#48527 = CARTESIAN_POINT ( 'NONE',  ( 17.20831665107776587, 37.88393115100078745, 7.208316651077764980 ) ) ;
#48528 = CARTESIAN_POINT ( 'NONE',  ( -8.000000000000000000, 80.99999999999994316, 3.000000000000000000 ) ) ;
#48530 = EDGE_CURVE ( 'NONE', #7679, #37275, #19510, .T. ) ;
#48529 = CARTESIAN_POINT ( 'NONE',  ( -0.8801773607111009756, 58.06368534415484106, 1.068504757029289695E-15 ) ) ;
#48531 = CARTESIAN_POINT ( 'NONE',  ( 6.565887622018943937, 35.16530133659708923, 12.81628187352647430 ) ) ;
#48532 = CARTESIAN_POINT ( 'NONE',  ( -5.204170427930421283E-15, -39.44625116508603213, -14.16423886937410082 ) ) ;
#48533 = CARTESIAN_POINT ( 'NONE',  ( 1.472469842513823179, 25.59226448433412315, -4.923371831947296329 ) ) ;
#48534 = CARTESIAN_POINT ( 'NONE',  ( 6.204703633549690345, 10.76208216824729824, -14.16423886937410259 ) ) ;
#48535 = ORIENTED_EDGE ( 'NONE', *, *, #61373, .T. ) ;
#48536 = ORIENTED_EDGE ( 'NONE', *, *, #81374, .F. ) ;
#48537 = EDGE_CURVE ( 'NONE', #19902, #37612, #98490, .T. ) ;
#48538 = CARTESIAN_POINT ( 'NONE',  ( 0.5774900079438590739, 32.64701867748816966, -5.440088680355550821 ) ) ;
#48539 = CARTESIAN_POINT ( 'NONE',  ( 22.26659068614895176, 34.72041550158063927, -7.082119434687042414 ) ) ;
#48540 = CARTESIAN_POINT ( 'NONE',  ( 17.20831665107776587, 47.88393115100078745, 7.208316651077764980 ) ) ;
#48541 = CARTESIAN_POINT ( 'NONE',  ( 5.076628168052704559, 10.17559781766745175, -8.527530157486179263 ) ) ;
#48543 = CARTESIAN_POINT ( 'NONE',  ( 64.56412365047462742, 13.99999999999999467, -9.500000000000000000 ) ) ;
#48542 = CARTESIAN_POINT ( 'NONE',  ( 19.38216949554541202, 50.99863466993042493, 9.382169495545424454 ) ) ;
#48544 = CARTESIAN_POINT ( 'NONE',  ( 17.96484262340118221, 24.93868534415484461, 7.964842623401181321 ) ) ;
#48545 = CARTESIAN_POINT ( 'NONE',  ( 11.49999999999999645, 75.00000000000000000, -8.525133428036872019 ) ) ;
#48546 = CARTESIAN_POINT ( 'NONE',  ( 13.43411237798105340, 25.58196800326374998, 12.81628187352647963 ) ) ;
#48547 = CARTESIAN_POINT ( 'NONE',  ( 2.791683348922237240, 35.38393115100079456, -7.208316651077763204 ) ) ;
#48548 = CARTESIAN_POINT ( 'NONE',  ( -2.915334737309917656, 4.105352010821503583, 10.88017736071110164 ) ) ;
#48549 = CARTESIAN_POINT ( 'NONE',  ( -25.69000000000001194, 93.50000000000000000, -10.09898361729590199 ) ) ;
#48551 = CARTESIAN_POINT ( 'NONE',  ( 18.95386800105010394, 33.23810908735718783, -6.500000000000008882 ) ) ;
#48550 = CARTESIAN_POINT ( 'NONE',  ( 10.00000000000000000, 61.81368534415484106, -10.88017736071110342 ) ) ;
#48552 = CARTESIAN_POINT ( 'NONE',  ( -10.91022435255008283, -52.91485255063000182, 4.000000000000000000 ) ) ;
#48553 = FACE_OUTER_BOUND ( 'NONE', #37530, .T. ) ;
#48554 = CARTESIAN_POINT ( 'NONE',  ( 7.084665262690076126, 59.10535201082150536, 10.88017736071109987 ) ) ;
#48555 = CARTESIAN_POINT ( 'NONE',  ( -0.8801773607110991993, 52.85535201082151247, -2.915334737309923874 ) ) ;
#48556 = DIRECTION ( 'NONE',  ( -0.000000000000000000, -1.000000000000000000, -0.000000000000000000 ) ) ;
#48558 = ADVANCED_FACE ( 'NONE', ( #10536 ), #93535, .T. ) ;
#48557 = FILL_AREA_STYLE ('',( #63559 ) ) ;
#48559 = CIRCLE ( 'NONE', #96479, 2.000000000000000888 ) ;
#48560 = CARTESIAN_POINT ( 'NONE',  ( 12.91533473730993009, 11.60535201082150714, -10.88017736071109987 ) ) ;
#48561 = CARTESIAN_POINT ( 'NONE',  ( 10.00000000000000178, 62.25893115100078745, 9.846743663894594434 ) ) ;
#48563 = CARTESIAN_POINT ( 'NONE',  ( 0.000000000000000000, 0.000000000000000000, 0.000000000000000000 ) ) ;
#48562 = CARTESIAN_POINT ( 'NONE',  ( 17.96484262340118221, 16.18868534415483396, -7.964842623401177768 ) ) ;
#48564 = CARTESIAN_POINT ( 'NONE',  ( 16.40814093676323893, 30.79030133659708923, 11.09922568453595026 ) ) ;
#48565 = ORIENTED_EDGE ( 'NONE', *, *, #17312, .F. ) ;
#48566 = CARTESIAN_POINT ( 'NONE',  ( -0.8801773607111009756, 53.06368534415484106, 1.068504757029289695E-15 ) ) ;
#48567 = EDGE_CURVE ( 'NONE', #30525, #40405, #27583, .T. ) ;
#48568 = CARTESIAN_POINT ( 'NONE',  ( 12.63842701281683922, 44.55059781766745175, -9.846743663894590881 ) ) ;
#48569 = AXIS2_PLACEMENT_3D ( 'NONE', #52233, #59725, #23729 ) ;
#48571 = SURFACE_STYLE_FILL_AREA ( #57055 ) ;
#48570 = CARTESIAN_POINT ( 'NONE',  ( 10.00000000000000000, 7.873634669930421381, -12.81628187352647608 ) ) ;
#48572 = CARTESIAN_POINT ( 'NONE',  ( 19.42250999205614548, 25.98035201082150891, -5.440088680355545492 ) ) ;
#48573 = CARTESIAN_POINT ( 'NONE',  ( 2.035157376598822676, 42.43868534415483396, -7.964842623401177768 ) ) ;
#48574 = CARTESIAN_POINT ( 'NONE',  ( -0.3689425029237898834, 51.17874883491397497, -10.36894250292378850 ) ) ;
#48575 = CARTESIAN_POINT ( 'NONE',  ( 17.20831665107776587, 37.88393115100078745, 7.208316651077764980 ) ) ;
#48576 = CARTESIAN_POINT ( 'NONE',  ( 19.42250999205614548, 60.98035201082151247, -5.440088680355545492 ) ) ;
#48577 = CARTESIAN_POINT ( 'NONE',  ( -0.8801773607111009756, 48.06368534415484817, 1.068504757029289695E-15 ) ) ;
#48578 = CARTESIAN_POINT ( 'NONE',  ( -8.564643372776458818, 14.63606914147517735, -12.31449893000756468 ) ) ;
#48579 = CARTESIAN_POINT ( 'NONE',  ( 24.16423886937410614, 14.30374883491396787, 8.672049930838204340E-16 ) ) ;
#48580 = DIRECTION ( 'NONE',  ( 0.000000000000000000, 1.000000000000000000, 0.000000000000000000 ) ) ;
#48581 = CARTESIAN_POINT ( 'NONE',  ( 0.2751277870542874204, 39.36607318730131055, -6.499999999999984901 ) ) ;
#48582 = ORIENTED_EDGE ( 'NONE', *, *, #57475, .T. ) ;
#48583 = ORIENTED_EDGE ( 'NONE', *, *, #57903, .F. ) ;
#48584 = CARTESIAN_POINT ( 'NONE',  ( 24.16423886937410614, 49.30374883491396787, 8.672049930838204340E-16 ) ) ;
#48585 = CARTESIAN_POINT ( 'NONE',  ( 20.36894250292379382, 38.67874883491396076, 10.36894250292379205 ) ) ;
#48586 = CARTESIAN_POINT ( 'NONE',  ( 1.472469842513823179, 21.42559781766745175, 4.923371831947296329 ) ) ;
#48587 = DIRECTION ( 'NONE',  ( -0.000000000000000000, -0.000000000000000000, 1.000000000000000000 ) ) ;
#48588 = CARTESIAN_POINT ( 'NONE',  ( 20.15039907845753220, 52.62777174578612716, -6.262539305110077947 ) ) ;
#48590 = CARTESIAN_POINT ( 'NONE',  ( -2.816281873526473856, 29.33196800326376064, 3.434112377981055619 ) ) ;
#48589 = CARTESIAN_POINT ( 'NONE',  ( 7.084665262690076126, 67.02201867748817676, -10.88017736071110164 ) ) ;
#48591 = CARTESIAN_POINT ( 'NONE',  ( -4.164238869374099927, 37.01208216824731068, 3.795296366450308767 ) ) ;
#48592 = CARTESIAN_POINT ( 'NONE',  ( 0.000000000000000000, 0.000000000000000000, 0.000000000000000000 ) ) ;
#48593 = CARTESIAN_POINT ( 'NONE',  ( 7.084665262690076126, 69.10535201082151957, 10.88017736071109987 ) ) ;
#48594 = CARTESIAN_POINT ( 'NONE',  ( -7.208316651077764980, -14.61606884899921077, -7.208316651077759651 ) ) ;
#48595 = CARTESIAN_POINT ( 'NONE',  ( 14.92337183194729633, 7.675597817667451750, 8.527530157486181039 ) ) ;
#48596 = EDGE_LOOP ( 'NONE', ( #25181, #61978, #2545, #95861 ) ) ;
#48597 =( NAMED_UNIT ( * ) SI_UNIT ( $, .STERADIAN. ) SOLID_ANGLE_UNIT ( ) );
#48598 = CARTESIAN_POINT ( 'NONE',  ( 1.472469842513823179, 16.42559781766745175, 4.923371831947296329 ) ) ;
#48599 = FACE_OUTER_BOUND ( 'NONE', #41974, .T. ) ;
#48600 = ORIENTED_EDGE ( 'NONE', *, *, #65382, .F. ) ;
#48601 = CARTESIAN_POINT ( 'NONE',  ( 24.16423886937410614, 4.512082168247300906, -3.795296366450302550 ) ) ;
#48603 = CARTESIAN_POINT ( 'NONE',  ( -0.8801773607111009756, 13.06368534415483929, 1.068504757029289695E-15 ) ) ;
#48602 = CARTESIAN_POINT ( 'NONE',  ( 7.084665262690076126, 9.105352010821503583, 10.88017736071109987 ) ) ;
#48605 = CARTESIAN_POINT ( 'NONE',  ( 0.6178305044545838731, 4.748634669930420493, 9.382169495545420901 ) ) ;
#48604 = CARTESIAN_POINT ( 'NONE',  ( 5.076628168052704559, 30.17559781766745175, -8.527530157486179263 ) ) ;
#48606 =( NAMED_UNIT ( * ) PLANE_ANGLE_UNIT ( ) SI_UNIT ( $, .RADIAN. ) );
#48607 = VECTOR ( 'NONE', #46743, 1000.000000000000000 ) ;
#48608 = CARTESIAN_POINT ( 'NONE',  ( -9.820177974736479243, 14.76984956101180835, 11.25994418464046198 ) ) ;
#48609 = EDGE_CURVE ( 'NONE', #24064, #56450, #25554, .T. ) ;
#48610 = CARTESIAN_POINT ( 'NONE',  ( 10.00000000000000000, 12.87363466993042138, -12.81628187352647608 ) ) ;
#48611 = EDGE_LOOP ( 'NONE', ( #2559, #27189, #78969, #95005 ) ) ;
#48612 = CARTESIAN_POINT ( 'NONE',  ( -0.3689425029237898834, 46.17874883491397497, -10.36894250292378850 ) ) ;
#48613 = ORIENTED_EDGE ( 'NONE', *, *, #70780, .F. ) ;
#48614 = CARTESIAN_POINT ( 'NONE',  ( 17.08211943468705840, 60.13708216824729647, -12.26659068614894466 ) ) ;
#48615 = ORIENTED_EDGE ( 'NONE', *, *, #80844, .F. ) ;
#48616 = CARTESIAN_POINT ( 'NONE',  ( 0.5774900079438590739, 27.64701867748817676, -5.440088680355550821 ) ) ;
#48617 = CARTESIAN_POINT ( 'NONE',  ( 0.5774900079438590739, 37.64701867748817676, -5.440088680355550821 ) ) ;
#48618 = CARTESIAN_POINT ( 'NONE',  ( 19.42250999205614548, 60.98035201082151247, -5.440088680355545492 ) ) ;
#48619 = CARTESIAN_POINT ( 'NONE',  ( 15.44008868035555260, 29.73035201082150891, 9.422509992056143702 ) ) ;
#48621 = EDGE_LOOP ( 'NONE', ( #6673, #70736, #79119, #4452 ) ) ;
#48620 = CARTESIAN_POINT ( 'NONE',  ( -8.000000000000000000, 41.24999999999999289, 4.000000000000000000 ) ) ;
#48622 = STYLED_ITEM ( 'NONE', ( #87864 ), #95471 ) ;
#48623 = CARTESIAN_POINT ( 'NONE',  ( 18.52753015748617571, 18.09226448433411960, 4.923371831947298993 ) ) ;
#48624 = CARTESIAN_POINT ( 'NONE',  ( -3.770608837557422710, -6.399801140515898545, 2.750000000000403677 ) ) ;
#48625 = VERTEX_POINT ( 'NONE', #4031 ) ;
#48626 = CARTESIAN_POINT ( 'NONE',  ( 11.33984840998195054, -87.82327540140187239, 3.750000000000000000 ) ) ;
#48627 = CARTESIAN_POINT ( 'NONE',  ( 2.791683348922237240, 45.38393115100079456, -7.208316651077763204 ) ) ;
#48628 = VECTOR ( 'NONE', #47441, 1000.000000000000000 ) ;
#48629 = DIRECTION ( 'NONE',  ( 0.000000000000000000, 1.000000000000000000, 0.000000000000000000 ) ) ;
#48630 = CARTESIAN_POINT ( 'NONE',  ( 3.591859063236761518, 44.95696800326376064, 11.09922568453594849 ) ) ;
#48631 = ADVANCED_FACE ( 'NONE', ( #56046 ), #96513, .T. ) ;
#48632 = CARTESIAN_POINT ( 'NONE',  ( -6.445967608602039434, -48.01283281809150338, 2.750000000000000000 ) ) ;
#48633 = CYLINDRICAL_SURFACE ( 'NONE', #26859, 1.000000000000007772 ) ;
#48634 = CARTESIAN_POINT ( 'NONE',  ( 7.993487411949270260, 0.04962888323599794205, 12.40005926694712990 ) ) ;
#48635 = CARTESIAN_POINT ( 'NONE',  ( 2.791683348922240793, 61.63393115100079456, 7.208316651077764092 ) ) ;
#48636 = CARTESIAN_POINT ( 'NONE',  ( 24.16423886937410614, 49.30374883491396787, 8.672049930838204340E-16 ) ) ;
#48637 = CARTESIAN_POINT ( 'NONE',  ( 6.689969769698871360, 15.00000000000000000, 12.58200319823975022 ) ) ;
#48638 = ORIENTED_EDGE ( 'NONE', *, *, #95617, .F. ) ;
#48639 = CARTESIAN_POINT ( 'NONE',  ( 1.042145700049401436, 4.742161081720030147, -6.499999999999861444 ) ) ;
#48640 = CARTESIAN_POINT ( 'NONE',  ( 1.472469842513823179, 26.42559781766745175, 4.923371831947296329 ) ) ;
#48641 = CARTESIAN_POINT ( 'NONE',  ( -2.816281873526473856, 64.33196800326376774, 3.434112377981055619 ) ) ;
#48642 = CARTESIAN_POINT ( 'NONE',  ( 1.472469842513823179, 65.59226448433412315, -4.923371831947296329 ) ) ;
#48643 = CARTESIAN_POINT ( 'NONE',  ( 14.92337183194729633, 2.675597817667451750, 8.527530157486181039 ) ) ;
#48644 = CARTESIAN_POINT ( 'NONE',  ( -0.03743638938523734944, 4.251975280310180239, -6.399506433553933782 ) ) ;
#48645 = B_SPLINE_CURVE_WITH_KNOTS ( 'NONE', 3,
 ( #74435, #21455, #82936, #21957, #14453, #27463 ),
 .UNSPECIFIED., .F., .F.,
 ( 4, 2, 4 ),
 ( 3.409110551496048698E-05, 0.0004400426677367984978, 0.0008459942299586365290 ),
 .UNSPECIFIED. ) ;
#48646 = CARTESIAN_POINT ( 'NONE',  ( 12.63842701281683922, 64.55059781766745175, -9.846743663894590881 ) ) ;
#48647 = CARTESIAN_POINT ( 'NONE',  ( 20.32896413005680358, 14.74545670184113710, 5.963430220938287007 ) ) ;
#48648 = MECHANICAL_DESIGN_GEOMETRIC_PRESENTATION_REPRESENTATION (  '', ( #64618 ), #37549 ) ;
#48649 = ADVANCED_FACE ( 'NONE', ( #48028 ), #89820, .T. ) ;
#48650 = EDGE_CURVE ( 'NONE', #75691, #73066, #67500, .T. ) ;
#48651 = VERTEX_POINT ( 'NONE', #21991 ) ;
#48652 = CARTESIAN_POINT ( 'NONE',  ( 24.16423886937410614, 59.51208216824728936, -3.795296366450302550 ) ) ;
#48653 = CARTESIAN_POINT ( 'NONE',  ( -18.89999999999999503, 92.00000000000000000, 8.000000000000000000 ) ) ;
#48654 = CARTESIAN_POINT ( 'NONE',  ( 7.084665262690076126, 47.02201867748818387, -10.88017736071110164 ) ) ;
#48656 = CARTESIAN_POINT ( 'NONE',  ( 17.96484262340118221, 66.18868534415483396, -7.964842623401177768 ) ) ;
#48655 = CARTESIAN_POINT ( 'NONE',  ( -2.816281873526471635, 13.91530133659708746, -3.434112377981056508 ) ) ;
#48657 = CARTESIAN_POINT ( 'NONE',  ( 10.93781366033347169, 0.5000000000000004441, -10.26470809774065351 ) ) ;
#48658 = CARTESIAN_POINT ( 'NONE',  ( 19.80777595082615861, 45.68878173731741299, -6.499999999999961808 ) ) ;
#48659 = CARTESIAN_POINT ( 'NONE',  ( 1.472469842513823179, 56.42559781766745886, 4.923371831947296329 ) ) ;
#48660 = CARTESIAN_POINT ( 'NONE',  ( 10.00000000000000178, 7.258931151000785675, 9.846743663894594434 ) ) ;
#48661 = CARTESIAN_POINT ( 'NONE',  ( 3.469446951953614189E-15, -35.68631465584515894, 10.88017736071110342 ) ) ;
#48662 = CARTESIAN_POINT ( 'NONE',  ( 22.81628187352647785, 6.623634669930420493, 6.195893100308588602E-16 ) ) ;
#48664 = DIRECTION ( 'NONE',  ( 0.000000000000000000, 0.000000000000000000, 1.000000000000000000 ) ) ;
#48663 = CARTESIAN_POINT ( 'NONE',  ( 10.00000000000000000, 21.81368534415484106, -10.88017736071110342 ) ) ;
#48665 = CARTESIAN_POINT ( 'NONE',  ( 13.99999999999999822, 10.49999999999999822, -6.000000000000000000 ) ) ;
#48666 =( GEOMETRIC_REPRESENTATION_CONTEXT ( 3 ) GLOBAL_UNCERTAINTY_ASSIGNED_CONTEXT ( ( #74264 ) ) GLOBAL_UNIT_ASSIGNED_CONTEXT ( ( #4608, #48606, #34087 ) ) REPRESENTATION_CONTEXT ( 'NONE', 'WORKASPACE' ) );
#48667 = CARTESIAN_POINT ( 'NONE',  ( 6.204703633549690345, 37.84541550158063927, 14.16423886937410082 ) ) ;
#48668 = CARTESIAN_POINT ( 'NONE',  ( 13.79529636645031943, 25.34541550158063572, -14.16423886937409904 ) ) ;
#48669 = CARTESIAN_POINT ( 'NONE',  ( 7.084665262690076126, 2.022018677488171434, -10.88017736071110164 ) ) ;
#48670 = CARTESIAN_POINT ( 'NONE',  ( 19.84674366389459266, 38.30059781766745175, 2.638427012816836559 ) ) ;
#48671 = CARTESIAN_POINT ( 'NONE',  ( 22.81628187352648496, 41.83196800326375353, -3.434112377981050290 ) ) ;
#48672 = CARTESIAN_POINT ( 'NONE',  ( -0.8801773607111009756, 13.06368534415483929, 1.068504757029289695E-15 ) ) ;
#48673 = ORIENTED_EDGE ( 'NONE', *, *, #40324, .F. ) ;
#48674 = CARTESIAN_POINT ( 'NONE',  ( 18.52753015748617571, 33.09226448433411605, 4.923371831947298993 ) ) ;
#48675 = CARTESIAN_POINT ( 'NONE',  ( -0.8801773607111008646, 43.27201867748817676, 2.915334737309923430 ) ) ;
#48676 = CARTESIAN_POINT ( 'NONE',  ( 6.565887622018943937, 10.16530133659708746, 12.81628187352647430 ) ) ;
#48678 = CARTESIAN_POINT ( 'NONE',  ( 17.35999999999999943, 33.99999999999997158, 10.00000000000000000 ) ) ;
#48677 = CARTESIAN_POINT ( 'NONE',  ( 17.08211943468705840, 15.13708216824730179, -12.26659068614894466 ) ) ;
#48680 = CARTESIAN_POINT ( 'NONE',  ( 14.40939250469964961, 15.00000000000000000, 1.618458416365853747 ) ) ;
#48679 = B_SPLINE_CURVE_WITH_KNOTS ( 'NONE', 3,
 ( #87924, #80928, #19441, #49930, #33924, #11936, #65415, #26933, #42441, #72923 ),
 .UNSPECIFIED., .F., .F.,
 ( 4, 3, 3, 4 ),
 ( 7.573910767901059648E-18, 0.0006253016069560791285, 0.001250604074564940806, 0.002501455912506563885 ),
 .UNSPECIFIED. ) ;
#48681 = CARTESIAN_POINT ( 'NONE',  ( 19.84674366389459266, 28.30059781766745886, 2.638427012816836559 ) ) ;
#48682 = CARTESIAN_POINT ( 'NONE',  ( -1.099225684535947600, 53.70696800326376064, -6.408140936763238038 ) ) ;
#48683 = CARTESIAN_POINT ( 'NONE',  ( 12.63842701281683922, 59.55059781766744464, -9.846743663894590881 ) ) ;
#48684 = ORIENTED_EDGE ( 'NONE', *, *, #46967, .F. ) ;
#48685 = EDGE_CURVE ( 'NONE', #33923, #34058, #5261, .T. ) ;
#48686 = CARTESIAN_POINT ( 'NONE',  ( 12.35505582470273644, 15.00000000000000000, -10.16021613965630443 ) ) ;
#48687 = CARTESIAN_POINT ( 'NONE',  ( 4.380000000000000782, 1.019547802438464545, 3.750000000000001776 ) ) ;
#48688 = CARTESIAN_POINT ( 'NONE',  ( -0.3689425029237881626, 62.42874883491396787, 10.36894250292379027 ) ) ;
#48689 = CARTESIAN_POINT ( 'NONE',  ( 22.26659068614895176, 9.720415501580633943, -7.082119434687042414 ) ) ;
#48690 = CARTESIAN_POINT ( 'NONE',  ( 20.88017736071110164, 65.35535201082150536, 2.915334737309930979 ) ) ;
#48691 = CARTESIAN_POINT ( 'NONE',  ( 5.076628168052704559, 45.17559781766745175, -8.527530157486179263 ) ) ;
#48692 = CARTESIAN_POINT ( 'NONE',  ( 2.035157376598824452, 23.68868534415484461, 7.964842623401179544 ) ) ;
#48693 = CARTESIAN_POINT ( 'NONE',  ( 4.219999999999999751, 36.75000000000000000, 2.750000000000000000 ) ) ;
#48694 = CARTESIAN_POINT ( 'NONE',  ( 18.52753015748617571, 63.09226448433412315, 4.923371831947298993 ) ) ;
#48695 = VECTOR ( 'NONE', #73889, 1000.000000000000000 ) ;
#48696 = ORIENTED_EDGE ( 'NONE', *, *, #92118, .F. ) ;
#48697 = EDGE_LOOP ( 'NONE', ( #38342, #28858, #3814, #4222, #10180, #7072 ) ) ;
#48698 = ORIENTED_EDGE ( 'NONE', *, *, #20227, .T. ) ;
#48699 = DIRECTION ( 'NONE',  ( 0.000000000000000000, 0.000000000000000000, 1.000000000000000000 ) ) ;
#48700 = CARTESIAN_POINT ( 'NONE',  ( 6.204703633549690345, 10.76208216824729824, -14.16423886937410259 ) ) ;
#48701 = FILL_AREA_STYLE ('',( #25248 ) ) ;
#48702 = CARTESIAN_POINT ( 'NONE',  ( 13.79529636645030344, 38.26208216824729647, 14.16423886937410614 ) ) ;
#48703 = CARTESIAN_POINT ( 'NONE',  ( 18.52753015748618282, 58.92559781766745886, -4.923371831947291888 ) ) ;
#48704 = CARTESIAN_POINT ( 'NONE',  ( 10.00000000000000000, 19.75893115100078390, -9.846743663894594434 ) ) ;
#48705 = CARTESIAN_POINT ( 'NONE',  ( -2.816281873526473856, 64.33196800326376774, 3.434112377981055619 ) ) ;
#48707 = CARTESIAN_POINT ( 'NONE',  ( 18.52753015748617571, 58.09226448433411605, 4.923371831947298993 ) ) ;
#48706 = CARTESIAN_POINT ( 'NONE',  ( 17.96484262340118221, 24.93868534415484461, 7.964842623401181321 ) ) ;
#48708 = CARTESIAN_POINT ( 'NONE',  ( -4.164238869374099927, 2.012082168247300906, 3.795296366450308767 ) ) ;
#48709 = CARTESIAN_POINT ( 'NONE',  ( 2.917880565312948704, 42.63708216824729647, 12.26659068614894643 ) ) ;
#48710 =( GEOMETRIC_REPRESENTATION_CONTEXT ( 3 ) GLOBAL_UNCERTAINTY_ASSIGNED_CONTEXT ( ( #51475 ) ) GLOBAL_UNIT_ASSIGNED_CONTEXT ( ( #67841, #14345, #13847 ) ) REPRESENTATION_CONTEXT ( 'NONE', 'WORKASPACE' ) );
#48711 = CARTESIAN_POINT ( 'NONE',  ( -0.8801773607111008646, 8.272018677488171434, 2.915334737309923430 ) ) ;
#48712 = CARTESIAN_POINT ( 'NONE',  ( 5.076628168052703671, 66.84226448433412315, 8.527530157486179263 ) ) ;
#48713 = DIRECTION ( 'NONE',  ( 0.000000000000000000, 1.000000000000000000, 0.000000000000000000 ) ) ;
#48714 = CARTESIAN_POINT ( 'NONE',  ( 15.44008868035555260, 64.73035201082151957, 9.422509992056143702 ) ) ;
#48715 = CARTESIAN_POINT ( 'NONE',  ( 14.92337183194729988, 34.34226448433411605, -8.527530157486177487 ) ) ;
#48716 = CARTESIAN_POINT ( 'NONE',  ( -7.121448108906508700, -73.25984652122873797, 3.750000000000000888 ) ) ;
#48717 = ORIENTED_EDGE ( 'NONE', *, *, #81866, .F. ) ;
#48718 = CARTESIAN_POINT ( 'NONE',  ( 0.9940297508536876103, -0.03417435944610275333, 14.21528771620250353 ) ) ;
#48719 = ORIENTED_EDGE ( 'NONE', *, *, #7294, .T. ) ;
#48720 = CARTESIAN_POINT ( 'NONE',  ( 18.52753015748617571, 23.09226448433411960, 4.923371831947298993 ) ) ;
#48721 = ORIENTED_EDGE ( 'NONE', *, *, #14032, .F. ) ;
#48722 = CARTESIAN_POINT ( 'NONE',  ( 24.16423886937410614, 39.30374883491396787, 8.672049930838204340E-16 ) ) ;
#48723 = CARTESIAN_POINT ( 'NONE',  ( 0.1532563361054083140, 36.00893115100078745, 1.131784320476157264E-15 ) ) ;
#48724 = CARTESIAN_POINT ( 'NONE',  ( 15.44008868035555260, 49.73035201082150536, 9.422509992056143702 ) ) ;
#48725 = CARTESIAN_POINT ( 'NONE',  ( 0.5774900079438590739, 47.64701867748817676, -5.440088680355550821 ) ) ;
#48726 = CARTESIAN_POINT ( 'NONE',  ( 14.49440716394873263, 4.853942851202206293E-16, 0.4026921475167233311 ) ) ;
#48727 = AXIS2_PLACEMENT_3D ( 'NONE', #24232, #32192, #86693 ) ;
#48728 = CARTESIAN_POINT ( 'NONE',  ( 6.408140936763236262, -2.543031996736243361, -11.09922568453595026 ) ) ;
#48729 = ORIENTED_EDGE ( 'NONE', *, *, #80448, .T. ) ;
#48730 = CARTESIAN_POINT ( 'NONE',  ( 20.88017736071110519, 45.56368534415484106, 2.639326808657452039E-16 ) ) ;
#48731 = CARTESIAN_POINT ( 'NONE',  ( -2.266590686148945544, 1.387082168247301128, -7.082119434687050408 ) ) ;
#48732 = ORIENTED_EDGE ( 'NONE', *, *, #32163, .F. ) ;
#48733 = CARTESIAN_POINT ( 'NONE',  ( 10.00000000000000178, 30.37363466993042138, 12.81628187352647608 ) ) ;
#48734 = CARTESIAN_POINT ( 'NONE',  ( 19.84674366389459266, 28.71726448433411960, -2.638427012816827677 ) ) ;
#48735 = PRESENTATION_STYLE_ASSIGNMENT (( #26724 ) ) ;
#48736 = CARTESIAN_POINT ( 'NONE',  ( 22.81628187352647785, 46.62363466993041783, 6.195893100308588602E-16 ) ) ;
#48737 = LINE ( 'NONE', #35709, #19186 ) ;
#48738 = CARTESIAN_POINT ( 'NONE',  ( 7.361572987183170547, 27.05059781766745175, 9.846743663894590881 ) ) ;
#48740 = EDGE_CURVE ( 'NONE', #54629, #23697, #60557, .T. ) ;
#48739 = PRESENTATION_LAYER_ASSIGNMENT (  '', '', ( #31181 ) ) ;
#48741 = CARTESIAN_POINT ( 'NONE',  ( 0.5774900079438607392, 58.48035201082151247, 5.440088680355550821 ) ) ;
#48742 = VECTOR ( 'NONE', #12646, 1000.000000000000000 ) ;
#48743 = CARTESIAN_POINT ( 'NONE',  ( 0.000000000000000000, 0.5000000000000004441, 0.000000000000000000 ) ) ;
#48744 = CARTESIAN_POINT ( 'NONE',  ( -46.30928139467842897, 104.0823827281712255, 5.529860068218143354 ) ) ;
#48745 = CARTESIAN_POINT ( 'NONE',  ( 1.847340224724850932, 14.95077488074853456, -14.63671528203490979 ) ) ;
#48746 = CARTESIAN_POINT ( 'NONE',  ( 19.84674366389459266, 3.300597817667451750, 2.638427012816836559 ) ) ;
#48747 = CARTESIAN_POINT ( 'NONE',  ( 19.38216949554541557, 7.248634669930421381, -9.382169495545420901 ) ) ;
#48748 = PLANE ( 'NONE',  #1998 ) ;
#48749 = TOROIDAL_SURFACE ( 'NONE', #43968, 14.49999999999999822, 0.5000000000000000000 ) ;
#48750 = CARTESIAN_POINT ( 'NONE',  ( 19.84674366389459266, 43.30059781766744464, 2.638427012816836559 ) ) ;
#48751 = CARTESIAN_POINT ( 'NONE',  ( 19.38216949554541557, 62.24863466993041072, -9.382169495545420901 ) ) ;
#48752 = CARTESIAN_POINT ( 'NONE',  ( 10.00000000000000178, 8.053748834913967869, 14.16423886937410082 ) ) ;
#48753 = CARTESIAN_POINT ( 'NONE',  ( 12.63842701281683922, 39.55059781766744464, -9.846743663894590881 ) ) ;
#48754 = CARTESIAN_POINT ( 'NONE',  ( -1.099225684535947600, 28.70696800326375353, -6.408140936763238038 ) ) ;
#48756 = CARTESIAN_POINT ( 'NONE',  ( 19.89103541497710737, 15.66234555792571292, -6.479102184480796112 ) ) ;
#48755 = CARTESIAN_POINT ( 'NONE',  ( 14.29730467489532408, 4.491438197698105257E-16, 2.416004766803315995 ) ) ;
#48757 = CARTESIAN_POINT ( 'NONE',  ( 2.035157376598824452, 43.68868534415484106, 7.964842623401179544 ) ) ;
#48758 = EDGE_CURVE ( 'NONE', #60661, #47206, #87992, .T. ) ;
#48759 = CARTESIAN_POINT ( 'NONE',  ( 13.43411237798106583, 12.66530133659708746, -12.81628187352647252 ) ) ;
#48760 = CARTESIAN_POINT ( 'NONE',  ( 1.472469842513823179, 41.42559781766745886, 4.923371831947296329 ) ) ;
#48761 = CARTESIAN_POINT ( 'NONE',  ( 0.1532563361054083140, 16.00893115100078390, 1.131784320476157264E-15 ) ) ;
#48762 = CARTESIAN_POINT ( 'NONE',  ( -0.8801773607111009756, 33.06368534415484106, 1.068504757029289695E-15 ) ) ;
#48763 = CARTESIAN_POINT ( 'NONE',  ( 21.09922568453595559, 27.04030133659708568, -6.408140936763230044 ) ) ;
#48764 = AXIS2_PLACEMENT_3D ( 'NONE', #93976, #24516, #85993 ) ;
#48765 = CARTESIAN_POINT ( 'NONE',  ( 5.076628168052704559, 25.17559781766745175, -8.527530157486179263 ) ) ;
#48766 =( LENGTH_UNIT ( ) NAMED_UNIT ( * ) SI_UNIT ( .MILLI., .METRE. ) );
#48767 = CARTESIAN_POINT ( 'NONE',  ( -9.884188733557275341, 88.99910865660901038, 5.687374854485731213 ) ) ;
#48768 = EDGE_CURVE ( 'NONE', #62241, #86312, #74901, .T. ) ;
#48769 = CARTESIAN_POINT ( 'NONE',  ( 4.559911319644449179, 38.89701867748817676, 9.422509992056141925 ) ) ;
#48770 = EDGE_CURVE ( 'NONE', #11363, #41505, #5008, .T. ) ;
#48771 = VERTEX_POINT ( 'NONE', #65986 ) ;
#48772 = CARTESIAN_POINT ( 'NONE',  ( 7.084665262690076126, 64.10535201082150536, 10.88017736071109987 ) ) ;
#48774 = CARTESIAN_POINT ( 'NONE',  ( 4.559911319644449179, 37.23035201082150536, -9.422509992056141925 ) ) ;
#48773 = CARTESIAN_POINT ( 'NONE',  ( 5.076628168052703671, 46.84226448433412315, 8.527530157486179263 ) ) ;
#48775 = SURFACE_STYLE_FILL_AREA ( #16818 ) ;
#48776 = CARTESIAN_POINT ( 'NONE',  ( 15.44008868035555793, 46.39701867748817676, -9.422509992056140149 ) ) ;
#48778 = SURFACE_STYLE_USAGE ( .BOTH. , #71305 ) ;
#48777 = CARTESIAN_POINT ( 'NONE',  ( 4.559911319644449179, 13.89701867748817321, 9.422509992056141925 ) ) ;
#48779 = CARTESIAN_POINT ( 'NONE',  ( 14.94699059465100888, 0.5000000000000004441, 1.259949270174915981 ) ) ;
#48780 = CARTESIAN_POINT ( 'NONE',  ( 2.791683348922237240, 40.38393115100078035, -7.208316651077763204 ) ) ;
#48782 = CARTESIAN_POINT ( 'NONE',  ( 6.382347221874334231, 15.00000000000000000, 13.57444820018231724 ) ) ;
#48781 = CARTESIAN_POINT ( 'NONE',  ( -4.164238869374098151, 36.59541550158063217, -3.795296366450310543 ) ) ;
#48783 = CARTESIAN_POINT ( 'NONE',  ( 1.821708436314931845, 6.667925641218958255, -6.500000000000002665 ) ) ;
#48784 = CARTESIAN_POINT ( 'NONE',  ( -0.2838433074297238012, 13.12729635533385597, 10.00000000000000000 ) ) ;
#48785 = CARTESIAN_POINT ( 'NONE',  ( 24.16423886937410614, 24.51208216824730002, -3.795296366450302550 ) ) ;
#48786 = CARTESIAN_POINT ( 'NONE',  ( -7.121364477235284873, -73.24716134357460362, 2.750000000000000444 ) ) ;
#48787 = ORIENTED_EDGE ( 'NONE', *, *, #6341, .F. ) ;
#48788 = MECHANICAL_DESIGN_GEOMETRIC_PRESENTATION_REPRESENTATION (  '', ( #10482 ), #37687 ) ;
#48789 = CARTESIAN_POINT ( 'NONE',  ( 0.5774900079438590739, 2.647018677488171434, -5.440088680355550821 ) ) ;
#48790 = CARTESIAN_POINT ( 'NONE',  ( 18.52753015748618282, 28.92559781766745175, -4.923371831947291888 ) ) ;
#48792 = CARTESIAN_POINT ( 'NONE',  ( -8.000343251535923628, 84.06932101904432386, -4.000000000000000000 ) ) ;
#48791 = FACE_OUTER_BOUND ( 'NONE', #61987, .T. ) ;
#48793 = CARTESIAN_POINT ( 'NONE',  ( -0.8801773607111008646, 53.27201867748816966, 2.915334737309923430 ) ) ;
#48794 = CARTESIAN_POINT ( 'NONE',  ( -2.816281873526471635, 63.91530133659708923, -3.434112377981056508 ) ) ;
#48795 = CARTESIAN_POINT ( 'NONE',  ( 12.91533473730993009, 31.60535201082150891, -10.88017736071109987 ) ) ;
#48796 = CARTESIAN_POINT ( 'NONE',  ( 3.591859063236761518, 59.95696800326375353, 11.09922568453594849 ) ) ;
#48797 = CARTESIAN_POINT ( 'NONE',  ( 0.6178305044545838731, 4.748634669930420493, 9.382169495545420901 ) ) ;
#48798 = CARTESIAN_POINT ( 'NONE',  ( 14.92337183194729633, 17.67559781766745175, 8.527530157486181039 ) ) ;
#48799 = VERTEX_POINT ( 'NONE', #58481 ) ;
#48800 = ADVANCED_FACE ( 'NONE', ( #28489 ), #58982, .F. ) ;
#48801 = LINE ( 'NONE', #33777, #7948 ) ;
#48802 = CARTESIAN_POINT ( 'NONE',  ( 6.204703633549690345, 65.76208216824731778, -14.16423886937410259 ) ) ;
#48803 = CARTESIAN_POINT ( 'NONE',  ( 20.36894250292379738, 29.92874883491396432, -10.36894250292379027 ) ) ;
#48804 = CARTESIAN_POINT ( 'NONE',  ( 12.91533473730993009, 36.60535201082151247, -10.88017736071109987 ) ) ;
#48805 = CARTESIAN_POINT ( 'NONE',  ( -0.8801773607111009756, 48.06368534415484817, 1.068504757029289695E-15 ) ) ;
#48806 = FILL_AREA_STYLE ('',( #9843 ) ) ;
#48807 = CARTESIAN_POINT ( 'NONE',  ( -7.674335239599113123, 0.2306972965111898366, -12.81961907869226991 ) ) ;
#48808 = CARTESIAN_POINT ( 'NONE',  ( 18.52753015748617571, 13.09226448433411960, 4.923371831947298993 ) ) ;
#48809 = FACE_OUTER_BOUND ( 'NONE', #85138, .T. ) ;
#48810 = CARTESIAN_POINT ( 'NONE',  ( 0.1532563361054100626, 25.80059781766744820, -2.638427012816831230 ) ) ;
#48811 = DIRECTION ( 'NONE',  ( 0.8070303256584299145, -0.5905099943842175847, 0.000000000000000000 ) ) ;
#48812 = CARTESIAN_POINT ( 'NONE',  ( 0.2751277870542967463, 70.00000000000000000, -6.500000000000000888 ) ) ;
#48813 = CARTESIAN_POINT ( 'NONE',  ( 7.361572987183169658, 19.96726448433411960, -9.846743663894592657 ) ) ;
#48814 = CARTESIAN_POINT ( 'NONE',  ( 2.791683348922240793, 46.63393115100077324, 7.208316651077764092 ) ) ;
#48815 = CARTESIAN_POINT ( 'NONE',  ( 22.81628187352647785, 41.62363466993042493, 6.195893100308588602E-16 ) ) ;
#48816 = COLOUR_RGB ( '', 0.66274510, 0.83137255, 0.94901961) ;
#48817 = CARTESIAN_POINT ( 'NONE',  ( 19.42250999205614548, 55.98035201082150536, -5.440088680355545492 ) ) ;
#48818 = CARTESIAN_POINT ( 'NONE',  ( 1.472469842513823179, 26.42559781766745175, 4.923371831947296329 ) ) ;
#48820 = CARTESIAN_POINT ( 'NONE',  ( 1.472469842513823179, 21.42559781766745175, 4.923371831947296329 ) ) ;
#48819 = CARTESIAN_POINT ( 'NONE',  ( -4.164238869374098151, 51.59541550158063217, -3.795296366450310543 ) ) ;
#48821 = DIRECTION ( 'NONE',  ( 0.9943711317468826305, 0.1059530667249613811, 0.000000000000000000 ) ) ;
#48822 = CARTESIAN_POINT ( 'NONE',  ( 1.472469842513823179, 65.59226448433412315, -4.923371831947296329 ) ) ;
#48823 = CARTESIAN_POINT ( 'NONE',  ( 22.26659068614894466, 28.88708216824730357, 7.082119434687054849 ) ) ;
#48824 = CARTESIAN_POINT ( 'NONE',  ( 0.1532563361054082862, 31.21726448433412315, 2.638427012816831674 ) ) ;
#48825 = CARTESIAN_POINT ( 'NONE',  ( 34.56412365047463453, 13.99999999999999645, -10.00000000000000000 ) ) ;
#48826 = CARTESIAN_POINT ( 'NONE',  ( 10.00000000000000178, 19.31368534415484106, 10.88017736071110342 ) ) ;
#48827 = CARTESIAN_POINT ( 'NONE',  ( 4.559911319644449179, 48.89701867748817676, 9.422509992056141925 ) ) ;
#48828 = CARTESIAN_POINT ( 'NONE',  ( 12.91533473730992121, 49.52201867748817676, 10.88017736071110164 ) ) ;
#48829 = ORIENTED_EDGE ( 'NONE', *, *, #70118, .F. ) ;
#48830 = CARTESIAN_POINT ( 'NONE',  ( 16.40814093676324603, 37.45696800326376064, -11.09922568453594671 ) ) ;
#48831 = CARTESIAN_POINT ( 'NONE',  ( 0.5774900079438607392, 58.48035201082151247, 5.440088680355550821 ) ) ;
#48832 = ORIENTED_EDGE ( 'NONE', *, *, #40681, .F. ) ;
#48833 = DIRECTION ( 'NONE',  ( -0.000000000000000000, -0.000000000000000000, 1.000000000000000000 ) ) ;
#48834 = CARTESIAN_POINT ( 'NONE',  ( 2.035157376598824452, 68.68868534415484817, 7.964842623401179544 ) ) ;
#48835 = AXIS2_PLACEMENT_3D ( 'NONE', #40917, #87383, #62405 ) ;
#48836 = ORIENTED_EDGE ( 'NONE', *, *, #77434, .F. ) ;
#48837 = CIRCLE ( 'NONE', #23316, 0.2500000000000002220 ) ;
#48838 = CARTESIAN_POINT ( 'NONE',  ( -0.8801773607111008646, 63.27201867748817676, 2.915334737309923430 ) ) ;
#48839 = CARTESIAN_POINT ( 'NONE',  ( 17.96484262340118221, 4.938685344154837509, 7.964842623401181321 ) ) ;
#48840 = CARTESIAN_POINT ( 'NONE',  ( 1.821708436314921853, 26.66792564121896802, -6.499999999999992006 ) ) ;
#48841 = LINE ( 'NONE', #63833, #26925 ) ;
#48842 = CARTESIAN_POINT ( 'NONE',  ( 4.559911319644449179, 12.23035201082150714, -9.422509992056141925 ) ) ;
#48843 = CARTESIAN_POINT ( 'NONE',  ( 0.1532563361054082862, 16.21726448433411960, 2.638427012816831674 ) ) ;
#48844 = CARTESIAN_POINT ( 'NONE',  ( 24.16423886937410614, 9.303748834913967869, 8.672049930838204340E-16 ) ) ;
#48845 = AXIS2_PLACEMENT_3D ( 'NONE', #58406, #65913, #36415 ) ;
#48846 = CARTESIAN_POINT ( 'NONE',  ( 10.00000000000000178, 2.258931151000784787, 9.846743663894594434 ) ) ;
#48847 = B_SPLINE_CURVE_WITH_KNOTS ( 'NONE', 3,
 ( #66895, #67893, #15397, #43884, #22398, #14402 ),
 .UNSPECIFIED., .F., .F.,
 ( 4, 2, 4 ),
 ( 0.000000000000000000, 0.0002701661927229319750, 0.0005403323854458639500 ),
 .UNSPECIFIED. ) ;
#48848 = CARTESIAN_POINT ( 'NONE',  ( 2.035157376598822676, 7.438685344154837509, -7.964842623401177768 ) ) ;
#48849 = CARTESIAN_POINT ( 'NONE',  ( 0.1532563361054100626, 40.80059781766745886, -2.638427012816831230 ) ) ;
#48850 = ORIENTED_EDGE ( 'NONE', *, *, #22611, .F. ) ;
#48851 = CARTESIAN_POINT ( 'NONE',  ( 10.00000000000000000, 54.75893115100078745, -9.846743663894594434 ) ) ;
#48852 = ORIENTED_EDGE ( 'NONE', *, *, #57142, .F. ) ;
#48853 = CARTESIAN_POINT ( 'NONE',  ( 7.084665262690076126, 47.02201867748818387, -10.88017736071110164 ) ) ;
#48854 = CARTESIAN_POINT ( 'NONE',  ( 7.361572987183170547, 47.05059781766745175, 9.846743663894590881 ) ) ;
#48855 = CARTESIAN_POINT ( 'NONE',  ( 3.591859063236761518, 29.95696800326375708, 11.09922568453594849 ) ) ;
#48857 = CARTESIAN_POINT ( 'NONE',  ( 6.091055032734291608, 15.00000000000000888, 13.29802223412760753 ) ) ;
#48856 = CARTESIAN_POINT ( 'NONE',  ( -13.48255862861931043, 4.084149796850864849E-16, 5.335786055104065007 ) ) ;
#48858 = CARTESIAN_POINT ( 'NONE',  ( 12.91533473730992121, 64.52201867748817676, 10.88017736071110164 ) ) ;
#48859 = CARTESIAN_POINT ( 'NONE',  ( 2.035157376598822676, 7.438685344154837509, -7.964842623401177768 ) ) ;
#48860 = EDGE_CURVE ( 'NONE', #79829, #14094, #80256, .T. ) ;
#48861 = CARTESIAN_POINT ( 'NONE',  ( 22.81628187352648496, 46.83196800326376064, -3.434112377981050290 ) ) ;
#48862 = DIRECTION ( 'NONE',  ( 0.000000000000000000, 0.000000000000000000, 1.000000000000000000 ) ) ;
#48863 = ORIENTED_EDGE ( 'NONE', *, *, #21031, .F. ) ;
#48864 = CARTESIAN_POINT ( 'NONE',  ( 21.09922568453595559, 22.04030133659708923, -6.408140936763230044 ) ) ;
#48865 = CARTESIAN_POINT ( 'NONE',  ( -0.8801773607111009756, 38.06368534415484106, 1.068504757029289695E-15 ) ) ;
#48866 = VERTEX_POINT ( 'NONE', #36490 ) ;
#48867 = CARTESIAN_POINT ( 'NONE',  ( 2.791683348922240793, 66.63393115100079456, 7.208316651077764092 ) ) ;
#48869 = CARTESIAN_POINT ( 'NONE',  ( 7.361572987183170547, 57.05059781766744464, 9.846743663894590881 ) ) ;
#48868 = CARTESIAN_POINT ( 'NONE',  ( 14.92337183194729633, 12.67559781766745353, 8.527530157486181039 ) ) ;
#48870 = CARTESIAN_POINT ( 'NONE',  ( -8.108506836784059146, -3.139057133285344303, 3.750000000000000888 ) ) ;
#48871 = CARTESIAN_POINT ( 'NONE',  ( 18.52753015748618282, 33.92559781766745886, -4.923371831947291888 ) ) ;
#48872 = DIRECTION ( 'NONE',  ( 1.000000000000000000, 0.000000000000000000, 0.000000000000000000 ) ) ;
#48873 = VECTOR ( 'NONE', #92585, 1000.000000000000000 ) ;
#48874 = AXIS2_PLACEMENT_3D ( 'NONE', #61676, #31675, #40176 ) ;
#48875 = CARTESIAN_POINT ( 'NONE',  ( -13.14228782657330896, 14.63595249122789177, -7.230509711182420141 ) ) ;
#48877 = SURFACE_STYLE_USAGE ( .BOTH. , #70420 ) ;
#48876 = CARTESIAN_POINT ( 'NONE',  ( 12.63842701281683034, 27.46726448433411250, 9.846743663894596210 ) ) ;
#48878 = FACE_OUTER_BOUND ( 'NONE', #28591, .T. ) ;
#48880 = EDGE_LOOP ( 'NONE', ( #90888, #71693, #33860, #83048 ) ) ;
#48879 = CARTESIAN_POINT ( 'NONE',  ( 14.92337183194729988, 59.34226448433412315, -8.527530157486177487 ) ) ;
#48881 = DIRECTION ( 'NONE',  ( -2.569960705150826877E-16, 1.000000000000000000, 0.000000000000000000 ) ) ;
#48882 = EDGE_CURVE ( 'NONE', #21081, #12912, #72257, .T. ) ;
#48883 = CARTESIAN_POINT ( 'NONE',  ( 3.591859063236761518, 24.95696800326375353, 11.09922568453594849 ) ) ;
#48884 = CARTESIAN_POINT ( 'NONE',  ( 19.84674366389459266, 48.71726448433413026, -2.638427012816827677 ) ) ;
#48885 = DIRECTION ( 'NONE',  ( 1.000000000000000000, 0.000000000000000000, -0.000000000000000000 ) ) ;
#48886 = CARTESIAN_POINT ( 'NONE',  ( 17.08211943468705840, 40.13708216824731068, -12.26659068614894466 ) ) ;
#48887 = CARTESIAN_POINT ( 'NONE',  ( 0.1532563361054100626, 15.80059781766745353, -2.638427012816831230 ) ) ;
#48888 = ADVANCED_FACE ( 'NONE', ( #12984 ), #51379, .T. ) ;
#48889 = VECTOR ( 'NONE', #64445, 1000.000000000000000 ) ;
#48890 = LINE ( 'NONE', #28362, #20083 ) ;
#48891 = CARTESIAN_POINT ( 'NONE',  ( -2.266590686148945544, 52.22041550158064638, 7.082119434687048631 ) ) ;
#48892 = CARTESIAN_POINT ( 'NONE',  ( 2.791683348922240793, 61.63393115100079456, 7.208316651077764092 ) ) ;
#48893 = CARTESIAN_POINT ( 'NONE',  ( -0.8801773607111008646, 8.272018677488171434, 2.915334737309923430 ) ) ;
#48894 = CARTESIAN_POINT ( 'NONE',  ( 13.79529636645031943, 40.34541550158063217, -14.16423886937409904 ) ) ;
#48896 = CARTESIAN_POINT ( 'NONE',  ( 17.39651004071897589, 34.08210964143323451, -6.499999999999361400 ) ) ;
#48895 = CARTESIAN_POINT ( 'NONE',  ( 24.16423886937410614, 44.51208216824730357, -3.795296366450302550 ) ) ;
#48897 = CARTESIAN_POINT ( 'NONE',  ( 66.76470751278411342, 40.99999999999997868, 9.500000000000000000 ) ) ;
#48898 = PRODUCT_DEFINITION ( 'UNKNOWN', '', #75905, #27487 ) ;
#48900 = CARTESIAN_POINT ( 'NONE',  ( 0.1532563361054082862, 51.21726448433412315, 2.638427012816831674 ) ) ;
#48899 = PLANE ( 'NONE',  #86765 ) ;
#48901 = ORIENTED_EDGE ( 'NONE', *, *, #55426, .T. ) ;
#48902 = CARTESIAN_POINT ( 'NONE',  ( 10.00000000000000000, 41.81368534415484106, -10.88017736071110342 ) ) ;
#48903 = DIRECTION ( 'NONE',  ( 0.000000000000000000, 0.000000000000000000, -1.000000000000000000 ) ) ;
#48904 = CARTESIAN_POINT ( 'NONE',  ( 1.042145700049408319, 64.74216108172002748, -6.499999999999931610 ) ) ;
#48905 = DIRECTION ( 'NONE',  ( 0.000000000000000000, 0.000000000000000000, -1.000000000000000000 ) ) ;
#48906 = CARTESIAN_POINT ( 'NONE',  ( 10.36894250292378850, -0.07125116508603752952, -10.36894250292379027 ) ) ;
#48907 = CARTESIAN_POINT ( 'NONE',  ( 5.076628168052703671, 61.84226448433412315, 8.527530157486179263 ) ) ;
#48908 = CARTESIAN_POINT ( 'NONE',  ( -41.94000000000001194, 93.50000000000000000, -10.09898361729590199 ) ) ;
#48909 = TOROIDAL_SURFACE ( 'NONE', #87234, 14.49999999999999822, 0.5000000000000000000 ) ;
#48910 = VERTEX_POINT ( 'NONE', #69943 ) ;
#48911 = CARTESIAN_POINT ( 'NONE',  ( 2.917880565312950480, 25.97041550158063572, -12.26659068614894821 ) ) ;
#48912 =( GEOMETRIC_REPRESENTATION_CONTEXT ( 3 ) GLOBAL_UNCERTAINTY_ASSIGNED_CONTEXT ( ( #94510 ) ) GLOBAL_UNIT_ASSIGNED_CONTEXT ( ( #13087, #49596, #80105 ) ) REPRESENTATION_CONTEXT ( 'NONE', 'WORKASPACE' ) );
#48913 = LINE ( 'NONE', #17458, #82178 ) ;
#48915 = CARTESIAN_POINT ( 'NONE',  ( 19.42250999205614193, 45.14701867748817676, 5.440088680355555262 ) ) ;
#48914 = CARTESIAN_POINT ( 'NONE',  ( -6.867320125558078914, -58.36821204062274404, -2.750000000000000000 ) ) ;
#48916 = CARTESIAN_POINT ( 'NONE',  ( 19.42250999205614548, 20.98035201082150891, -5.440088680355545492 ) ) ;
#48917 = CARTESIAN_POINT ( 'NONE',  ( 3.591859063236761518, 24.95696800326375353, 11.09922568453594849 ) ) ;
#48918 = DIRECTION ( 'NONE',  ( 0.000000000000000000, 0.000000000000000000, 1.000000000000000000 ) ) ;
#48919 = CARTESIAN_POINT ( 'NONE',  ( 1.472469842513823179, 15.59226448433411960, -4.923371831947296329 ) ) ;
#48920 = CARTESIAN_POINT ( 'NONE',  ( 20.15039907845753575, 59.72266099184918176, 6.262539305110074395 ) ) ;
#48921 = CARTESIAN_POINT ( 'NONE',  ( 2.603489959281199972, 21.58210964143324873, 6.499999999999559464 ) ) ;
#48922 = DIRECTION ( 'NONE',  ( 0.000000000000000000, -1.000000000000000000, 0.000000000000000000 ) ) ;
#48923 = CARTESIAN_POINT ( 'NONE',  ( 0.5774900079438590739, 7.647018677488171434, -5.440088680355550821 ) ) ;
#48924 = CARTESIAN_POINT ( 'NONE',  ( 12.83294900548066053, 0.3639312116172450096, -7.766300266068392411 ) ) ;
#48925 = CARTESIAN_POINT ( 'NONE',  ( 17.96484262340118221, 36.18868534415484106, -7.964842623401177768 ) ) ;
#48926 = CARTESIAN_POINT ( 'NONE',  ( -0.8801773607111008646, 33.27201867748817676, 2.915334737309923430 ) ) ;
#48927 = CARTESIAN_POINT ( 'NONE',  ( 3.591859063236763294, 3.290301336597087012, -11.09922568453595026 ) ) ;
#48928 = CARTESIAN_POINT ( 'NONE',  ( 4.999999999999999112, 61.00000000000000000, 6.500000000000000888 ) ) ;
#48929 = CARTESIAN_POINT ( 'NONE',  ( -2.816281873526473856, 59.12363466993042493, 9.499525473075851096E-16 ) ) ;
#48930 = CARTESIAN_POINT ( 'NONE',  ( 12.63842701281683922, 9.550597817667449974, -9.846743663894590881 ) ) ;
#48931 = EDGE_LOOP ( 'NONE', ( #62481, #26037, #40826, #33775 ) ) ;
#48932 = CARTESIAN_POINT ( 'NONE',  ( 12.91533473730992121, 29.52201867748817321, 10.88017736071110164 ) ) ;
#48933 = CARTESIAN_POINT ( 'NONE',  ( -1.099225684535947600, 33.70696800326375353, -6.408140936763238038 ) ) ;
#48934 = CIRCLE ( 'NONE', #50507, 0.5000000000000004441 ) ;
#48935 = VECTOR ( 'NONE', #76458, 1000.000000000000000 ) ;
#48936 = CIRCLE ( 'NONE', #95251, 14.49999999999999822 ) ;
#48937 = CARTESIAN_POINT ( 'NONE',  ( 0.1532563361054083140, 56.00893115100078745, 1.131784320476157264E-15 ) ) ;
#48938 = CARTESIAN_POINT ( 'NONE',  ( 2.035157376598822676, 67.43868534415484817, -7.964842623401177768 ) ) ;
#48939 = CARTESIAN_POINT ( 'NONE',  ( 0.1532563361054083140, 6.008931151000784787, 1.131784320476157264E-15 ) ) ;
#48940 = CARTESIAN_POINT ( 'NONE',  ( -2.816281873526473856, 29.12363466993041783, 9.499525473075851096E-16 ) ) ;
#48942 = LINE ( 'NONE', #3949, #11247 ) ;
#48941 = CARTESIAN_POINT ( 'NONE',  ( 7.361572987183169658, 4.967264484334119601, -9.846743663894592657 ) ) ;
#48943 = ORIENTED_EDGE ( 'NONE', *, *, #47163, .T. ) ;
#48944 = SURFACE_STYLE_FILL_AREA ( #56936 ) ;
#48945 = DIRECTION ( 'NONE',  ( -1.000000000000000000, -0.000000000000000000, -0.000000000000000000 ) ) ;
#48946 = CARTESIAN_POINT ( 'NONE',  ( 2.035157376598822676, 2.438685344154837953, -7.964842623401177768 ) ) ;
#48948 = CARTESIAN_POINT ( 'NONE',  ( 10.00000000000000000, 25.55374883491396787, -14.16423886937410082 ) ) ;
#48947 = CARTESIAN_POINT ( 'NONE',  ( -2.816281873526473856, 64.33196800326376774, 3.434112377981055619 ) ) ;
#48949 = CARTESIAN_POINT ( 'NONE',  ( 18.52753015748618282, 18.92559781766745175, -4.923371831947291888 ) ) ;
#48950 = CARTESIAN_POINT ( 'NONE',  ( 7.084665262690076126, 7.022018677488169658, -10.88017736071110164 ) ) ;
#48951 = CARTESIAN_POINT ( 'NONE',  ( 12.63842701281683034, 27.46726448433411250, 9.846743663894596210 ) ) ;
#48952 = CARTESIAN_POINT ( 'NONE',  ( 2.035157376598824452, 3.688685344154837953, 7.964842623401179544 ) ) ;
#48953 = VERTEX_POINT ( 'NONE', #67974 ) ;
#48954 = AXIS2_PLACEMENT_3D ( 'NONE', #39667, #62628, #4495 ) ;
#48955 = CARTESIAN_POINT ( 'NONE',  ( 17.96484262340118221, 9.938685344154837509, 7.964842623401181321 ) ) ;
#48956 = CARTESIAN_POINT ( 'NONE',  ( 15.44008868035555260, 14.73035201082150536, 9.422509992056143702 ) ) ;
#48957 = CARTESIAN_POINT ( 'NONE',  ( -45.94000000000000483, 92.00000000000000000, 5.000000000000000000 ) ) ;
#48958 = ORIENTED_EDGE ( 'NONE', *, *, #81770, .F. ) ;
#48959 = CARTESIAN_POINT ( 'NONE',  ( 12.74305857943745046, -3.163668057994810583E-15, 7.177950183686947483 ) ) ;
#48960 = CARTESIAN_POINT ( 'NONE',  ( 4.559911319644449179, 28.89701867748817321, 9.422509992056141925 ) ) ;
#48961 = CARTESIAN_POINT ( 'NONE',  ( 10.00000000000000178, 62.25893115100078745, 9.846743663894594434 ) ) ;
#48962 = CYLINDRICAL_SURFACE ( 'NONE', #39454, 11.25000000000000178 ) ;
#48963 = CARTESIAN_POINT ( 'NONE',  ( 3.591859063236763294, 48.29030133659708923, -11.09922568453595026 ) ) ;
#48964 = LINE ( 'NONE', #10973, #25308 ) ;
#48965 = CARTESIAN_POINT ( 'NONE',  ( 24.16423886937409904, 34.09541550158064638, 3.795296366450317205 ) ) ;
#48966 = CARTESIAN_POINT ( 'NONE',  ( 12.91533473730992121, 34.52201867748817676, 10.88017736071110164 ) ) ;
#48968 = B_SPLINE_CURVE_WITH_KNOTS ( 'NONE', 3,
 ( #76383, #37910, #75890, #63209, #7898, #6904 ),
 .UNSPECIFIED., .F., .F.,
 ( 4, 2, 4 ),
 ( 3.409110551494651432E-05, 0.0004400426677367925347, 0.0008459942299586384806 ),
 .UNSPECIFIED. ) ;
#48967 = CARTESIAN_POINT ( 'NONE',  ( 15.44008868035555793, 11.39701867748817143, -9.422509992056140149 ) ) ;
#48969 = CARTESIAN_POINT ( 'NONE',  ( 0.1532563361054082862, 51.21726448433412315, 2.638427012816831674 ) ) ;
#48970 = AXIS2_PLACEMENT_3D ( 'NONE', #97561, #30504, #29024 ) ;
#48971 = CARTESIAN_POINT ( 'NONE',  ( 18.72515096720590577, 61.07228050351029935, -6.499999999999718447 ) ) ;
#48972 = CARTESIAN_POINT ( 'NONE',  ( 5.076628168052703671, 36.84226448433412315, 8.527530157486179263 ) ) ;
#48973 = CARTESIAN_POINT ( 'NONE',  ( 0.000000000000000000, 14.49999999999999822, 0.000000000000000000 ) ) ;
#48974 = CARTESIAN_POINT ( 'NONE',  ( 14.92337183194729988, 14.34226448433411782, -8.527530157486177487 ) ) ;
#48975 = CARTESIAN_POINT ( 'NONE',  ( 3.469446951953614189E-15, -29.62636533006957862, 12.81628187352647608 ) ) ;
#48976 = ORIENTED_EDGE ( 'NONE', *, *, #88312, .F. ) ;
#48977 = CARTESIAN_POINT ( 'NONE',  ( -0.8801773607111009756, 18.06368534415484106, 1.068504757029289695E-15 ) ) ;
#48978 = CARTESIAN_POINT ( 'NONE',  ( 18.52753015748618282, 8.925597817667451750, -4.923371831947291888 ) ) ;
#48979 = CARTESIAN_POINT ( 'NONE',  ( 19.38216949554541202, 0.9986346699304200492, 9.382169495545424454 ) ) ;
#48980 = CARTESIAN_POINT ( 'NONE',  ( 20.88017736071110164, 50.35535201082151247, 2.915334737309930979 ) ) ;
#48982 = CARTESIAN_POINT ( 'NONE',  ( 22.81628187352648496, 41.83196800326375353, -3.434112377981050290 ) ) ;
#48981 = CARTESIAN_POINT ( 'NONE',  ( 19.42250999205614193, 20.14701867748817321, 5.440088680355555262 ) ) ;
#48983 = CARTESIAN_POINT ( 'NONE',  ( 13.79529636645030344, 28.26208216824729647, 14.16423886937410614 ) ) ;
#48984 = EDGE_CURVE ( 'NONE', #82368, #79612, #55778, .T. ) ;
#48985 = CYLINDRICAL_SURFACE ( 'NONE', #68223, 15.00000000000000000 ) ;
#48986 = PRESENTATION_LAYER_ASSIGNMENT (  '', '', ( #18657 ) ) ;
#48988 = CARTESIAN_POINT ( 'NONE',  ( 10.00000000000000000, 52.87363466993041783, -12.81628187352647608 ) ) ;
#48987 = VECTOR ( 'NONE', #84681, 1000.000000000000000 ) ;
#48989 = ORIENTED_EDGE ( 'NONE', *, *, #2579, .T. ) ;
#48990 = CARTESIAN_POINT ( 'NONE',  ( 14.92337183194729988, 64.34226448433412315, -8.527530157486177487 ) ) ;
#48991 = CARTESIAN_POINT ( 'NONE',  ( 4.559911319644449179, 37.23035201082150536, -9.422509992056141925 ) ) ;
#48992 = EDGE_LOOP ( 'NONE', ( #67602, #69193, #54762, #15144 ) ) ;
#48994 = CARTESIAN_POINT ( 'NONE',  ( -3.271887613349916180, -0.8417457659429956607, 2.500000000000000888 ) ) ;
#48993 = CARTESIAN_POINT ( 'NONE',  ( 10.00000000000000000, -0.2410688489992152128, -9.846743663894594434 ) ) ;
#48995 = CARTESIAN_POINT ( 'NONE',  ( 8.879999999999991900, 27.04366094290857347, 2.900000000000000355 ) ) ;
#48996 = CARTESIAN_POINT ( 'NONE',  ( 12.63842701281683034, 27.46726448433411250, 9.846743663894596210 ) ) ;
#48997 = CARTESIAN_POINT ( 'NONE',  ( 17.20831665107776587, 9.133931151000787452, -7.208316651077762316 ) ) ;
#48998 = CARTESIAN_POINT ( 'NONE',  ( 0.1532563361054100626, 0.8005978176674514168, -2.638427012816831230 ) ) ;
#49001 = LINE ( 'NONE', #94499, #93487 ) ;
#49000 = VECTOR ( 'NONE', #93527, 1000.000000000000000 ) ;
#48999 = CARTESIAN_POINT ( 'NONE',  ( 4.559911319644449179, 58.89701867748817676, 9.422509992056141925 ) ) ;
#49002 = CARTESIAN_POINT ( 'NONE',  ( 7.084665262690076126, 59.10535201082150536, 10.88017736071109987 ) ) ;
#49004 = ORIENTED_EDGE ( 'NONE', *, *, #29174, .T. ) ;
#49003 = CARTESIAN_POINT ( 'NONE',  ( 10.00000000000000000, 24.75893115100078745, -9.846743663894594434 ) ) ;
#49005 = CIRCLE ( 'NONE', #7496, 0.5000000000000004441 ) ;
#49006 = CARTESIAN_POINT ( 'NONE',  ( 5.815488105659666118, 14.76984994604921475, 13.76235181012722286 ) ) ;
#49008 = EDGE_CURVE ( 'NONE', #84748, #59823, #92920, .T. ) ;
#49007 =( GEOMETRIC_REPRESENTATION_CONTEXT ( 3 ) GLOBAL_UNCERTAINTY_ASSIGNED_CONTEXT ( ( #71465 ) ) GLOBAL_UNIT_ASSIGNED_CONTEXT ( ( #89494, #14498, #44969 ) ) REPRESENTATION_CONTEXT ( 'NONE', 'WORKASPACE' ) );
#49009 = CARTESIAN_POINT ( 'NONE',  ( 14.92337183194729988, 54.34226448433412315, -8.527530157486177487 ) ) ;
#49010 = ORIENTED_EDGE ( 'NONE', *, *, #48034, .T. ) ;
#49011 = CARTESIAN_POINT ( 'NONE',  ( -12.22506292814027873, 14.76930270348881002, 8.589871424854626625 ) ) ;
#49012 = CARTESIAN_POINT ( 'NONE',  ( -0.3689425029237898834, 11.17874883491396787, -10.36894250292378850 ) ) ;
#49013 = DIRECTION ( 'NONE',  ( 0.000000000000000000, 0.000000000000000000, -1.000000000000000000 ) ) ;
#49014 = CARTESIAN_POINT ( 'NONE',  ( -4.164238869374099927, 2.012082168247300906, 3.795296366450308767 ) ) ;
#49015 = CARTESIAN_POINT ( 'NONE',  ( 24.16423886937409904, 39.09541550158062506, 3.795296366450317205 ) ) ;
#49016 = CARTESIAN_POINT ( 'NONE',  ( -0.03447792253739288132, 45.15514106990688958, 6.401564815979726930 ) ) ;
#49017 = DIRECTION ( 'NONE',  ( 0.9970872288863208421, 0.07626964003977952655, -0.000000000000000000 ) ) ;
#49018 = CARTESIAN_POINT ( 'NONE',  ( 0.5774900079438590739, 37.64701867748817676, -5.440088680355550821 ) ) ;
#49019 = SURFACE_SIDE_STYLE ('',( #94518 ) ) ;
#49020 = ORIENTED_EDGE ( 'NONE', *, *, #88474, .F. ) ;
#49021 = CARTESIAN_POINT ( 'NONE',  ( 0.1532563361054100626, 10.80059781766745175, -2.638427012816831230 ) ) ;
#49022 = COLOUR_RGB ( '', 0.72549020, 0.75294118, 0.79215686) ;
#49024 = CARTESIAN_POINT ( 'NONE',  ( 10.00000000000000178, 12.25893115100078568, 9.846743663894594434 ) ) ;
#49023 = CARTESIAN_POINT ( 'NONE',  ( 2.035157376598824452, 58.68868534415482685, 7.964842623401179544 ) ) ;
#49025 = CARTESIAN_POINT ( 'NONE',  ( 16.40814093676324603, 42.45696800326375353, -11.09922568453594671 ) ) ;
#49026 = CARTESIAN_POINT ( 'NONE',  ( 10.00000000000000178, 37.25893115100078745, 9.846743663894594434 ) ) ;
#49027 = DIRECTION ( 'NONE',  ( -0.000000000000000000, -1.000000000000000000, -4.683753385137374737E-14 ) ) ;
#49028 = CARTESIAN_POINT ( 'NONE',  ( 20.88017736071110519, 60.56368534415484106, 2.639326808657452039E-16 ) ) ;
#49029 = CARTESIAN_POINT ( 'NONE',  ( 12.63842701281683034, 22.46726448433411605, 9.846743663894596210 ) ) ;
#49030 = CARTESIAN_POINT ( 'NONE',  ( 6.565887622018943937, 28.08196800326375353, -12.81628187352647608 ) ) ;
#49031 = CARTESIAN_POINT ( 'NONE',  ( 14.16423886937410259, -35.69625116508602503, -2.602085213965210642E-15 ) ) ;
#49032 = STYLED_ITEM ( 'NONE', ( #70958 ), #40953 ) ;
#49033 = CARTESIAN_POINT ( 'NONE',  ( 2.791683348922240793, 26.63393115100078745, 7.208316651077764092 ) ) ;
#49034 = CARTESIAN_POINT ( 'NONE',  ( -0.3689425029237898834, 11.17874883491396787, -10.36894250292378850 ) ) ;
#49035 = VERTEX_POINT ( 'NONE', #75957 ) ;
#49036 = CIRCLE ( 'NONE', #2817, 11.25000000000000178 ) ;
#49037 = CARTESIAN_POINT ( 'NONE',  ( 4.559911319644449179, 38.89701867748817676, 9.422509992056141925 ) ) ;
#49038 = CARTESIAN_POINT ( 'NONE',  ( -0.8801773607110991993, 57.85535201082149825, -2.915334737309923874 ) ) ;
#49039 = CARTESIAN_POINT ( 'NONE',  ( 13.79529636645031943, 35.34541550158063927, -14.16423886937409904 ) ) ;
#49040 = CARTESIAN_POINT ( 'NONE',  ( 17.20831665107776587, 54.13393115100079456, -7.208316651077762316 ) ) ;
#49041 = CARTESIAN_POINT ( 'NONE',  ( 14.92337183194729633, 12.67559781766745353, 8.527530157486181039 ) ) ;
#49043 = CARTESIAN_POINT ( 'NONE',  ( -9.402796353260967521, 15.00000000000000000, -11.68706210897770248 ) ) ;
#49042 = CARTESIAN_POINT ( 'NONE',  ( 22.81628187352648496, 61.83196800326376774, -3.434112377981050290 ) ) ;
#49044 = CARTESIAN_POINT ( 'NONE',  ( 15.44008868035555260, 39.73035201082150536, 9.422509992056143702 ) ) ;
#49045 = CARTESIAN_POINT ( 'NONE',  ( -6.767445849361338972, 0.3639308223168559175, 13.38662304974495854 ) ) ;
#49046 = EDGE_CURVE ( 'NONE', #4379, #67947, #61930, .T. ) ;
#49047 = CARTESIAN_POINT ( 'NONE',  ( 6.565887622018943937, 18.08196800326375708, -12.81628187352647608 ) ) ;
#49048 = CARTESIAN_POINT ( 'NONE',  ( 0.6178305044545818747, 18.49863466993041428, -9.382169495545419124 ) ) ;
#49049 = CARTESIAN_POINT ( 'NONE',  ( 12.63842701281683922, 54.55059781766745175, -9.846743663894590881 ) ) ;
#49050 = CARTESIAN_POINT ( 'NONE',  ( -10.88017736071110164, 17.85535201082151247, -2.915334737309917212 ) ) ;
#49051 = PRESENTATION_STYLE_ASSIGNMENT (( #33538 ) ) ;
#49053 = LINE ( 'NONE', #43389, #31841 ) ;
#49052 = CARTESIAN_POINT ( 'NONE',  ( 12.91533473730993009, 66.60535201082150536, -10.88017736071109987 ) ) ;
#49054 = EDGE_CURVE ( 'NONE', #2122, #18620, #50568, .T. ) ;
#49055 = CARTESIAN_POINT ( 'NONE',  ( 0.000000000000000000, 15.00000000000000000, 0.000000000000000000 ) ) ;
#49056 = PLANE ( 'NONE',  #75187 ) ;
#49057 = CARTESIAN_POINT ( 'NONE',  ( 0.5774900079438607392, 63.48035201082149825, 5.440088680355550821 ) ) ;
#49058 = CARTESIAN_POINT ( 'NONE',  ( 4.559911319644449179, 62.23035201082150536, -9.422509992056141925 ) ) ;
#49059 = FACE_OUTER_BOUND ( 'NONE', #53771, .T. ) ;
#49060 = CARTESIAN_POINT ( 'NONE',  ( 8.731067818237036704, 11.56330936912750573, 8.731067818237033151 ) ) ;
#49061 = CARTESIAN_POINT ( 'NONE',  ( 14.92337183194729988, 24.34226448433411960, -8.527530157486177487 ) ) ;
#49062 = AXIS2_PLACEMENT_3D ( 'NONE', #63524, #32536, #63034 ) ;
#49063 = CARTESIAN_POINT ( 'NONE',  ( 15.44008868035555793, 21.39701867748817321, -9.422509992056140149 ) ) ;
#49064 = CARTESIAN_POINT ( 'NONE',  ( 18.52753015748618282, 58.92559781766745886, -4.923371831947291888 ) ) ;
#49066 = DIRECTION ( 'NONE',  ( 0.000000000000000000, 0.000000000000000000, -1.000000000000000000 ) ) ;
#49065 = CARTESIAN_POINT ( 'NONE',  ( -0.8801773607111009756, 28.06368534415484106, 1.068504757029289695E-15 ) ) ;
#49067 =( NAMED_UNIT ( * ) PLANE_ANGLE_UNIT ( ) SI_UNIT ( $, .RADIAN. ) );
#49068 = CARTESIAN_POINT ( 'NONE',  ( 3.591859063236763294, 38.29030133659708923, -11.09922568453595026 ) ) ;
#49069 = ORIENTED_EDGE ( 'NONE', *, *, #66975, .T. ) ;
#49070 = CARTESIAN_POINT ( 'NONE',  ( 19.42250999205614548, 50.98035201082151247, -5.440088680355545492 ) ) ;
#49071 = CARTESIAN_POINT ( 'NONE',  ( 0.6178305044545838731, 14.74863466993041783, 9.382169495545420901 ) ) ;
#49072 = CARTESIAN_POINT ( 'NONE',  ( 15.44008868035555793, 26.39701867748817321, -9.422509992056140149 ) ) ;
#49073 = CARTESIAN_POINT ( 'NONE',  ( 10.00000000000000000, 55.55374883491396787, -14.16423886937410082 ) ) ;
#49074 = AXIS2_PLACEMENT_3D ( 'NONE', #39555, #85535, #25535 ) ;
#49075 = CARTESIAN_POINT ( 'NONE',  ( 7.361572987183169658, 34.96726448433411605, -9.846743663894592657 ) ) ;
#49076 = CARTESIAN_POINT ( 'NONE',  ( 18.52753015748618282, 3.925597817667451306, -4.923371831947291888 ) ) ;
#49077 = CARTESIAN_POINT ( 'NONE',  ( 0.5774900079438607392, 43.48035201082151247, 5.440088680355550821 ) ) ;
#49078 = CARTESIAN_POINT ( 'NONE',  ( -5.448048636097846398, 0.000000000000000000, 0.2378669404634123075 ) ) ;
#49079 = CARTESIAN_POINT ( 'NONE',  ( 2.917880565312950480, 10.97041550158063572, -12.26659068614894821 ) ) ;
#49080 = COLOUR_RGB ( '', 0.08235294, 0.09019608, 0.10196078) ;
#49081 = AXIS2_PLACEMENT_3D ( 'NONE', #63865, #64847, #70417 ) ;
#49082 = PRESENTATION_STYLE_ASSIGNMENT (( #18589 ) ) ;
#49083 = DIRECTION ( 'NONE',  ( 0.06975647374412544122, 0.9975640502598241977, -0.000000000000000000 ) ) ;
#49084 = ORIENTED_EDGE ( 'NONE', *, *, #64872, .T. ) ;
#49085 = CARTESIAN_POINT ( 'NONE',  ( -0.3689425029237898834, 46.17874883491397497, -10.36894250292378850 ) ) ;
#49086 = CARTESIAN_POINT ( 'NONE',  ( 24.16423886937409904, 44.09541550158063927, 3.795296366450317205 ) ) ;
#49087 = CARTESIAN_POINT ( 'NONE',  ( 12.63842701281683034, 12.46726448433411782, 9.846743663894596210 ) ) ;
#49088 = CARTESIAN_POINT ( 'NONE',  ( -2.816281873526471635, 13.91530133659708746, -3.434112377981056508 ) ) ;
#49089 = DIRECTION ( 'NONE',  ( -0.000000000000000000, 0.000000000000000000, -1.000000000000000000 ) ) ;
#49090 = CARTESIAN_POINT ( 'NONE',  ( -8.000000000000000000, 1.019547802438466100, 4.000000000000000000 ) ) ;
#49092 = CARTESIAN_POINT ( 'NONE',  ( 10.00000000000000000, 27.87363466993042138, -12.81628187352647608 ) ) ;
#49091 = CARTESIAN_POINT ( 'NONE',  ( 19.42250999205614193, 5.147018677488171434, 5.440088680355555262 ) ) ;
#49093 = CARTESIAN_POINT ( 'NONE',  ( 13.79529636645030344, 38.26208216824729647, 14.16423886937410614 ) ) ;
#49094 = FACE_OUTER_BOUND ( 'NONE', #21069, .T. ) ;
#49095 = CARTESIAN_POINT ( 'NONE',  ( -4.923371831947292776, 1.842264484334124486, 8.527530157486181039 ) ) ;
#49096 = ORIENTED_EDGE ( 'NONE', *, *, #94809, .T. ) ;
#49097 = CARTESIAN_POINT ( 'NONE',  ( 19.84674366389459621, 23.50893115100078390, 7.409399052514197653E-17 ) ) ;
#49098 = CARTESIAN_POINT ( 'NONE',  ( 0.000000000000000000, 14.49999999999999822, 0.000000000000000000 ) ) ;
#49099 = ORIENTED_EDGE ( 'NONE', *, *, #29211, .T. ) ;
#49101 = CARTESIAN_POINT ( 'NONE',  ( 10.00000000000000000, 16.81368534415483751, -10.88017736071110342 ) ) ;
#49100 = CARTESIAN_POINT ( 'NONE',  ( -4.164238869374098151, 66.59541550158060375, -3.795296366450310543 ) ) ;
#49103 = CARTESIAN_POINT ( 'NONE',  ( 6.565887622018943937, 8.081968003263751754, -12.81628187352647608 ) ) ;
#49102 = CARTESIAN_POINT ( 'NONE',  ( 1.472469842513823179, 45.59226448433412315, -4.923371831947296329 ) ) ;
#49104 = DIRECTION ( 'NONE',  ( 0.000000000000000000, -1.000000000000000000, 0.000000000000000000 ) ) ;
#49105 = CARTESIAN_POINT ( 'NONE',  ( -9.876730923139437124, 14.49999999999999112, 11.28938378619059613 ) ) ;
#49106 = EDGE_CURVE ( 'NONE', #31960, #94230, #65318, .T. ) ;
#49107 = B_SPLINE_CURVE_WITH_KNOTS ( 'NONE', 3,
 ( #98269, #16218, #98766, #259, #36756, #60720 ),
 .UNSPECIFIED., .F., .F.,
 ( 4, 2, 4 ),
 ( 0.0002800170536516726491, 0.0006862224498868382903, 0.001092427846122004040 ),
 .UNSPECIFIED. ) ;
#49108 = B_SPLINE_CURVE_WITH_KNOTS ( 'NONE', 3,
 ( #55303, #63772, #61817, #48290, #39336, #85813 ),
 .UNSPECIFIED., .F., .F.,
 ( 4, 2, 4 ),
 ( 3.409110551496102908E-05, 0.0004400426677367863006, 0.0008459942299586115924 ),
 .UNSPECIFIED. ) ;
#49109 = CARTESIAN_POINT ( 'NONE',  ( 6.565887622018943937, 25.16530133659708213, 12.81628187352647430 ) ) ;
#49110 = CIRCLE ( 'NONE', #61879, 0.5000000000000004441 ) ;
#49111 = ORIENTED_EDGE ( 'NONE', *, *, #22611, .T. ) ;
#49112 = CARTESIAN_POINT ( 'NONE',  ( -4.164238869374099039, 61.80374883491397497, 8.674139862899312516E-16 ) ) ;
#49113 = EDGE_LOOP ( 'NONE', ( #17220, #60703, #74745, #74846 ) ) ;
#49114 = CARTESIAN_POINT ( 'NONE',  ( 22.26659068614894466, 58.88708216824729647, 7.082119434687054849 ) ) ;
#49115 = VERTEX_POINT ( 'NONE', #491 ) ;
#49116 = CARTESIAN_POINT ( 'NONE',  ( 4.559911319644449179, 33.89701867748817676, 9.422509992056141925 ) ) ;
#49117 = CARTESIAN_POINT ( 'NONE',  ( 17.96484262340118221, 51.18868534415483396, -7.964842623401177768 ) ) ;
#49118 = CARTESIAN_POINT ( 'NONE',  ( 4.559911319644449179, 42.23035201082151247, -9.422509992056141925 ) ) ;
#49119 = CARTESIAN_POINT ( 'NONE',  ( -10.09048698379360687, 46.92328126389585208, 0.000000000000000000 ) ) ;
#49120 = CARTESIAN_POINT ( 'NONE',  ( 2.035157376598822676, 37.43868534415484106, -7.964842623401177768 ) ) ;
#49122 = COLOUR_RGB ( '', 0.08235294, 0.09019608, 0.10196078) ;
#49121 = CARTESIAN_POINT ( 'NONE',  ( 4.999999999999999112, 11.50000000000000000, 6.000000000000000000 ) ) ;
#49123 = EDGE_CURVE ( 'NONE', #85384, #28167, #58226, .T. ) ;
#49124 = CARTESIAN_POINT ( 'NONE',  ( 12.63842701281683922, 9.550597817667449974, -9.846743663894590881 ) ) ;
#49125 = EDGE_LOOP ( 'NONE', ( #92532, #5608, #45637, #41370, #39629, #61755 ) ) ;
#49126 = CARTESIAN_POINT ( 'NONE',  ( 11.01504402823088213, -96.09667835297135241, 4.000000000000000000 ) ) ;
#49127 = CARTESIAN_POINT ( 'NONE',  ( 19.84674366389459266, 48.71726448433413026, -2.638427012816827677 ) ) ;
#49128 = CARTESIAN_POINT ( 'NONE',  ( 10.00000000000000178, 70.00000000000000000, 0.000000000000000000 ) ) ;
#49129 = CARTESIAN_POINT ( 'NONE',  ( -1.099225684535947600, 59.54030133659708923, 6.408140936763237150 ) ) ;
#49130 = ADVANCED_FACE ( 'NONE', ( #71427 ), #18038, .T. ) ;
#49131 =( NAMED_UNIT ( * ) PLANE_ANGLE_UNIT ( ) SI_UNIT ( $, .RADIAN. ) );
#49132 = VECTOR ( 'NONE', #67680, 1000.000000000000000 ) ;
#49133 = LINE ( 'NONE', #11623, #58769 ) ;
#49134 = FILL_AREA_STYLE_COLOUR ( '', #83347 ) ;
#49135 = CARTESIAN_POINT ( 'NONE',  ( 22.26659068614895176, 59.72041550158063927, -7.082119434687042414 ) ) ;
#49136 = DIRECTION ( 'NONE',  ( 0.000000000000000000, 1.000000000000000000, 0.000000000000000000 ) ) ;
#49137 = ORIENTED_EDGE ( 'NONE', *, *, #64795, .F. ) ;
#49138 = DIRECTION ( 'NONE',  ( -1.000000000000000000, 0.000000000000000000, 0.000000000000000000 ) ) ;
#49139 = CARTESIAN_POINT ( 'NONE',  ( 12.63842701281683034, 27.46726448433411250, 9.846743663894596210 ) ) ;
#49140 = AXIS2_PLACEMENT_3D ( 'NONE', #50882, #51372, #5877 ) ;
#49141 = FILL_AREA_STYLE_COLOUR ( '', #80250 ) ;
#49142 = CARTESIAN_POINT ( 'NONE',  ( -1.099225684535947600, 4.540301336597087456, 6.408140936763237150 ) ) ;
#49143 = CARTESIAN_POINT ( 'NONE',  ( 7.084665262690076126, 67.02201867748817676, -10.88017736071110164 ) ) ;
#49144 = AXIS2_PLACEMENT_3D ( 'NONE', #17206, #88014, #9193 ) ;
#49145 = SURFACE_SIDE_STYLE ('',( #79646 ) ) ;
#49146 = CARTESIAN_POINT ( 'NONE',  ( 2.791683348922237240, 55.38393115100078745, -7.208316651077763204 ) ) ;
#49147 = AXIS2_PLACEMENT_3D ( 'NONE', #78115, #9623, #70623 ) ;
#49148 = CARTESIAN_POINT ( 'NONE',  ( 0.4400000000000020006, 1.019547802438468986, 2.750000000000000000 ) ) ;
#49149 = ORIENTED_EDGE ( 'NONE', *, *, #47254, .F. ) ;
#49150 = CARTESIAN_POINT ( 'NONE',  ( 2.035157376598822676, 2.438685344154838397, -7.964842623401177768 ) ) ;
#49151 = DIRECTION ( 'NONE',  ( -1.000000000000000000, 0.000000000000000000, 0.000000000000000000 ) ) ;
#49152 = CARTESIAN_POINT ( 'NONE',  ( 20.88017736071110164, 40.35535201082150536, 2.915334737309930979 ) ) ;
#49154 = CARTESIAN_POINT ( 'NONE',  ( 7.084665262690076126, 69.10535201082151957, 10.88017736071109987 ) ) ;
#49153 = CARTESIAN_POINT ( 'NONE',  ( -1.099225684535947600, 9.540301336597087456, 6.408140936763237150 ) ) ;
#49155 = CARTESIAN_POINT ( 'NONE',  ( 2.035157376598824452, 3.688685344154837953, 7.964842623401179544 ) ) ;
#49156 = LINE ( 'NONE', #41187, #96486 ) ;
#49157 = FACE_OUTER_BOUND ( 'NONE', #78924, .T. ) ;
#49158 = CARTESIAN_POINT ( 'NONE',  ( 0.1532563361054083140, 46.00893115100079456, 1.131784320476157264E-15 ) ) ;
#49159 = CARTESIAN_POINT ( 'NONE',  ( 17.20831665107776587, 19.13393115100078035, -7.208316651077762316 ) ) ;
#49160 = CARTESIAN_POINT ( 'NONE',  ( 5.440088680355556150, -20.26964798917849109, 9.422509992056138373 ) ) ;
#49161 = CARTESIAN_POINT ( 'NONE',  ( -2.816281873526473856, 19.33196800326375708, 3.434112377981055619 ) ) ;
#49162 = CARTESIAN_POINT ( 'NONE',  ( -11.37644997975658612, -81.99697149686846842, -4.000000000000000000 ) ) ;
#49163 = CARTESIAN_POINT ( 'NONE',  ( 19.42250999205614193, 30.14701867748817321, 5.440088680355555262 ) ) ;
#49164 = FACE_OUTER_BOUND ( 'NONE', #7805, .T. ) ;
#49165 = CARTESIAN_POINT ( 'NONE',  ( 2.917880565312950480, 30.97041550158063572, -12.26659068614894821 ) ) ;
#49166 = ADVANCED_FACE ( 'NONE', ( #71895 ), #16940, .F. ) ;
#49167 = CARTESIAN_POINT ( 'NONE',  ( -2.266590686148945544, 32.22041550158063927, 7.082119434687048631 ) ) ;
#49168 = CARTESIAN_POINT ( 'NONE',  ( 7.084665262690076126, 12.02201867748817321, -10.88017736071110164 ) ) ;
#49169 = CARTESIAN_POINT ( 'NONE',  ( 14.92337183194729633, 47.67559781766745175, 8.527530157486181039 ) ) ;
#49170 = CARTESIAN_POINT ( 'NONE',  ( 3.591859063236761518, 39.95696800326375353, 11.09922568453594849 ) ) ;
#49171 = CARTESIAN_POINT ( 'NONE',  ( 2.035157376598824452, 13.68868534415483751, 7.964842623401179544 ) ) ;
#49172 = CARTESIAN_POINT ( 'NONE',  ( 19.84674366389459266, 33.71726448433410894, -2.638427012816827677 ) ) ;
#49173 = CARTESIAN_POINT ( 'NONE',  ( 17.96484262340118221, 44.93868534415483396, 7.964842623401181321 ) ) ;
#49174 = CARTESIAN_POINT ( 'NONE',  ( 22.81628187352647785, 1.415301336597087012, 3.434112377981063169 ) ) ;
#49175 = CARTESIAN_POINT ( 'NONE',  ( 10.00000000000000178, 28.05374883491396787, 14.16423886937410082 ) ) ;
#49176 = CARTESIAN_POINT ( 'NONE',  ( 14.52844422123120616, 15.00000000000000533, 1.683098224408404953 ) ) ;
#49177 = UNCERTAINTY_MEASURE_WITH_UNIT (LENGTH_MEASURE( 1.000000000000000082E-05 ), #49709, 'distance_accuracy_value', 'NONE');
#49178 = CARTESIAN_POINT ( 'NONE',  ( 2.791683348922240793, 26.63393115100078745, 7.208316651077764092 ) ) ;
#49179 = CARTESIAN_POINT ( 'NONE',  ( -1.099225684535947600, 49.54030133659708923, 6.408140936763237150 ) ) ;
#49180 = CARTESIAN_POINT ( 'NONE',  ( 18.52753015748618282, 48.92559781766745886, -4.923371831947291888 ) ) ;
#49181 = VERTEX_POINT ( 'NONE', #55425 ) ;
#49182 = CARTESIAN_POINT ( 'NONE',  ( -7.750000000000000000, 41.24999999999999289, 6.250000000000000000 ) ) ;
#49183 = CARTESIAN_POINT ( 'NONE',  ( 2.917880565312948704, 67.63708216824730357, 12.26659068614894643 ) ) ;
#49184 = CARTESIAN_POINT ( 'NONE',  ( 10.00000000000000000, 61.81368534415484106, -10.88017736071110342 ) ) ;
#49185 = CARTESIAN_POINT ( 'NONE',  ( 2.917880565312948704, 7.637082168247301794, 12.26659068614894643 ) ) ;
#49186 = CARTESIAN_POINT ( 'NONE',  ( 0.1532563361054083140, 1.008931151000784787, 1.131784320476157264E-15 ) ) ;
#49187 = CARTESIAN_POINT ( 'NONE',  ( 10.00000000000000178, 47.25893115100078745, 9.846743663894594434 ) ) ;
#49188 = CARTESIAN_POINT ( 'NONE',  ( 19.42250999205614193, 30.14701867748817321, 5.440088680355555262 ) ) ;
#49189 = DIRECTION ( 'NONE',  ( 0.7253743710122775301, 0.000000000000000000, 0.6883545756937645699 ) ) ;
#49190 = CARTESIAN_POINT ( 'NONE',  ( 7.361572987183169658, 59.96726448433410894, -9.846743663894592657 ) ) ;
#49191 = ORIENTED_EDGE ( 'NONE', *, *, #59021, .T. ) ;
#49192 = CIRCLE ( 'NONE', #95522, 14.49999999999999822 ) ;
#49193 = CARTESIAN_POINT ( 'NONE',  ( -4.838527690343428667, 0.3640475087720985714, -14.19819177887734440 ) ) ;
#49194 = EDGE_LOOP ( 'NONE', ( #49228, #33881, #88814, #87263 ) ) ;
#49195 = ORIENTED_EDGE ( 'NONE', *, *, #11090, .F. ) ;
#49196 = DIRECTION ( 'NONE',  ( 0.000000000000000000, 1.000000000000000000, 0.000000000000000000 ) ) ;
#49197 = CARTESIAN_POINT ( 'NONE',  ( 2.917880565312948704, 7.637082168247301794, 12.26659068614894643 ) ) ;
#49198 = CARTESIAN_POINT ( 'NONE',  ( -2.266590686148945544, 16.38708216824730357, -7.082119434687050408 ) ) ;
#49199 = CARTESIAN_POINT ( 'NONE',  ( 0.1532563361054082862, 56.21726448433411605, 2.638427012816831674 ) ) ;
#49200 = CARTESIAN_POINT ( 'NONE',  ( 18.52753015748618282, 28.92559781766745175, -4.923371831947291888 ) ) ;
#49201 = CARTESIAN_POINT ( 'NONE',  ( 13.21236992757673789, -0.03417435944610275333, -5.338143956176714333 ) ) ;
#49203 = CARTESIAN_POINT ( 'NONE',  ( 0.1532563361054082862, 61.21726448433412315, 2.638427012816831674 ) ) ;
#49202 = CARTESIAN_POINT ( 'NONE',  ( 2.035157376598824452, 28.68868534415484106, 7.964842623401179544 ) ) ;
#49204 = CARTESIAN_POINT ( 'NONE',  ( 22.26659068614895176, 9.720415501580633943, -7.082119434687042414 ) ) ;
#49205 = CARTESIAN_POINT ( 'NONE',  ( 17.96484262340118221, 9.938685344154839285, 7.964842623401181321 ) ) ;
#49206 = DIRECTION ( 'NONE',  ( 0.06104853953486361756, 0.000000000000000000, -0.9981347984218665870 ) ) ;
#49207 = DIRECTION ( 'NONE',  ( -1.000000000000000000, -0.000000000000000000, -0.000000000000000000 ) ) ;
#49208 = CARTESIAN_POINT ( 'NONE',  ( 20.88017736071110164, 60.35535201082151957, 2.915334737309930979 ) ) ;
#49209 = CARTESIAN_POINT ( 'NONE',  ( 7.361572987183169658, 24.96726448433412315, -9.846743663894592657 ) ) ;
#49210 = AXIS2_PLACEMENT_3D ( 'NONE', #19093, #49573, #94594 ) ;
#49211 = CARTESIAN_POINT ( 'NONE',  ( 4.923371831947295441, -35.65773551566588395, -8.527530157486179263 ) ) ;
#49212 = EDGE_LOOP ( 'NONE', ( #5981, #36887, #78123, #28849, #61727, #56850, #34958, #5855, #45551, #65645, #29300, #46769, #79222, #39151, #18105, #53188, #35885, #66189, #79100, #87696, #76216, #58014, #75188, #66074, #29128, #61472, #31711, #23186, #21552, #65353, #60934, #63444, #92607, #76911, #56354, #74956, #6605, #77629, #33846, #83139, #16928, #8213, #20055, #83658, #39547, #38497, #53676, #42634, #6670, #63503, #17534, #84547, #55624, #88661, #80082, #28307, #76874, #73675, #96683, #20123, #74635, #16675, #40498, #45750, #28076, #61746, #43806, #7568, #54693, #24386, #34429, #50116, #44290, #84091, #70761, #47056, #46571, #90073, #51529, #92287, #91915, #39529, #46297, #2616, #87362, #80452, #53664, #89593, #30070, #16992, #20952, #81086, #48976, #41592, #32021, #8260, #74436, #92659, #13816, #71245, #93978, #74774, #92770, #15901, #90895, #47219, #91885, #38419, #4512, #68305 ) ) ;
#49213 = ORIENTED_EDGE ( 'NONE', *, *, #11408, .F. ) ;
#49214 = CARTESIAN_POINT ( 'NONE',  ( 14.92337183194729988, 24.34226448433411960, -8.527530157486177487 ) ) ;
#49215 = ORIENTED_EDGE ( 'NONE', *, *, #14952, .T. ) ;
#49216 = CARTESIAN_POINT ( 'NONE',  ( -0.3689425029237898834, 31.17874883491396787, -10.36894250292378850 ) ) ;
#49217 = CARTESIAN_POINT ( 'NONE',  ( 2.791683348922240793, 36.63393115100078035, 7.208316651077764092 ) ) ;
#49218 = CARTESIAN_POINT ( 'NONE',  ( 7.084665262690076126, 59.10535201082150536, 10.88017736071109987 ) ) ;
#49219 = VECTOR ( 'NONE', #28288, 1000.000000000000114 ) ;
#49220 = DIRECTION ( 'NONE',  ( -0.8526401643540884034, 0.000000000000000000, -0.5224985647159552382 ) ) ;
#49221 = EDGE_CURVE ( 'NONE', #15093, #95449, #93034, .T. ) ;
#49222 = CIRCLE ( 'NONE', #63619, 14.49999999999999822 ) ;
#49223 = CARTESIAN_POINT ( 'NONE',  ( 17.96484262340118221, 44.93868534415483396, 7.964842623401181321 ) ) ;
#49224 = CARTESIAN_POINT ( 'NONE',  ( 14.92337183194729633, 47.67559781766745175, 8.527530157486181039 ) ) ;
#49225 = EDGE_CURVE ( 'NONE', #91084, #95857, #86695, .T. ) ;
#49226 = EDGE_CURVE ( 'NONE', #26337, #97969, #81971, .T. ) ;
#49227 = CARTESIAN_POINT ( 'NONE',  ( -3.434112377981047626, -9.834698663402914320, 12.81628187352647963 ) ) ;
#49228 = ORIENTED_EDGE ( 'NONE', *, *, #76771, .T. ) ;
#49229 = CARTESIAN_POINT ( 'NONE',  ( -0.3689425029237898834, 21.17874883491396432, -10.36894250292378850 ) ) ;
#49230 = VERTEX_POINT ( 'NONE', #18413 ) ;
#49231 = ORIENTED_EDGE ( 'NONE', *, *, #63487, .T. ) ;
#49232 = CARTESIAN_POINT ( 'NONE',  ( 3.591859063236761518, 34.95696800326375353, 11.09922568453594849 ) ) ;
#49233 = SURFACE_SIDE_STYLE ('',( #40758 ) ) ;
#49234 = CARTESIAN_POINT ( 'NONE',  ( 7.361572987183169658, 24.96726448433412315, -9.846743663894592657 ) ) ;
#49235 = CARTESIAN_POINT ( 'NONE',  ( -0.8801773607110991993, 2.855352010821504471, -2.915334737309923874 ) ) ;
#49236 = CARTESIAN_POINT ( 'NONE',  ( 3.591859063236763294, 58.29030133659708923, -11.09922568453595026 ) ) ;
#49237 = CARTESIAN_POINT ( 'NONE',  ( 14.92337183194729988, 24.34226448433411960, -8.527530157486177487 ) ) ;
#49239 = ORIENTED_EDGE ( 'NONE', *, *, #10295, .F. ) ;
#49238 = CARTESIAN_POINT ( 'NONE',  ( 4.559911319644449179, 57.23035201082150536, -9.422509992056141925 ) ) ;
#49240 = ADVANCED_FACE ( 'NONE', ( #17925 ), #70936, .T. ) ;
#49241 = DIRECTION ( 'NONE',  ( 0.000000000000000000, 1.000000000000000000, 0.000000000000000000 ) ) ;
#49242 = CARTESIAN_POINT ( 'NONE',  ( 7.084665262690076126, 69.10535201082151957, 10.88017736071109987 ) ) ;
#49243 = CARTESIAN_POINT ( 'NONE',  ( -44.17147705133852043, 106.3134523618952869, 4.660915905273111726 ) ) ;
#49244 = CARTESIAN_POINT ( 'NONE',  ( -8.000000000000000000, 40.74999999999999289, -4.250000000000000000 ) ) ;
#49245 = CARTESIAN_POINT ( 'NONE',  ( 2.791683348922240793, 1.633931151000784565, 7.208316651077764092 ) ) ;
#49246 = CARTESIAN_POINT ( 'NONE',  ( 22.81628187352648496, 16.83196800326374998, -3.434112377981050290 ) ) ;
#49247 = EDGE_CURVE ( 'NONE', #32664, #57881, #77924, .T. ) ;
#49248 = SURFACE_SIDE_STYLE ('',( #43215 ) ) ;
#49249 = VECTOR ( 'NONE', #2355, 1000.000000000000000 ) ;
#49250 = CARTESIAN_POINT ( 'NONE',  ( 19.84674366389459266, 43.71726448433410894, -2.638427012816827677 ) ) ;
#49251 = CYLINDRICAL_SURFACE ( 'NONE', #28146, 1.999999999999996669 ) ;
#49252 = CARTESIAN_POINT ( 'NONE',  ( 20.36894250292379382, 8.678748834913967869, 10.36894250292379205 ) ) ;
#49253 = CARTESIAN_POINT ( 'NONE',  ( 10.00000000000000000, 29.75893115100078745, -9.846743663894594434 ) ) ;
#49254 =( BOUNDED_SURFACE ( )  B_SPLINE_SURFACE ( 1, 2, ( 
 ( #32251, #78255, #71261, #33719, #93256, #24780, #55256, #64668, #72187, #42203, #94703, #79204, #12179, #4204, #42685, #27671, #58157, #41718, #95690, #88667, #50173, #41231, #87680, #71709, #63697, #56222, #3221, #27174, #94200, #3716, #19194, #49676, #80683, #64182, #49197, #26208, #35166, #33685, #79700, #10714, #34177, #20175, #56700, #95179, #11197, #73164, #25731, #87191, #34674, #48700, #80181, #40722, #65170, #57677, #4703, #18714, #26687, #65666, #96188, #57183, #11694, #72669, #18220, #88172, #50679, #10230, #19686, #71224, #2748, #33202, #86716, #90634, #73659, #5186, #20676, #60136, #89658, #98677, #7153, #59151, #51671, #74653, #59649, #29629, #6654, #21168, #37170, #68155, #98173, #60631, #90140, #82149, #97681, #22158, #43661, #13661, #44143, #6164, #52641, #21670, #66666, #83145, #37657, #35673, #52155, #36668, #67156, #14165, #29143, #30126, #51170, #74147, #14670, #82648, #28659, #91133, #45136, #44649, #66156, #75144, #67663, #75642, #22658, #81171, #12671, #43171, #96690, #5680, #28169, #58663, #89165, #81654, #13163, #36165, #97191, #77112, #16626, #15159, #63095, #23653, #31608, #46616, #38635, #40111, #8626, #32094, #47610, #45639, #2139, #78105, #24628, #54114, #170, #39135, #70613, #665, #8143, #85614, #9611, #53628, #69624, #84627, #93595, #53135, #91635, #62593, #38154, #46137, #84146, #23153, #17131, #1147, #92609, #16130, #92127, #32597, #24134, #15654, #62100, #83644, #76136, #7663, #54601, #93098, #85117, #47103, #68641, #55094, #30619, #77602, #61126, #9116, #39630, #70120, #1642, #76623, #69137, #31115, #61610, #79588, #86108, #72556, #73052, #57073, #80069, #17619, #87569, #2635, #18592, #3115, #87081, #33088, #79085, #57559, #94091, #63582, #65047, #42089, #33571, #49085, #86600, #4585, #11088, #19081, #65547, #41606, #48089, #26570, #71602, #80570, #35047, #3601, #25612, #34552, #48584, #56105, #18107, #10598, #64065, #42568, #25133, #94580, #26096, #95573, #27060, #41112, #88057, #78601, #10111, #56591, #4088, #72075, #55611, #50067, #34060, #64556, #95064, #49556, #19569, #11575, #12065, #40610, #71107, #14053, #75528, #6055, #74037, #13548, #44535, #58544, #5569, #28549, #21056, #75031, #74534, #81538, #98058, #22053, #88554, #67043, #51549, #36045, #29029, #82037, #90031, #44032, #7041, #20057, #97077, #37047, #43542, #66549, #89051, #52527, #97565, #59041, #50560, #66044, #96571, #83035, #28048, #20562, #51048, #82534, #5068, #73543, #89547, #36553, #6538, #35555, #59537, #21554, #52044, #13048, #67545, #29515, #60023, #90518, #14552, #45021, #37546, #96073, #27554, #58047, #81055 ),
 ( #12559, #43062, #77989, #70007, #30017, #39018, #45520, #16014, #54009, #558, #31003, #38041, #24022, #85005, #7551, #23536, #60521, #16517, #17008, #1029, #54490, #91012, #31490, #76020, #61499, #46029, #92007, #68532, #23038, #1531, #31976, #61993, #53015, #84518, #69513, #92493, #46504, #47486, #39514, #68037, #77003, #30510, #46992, #77486, #8516, #8998, #62, #62482, #92986, #24520, #54978, #22545, #9494, #38527, #85497, #98563, #53511, #83530, #15048, #61013, #91524, #84022, #15544, #76513, #8029, #69024, #70500, #93483, #78482, #32485, #62979, #47973, #39995, #25009, #55496, #85997, #2022, #17508, #73639, #14149, #20157, #28151, #66139, #5167, #98156, #28641, #74636, #5664, #74127, #60119, #6148, #35653, #89640, #52626, #96170, #14654, #36146, #44633, #21151, #97174, #45118, #37151, #27653, #36650, #12653, #82132, #51652, #66650, #59131, #96671, #90125, #52138, #58648, #13641, #58140, #82633, #83127, #67138, #21653, #88649, #97662, #43151, #44126, #13145, #29129, #89146, #20657, #67647, #51152, #81637, #75129, #6635, #43642, #59630, #29614, #75626, #90618, #22142, #35147, #65646, #50660, #81149, #53610, #62579, #55080, #84613, #76120, #16611, #30606, #7649, #38140, #85599, #45623, #68627, #47089, #16115, #84128, #17113, #24613, #68138, #47596, #8126, #77585, #61595, #69121, #7138, #9101, #98664, #77099, #83629, #54098, #92108, #38620, #652, #157, #62087, #24118, #61111, #23639, #30112, #54587, #37640, #39119, #92594, #60618, #69609, #15145, #31101, #15639, #46600, #91620, #23137, #39615, #46122, #76609, #70104, #85102, #8611, #1130, #31592, #91117, #1629, #32078, #22640, #93083, #53121, #79573, #25597, #34535, #27045, #56576, #48072, #87555, #2617, #78585, #10096, #57543, #17602, #40594, #19065, #87067, #56090, #88042, #80054, #41593, #63078, #71588, #11072, #72060, #18577, #19554, #49544, #78090, #33554, #71091, #3587, #49070, #34045, #95049, #33072, #11557, #41091, #3100, #64541, #40097, #9593, #48566, #26556, #64052, #63568, #65029, #94564, #57053, #72538, #70597, #2123, #4072, #42077, #79067, #25114, #26082, #95556, #86582, #94076, #32582, #93579, #18091, #55596, #10581, #86091, #50050, #88539, #29012, #35030, #43045, #81037, #20041, #14038, #43526, #89531, #20546, #89035, #75016, #21040, #50543, #5551, #67527, #98044, #81524, #36539, #29500, #90015, #12544, #28531, #73525, #4568, #96055, #5053, #67028, #65532, #13032, #59025, #51530, #21535, #35536, #51031, #66029, #6521, #96557, #74022, #28032, #36029, #60008, #58527, #66531, #97058, #52028, #27539, #82022, #44016, #13533, #74519, #80553, #6039, #97550 ) ),
 .UNSPECIFIED., .F., .F., .T. ) 
 B_SPLINE_SURFACE_WITH_KNOTS ( ( 2, 2 ),
 ( 3, 2, 2, 2, 2, 2, 2, 2, 2, 2, 2, 2, 2, 2, 2, 2, 2, 2, 2, 2, 2, 2, 2, 2, 2, 2, 2, 2, 2, 2, 2, 2, 2, 2, 2, 2, 2, 2, 2, 2, 2, 2, 2, 2, 2, 2, 2, 2, 2, 2, 2, 2, 2, 2, 2, 2, 2, 2, 2, 2, 2, 2, 2, 2, 2, 2, 2, 2, 2, 2, 2, 2, 2, 2, 2, 2, 2, 2, 2, 2, 2, 2, 2, 2, 2, 2, 2, 2, 2, 2, 2, 2, 2, 2, 2, 2, 2, 2, 2, 2, 2, 2, 2, 2, 2, 2, 2, 2, 2, 2, 2, 2, 2, 2, 2, 2, 2, 2, 2, 2, 2, 2, 2, 2, 2, 2, 2, 2, 2, 2, 2, 2, 2, 2, 2, 2, 2, 2, 2, 2, 2, 2, 2, 2, 2, 2, 2, 2, 2, 2, 2, 2, 2, 2, 2, 2, 2, 2, 2, 2, 2, 2, 3 ),
 ( 0.000000000000000000, 1.000000000000000000 ),
 ( 0.000000000000000000, 0.005952380952380952051, 0.01190476190476190410, 0.01785714285714285615, 0.02380952380952380820, 0.02976190476190476025, 0.03571428571428571230, 0.04166666666666666435, 0.04761904761904761640, 0.05357142857142856845, 0.05952380952380952051, 0.06547619047619047949, 0.07142857142857142461, 0.07738095238095238360, 0.08333333333333332871, 0.08928571428571428770, 0.09523809523809523281, 0.1011904761904761918, 0.1071428571428571369, 0.1130952380952380959, 0.1190476190476190410, 0.1250000000000000000, 0.1309523809523809590, 0.1369047619047619180, 0.1428571428571428492, 0.1488095238095238082, 0.1547619047619047672, 0.1607142857142857262, 0.1666666666666666574, 0.1726190476190476164, 0.1785714285714285754, 0.1845238095238095344, 0.1904761904761904656, 0.1964285714285714246, 0.2023809523809523836, 0.2083333333333333426, 0.2142857142857142738, 0.2202380952380952328, 0.2261904761904761918, 0.2321428571428571508, 0.2380952380952380820, 0.2440476190476190410, 0.2500000000000000000, 0.2559523809523809312, 0.2619047619047619180, 0.2678571428571428492, 0.2738095238095238360, 0.2797619047619047672, 0.2857142857142856984, 0.2916666666666666852, 0.2976190476190476164, 0.3035714285714285476, 0.3095238095238095344, 0.3154761904761904656, 0.3214285714285714524, 0.3273809523809523836, 0.3333333333333333148, 0.3392857142857143016, 0.3452380952380952328, 0.3511904761904761640, 0.3571428571428571508, 0.3630952380952380820, 0.3690476190476190688, 0.3750000000000000000, 0.3809523809523809312, 0.3869047619047619180, 0.3928571428571428492, 0.3988095238095238360, 0.4047619047619047672, 0.4107142857142856984, 0.4166666666666666852, 0.4226190476190476164, 0.4285714285714285476, 0.4345238095238095344, 0.4404761904761904656, 0.4464285714285714524, 0.4523809523809523836, 0.4583333333333333148, 0.4642857142857143016, 0.4702380952380952328, 0.4761904761904761640, 0.4821428571428571508, 0.4880952380952380820, 0.4940476190476190688, 0.5000000000000000000, 0.5059523809523809312, 0.5119047619047618625, 0.5178571428571429047, 0.5238095238095238360, 0.5297619047619047672, 0.5357142857142856984, 0.5416666666666666297, 0.5476190476190476719, 0.5535714285714286031, 0.5595238095238095344, 0.5654761904761904656, 0.5714285714285713969, 0.5773809523809523281, 0.5833333333333333703, 0.5892857142857143016, 0.5952380952380952328, 0.6011904761904761640, 0.6071428571428570953, 0.6130952380952381375, 0.6190476190476190688, 0.6250000000000000000, 0.6309523809523809312, 0.6369047619047618625, 0.6428571428571429047, 0.6488095238095238360, 0.6547619047619047672, 0.6607142857142856984, 0.6666666666666666297, 0.6726190476190476719, 0.6785714285714286031, 0.6845238095238095344, 0.6904761904761904656, 0.6964285714285713969, 0.7023809523809523281, 0.7083333333333333703, 0.7142857142857143016, 0.7202380952380952328, 0.7261904761904761640, 0.7321428571428570953, 0.7380952380952381375, 0.7440476190476190688, 0.7500000000000000000, 0.7559523809523809312, 0.7619047619047618625, 0.7678571428571429047, 0.7738095238095238360, 0.7797619047619047672, 0.7857142857142856984, 0.7916666666666666297, 0.7976190476190476719, 0.8035714285714286031, 0.8095238095238095344, 0.8154761904761904656, 0.8214285714285713969, 0.8273809523809523281, 0.8333333333333333703, 0.8392857142857143016, 0.8452380952380952328, 0.8511904761904761640, 0.8571428571428570953, 0.8630952380952381375, 0.8690476190476190688, 0.8750000000000000000, 0.8809523809523809312, 0.8869047619047618625, 0.8928571428571429047, 0.8988095238095238360, 0.9047619047619047672, 0.9107142857142856984, 0.9166666666666666297, 0.9226190476190476719, 0.9285714285714286031, 0.9345238095238095344, 0.9404761904761904656, 0.9464285714285713969, 0.9523809523809523281, 0.9583333333333333703, 0.9642857142857143016 ),
 .UNSPECIFIED. ) 
 GEOMETRIC_REPRESENTATION_ITEM ( )  RATIONAL_B_SPLINE_SURFACE ( (
 ( 1.000000000000000000, 0.9659258262890683122, 1.000000000000000000, 0.9659258262890683122, 1.000000000000000000, 0.9659258262890683122, 1.000000000000000000, 0.9659258262890683122, 1.000000000000000000, 0.9659258262890683122, 1.000000000000000000, 0.9659258262890683122, 1.000000000000000000, 0.9659258262890683122, 1.000000000000000000, 0.9659258262890683122, 1.000000000000000000, 0.9659258262890683122, 1.000000000000000000, 0.9659258262890683122, 1.000000000000000000, 0.9659258262890683122, 1.000000000000000000, 0.9659258262890683122, 1.000000000000000000, 0.9659258262890683122, 1.000000000000000000, 0.9659258262890683122, 1.000000000000000000, 0.9659258262890683122, 1.000000000000000000, 0.9659258262890683122, 1.000000000000000000, 0.9659258262890683122, 1.000000000000000000, 0.9659258262890683122, 1.000000000000000000, 0.9659258262890683122, 1.000000000000000000, 0.9659258262890683122, 1.000000000000000000, 0.9659258262890683122, 1.000000000000000000, 0.9659258262890683122, 1.000000000000000000, 0.9659258262890683122, 1.000000000000000000, 0.9659258262890683122, 1.000000000000000000, 0.9659258262890683122, 1.000000000000000000, 0.9659258262890683122, 1.000000000000000000, 0.9659258262890683122, 1.000000000000000000, 0.9659258262890683122, 1.000000000000000000, 0.9659258262890683122, 1.000000000000000000, 0.9659258262890683122, 1.000000000000000000, 0.9659258262890683122, 1.000000000000000000, 0.9659258262890683122, 1.000000000000000000, 0.9659258262890683122, 1.000000000000000000, 0.9659258262890683122, 1.000000000000000000, 0.9659258262890683122, 1.000000000000000000, 0.9659258262890683122, 1.000000000000000000, 0.9659258262890683122, 1.000000000000000000, 0.9659258262890683122, 1.000000000000000000, 0.9659258262890683122, 1.000000000000000000, 0.9659258262890683122, 1.000000000000000000, 0.9659258262890683122, 1.000000000000000000, 0.9659258262890683122, 1.000000000000000000, 0.9659258262890683122, 1.000000000000000000, 0.9659258262890683122, 1.000000000000000000, 0.9659258262890683122, 1.000000000000000000, 0.9659258262890683122, 1.000000000000000000, 0.9659258262890683122, 1.000000000000000000, 0.9659258262890683122, 1.000000000000000000, 0.9659258262890683122, 1.000000000000000000, 0.9659258262890683122, 1.000000000000000000, 0.9659258262890683122, 1.000000000000000000, 0.9659258262890683122, 1.000000000000000000, 0.9659258262890683122, 1.000000000000000000, 0.9659258262890683122, 1.000000000000000000, 0.9659258262890683122, 1.000000000000000000, 0.9659258262890683122, 1.000000000000000000, 0.9659258262890683122, 1.000000000000000000, 0.9659258262890683122, 1.000000000000000000, 0.9659258262890683122, 1.000000000000000000, 0.9659258262890683122, 1.000000000000000000, 0.9659258262890683122, 1.000000000000000000, 0.9659258262890683122, 1.000000000000000000, 0.9659258262890683122, 1.000000000000000000, 0.9659258262890683122, 1.000000000000000000, 0.9659258262890683122, 1.000000000000000000, 0.9659258262890683122, 1.000000000000000000, 0.9659258262890683122, 1.000000000000000000, 0.9659258262890683122, 1.000000000000000000, 0.9659258262890683122, 1.000000000000000000, 0.9659258262890683122, 1.000000000000000000, 0.9659258262890683122, 1.000000000000000000, 0.9659258262890683122, 1.000000000000000000, 0.9659258262890683122, 1.000000000000000000, 0.9659258262890683122, 1.000000000000000000, 0.9659258262890683122, 1.000000000000000000, 0.9659258262890683122, 1.000000000000000000, 0.9659258262890683122, 1.000000000000000000, 0.9659258262890683122, 1.000000000000000000, 0.9659258262890683122, 1.000000000000000000, 0.9659258262890683122, 1.000000000000000000, 0.9659258262890683122, 1.000000000000000000, 0.9659258262890683122, 1.000000000000000000, 0.9659258262890683122, 1.000000000000000000, 0.9659258262890683122, 1.000000000000000000, 0.9659258262890683122, 1.000000000000000000, 0.9659258262890683122, 1.000000000000000000, 0.9659258262890683122, 1.000000000000000000, 0.9659258262890683122, 1.000000000000000000, 0.9659258262890683122, 1.000000000000000000, 0.9659258262890683122, 1.000000000000000000, 0.9659258262890683122, 1.000000000000000000, 0.9659258262890683122, 1.000000000000000000, 0.9659258262890683122, 1.000000000000000000, 0.9659258262890683122, 1.000000000000000000, 0.9659258262890683122, 1.000000000000000000, 0.9659258262890683122, 1.000000000000000000, 0.9659258262890683122, 1.000000000000000000, 0.9659258262890683122, 1.000000000000000000, 0.9659258262890683122, 1.000000000000000000, 0.9659258262890683122, 1.000000000000000000, 0.9659258262890683122, 1.000000000000000000, 0.9659258262890683122, 1.000000000000000000, 0.9659258262890683122, 1.000000000000000000, 0.9659258262890683122, 1.000000000000000000, 0.9659258262890683122, 1.000000000000000000, 0.9659258262890683122, 1.000000000000000000, 0.9659258262890683122, 1.000000000000000000, 0.9659258262890683122, 1.000000000000000000, 0.9659258262890683122, 1.000000000000000000, 0.9659258262890683122, 1.000000000000000000, 0.9659258262890683122, 1.000000000000000000, 0.9659258262890683122, 1.000000000000000000, 0.9659258262890683122, 1.000000000000000000, 0.9659258262890683122, 1.000000000000000000, 0.9659258262890683122, 1.000000000000000000, 0.9659258262890683122, 1.000000000000000000, 0.9659258262890683122, 1.000000000000000000, 0.9659258262890683122, 1.000000000000000000, 0.9659258262890683122, 1.000000000000000000, 0.9659258262890683122, 1.000000000000000000, 0.9659258262890683122, 1.000000000000000000, 0.9659258262890683122, 1.000000000000000000, 0.9659258262890683122, 1.000000000000000000, 0.9659258262890683122, 1.000000000000000000, 0.9659258262890683122, 1.000000000000000000, 0.9659258262890683122, 1.000000000000000000, 0.9659258262890683122, 1.000000000000000000, 0.9659258262890683122, 1.000000000000000000, 0.9659258262890683122, 1.000000000000000000, 0.9659258262890683122, 1.000000000000000000, 0.9659258262890683122, 1.000000000000000000, 0.9659258262890683122, 1.000000000000000000, 0.9659258262890683122, 1.000000000000000000, 0.9659258262890683122, 1.000000000000000000, 0.9659258262890683122, 1.000000000000000000, 0.9659258262890683122, 1.000000000000000000, 0.9659258262890683122, 1.000000000000000000, 0.9659258262890683122, 1.000000000000000000, 0.9659258262890683122, 1.000000000000000000, 0.9659258262890683122, 1.000000000000000000, 0.9659258262890683122, 1.000000000000000000, 0.9659258262890683122, 1.000000000000000000, 0.9659258262890683122, 1.000000000000000000, 0.9659258262890683122, 1.000000000000000000, 0.9659258262890683122, 1.000000000000000000, 0.9659258262890683122, 1.000000000000000000, 0.9659258262890683122, 1.000000000000000000, 0.9659258262890683122, 1.000000000000000000, 0.9659258262890683122, 1.000000000000000000, 0.9659258262890683122, 1.000000000000000000, 0.9659258262890683122, 1.000000000000000000, 0.9659258262890683122, 1.000000000000000000, 0.9659258262890683122, 1.000000000000000000, 0.9659258262890683122, 1.000000000000000000, 0.9659258262890683122, 1.000000000000000000, 0.9659258262890683122, 1.000000000000000000, 0.9659258262890683122, 1.000000000000000000, 0.9659258262890683122, 1.000000000000000000, 0.9659258262890683122, 1.000000000000000000, 0.9659258262890683122, 1.000000000000000000, 0.9659258262890683122, 1.000000000000000000, 0.9659258262890683122, 1.000000000000000000),
 ( 1.000000000000000000, 0.9659258262890683122, 1.000000000000000000, 0.9659258262890683122, 1.000000000000000000, 0.9659258262890683122, 1.000000000000000000, 0.9659258262890683122, 1.000000000000000000, 0.9659258262890683122, 1.000000000000000000, 0.9659258262890683122, 1.000000000000000000, 0.9659258262890683122, 1.000000000000000000, 0.9659258262890683122, 1.000000000000000000, 0.9659258262890683122, 1.000000000000000000, 0.9659258262890683122, 1.000000000000000000, 0.9659258262890683122, 1.000000000000000000, 0.9659258262890683122, 1.000000000000000000, 0.9659258262890683122, 1.000000000000000000, 0.9659258262890683122, 1.000000000000000000, 0.9659258262890683122, 1.000000000000000000, 0.9659258262890683122, 1.000000000000000000, 0.9659258262890683122, 1.000000000000000000, 0.9659258262890683122, 1.000000000000000000, 0.9659258262890683122, 1.000000000000000000, 0.9659258262890683122, 1.000000000000000000, 0.9659258262890683122, 1.000000000000000000, 0.9659258262890683122, 1.000000000000000000, 0.9659258262890683122, 1.000000000000000000, 0.9659258262890683122, 1.000000000000000000, 0.9659258262890683122, 1.000000000000000000, 0.9659258262890683122, 1.000000000000000000, 0.9659258262890683122, 1.000000000000000000, 0.9659258262890683122, 1.000000000000000000, 0.9659258262890683122, 1.000000000000000000, 0.9659258262890683122, 1.000000000000000000, 0.9659258262890683122, 1.000000000000000000, 0.9659258262890683122, 1.000000000000000000, 0.9659258262890683122, 1.000000000000000000, 0.9659258262890683122, 1.000000000000000000, 0.9659258262890683122, 1.000000000000000000, 0.9659258262890683122, 1.000000000000000000, 0.9659258262890683122, 1.000000000000000000, 0.9659258262890683122, 1.000000000000000000, 0.9659258262890683122, 1.000000000000000000, 0.9659258262890683122, 1.000000000000000000, 0.9659258262890683122, 1.000000000000000000, 0.9659258262890683122, 1.000000000000000000, 0.9659258262890683122, 1.000000000000000000, 0.9659258262890683122, 1.000000000000000000, 0.9659258262890683122, 1.000000000000000000, 0.9659258262890683122, 1.000000000000000000, 0.9659258262890683122, 1.000000000000000000, 0.9659258262890683122, 1.000000000000000000, 0.9659258262890683122, 1.000000000000000000, 0.9659258262890683122, 1.000000000000000000, 0.9659258262890683122, 1.000000000000000000, 0.9659258262890683122, 1.000000000000000000, 0.9659258262890683122, 1.000000000000000000, 0.9659258262890683122, 1.000000000000000000, 0.9659258262890683122, 1.000000000000000000, 0.9659258262890683122, 1.000000000000000000, 0.9659258262890683122, 1.000000000000000000, 0.9659258262890683122, 1.000000000000000000, 0.9659258262890683122, 1.000000000000000000, 0.9659258262890683122, 1.000000000000000000, 0.9659258262890683122, 1.000000000000000000, 0.9659258262890683122, 1.000000000000000000, 0.9659258262890683122, 1.000000000000000000, 0.9659258262890683122, 1.000000000000000000, 0.9659258262890683122, 1.000000000000000000, 0.9659258262890683122, 1.000000000000000000, 0.9659258262890683122, 1.000000000000000000, 0.9659258262890683122, 1.000000000000000000, 0.9659258262890683122, 1.000000000000000000, 0.9659258262890683122, 1.000000000000000000, 0.9659258262890683122, 1.000000000000000000, 0.9659258262890683122, 1.000000000000000000, 0.9659258262890683122, 1.000000000000000000, 0.9659258262890683122, 1.000000000000000000, 0.9659258262890683122, 1.000000000000000000, 0.9659258262890683122, 1.000000000000000000, 0.9659258262890683122, 1.000000000000000000, 0.9659258262890683122, 1.000000000000000000, 0.9659258262890683122, 1.000000000000000000, 0.9659258262890683122, 1.000000000000000000, 0.9659258262890683122, 1.000000000000000000, 0.9659258262890683122, 1.000000000000000000, 0.9659258262890683122, 1.000000000000000000, 0.9659258262890683122, 1.000000000000000000, 0.9659258262890683122, 1.000000000000000000, 0.9659258262890683122, 1.000000000000000000, 0.9659258262890683122, 1.000000000000000000, 0.9659258262890683122, 1.000000000000000000, 0.9659258262890683122, 1.000000000000000000, 0.9659258262890683122, 1.000000000000000000, 0.9659258262890683122, 1.000000000000000000, 0.9659258262890683122, 1.000000000000000000, 0.9659258262890683122, 1.000000000000000000, 0.9659258262890683122, 1.000000000000000000, 0.9659258262890683122, 1.000000000000000000, 0.9659258262890683122, 1.000000000000000000, 0.9659258262890683122, 1.000000000000000000, 0.9659258262890683122, 1.000000000000000000, 0.9659258262890683122, 1.000000000000000000, 0.9659258262890683122, 1.000000000000000000, 0.9659258262890683122, 1.000000000000000000, 0.9659258262890683122, 1.000000000000000000, 0.9659258262890683122, 1.000000000000000000, 0.9659258262890683122, 1.000000000000000000, 0.9659258262890683122, 1.000000000000000000, 0.9659258262890683122, 1.000000000000000000, 0.9659258262890683122, 1.000000000000000000, 0.9659258262890683122, 1.000000000000000000, 0.9659258262890683122, 1.000000000000000000, 0.9659258262890683122, 1.000000000000000000, 0.9659258262890683122, 1.000000000000000000, 0.9659258262890683122, 1.000000000000000000, 0.9659258262890683122, 1.000000000000000000, 0.9659258262890683122, 1.000000000000000000, 0.9659258262890683122, 1.000000000000000000, 0.9659258262890683122, 1.000000000000000000, 0.9659258262890683122, 1.000000000000000000, 0.9659258262890683122, 1.000000000000000000, 0.9659258262890683122, 1.000000000000000000, 0.9659258262890683122, 1.000000000000000000, 0.9659258262890683122, 1.000000000000000000, 0.9659258262890683122, 1.000000000000000000, 0.9659258262890683122, 1.000000000000000000, 0.9659258262890683122, 1.000000000000000000, 0.9659258262890683122, 1.000000000000000000, 0.9659258262890683122, 1.000000000000000000, 0.9659258262890683122, 1.000000000000000000, 0.9659258262890683122, 1.000000000000000000, 0.9659258262890683122, 1.000000000000000000, 0.9659258262890683122, 1.000000000000000000, 0.9659258262890683122, 1.000000000000000000, 0.9659258262890683122, 1.000000000000000000, 0.9659258262890683122, 1.000000000000000000, 0.9659258262890683122, 1.000000000000000000, 0.9659258262890683122, 1.000000000000000000, 0.9659258262890683122, 1.000000000000000000, 0.9659258262890683122, 1.000000000000000000, 0.9659258262890683122, 1.000000000000000000, 0.9659258262890683122, 1.000000000000000000, 0.9659258262890683122, 1.000000000000000000, 0.9659258262890683122, 1.000000000000000000, 0.9659258262890683122, 1.000000000000000000, 0.9659258262890683122, 1.000000000000000000, 0.9659258262890683122, 1.000000000000000000, 0.9659258262890683122, 1.000000000000000000, 0.9659258262890683122, 1.000000000000000000, 0.9659258262890683122, 1.000000000000000000, 0.9659258262890683122, 1.000000000000000000, 0.9659258262890683122, 1.000000000000000000, 0.9659258262890683122, 1.000000000000000000, 0.9659258262890683122, 1.000000000000000000, 0.9659258262890683122, 1.000000000000000000, 0.9659258262890683122, 1.000000000000000000, 0.9659258262890683122, 1.000000000000000000, 0.9659258262890683122, 1.000000000000000000, 0.9659258262890683122, 1.000000000000000000, 0.9659258262890683122, 1.000000000000000000, 0.9659258262890683122, 1.000000000000000000, 0.9659258262890683122, 1.000000000000000000, 0.9659258262890683122, 1.000000000000000000, 0.9659258262890683122, 1.000000000000000000, 0.9659258262890683122, 1.000000000000000000) ) ) 
 REPRESENTATION_ITEM ( '' )  SURFACE ( )  );
#49255 = CARTESIAN_POINT ( 'NONE',  ( 13.43411237798106583, 27.66530133659708568, -12.81628187352647252 ) ) ;
#49257 = CARTESIAN_POINT ( 'NONE',  ( -4.000000000000000000, 78.07179676972445748, -6.250000000000000000 ) ) ;
#49256 = CARTESIAN_POINT ( 'NONE',  ( -14.15369600240084225, 7.013432803265604835E-16, -3.689340892730420762 ) ) ;
#49258 = CARTESIAN_POINT ( 'NONE',  ( 0.5774900079438590739, 67.64701867748817676, -5.440088680355550821 ) ) ;
#49259 = CARTESIAN_POINT ( 'NONE',  ( 3.591859063236763294, 8.290301336597087456, -11.09922568453595026 ) ) ;
#49260 = CARTESIAN_POINT ( 'NONE',  ( 12.63842701281683034, 32.46726448433412315, 9.846743663894596210 ) ) ;
#49261 = CARTESIAN_POINT ( 'NONE',  ( 4.559911319644449179, 27.23035201082150536, -9.422509992056141925 ) ) ;
#49262 = CARTESIAN_POINT ( 'NONE',  ( 19.38216949554541202, 25.99863466993042138, 9.382169495545424454 ) ) ;
#49263 = AXIS2_PLACEMENT_3D ( 'NONE', #44904, #44415, #74919 ) ;
#49264 = CARTESIAN_POINT ( 'NONE',  ( 1.472469842513823179, 26.42559781766745175, 4.923371831947296329 ) ) ;
#49265 = CARTESIAN_POINT ( 'NONE',  ( -12.60874940350953111, 15.00000000000000000, 7.160268045226944267 ) ) ;
#49266 = CARTESIAN_POINT ( 'NONE',  ( 20.88017736071110519, 30.56368534415484106, 2.639326808657452039E-16 ) ) ;
#49267 = EDGE_LOOP ( 'NONE', ( #97057, #73585, #41004, #20101 ) ) ;
#49268 = CARTESIAN_POINT ( 'NONE',  ( 2.035157376598824452, 58.68868534415482685, 7.964842623401179544 ) ) ;
#49270 = CARTESIAN_POINT ( 'NONE',  ( 10.00000000000000000, 31.81368534415483751, -10.88017736071110342 ) ) ;
#49269 = CARTESIAN_POINT ( 'NONE',  ( 14.92337183194729988, 49.34226448433411605, -8.527530157486177487 ) ) ;
#49271 =( NAMED_UNIT ( * ) SI_UNIT ( $, .STERADIAN. ) SOLID_ANGLE_UNIT ( ) );
#49272 = CARTESIAN_POINT ( 'NONE',  ( 4.559911319644449179, 42.23035201082151247, -9.422509992056141925 ) ) ;
#49273 = VECTOR ( 'NONE', #5118, 1000.000000000000000 ) ;
#49275 =( NAMED_UNIT ( * ) SI_UNIT ( $, .STERADIAN. ) SOLID_ANGLE_UNIT ( ) );
#49274 = CARTESIAN_POINT ( 'NONE',  ( -0.8801773607111009756, 18.06368534415484106, 1.068504757029289695E-15 ) ) ;
#49276 = CARTESIAN_POINT ( 'NONE',  ( 5.076628168052704559, 35.17559781766745175, -8.527530157486179263 ) ) ;
#49278 = CARTESIAN_POINT ( 'NONE',  ( -12.00809552683965187, 0.5000000000000004441, 8.989195838243462688 ) ) ;
#49277 = CARTESIAN_POINT ( 'NONE',  ( 10.00000000000000178, 53.05374883491396787, 14.16423886937410082 ) ) ;
#49279 = DIRECTION ( 'NONE',  ( -1.000000000000000000, 0.000000000000000000, 0.000000000000000000 ) ) ;
#49280 = EDGE_CURVE ( 'NONE', #16647, #60661, #65908, .T. ) ;
#49281 = AXIS2_PLACEMENT_3D ( 'NONE', #9780, #54766, #17292 ) ;
#49282 = CARTESIAN_POINT ( 'NONE',  ( 6.204703633549690345, 37.84541550158063927, 14.16423886937410082 ) ) ;
#49283 = CARTESIAN_POINT ( 'NONE',  ( -3.627897631252527511, -3.626520420884125517, 2.750000000000000000 ) ) ;
#49284 = EDGE_LOOP ( 'NONE', ( #47471, #40254, #51689, #83408, #51106, #31274 ) ) ;
#49285 = CARTESIAN_POINT ( 'NONE',  ( -4.164238869374099927, 62.01208216824728936, 3.795296366450308767 ) ) ;
#49286 = CARTESIAN_POINT ( 'NONE',  ( 2.791683348922237240, 35.38393115100079456, -7.208316651077763204 ) ) ;
#49287 = SURFACE_SIDE_STYLE ('',( #71318 ) ) ;
#49288 = CARTESIAN_POINT ( 'NONE',  ( 4.559911319644449179, 53.89701867748817676, 9.422509992056141925 ) ) ;
#49289 = CARTESIAN_POINT ( 'NONE',  ( 0.6178305044545838731, 64.74863466993043914, 9.382169495545420901 ) ) ;
#49290 = CARTESIAN_POINT ( 'NONE',  ( 7.084665262690076126, 27.02201867748817676, -10.88017736071110164 ) ) ;
#49291 = CARTESIAN_POINT ( 'NONE',  ( 16.40814093676324603, 57.45696800326375353, -11.09922568453594671 ) ) ;
#49292 = CARTESIAN_POINT ( 'NONE',  ( 10.00000000000000178, 15.37363466993042138, 12.81628187352647608 ) ) ;
#49293 = CARTESIAN_POINT ( 'NONE',  ( 1.472469842513823179, 15.59226448433411960, -4.923371831947296329 ) ) ;
#49294 = ORIENTED_EDGE ( 'NONE', *, *, #1437, .F. ) ;
#49295 = CARTESIAN_POINT ( 'NONE',  ( 17.62281668512002142, 3.285933195168227794, 6.500000000000010658 ) ) ;
#49296 = CARTESIAN_POINT ( 'NONE',  ( 6.204703633549690345, 62.84541550158063927, 14.16423886937410082 ) ) ;
#49297 = CARTESIAN_POINT ( 'NONE',  ( -2.266590686148945544, 32.22041550158063927, 7.082119434687048631 ) ) ;
#49298 = CARTESIAN_POINT ( 'NONE',  ( 12.91533473730993009, 31.60535201082150891, -10.88017736071109987 ) ) ;
#49299 = CARTESIAN_POINT ( 'NONE',  ( 7.084665262690076126, 44.10535201082151247, 10.88017736071109987 ) ) ;
#49300 = DIRECTION ( 'NONE',  ( 0.000000000000000000, -0.000000000000000000, -1.000000000000000000 ) ) ;
#49301 = SURFACE_STYLE_FILL_AREA ( #95294 ) ;
#49302 = CARTESIAN_POINT ( 'NONE',  ( 17.20831665107776587, 12.88393115100078390, 7.208316651077764980 ) ) ;
#49303 = CARTESIAN_POINT ( 'NONE',  ( 14.92337183194729633, 27.67559781766745530, 8.527530157486181039 ) ) ;
#49304 = FILL_AREA_STYLE ('',( #26307 ) ) ;
#49305 = CARTESIAN_POINT ( 'NONE',  ( 0.000000000000000000, 0.5000000000000004441, 0.000000000000000000 ) ) ;
#49306 = CARTESIAN_POINT ( 'NONE',  ( 19.84674366389459266, 23.71726448433412315, -2.638427012816827677 ) ) ;
#49307 = CARTESIAN_POINT ( 'NONE',  ( 2.791683348922237240, 55.38393115100078745, -7.208316651077763204 ) ) ;
#49308 = CARTESIAN_POINT ( 'NONE',  ( 12.91533473730993009, 21.60535201082150536, -10.88017736071109987 ) ) ;
#49309 = CARTESIAN_POINT ( 'NONE',  ( 22.81628187352647785, 41.41530133659708923, 3.434112377981063169 ) ) ;
#49310 = CARTESIAN_POINT ( 'NONE',  ( 12.91533473730993009, 66.60535201082150536, -10.88017736071109987 ) ) ;
#49311 = CARTESIAN_POINT ( 'NONE',  ( 18.52753015748618282, 33.92559781766745886, -4.923371831947291888 ) ) ;
#49313 = CARTESIAN_POINT ( 'NONE',  ( 2.791683348922237240, 25.38393115100078390, -7.208316651077763204 ) ) ;
#49312 = CARTESIAN_POINT ( 'NONE',  ( 24.16423886937409904, 64.09541550158064638, 3.795296366450317205 ) ) ;
#49314 = CARTESIAN_POINT ( 'NONE',  ( -0.1038446121089033475, 44.24302437010793909, -6.337995344473784876 ) ) ;
#49315 = CARTESIAN_POINT ( 'NONE',  ( 14.92337183194729633, 62.67559781766745886, 8.527530157486181039 ) ) ;
#49316 = CARTESIAN_POINT ( 'NONE',  ( 24.16423886937409904, 4.095415501580634832, 3.795296366450317205 ) ) ;
#49317 = CARTESIAN_POINT ( 'NONE',  ( -0.3689425029237898834, 36.17874883491396787, -10.36894250292378850 ) ) ;
#49318 = CARTESIAN_POINT ( 'NONE',  ( 7.361572987183169658, 34.96726448433411605, -9.846743663894592657 ) ) ;
#49319 = DIRECTION ( 'NONE',  ( -0.9636304532086248376, 0.000000000000000000, 0.2672383760782501838 ) ) ;
#49320 = CARTESIAN_POINT ( 'NONE',  ( 10.00000000000000178, 29.31368534415483751, 10.88017736071110342 ) ) ;
#49321 = CARTESIAN_POINT ( 'NONE',  ( -0.8801773607111009756, 63.06368534415484106, 1.068504757029289695E-15 ) ) ;
#49322 = VECTOR ( 'NONE', #34160, 1000.000000000000000 ) ;
#49323 = ORIENTED_EDGE ( 'NONE', *, *, #7735, .T. ) ;
#49324 = CARTESIAN_POINT ( 'NONE',  ( 6.565887622018943937, 50.16530133659708213, 12.81628187352647430 ) ) ;
#49325 = ADVANCED_FACE ( 'NONE', ( #26890 ), #14839, .T. ) ;
#49326 = CARTESIAN_POINT ( 'NONE',  ( 0.5774900079438607392, 53.48035201082151247, 5.440088680355550821 ) ) ;
#49327 = VERTEX_POINT ( 'NONE', #85432 ) ;
#49328 = CARTESIAN_POINT ( 'NONE',  ( -10.70613742633263321, 15.00000000000000000, 9.778988772285140740 ) ) ;
#49329 = CARTESIAN_POINT ( 'NONE',  ( 20.88017736071110519, 60.56368534415484106, 2.639326808657452039E-16 ) ) ;
#49330 = ORIENTED_EDGE ( 'NONE', *, *, #52075, .T. ) ;
#49332 = EDGE_CURVE ( 'NONE', #65562, #14583, #3366, .T. ) ;
#49331 = CARTESIAN_POINT ( 'NONE',  ( 10.00000000000000178, 59.31368534415484106, 10.88017736071110342 ) ) ;
#49333 = CARTESIAN_POINT ( 'NONE',  ( 7.084665262690076126, 2.022018677488170990, -10.88017736071110164 ) ) ;
#49334 = CARTESIAN_POINT ( 'NONE',  ( 18.52753015748618282, 8.925597817667451750, -4.923371831947291888 ) ) ;
#49335 = CARTESIAN_POINT ( 'NONE',  ( 0.000000000000000000, 35.00000000000000000, -11.92686044187656513 ) ) ;
#49336 = CARTESIAN_POINT ( 'NONE',  ( 0.5774900079438607392, 13.48035201082150358, 5.440088680355550821 ) ) ;
#49337 = CARTESIAN_POINT ( 'NONE',  ( 19.84674366389459266, 3.300597817667451750, 2.638427012816836559 ) ) ;
#49338 = CARTESIAN_POINT ( 'NONE',  ( 22.26659068614895176, 9.720415501580633943, -7.082119434687042414 ) ) ;
#49339 = EDGE_CURVE ( 'NONE', #93548, #70269, #62920, .T. ) ;
#49340 = CARTESIAN_POINT ( 'NONE',  ( 12.63842701281683922, 4.550597817667451750, -9.846743663894590881 ) ) ;
#49341 = CARTESIAN_POINT ( 'NONE',  ( 0.5774900079438607392, 18.48035201082150536, 5.440088680355550821 ) ) ;
#49342 = CARTESIAN_POINT ( 'NONE',  ( 12.63842701281683922, 44.55059781766745175, -9.846743663894590881 ) ) ;
#49343 = EDGE_LOOP ( 'NONE', ( #45935, #67596, #90576, #48698, #23023, #84200 ) ) ;
#49344 = CARTESIAN_POINT ( 'NONE',  ( 7.361572987183169658, 44.96726448433412315, -9.846743663894592657 ) ) ;
#49345 = VERTEX_POINT ( 'NONE', #78416 ) ;
#49346 = DIRECTION ( 'NONE',  ( -0.000000000000000000, 0.000000000000000000, 1.000000000000000000 ) ) ;
#49347 = CARTESIAN_POINT ( 'NONE',  ( 19.42250999205614548, 50.98035201082151247, -5.440088680355545492 ) ) ;
#49348 = CARTESIAN_POINT ( 'NONE',  ( 18.52753015748617571, 53.09226448433412315, 4.923371831947298993 ) ) ;
#49350 = DIRECTION ( 'NONE',  ( -0.000000000000000000, -0.000000000000000000, -1.000000000000000000 ) ) ;
#49349 = CARTESIAN_POINT ( 'NONE',  ( 4.559911319644449179, 8.897018677488171434, 9.422509992056141925 ) ) ;
#49351 = CARTESIAN_POINT ( 'NONE',  ( 2.035157376598822676, 62.43868534415483396, -7.964842623401177768 ) ) ;
#49352 = CARTESIAN_POINT ( 'NONE',  ( -0.8801773607111008646, 8.272018677488171434, 2.915334737309923430 ) ) ;
#49353 = EDGE_CURVE ( 'NONE', #87486, #44443, #10422, .T. ) ;
#49354 = AXIS2_PLACEMENT_3D ( 'NONE', #34079, #64571, #81555 ) ;
#49355 = CARTESIAN_POINT ( 'NONE',  ( 19.38216949554541557, 37.24863466993041783, -9.382169495545420901 ) ) ;
#49356 = CARTESIAN_POINT ( 'NONE',  ( 15.44008868035555260, 29.73035201082150891, 9.422509992056143702 ) ) ;
#49357 = DIRECTION ( 'NONE',  ( 0.000000000000000000, 0.000000000000000000, 1.000000000000000000 ) ) ;
#49358 = VERTEX_POINT ( 'NONE', #48409 ) ;
#49359 = CARTESIAN_POINT ( 'NONE',  ( 16.40814093676324603, 47.45696800326375353, -11.09922568453594671 ) ) ;
#49360 = CARTESIAN_POINT ( 'NONE',  ( 15.44008868035555793, 36.39701867748816966, -9.422509992056140149 ) ) ;
#49362 = ORIENTED_EDGE ( 'NONE', *, *, #17959, .F. ) ;
#49361 = ADVANCED_FACE ( 'NONE', ( #56891 ), #32418, .F. ) ;
#49363 = CARTESIAN_POINT ( 'NONE',  ( 14.92337183194729633, 57.67559781766745886, 8.527530157486181039 ) ) ;
#49365 = CARTESIAN_POINT ( 'NONE',  ( 18.52753015748618282, 48.92559781766745886, -4.923371831947291888 ) ) ;
#49364 = CARTESIAN_POINT ( 'NONE',  ( 1.472469842513823179, 11.42559781766745175, 4.923371831947296329 ) ) ;
#49366 = CARTESIAN_POINT ( 'NONE',  ( -0.8801773607110991993, 27.85535201082150181, -2.915334737309923874 ) ) ;
#49367 = LINE ( 'NONE', #79869, #79448 ) ;
#49368 = CARTESIAN_POINT ( 'NONE',  ( 10.00000000000000000, 39.75893115100078745, -9.846743663894594434 ) ) ;
#49369 = DIRECTION ( 'NONE',  ( 1.000000000000000000, 0.000000000000000000, -6.938893903907221278E-15 ) ) ;
#49370 = FACE_OUTER_BOUND ( 'NONE', #37083, .T. ) ;
#49371 = PRESENTATION_LAYER_ASSIGNMENT (  '', '', ( #3083 ) ) ;
#49373 = CARTESIAN_POINT ( 'NONE',  ( -8.000000000000000000, 40.74999999999999289, 4.250000000000000000 ) ) ;
#49372 = CARTESIAN_POINT ( 'NONE',  ( 5.076628168052703671, 31.84226448433412315, 8.527530157486179263 ) ) ;
#49375 = VERTEX_POINT ( 'NONE', #73863 ) ;
#49374 = CARTESIAN_POINT ( 'NONE',  ( 18.52753015748618282, 53.92559781766745175, -4.923371831947291888 ) ) ;
#49376 = EDGE_CURVE ( 'NONE', #65168, #85153, #37914, .T. ) ;
#49377 = CARTESIAN_POINT ( 'NONE',  ( 19.38216949554541557, 27.24863466993041783, -9.382169495545420901 ) ) ;
#49378 = CARTESIAN_POINT ( 'NONE',  ( 5.076628168052703671, 46.84226448433412315, 8.527530157486179263 ) ) ;
#49379 = LINE ( 'NONE', #62908, #74384 ) ;
#49380 = CARTESIAN_POINT ( 'NONE',  ( 24.16423886937409904, 59.09541550158063217, 3.795296366450317205 ) ) ;
#49381 = CARTESIAN_POINT ( 'NONE',  ( 19.84674366389459266, 23.71726448433412315, -2.638427012816827677 ) ) ;
#49382 = CARTESIAN_POINT ( 'NONE',  ( -1.926860441876562025, 39.47997603579417358, -3.195792623639529761 ) ) ;
#49383 = CARTESIAN_POINT ( 'NONE',  ( -4.164238869374099927, 62.01208216824728936, 3.795296366450308767 ) ) ;
#49384 = CARTESIAN_POINT ( 'NONE',  ( 14.92337183194729988, 54.34226448433412315, -8.527530157486177487 ) ) ;
#49385 = CARTESIAN_POINT ( 'NONE',  ( -2.266590686148945544, 67.22041550158063217, 7.082119434687048631 ) ) ;
#49386 = CARTESIAN_POINT ( 'NONE',  ( -4.164238869374099039, 31.80374883491396432, 8.674139862899312516E-16 ) ) ;
#49387 = CARTESIAN_POINT ( 'NONE',  ( 6.204703633549690345, 37.84541550158063927, 14.16423886937410082 ) ) ;
#49388 = CARTESIAN_POINT ( 'NONE',  ( 2.831191079880678085, 79.91181047996344944, 9.500000000000000000 ) ) ;
#49389 = AXIS2_PLACEMENT_3D ( 'NONE', #52952, #16448, #76451 ) ;
#49391 = CARTESIAN_POINT ( 'NONE',  ( 12.63842701281683922, 59.55059781766744464, -9.846743663894590881 ) ) ;
#49390 = CARTESIAN_POINT ( 'NONE',  ( 0.8952175423694904710, 27.60160829253885950, -5.990408912944333863 ) ) ;
#49392 = CARTESIAN_POINT ( 'NONE',  ( 17.96484262340118221, 54.93868534415484106, 7.964842623401181321 ) ) ;
#49393 = DIRECTION ( 'NONE',  ( 1.000000000000000000, 0.000000000000000000, 0.000000000000000000 ) ) ;
#49394 = AXIS2_PLACEMENT_3D ( 'NONE', #41075, #66885, #96416 ) ;
#49395 = CARTESIAN_POINT ( 'NONE',  ( 7.361572987183169658, 49.96726448433410894, -9.846743663894592657 ) ) ;
#49396 = CARTESIAN_POINT ( 'NONE',  ( 17.35999999999999588, 33.99999999999997868, -9.632054252037207220 ) ) ;
#49397 = CARTESIAN_POINT ( 'NONE',  ( 10.00000000000000178, 52.25893115100078745, 9.846743663894594434 ) ) ;
#49398 = DIRECTION ( 'NONE',  ( -0.000000000000000000, -0.000000000000000000, 1.000000000000000000 ) ) ;
#49399 = ORIENTED_EDGE ( 'NONE', *, *, #87589, .F. ) ;
#49400 = CARTESIAN_POINT ( 'NONE',  ( -4.164238869374099039, 26.80374883491397142, 8.674139862899312516E-16 ) ) ;
#49401 = PRESENTATION_STYLE_ASSIGNMENT (( #20398 ) ) ;
#49403 = CARTESIAN_POINT ( 'NONE',  ( 19.10478245763052385, 46.02576239577081907, -5.990408912944311659 ) ) ;
#49402 = CARTESIAN_POINT ( 'NONE',  ( -4.285674571758069540, -17.54407107684652445, -2.500000000000000000 ) ) ;
#49404 = CARTESIAN_POINT ( 'NONE',  ( -0.8801773607111009756, 18.06368534415484106, 1.068504757029289695E-15 ) ) ;
#49405 = CARTESIAN_POINT ( 'NONE',  ( 0.6178305044545818747, 28.49863466993041783, -9.382169495545419124 ) ) ;
#49406 = CARTESIAN_POINT ( 'NONE',  ( 20.32896413005680003, 61.77164270246083788, 5.963430220938287007 ) ) ;
#49407 = CARTESIAN_POINT ( 'NONE',  ( 18.52753015748618282, 13.92559781766745175, -4.923371831947291888 ) ) ;
#49408 = VERTEX_POINT ( 'NONE', #49879 ) ;
#49409 = CARTESIAN_POINT ( 'NONE',  ( 4.573751236499521866, -6.413519960490759786, -4.000000000000000000 ) ) ;
#49410 = CARTESIAN_POINT ( 'NONE',  ( 17.08211943468705130, 33.47041550158063927, 12.26659068614894998 ) ) ;
#49411 = FACE_OUTER_BOUND ( 'NONE', #84051, .T. ) ;
#49412 = EDGE_CURVE ( 'NONE', #23105, #3928, #33922, .T. ) ;
#49413 = CARTESIAN_POINT ( 'NONE',  ( 20.88017736071110519, 5.563685344154838397, 2.639326808657452039E-16 ) ) ;
#49414 = LINE ( 'NONE', #20414, #55947 ) ;
#49415 = CARTESIAN_POINT ( 'NONE',  ( -0.8801773607111008646, 43.27201867748817676, 2.915334737309923430 ) ) ;
#49416 = CARTESIAN_POINT ( 'NONE',  ( 19.42250999205614193, 35.14701867748816966, 5.440088680355555262 ) ) ;
#49417 = CARTESIAN_POINT ( 'NONE',  ( 22.81628187352648496, 1.831968003263753753, -3.434112377981050290 ) ) ;
#49418 = CARTESIAN_POINT ( 'NONE',  ( 17.20831665107776587, 64.13393115100079456, -7.208316651077762316 ) ) ;
#49419 = DIRECTION ( 'NONE',  ( -0.9990482215818579093, 0.000000000000000000, 0.04361938736533305799 ) ) ;
#49420 = CARTESIAN_POINT ( 'NONE',  ( 18.52753015748617571, 13.09226448433411960, 4.923371831947298993 ) ) ;
#49421 = CARTESIAN_POINT ( 'NONE',  ( 18.39792806157246829, 49.52224192338640307, 6.500000000000079936 ) ) ;
#49422 = EDGE_CURVE ( 'NONE', #65076, #23913, #33991, .T. ) ;
#49423 = CARTESIAN_POINT ( 'NONE',  ( 10.00000000000000178, 49.31368534415484106, 10.88017736071110342 ) ) ;
#49424 = CARTESIAN_POINT ( 'NONE',  ( -1.099225684535947600, 3.706968003263753531, -6.408140936763238038 ) ) ;
#49425 = CARTESIAN_POINT ( 'NONE',  ( -0.8801773607110991993, 62.85535201082150536, -2.915334737309923874 ) ) ;
#49426 = CARTESIAN_POINT ( 'NONE',  ( 1.472469842513823179, 30.59226448433411960, -4.923371831947296329 ) ) ;
#49427 = CARTESIAN_POINT ( 'NONE',  ( 19.38216949554541557, 37.24863466993041783, -9.382169495545420901 ) ) ;
#49429 = CARTESIAN_POINT ( 'NONE',  ( -5.815488105659576412, 14.76984994604921475, -13.76235181012726549 ) ) ;
#49428 = CARTESIAN_POINT ( 'NONE',  ( 10.00000000000000000, 9.758931151000785675, -9.846743663894594434 ) ) ;
#49430 = ORIENTED_EDGE ( 'NONE', *, *, #44801, .T. ) ;
#49431 = DIRECTION ( 'NONE',  ( 0.000000000000000000, -1.000000000000000000, 0.000000000000000000 ) ) ;
#49432 = CARTESIAN_POINT ( 'NONE',  ( 8.629999999999995453, 40.74999999999999289, 4.250000000000000000 ) ) ;
#49433 = CARTESIAN_POINT ( 'NONE',  ( 10.00000000000000000, 6.813685344154838397, -10.88017736071110342 ) ) ;
#49435 = CARTESIAN_POINT ( 'NONE',  ( -0.3689425029237881626, 22.42874883491397142, 10.36894250292379027 ) ) ;
#49434 = CARTESIAN_POINT ( 'NONE',  ( 21.09922568453594849, 61.20696800326376064, 6.408140936763242479 ) ) ;
#49436 = CARTESIAN_POINT ( 'NONE',  ( 2.791683348922237240, 35.38393115100079456, -7.208316651077763204 ) ) ;
#49437 = AXIS2_PLACEMENT_3D ( 'NONE', #95419, #65398, #74374 ) ;
#49438 = CARTESIAN_POINT ( 'NONE',  ( 4.559911319644449179, 22.23035201082150536, -9.422509992056141925 ) ) ;
#49439 = CARTESIAN_POINT ( 'NONE',  ( 10.00000000000000000, 6.813685344154838397, -10.88017736071110342 ) ) ;
#49440 = ORIENTED_EDGE ( 'NONE', *, *, #73827, .T. ) ;
#49441 = VECTOR ( 'NONE', #67820, 1000.000000000000000 ) ;
#49442 = CARTESIAN_POINT ( 'NONE',  ( 15.44008868035555260, 19.73035201082150536, 9.422509992056143702 ) ) ;
#49443 = CARTESIAN_POINT ( 'NONE',  ( 2.035157376598824452, 23.68868534415484461, 7.964842623401179544 ) ) ;
#49444 = DIRECTION ( 'NONE',  ( 0.000000000000000000, -1.000000000000000000, 0.000000000000000000 ) ) ;
#49445 = ORIENTED_EDGE ( 'NONE', *, *, #80497, .F. ) ;
#49446 = CARTESIAN_POINT ( 'NONE',  ( 10.00000000000000178, 67.25893115100079456, 9.846743663894594434 ) ) ;
#49448 = EDGE_CURVE ( 'NONE', #67150, #75159, #5392, .T. ) ;
#49447 = CARTESIAN_POINT ( 'NONE',  ( 10.00000000000000178, 24.31368534415484106, 10.88017736071110342 ) ) ;
#49449 = CARTESIAN_POINT ( 'NONE',  ( 17.20831665107776587, 57.88393115100078745, 7.208316651077764980 ) ) ;
#49450 = DIRECTION ( 'NONE',  ( 1.000000000000000000, 0.000000000000000000, 0.000000000000000000 ) ) ;
#49451 = DIRECTION ( 'NONE',  ( 1.776356839400250465E-15, 0.000000000000000000, 1.000000000000000000 ) ) ;
#49452 = CARTESIAN_POINT ( 'NONE',  ( 6.204703633549690345, 27.84541550158063217, 14.16423886937410082 ) ) ;
#49453 = CARTESIAN_POINT ( 'NONE',  ( 20.88017736071110164, 45.35535201082149115, 2.915334737309930979 ) ) ;
#49454 = CARTESIAN_POINT ( 'NONE',  ( 7.084665262690076126, 19.10535201082150181, 10.88017736071109987 ) ) ;
#49455 = CARTESIAN_POINT ( 'NONE',  ( 1.472469842513823179, 60.59226448433412315, -4.923371831947296329 ) ) ;
#49456 = EDGE_CURVE ( 'NONE', #51188, #43096, #85128, .T. ) ;
#49457 = CARTESIAN_POINT ( 'NONE',  ( -11.26206397713064256, -93.45673894084376343, -3.749999999999999556 ) ) ;
#49458 = CARTESIAN_POINT ( 'NONE',  ( 0.1532563361054082862, 46.21726448433411605, 2.638427012816831674 ) ) ;
#49459 = CARTESIAN_POINT ( 'NONE',  ( 12.63842701281683034, 2.467264484334118269, 9.846743663894596210 ) ) ;
#49460 = CARTESIAN_POINT ( 'NONE',  ( 12.81628187352647252, -38.16803199673624647, -3.434112377981059172 ) ) ;
#49461 = ORIENTED_EDGE ( 'NONE', *, *, #35122, .F. ) ;
#49462 = CARTESIAN_POINT ( 'NONE',  ( 20.88017736071110164, 10.35535201082150714, 2.915334737309930979 ) ) ;
#49463 = CARTESIAN_POINT ( 'NONE',  ( 1.472469842513823179, 6.425597817667451750, 4.923371831947296329 ) ) ;
#49464 = CARTESIAN_POINT ( 'NONE',  ( 22.81628187352647785, 1.415301336597087012, 3.434112377981063169 ) ) ;
#49465 = CARTESIAN_POINT ( 'NONE',  ( 15.44008868035555793, 46.39701867748817676, -9.422509992056140149 ) ) ;
#49467 = CARTESIAN_POINT ( 'NONE',  ( -2.816281873526473856, 39.33196800326374643, 3.434112377981055619 ) ) ;
#49466 = CARTESIAN_POINT ( 'NONE',  ( 0.5774900079438607392, 13.48035201082150358, 5.440088680355550821 ) ) ;
#49468 = CARTESIAN_POINT ( 'NONE',  ( -4.164238869374099927, 27.01208216824730357, 3.795296366450308767 ) ) ;
#49469 = CARTESIAN_POINT ( 'NONE',  ( -2.168404344971008868E-15, 78.91966277462715595, -9.500000000000000000 ) ) ;
#49470 = EDGE_CURVE ( 'NONE', #17007, #38580, #9681, .T. ) ;
#49471 = CARTESIAN_POINT ( 'NONE',  ( 16.40814093676324603, 52.45696800326375353, -11.09922568453594671 ) ) ;
#49472 = ORIENTED_EDGE ( 'NONE', *, *, #5431, .F. ) ;
#49473 = CARTESIAN_POINT ( 'NONE',  ( 22.81628187352647785, 6.415301336597088344, 3.434112377981063169 ) ) ;
#49474 = CARTESIAN_POINT ( 'NONE',  ( 0.5774900079438607392, 33.48035201082150536, 5.440088680355550821 ) ) ;
#49475 = CARTESIAN_POINT ( 'NONE',  ( 0.1532563361054083140, 61.00893115100078745, 1.131784320476157264E-15 ) ) ;
#49477 = EDGE_LOOP ( 'NONE', ( #17601, #23439, #18355, #38109, #83162 ) ) ;
#49476 = EDGE_CURVE ( 'NONE', #18635, #8299, #65866, .T. ) ;
#49479 = CARTESIAN_POINT ( 'NONE',  ( -6.617298650316659980, -58.37178459782695228, 2.500000000000000000 ) ) ;
#49478 = CARTESIAN_POINT ( 'NONE',  ( 14.92337183194729633, 7.675597817667451750, 8.527530157486181039 ) ) ;
#49480 = CARTESIAN_POINT ( 'NONE',  ( 17.20831665107776587, 7.883931151000784787, 7.208316651077764980 ) ) ;
#49481 = CARTESIAN_POINT ( 'NONE',  ( 5.076628168052703671, 16.84226448433411960, 8.527530157486179263 ) ) ;
#49482 = CARTESIAN_POINT ( 'NONE',  ( 2.791683348922237240, 5.383931151000785675, -7.208316651077763204 ) ) ;
#49483 = SURFACE_SIDE_STYLE ('',( #56987 ) ) ;
#49485 = CARTESIAN_POINT ( 'NONE',  ( -0.8801773607110990882, 37.85535201082150536, -2.915334737309924318 ) ) ;
#49484 = CARTESIAN_POINT ( 'NONE',  ( 0.5774900079438607392, 58.48035201082151247, 5.440088680355550821 ) ) ;
#49486 = CARTESIAN_POINT ( 'NONE',  ( 12.91533473730993009, 66.60535201082150536, -10.88017736071109987 ) ) ;
#49488 = ORIENTED_EDGE ( 'NONE', *, *, #50935, .T. ) ;
#49487 = CARTESIAN_POINT ( 'NONE',  ( 17.20831665107776587, 14.13393115100078568, -7.208316651077762316 ) ) ;
#49489 = CARTESIAN_POINT ( 'NONE',  ( 5.810213597521703299, 14.95037102642602278, 13.56092647078875224 ) ) ;
#49490 = CARTESIAN_POINT ( 'NONE',  ( 0.1532563361054100626, 55.80059781766745175, -2.638427012816831230 ) ) ;
#49491 = VERTEX_POINT ( 'NONE', #58353 ) ;
#49492 = ORIENTED_EDGE ( 'NONE', *, *, #58216, .F. ) ;
#49493 = FACE_OUTER_BOUND ( 'NONE', #25727, .T. ) ;
#49494 = CARTESIAN_POINT ( 'NONE',  ( 10.00000000000000178, 13.05374883491396787, 14.16423886937410082 ) ) ;
#49495 = UNCERTAINTY_MEASURE_WITH_UNIT (LENGTH_MEASURE( 1.000000000000000082E-05 ), #75690, 'distance_accuracy_value', 'NONE');
#49496 = CARTESIAN_POINT ( 'NONE',  ( 2.393480905993071062, 0.3639310596586424751, 14.80781041047755942 ) ) ;
#49497 = CARTESIAN_POINT ( 'NONE',  ( 22.26659068614894466, 13.88708216824730179, 7.082119434687054849 ) ) ;
#49498 = CIRCLE ( 'NONE', #28735, 1.499999999999996669 ) ;
#49499 = CARTESIAN_POINT ( 'NONE',  ( -0.3689425029237898834, 26.17874883491396432, -10.36894250292378850 ) ) ;
#49500 = CARTESIAN_POINT ( 'NONE',  ( 10.00000000000000000, 31.81368534415483751, -10.88017736071110342 ) ) ;
#49501 = CARTESIAN_POINT ( 'NONE',  ( 14.99847009497950800, 14.49999999999999112, -0.2142307401080081053 ) ) ;
#49502 = EDGE_LOOP ( 'NONE', ( #92888, #1060, #9661, #22178 ) ) ;
#49503 = CARTESIAN_POINT ( 'NONE',  ( 5.076628168052703671, 11.84226448433411960, 8.527530157486179263 ) ) ;
#49505 = CARTESIAN_POINT ( 'NONE',  ( 0.1532563361054082862, 11.21726448433411605, 2.638427012816831674 ) ) ;
#49504 = CARTESIAN_POINT ( 'NONE',  ( 2.035157376598822676, 52.43868534415483396, -7.964842623401177768 ) ) ;
#49506 = CARTESIAN_POINT ( 'NONE',  ( -1.099225684535947600, 49.54030133659708923, 6.408140936763237150 ) ) ;
#49507 = CARTESIAN_POINT ( 'NONE',  ( 2.791683348922240793, 36.63393115100078035, 7.208316651077764092 ) ) ;
#49508 = VECTOR ( 'NONE', #41986, 1000.000000000000227 ) ;
#49509 = CARTESIAN_POINT ( 'NONE',  ( 0.000000000000000000, 15.00000000000000000, 0.000000000000000000 ) ) ;
#49510 = CARTESIAN_POINT ( 'NONE',  ( 22.81628187352647785, 31.41530133659709279, 3.434112377981063169 ) ) ;
#49511 = CARTESIAN_POINT ( 'NONE',  ( -10.36894250292379205, -38.82125116508603924, -10.36894250292378672 ) ) ;
#49512 = CARTESIAN_POINT ( 'NONE',  ( 0.1532563361054083140, 26.00893115100078745, 1.131784320476157264E-15 ) ) ;
#49513 = CARTESIAN_POINT ( 'NONE',  ( 20.36894250292379382, 18.67874883491397142, 10.36894250292379205 ) ) ;
#49514 = ORIENTED_EDGE ( 'NONE', *, *, #31312, .F. ) ;
#49515 = CARTESIAN_POINT ( 'NONE',  ( -0.8801773607111008646, 48.27201867748816966, 2.915334737309923430 ) ) ;
#49516 = CARTESIAN_POINT ( 'NONE',  ( 20.88017736071110164, 55.35535201082149825, 2.915334737309930979 ) ) ;
#49517 = CARTESIAN_POINT ( 'NONE',  ( -2.266590686148945544, 47.22041550158063927, 7.082119434687048631 ) ) ;
#49518 = CARTESIAN_POINT ( 'NONE',  ( 2.791683348922240793, 51.63393115100078745, 7.208316651077764092 ) ) ;
#49519 = CARTESIAN_POINT ( 'NONE',  ( 2.791683348922240793, 16.63393115100078745, 7.208316651077764092 ) ) ;
#49521 = CARTESIAN_POINT ( 'NONE',  ( -8.646548597236174416, 87.41340560412834293, 4.720830526302458807 ) ) ;
#49520 = CARTESIAN_POINT ( 'NONE',  ( 10.00000000000000178, 65.37363466993042493, 12.81628187352647608 ) ) ;
#49522 = CARTESIAN_POINT ( 'NONE',  ( 4.559911319644449179, 42.23035201082151247, -9.422509992056141925 ) ) ;
#49523 = CARTESIAN_POINT ( 'NONE',  ( 0.000000000000000000, 99.74999999999998579, -7.750000000000000000 ) ) ;
#49524 = VECTOR ( 'NONE', #74224, 1000.000000000000000 ) ;
#49525 = CARTESIAN_POINT ( 'NONE',  ( -2.816281873526473856, 29.33196800326376064, 3.434112377981055619 ) ) ;
#49526 = CARTESIAN_POINT ( 'NONE',  ( 1.472469842513823179, 56.42559781766745886, 4.923371831947296329 ) ) ;
#49527 = CARTESIAN_POINT ( 'NONE',  ( 5.440088680355549045, 16.39701867748817676, -9.422509992056141925 ) ) ;
#49528 = CARTESIAN_POINT ( 'NONE',  ( 20.88017736071110519, 5.563685344154837509, 2.639326808657452039E-16 ) ) ;
#49529 = CARTESIAN_POINT ( 'NONE',  ( 2.035157376598822676, 67.43868534415484817, -7.964842623401177768 ) ) ;
#49530 = EDGE_CURVE ( 'NONE', #31960, #31762, #20875, .T. ) ;
#49531 = SURFACE_STYLE_FILL_AREA ( #36016 ) ;
#49532 = CARTESIAN_POINT ( 'NONE',  ( 0.2751277870542909176, 59.36607318730130345, -6.499999999999992006 ) ) ;
#49533 = CARTESIAN_POINT ( 'NONE',  ( -0.8801773607111009756, 63.06368534415484106, 1.068504757029289695E-15 ) ) ;
#49534 = CARTESIAN_POINT ( 'NONE',  ( 12.63842701281683034, 2.467264484334118269, 9.846743663894596210 ) ) ;
#49535 = CARTESIAN_POINT ( 'NONE',  ( 18.00000000000000000, 78.09931407715666296, -3.985200473436270485 ) ) ;
#49536 = CARTESIAN_POINT ( 'NONE',  ( 0.1532563361054083140, 36.00893115100078745, 1.131784320476157264E-15 ) ) ;
#49537 = CARTESIAN_POINT ( 'NONE',  ( 0.5774900079438607392, 18.48035201082150536, 5.440088680355550821 ) ) ;
#49538 = CARTESIAN_POINT ( 'NONE',  ( 17.20831665107776587, 62.88393115100078745, 7.208316651077764980 ) ) ;
#49540 = CARTESIAN_POINT ( 'NONE',  ( -9.011287250621620615, 14.76930270348882068, -11.91783356064799726 ) ) ;
#49539 = CARTESIAN_POINT ( 'NONE',  ( 15.44008868035555260, 34.73035201082151247, 9.422509992056143702 ) ) ;
#49541 =( NAMED_UNIT ( * ) SI_UNIT ( $, .STERADIAN. ) SOLID_ANGLE_UNIT ( ) );
#49542 = CARTESIAN_POINT ( 'NONE',  ( -2.816281873526473856, 34.12363466993042493, 9.499525473075851096E-16 ) ) ;
#49543 = ORIENTED_EDGE ( 'NONE', *, *, #14589, .T. ) ;
#49544 = CARTESIAN_POINT ( 'NONE',  ( 17.96484262340118221, 49.93868534415484106, 7.964842623401181321 ) ) ;
#49545 = CARTESIAN_POINT ( 'NONE',  ( 19.38216949554541557, 22.24863466993041428, -9.382169495545420901 ) ) ;
#49546 = CARTESIAN_POINT ( 'NONE',  ( 2.035157376598824452, 28.68868534415484106, 7.964842623401179544 ) ) ;
#49547 = CARTESIAN_POINT ( 'NONE',  ( 2.035157376598822676, 2.438685344154838397, -7.964842623401177768 ) ) ;
#49548 = CARTESIAN_POINT ( 'NONE',  ( 7.361572987183169658, 44.96726448433412315, -9.846743663894592657 ) ) ;
#49549 = CARTESIAN_POINT ( 'NONE',  ( 1.472469842513823179, 6.425597817667451750, 4.923371831947296329 ) ) ;
#49550 = CARTESIAN_POINT ( 'NONE',  ( -0.8801773607111009756, 58.06368534415484106, 1.068504757029289695E-15 ) ) ;
#49551 = DIRECTION ( 'NONE',  ( -6.938893903907222067E-15, 0.000000000000000000, 1.000000000000000000 ) ) ;
#49552 = CARTESIAN_POINT ( 'NONE',  ( 17.08211943468705840, 35.13708216824730357, -12.26659068614894466 ) ) ;
#49553 = CARTESIAN_POINT ( 'NONE',  ( -3.750000001621983436, 0.08803144853716619866, -4.000000000000000000 ) ) ;
#49554 = EDGE_LOOP ( 'NONE', ( #5447, #36077, #86062, #46758 ) ) ;
#49555 = ORIENTED_EDGE ( 'NONE', *, *, #22702, .F. ) ;
#49556 = CARTESIAN_POINT ( 'NONE',  ( 24.16423886937409904, 54.09541550158063217, 3.795296366450317205 ) ) ;
#49558 = EDGE_CURVE ( 'NONE', #93263, #44802, #34875, .T. ) ;
#49557 = CARTESIAN_POINT ( 'NONE',  ( 13.79529636645030344, 53.26208216824730357, 14.16423886937410614 ) ) ;
#49559 = CARTESIAN_POINT ( 'NONE',  ( 19.84674366389459266, 13.30059781766745353, 2.638427012816836559 ) ) ;
#49560 = CARTESIAN_POINT ( 'NONE',  ( 19.38216949554541202, 15.99863466993042138, 9.382169495545424454 ) ) ;
#49561 = CARTESIAN_POINT ( 'NONE',  ( -27.43587634952537968, 22.49999999999998934, 10.00000000000000000 ) ) ;
#49562 = LINE ( 'NONE', #65551, #41888 ) ;
#49564 = CARTESIAN_POINT ( 'NONE',  ( 16.40814093676323893, 30.79030133659708923, 11.09922568453595026 ) ) ;
#49563 = CARTESIAN_POINT ( 'NONE',  ( -0.8801773607110991993, 2.855352010821504471, -2.915334737309923874 ) ) ;
#49565 = CARTESIAN_POINT ( 'NONE',  ( 2.917880565312950480, 45.97041550158063927, -12.26659068614894821 ) ) ;
#49566 = ADVANCED_FACE ( 'NONE', ( #13869 ), #50874, .T. ) ;
#49567 = DIRECTION ( 'NONE',  ( 0.000000000000000000, 0.000000000000000000, -1.000000000000000000 ) ) ;
#49568 = CARTESIAN_POINT ( 'NONE',  ( 10.00000000000000178, 12.25893115100078568, 9.846743663894594434 ) ) ;
#49569 = STYLED_ITEM ( 'NONE', ( #44383 ), #45605 ) ;
#49570 = AXIS2_PLACEMENT_3D ( 'NONE', #63930, #71942, #33921 ) ;
#49571 = CARTESIAN_POINT ( 'NONE',  ( 8.527530157486175710, -1.074402182332540034, -4.923371831947298993 ) ) ;
#49572 = ORIENTED_EDGE ( 'NONE', *, *, #70799, .T. ) ;
#49573 = DIRECTION ( 'NONE',  ( -0.8320502943378437211, 0.5547001962252290364, 0.000000000000000000 ) ) ;
#49574 = CARTESIAN_POINT ( 'NONE',  ( 10.00000000000000000, 19.75893115100078390, -9.846743663894594434 ) ) ;
#49575 = VECTOR ( 'NONE', #88705, 1000.000000000000000 ) ;
#49576 = ORIENTED_EDGE ( 'NONE', *, *, #95041, .T. ) ;
#49578 = CARTESIAN_POINT ( 'NONE',  ( 20.88017736071110875, 30.77201867748816966, -2.915334737309920765 ) ) ;
#49577 = CARTESIAN_POINT ( 'NONE',  ( 6.204703633549690345, 67.84541550158060375, 14.16423886937410082 ) ) ;
#49580 = CARTESIAN_POINT ( 'NONE',  ( 6.565887622018943937, -1.918031996736246692, -12.81628187352647608 ) ) ;
#49579 = CARTESIAN_POINT ( 'NONE',  ( 2.791683348922237240, 55.38393115100078745, -7.208316651077763204 ) ) ;
#49581 = FACE_OUTER_BOUND ( 'NONE', #98866, .T. ) ;
#49582 = CARTESIAN_POINT ( 'NONE',  ( 3.591859063236763294, 18.29030133659708568, -11.09922568453595026 ) ) ;
#49583 = VERTEX_POINT ( 'NONE', #36864 ) ;
#49584 = CARTESIAN_POINT ( 'NONE',  ( 6.204703633549690345, 65.76208216824731778, -14.16423886937410259 ) ) ;
#49585 = CARTESIAN_POINT ( 'NONE',  ( 24.16423886937409904, 59.09541550158063217, 3.795296366450317205 ) ) ;
#49586 = ORIENTED_EDGE ( 'NONE', *, *, #82899, .F. ) ;
#49587 = CARTESIAN_POINT ( 'NONE',  ( 0.5774900079438607392, 33.48035201082150536, 5.440088680355550821 ) ) ;
#49588 = CARTESIAN_POINT ( 'NONE',  ( 19.42250999205614193, 50.14701867748817676, 5.440088680355555262 ) ) ;
#49589 = AXIS2_PLACEMENT_3D ( 'NONE', #98141, #45105, #83113 ) ;
#49590 = CARTESIAN_POINT ( 'NONE',  ( 7.084665262690076126, 52.02201867748816255, -10.88017736071110164 ) ) ;
#49591 = DIRECTION ( 'NONE',  ( -0.06975647374412567714, -0.9975640502598243087, 0.000000000000000000 ) ) ;
#49592 = CARTESIAN_POINT ( 'NONE',  ( 20.88017736071110519, 40.56368534415484106, 2.639326808657452039E-16 ) ) ;
#49593 = B_SPLINE_CURVE_WITH_KNOTS ( 'NONE', 3,
 ( #45405, #38417, #60902, #30895, #53399, #84893 ),
 .UNSPECIFIED., .F., .F.,
 ( 4, 2, 4 ),
 ( 3.409110551495941633E-05, 0.0004400426677367835358, 0.0008459942299586075808 ),
 .UNSPECIFIED. ) ;
#49594 = VECTOR ( 'NONE', #17580, 1000.000000000000000 ) ;
#49595 = EDGE_CURVE ( 'NONE', #91901, #41376, #19898, .T. ) ;
#49596 =( NAMED_UNIT ( * ) PLANE_ANGLE_UNIT ( ) SI_UNIT ( $, .RADIAN. ) );
#49597 = VECTOR ( 'NONE', #71164, 1000.000000000000000 ) ;
#49598 = CARTESIAN_POINT ( 'NONE',  ( 19.84674366389459266, 13.30059781766745353, 2.638427012816836559 ) ) ;
#49599 = VERTEX_POINT ( 'NONE', #53834 ) ;
#49600 = CARTESIAN_POINT ( 'NONE',  ( 11.33984840991517373, -87.82327540140084920, 4.000000000000000000 ) ) ;
#49601 = CARTESIAN_POINT ( 'NONE',  ( 19.84674366389459621, 38.50893115100078745, 7.409399052514197653E-17 ) ) ;
#49602 = CARTESIAN_POINT ( 'NONE',  ( -9.000000000000003553, 80.99999999999994316, -1.249999999999987121 ) ) ;
#49603 = CARTESIAN_POINT ( 'NONE',  ( 0.6178305044545838731, 49.74863466993041072, 9.382169495545420901 ) ) ;
#49604 = CARTESIAN_POINT ( 'NONE',  ( -6.841090228438033272, -58.65898919720570603, 2.750000000000000000 ) ) ;
#49605 = ORIENTED_EDGE ( 'NONE', *, *, #84272, .T. ) ;
#49606 = CYLINDRICAL_SURFACE ( 'NONE', #71564, 11.92686044187656513 ) ;
#49607 = CARTESIAN_POINT ( 'NONE',  ( -7.750000000000000000, 40.99999999999999289, -6.250000000000000000 ) ) ;
#49608 = DIRECTION ( 'NONE',  ( 0.000000000000000000, -1.000000000000000000, 0.000000000000000000 ) ) ;
#49609 = CARTESIAN_POINT ( 'NONE',  ( 10.00000000000000000, 65.55374883491396076, -14.16423886937410082 ) ) ;
#49610 = CARTESIAN_POINT ( 'NONE',  ( 0.000000000000000000, 0.5000000000000004441, 0.000000000000000000 ) ) ;
#49611 = VERTEX_POINT ( 'NONE', #61813 ) ;
#49612 = CARTESIAN_POINT ( 'NONE',  ( 14.35000000000000142, 98.49999999999998579, -8.525133428036873795 ) ) ;
#49613 = CARTESIAN_POINT ( 'NONE',  ( 14.92337183194729988, 39.34226448433412315, -8.527530157486177487 ) ) ;
#49614 = PRESENTATION_STYLE_ASSIGNMENT (( #94144 ) ) ;
#49615 = CARTESIAN_POINT ( 'NONE',  ( 22.81628187352648496, 11.83196800326375531, -3.434112377981050290 ) ) ;
#49616 = CARTESIAN_POINT ( 'NONE',  ( 12.91533473730993009, 66.60535201082150536, -10.88017736071109987 ) ) ;
#49617 = CARTESIAN_POINT ( 'NONE',  ( -0.1038446121089073443, 4.243024370107933763, -6.337995344473778658 ) ) ;
#49618 = CARTESIAN_POINT ( 'NONE',  ( 19.84674366389459266, 8.717264484334116048, -2.638427012816827677 ) ) ;
#49619 = CARTESIAN_POINT ( 'NONE',  ( 19.84674366389459266, 58.71726448433411605, -2.638427012816827677 ) ) ;
#49620 = DIRECTION ( 'NONE',  ( 0.000000000000000000, -1.000000000000000000, 0.000000000000000000 ) ) ;
#49621 = CIRCLE ( 'NONE', #6535, 2.500000000000002220 ) ;
#49622 = ORIENTED_EDGE ( 'NONE', *, *, #5326, .F. ) ;
#49623 = CARTESIAN_POINT ( 'NONE',  ( -2.266590686148945544, 61.38708216824730357, -7.082119434687050408 ) ) ;
#49624 = CARTESIAN_POINT ( 'NONE',  ( -2.266590686148945544, 12.22041550158063394, 7.082119434687048631 ) ) ;
#49625 = CARTESIAN_POINT ( 'NONE',  ( 12.63842701281683034, 12.46726448433411782, 9.846743663894596210 ) ) ;
#49626 = CARTESIAN_POINT ( 'NONE',  ( -0.8801773607111008646, 48.27201867748816966, 2.915334737309923430 ) ) ;
#49627 = VECTOR ( 'NONE', #78582, 999.9999999999998863 ) ;
#49629 = CARTESIAN_POINT ( 'NONE',  ( 10.44173051747104708, 12.78704354326105275, -4.918064008119704233 ) ) ;
#49628 = CARTESIAN_POINT ( 'NONE',  ( 22.81628187352647785, 26.62363466993042138, 6.195893100308588602E-16 ) ) ;
#49630 = CARTESIAN_POINT ( 'NONE',  ( 19.42250999205614193, 5.147018677488171434, 5.440088680355555262 ) ) ;
#49632 = AXIS2_PLACEMENT_3D ( 'NONE', #92394, #32376, #70894 ) ;
#49631 = CARTESIAN_POINT ( 'NONE',  ( 0.000000000000000000, 0.5000000000000004441, 0.000000000000000000 ) ) ;
#49633 = DIRECTION ( 'NONE',  ( -1.000000000000000000, 0.000000000000000000, 0.000000000000000000 ) ) ;
#49634 = CARTESIAN_POINT ( 'NONE',  ( 1.472469842513823179, 55.59226448433412315, -4.923371831947296329 ) ) ;
#49635 = CARTESIAN_POINT ( 'NONE',  ( 5.076628168052703671, 11.84226448433411960, 8.527530157486179263 ) ) ;
#49636 = CARTESIAN_POINT ( 'NONE',  ( 5.440088680355556150, -30.26964798917849109, 9.422509992056138373 ) ) ;
#49637 = CARTESIAN_POINT ( 'NONE',  ( 16.40814093676323893, 20.79030133659708923, 11.09922568453595026 ) ) ;
#49638 = CARTESIAN_POINT ( 'NONE',  ( 1.274849032794292736, 52.55509018479936856, -6.499999999999977796 ) ) ;
#49639 = CARTESIAN_POINT ( 'NONE',  ( 15.44008868035555793, 31.39701867748817676, -9.422509992056140149 ) ) ;
#49640 = DIRECTION ( 'NONE',  ( 0.000000000000000000, 0.000000000000000000, 1.000000000000000000 ) ) ;
#49641 = CARTESIAN_POINT ( 'NONE',  ( 24.16423886937409904, 49.09541550158063217, 3.795296366450317205 ) ) ;
#49642 = ADVANCED_FACE ( 'NONE', ( #60830 ), #30106, .T. ) ;
#49643 = CARTESIAN_POINT ( 'NONE',  ( 10.00000000000000000, 25.55374883491396787, -14.16423886937410082 ) ) ;
#49644 = CARTESIAN_POINT ( 'NONE',  ( 7.361572987183170547, 42.05059781766745886, 9.846743663894590881 ) ) ;
#49645 = CARTESIAN_POINT ( 'NONE',  ( 0.6178305044545838731, 34.74863466993042493, 9.382169495545420901 ) ) ;
#49646 = CARTESIAN_POINT ( 'NONE',  ( 10.00000000000000178, 24.31368534415484106, 10.88017736071110342 ) ) ;
#49647 = B_SPLINE_CURVE_WITH_KNOTS ( 'NONE', 3,
 ( #57141, #19151, #26645, #96145, #88129, #19641, #3669, #55681, #4159, #87637, #49629, #34626, #94158, #50134, #79655, #11153, #80138, #71665, #56657, #11648, #3175, #17691, #25684, #33640 ),
 .UNSPECIFIED., .F., .F.,
 ( 4, 2, 2, 2, 2, 2, 2, 2, 2, 2, 2, 4 ),
 ( 0.000000000000000000, 0.002011827134370535418, 0.003017740701555803127, 0.004023654268741070836, 0.006035481403111603652, 0.007041394970296870927, 0.008047308537482138202, 0.01005913567185267796, 0.01106504923903794783, 0.01207096280622321945, 0.01408278994059376787, 0.01609461707496431804 ),
 .UNSPECIFIED. ) ;
#49648 = CARTESIAN_POINT ( 'NONE',  ( 12.63842701281683034, 57.46726448433411605, 9.846743663894596210 ) ) ;
#49649 = CARTESIAN_POINT ( 'NONE',  ( 20.88017736071110519, 45.56368534415484106, 2.639326808657452039E-16 ) ) ;
#49650 = CARTESIAN_POINT ( 'NONE',  ( 13.43411237798105340, 10.58196800326375353, 12.81628187352647963 ) ) ;
#49651 = CARTESIAN_POINT ( 'NONE',  ( 13.79529636645030344, 38.26208216824729647, 14.16423886937410614 ) ) ;
#49652 = DIRECTION ( 'NONE',  ( 0.6755902076156591329, 0.000000000000000000, -0.7372773368101250835 ) ) ;
#49653 = CARTESIAN_POINT ( 'NONE',  ( 1.472469842513823179, 30.59226448433411960, -4.923371831947296329 ) ) ;
#49654 = CARTESIAN_POINT ( 'NONE',  ( 13.43411237798106583, 62.66530133659708923, -12.81628187352647252 ) ) ;
#49655 = CARTESIAN_POINT ( 'NONE',  ( 3.591859063236761518, 4.956968003263753531, 11.09922568453594849 ) ) ;
#49656 = VERTEX_POINT ( 'NONE', #26289 ) ;
#49657 = DIRECTION ( 'NONE',  ( 0.000000000000000000, 0.000000000000000000, 1.000000000000000000 ) ) ;
#49658 = LINE ( 'NONE', #50662, #71485 ) ;
#49659 = CARTESIAN_POINT ( 'NONE',  ( 15.44008868035555260, 19.73035201082150536, 9.422509992056143702 ) ) ;
#49661 = DIRECTION ( 'NONE',  ( -0.000000000000000000, 1.000000000000000000, -0.000000000000000000 ) ) ;
#49660 = CARTESIAN_POINT ( 'NONE',  ( 20.36894250292379738, 9.928748834913966093, -10.36894250292379027 ) ) ;
#49662 = CARTESIAN_POINT ( 'NONE',  ( 17.20831665107776587, 4.133931151000785675, -7.208316651077762316 ) ) ;
#49663 = CARTESIAN_POINT ( 'NONE',  ( 10.00000000000000178, 52.25893115100078745, 9.846743663894594434 ) ) ;
#49664 = CARTESIAN_POINT ( 'NONE',  ( 7.084665262690076126, 34.10535201082151247, 10.88017736071109987 ) ) ;
#49665 = CARTESIAN_POINT ( 'NONE',  ( 10.93781366033347169, 15.00000000000000000, -10.26470809774065351 ) ) ;
#49666 = CARTESIAN_POINT ( 'NONE',  ( 18.72515096720568195, 26.07228050351032778, -6.500000000000018652 ) ) ;
#49667 = ADVANCED_FACE ( 'NONE', ( #95279 ), #9830, .F. ) ;
#49668 = AXIS2_PLACEMENT_3D ( 'NONE', #46341, #8343, #1361 ) ;
#49669 = VECTOR ( 'NONE', #69831, 1000.000000000000000 ) ;
#49670 = ORIENTED_EDGE ( 'NONE', *, *, #36258, .F. ) ;
#49671 = CARTESIAN_POINT ( 'NONE',  ( -18.89999999999999503, 92.00000000000000000, -7.750000000000000000 ) ) ;
#49672 = VERTEX_POINT ( 'NONE', #87285 ) ;
#49673 = ORIENTED_EDGE ( 'NONE', *, *, #6708, .F. ) ;
#49674 = VECTOR ( 'NONE', #7988, 1000.000000000000000 ) ;
#49675 = CARTESIAN_POINT ( 'NONE',  ( 6.382347221874359988, 0.3639313913011580359, 13.57444820018234388 ) ) ;
#49676 = CARTESIAN_POINT ( 'NONE',  ( -4.164238869374099927, 7.012082168247302683, 3.795296366450308767 ) ) ;
#49678 = EDGE_CURVE ( 'NONE', #22113, #28657, #16470, .T. ) ;
#49677 = CARTESIAN_POINT ( 'NONE',  ( 17.08211943468705840, 5.137082168247300906, -12.26659068614894466 ) ) ;
#49679 = CARTESIAN_POINT ( 'NONE',  ( 13.79529636645031943, 50.34541550158064638, -14.16423886937409904 ) ) ;
#49680 = CARTESIAN_POINT ( 'NONE',  ( 1.472469842513823179, 60.59226448433412315, -4.923371831947296329 ) ) ;
#49681 = CARTESIAN_POINT ( 'NONE',  ( 10.00000000000000000, 34.75893115100078745, -9.846743663894594434 ) ) ;
#49682 = CARTESIAN_POINT ( 'NONE',  ( 0.1922240491738438917, 38.18878173731739878, 6.499999999999968914 ) ) ;
#49684 = CARTESIAN_POINT ( 'NONE',  ( 3.591859063236763294, -1.709698663402913210, -11.09922568453595026 ) ) ;
#49683 = CARTESIAN_POINT ( 'NONE',  ( 10.00000000000000178, 29.31368534415483751, 10.88017736071110342 ) ) ;
#49685 = CARTESIAN_POINT ( 'NONE',  ( 2.917880565312950480, 0.9704155015806342766, -12.26659068614894821 ) ) ;
#49686 = CARTESIAN_POINT ( 'NONE',  ( 13.79529636645030344, 58.26208216824728936, 14.16423886937410614 ) ) ;
#49687 = CARTESIAN_POINT ( 'NONE',  ( -0.8801773607111009756, 3.063685344154838397, 1.068504757029289695E-15 ) ) ;
#49688 = CARTESIAN_POINT ( 'NONE',  ( 0.000000000000000000, 15.00000000000000000, 0.000000000000000000 ) ) ;
#49689 = CARTESIAN_POINT ( 'NONE',  ( 0.4195498155886417946, 0.4999999999999971689, -9.500000000000000000 ) ) ;
#49690 = EDGE_CURVE ( 'NONE', #28000, #39649, #15239, .T. ) ;
#49691 = CARTESIAN_POINT ( 'NONE',  ( -7.208316651077764980, -34.61606884899921965, -7.208316651077759651 ) ) ;
#49692 = ORIENTED_EDGE ( 'NONE', *, *, #61077, .F. ) ;
#49693 = LINE ( 'NONE', #4221, #23614 ) ;
#49694 = CARTESIAN_POINT ( 'NONE',  ( 1.472469842513823179, 20.59226448433411960, -4.923371831947296329 ) ) ;
#49695 = VERTEX_POINT ( 'NONE', #2347 ) ;
#49696 = CARTESIAN_POINT ( 'NONE',  ( 13.79529636645031943, 35.34541550158063927, -14.16423886937409904 ) ) ;
#49697 = CARTESIAN_POINT ( 'NONE',  ( 19.84674366389459266, 38.71726448433412315, -2.638427012816827677 ) ) ;
#49698 = CARTESIAN_POINT ( 'NONE',  ( 10.00000000000000000, 61.81368534415484106, -10.88017736071110342 ) ) ;
#49699 = DIRECTION ( 'NONE',  ( -0.000000000000000000, -0.000000000000000000, -1.000000000000000000 ) ) ;
#49700 = AXIS2_PLACEMENT_3D ( 'NONE', #37519, #90005, #83505 ) ;
#49701 = CARTESIAN_POINT ( 'NONE',  ( 0.5774900079438607392, 48.48035201082150536, 5.440088680355550821 ) ) ;
#49702 = CARTESIAN_POINT ( 'NONE',  ( 2.791683348922240793, 51.63393115100078745, 7.208316651077764092 ) ) ;
#49703 = CARTESIAN_POINT ( 'NONE',  ( 19.38216949554541557, 62.24863466993041072, -9.382169495545420901 ) ) ;
#49704 = CARTESIAN_POINT ( 'NONE',  ( -11.09922568453595382, 8.706968003263760636, -6.408140936763226492 ) ) ;
#49705 = VERTEX_POINT ( 'NONE', #55823 ) ;
#49706 = CARTESIAN_POINT ( 'NONE',  ( -4.164238869374098151, 21.59541550158063217, -3.795296366450310543 ) ) ;
#49707 = VERTEX_POINT ( 'NONE', #56314 ) ;
#49708 = CARTESIAN_POINT ( 'NONE',  ( 13.43411237798106583, 32.66530133659708213, -12.81628187352647252 ) ) ;
#49709 =( LENGTH_UNIT ( ) NAMED_UNIT ( * ) SI_UNIT ( .MILLI., .METRE. ) );
#49710 = CARTESIAN_POINT ( 'NONE',  ( 2.791683348922237240, 25.38393115100078390, -7.208316651077763204 ) ) ;
#49711 = CARTESIAN_POINT ( 'NONE',  ( 19.42250999205614193, 15.14701867748817143, 5.440088680355555262 ) ) ;
#49712 = VECTOR ( 'NONE', #32594, 1000.000000000000000 ) ;
#49713 = CARTESIAN_POINT ( 'NONE',  ( 3.591859063236763294, 53.29030133659708923, -11.09922568453595026 ) ) ;
#49714 = CARTESIAN_POINT ( 'NONE',  ( -46.21538524526005887, 104.1852450480875660, -5.851526435683386040 ) ) ;
#49715 = CARTESIAN_POINT ( 'NONE',  ( 10.00000000000000178, 27.25893115100078390, 9.846743663894594434 ) ) ;
#49716 = EDGE_CURVE ( 'NONE', #26946, #89452, #30794, .T. ) ;
#49718 = ORIENTED_EDGE ( 'NONE', *, *, #36058, .T. ) ;
#49717 = CARTESIAN_POINT ( 'NONE',  ( 19.39235739573469530, 19.87576471608601025, 6.499999999999990230 ) ) ;
#49719 = SURFACE_STYLE_FILL_AREA ( #20222 ) ;
#49720 = CARTESIAN_POINT ( 'NONE',  ( 17.96484262340118221, 64.93868534415483396, 7.964842623401181321 ) ) ;
#49721 = CARTESIAN_POINT ( 'NONE',  ( -0.1503990784575328643, 70.00000000000000000, -6.262539305110068177 ) ) ;
#49722 = CARTESIAN_POINT ( 'NONE',  ( 0.2751277870542986892, 7.282175860852375671, -6.500000000000003553 ) ) ;
#49723 = CARTESIAN_POINT ( 'NONE',  ( 10.00000000000000178, 7.258931151000785675, 9.846743663894594434 ) ) ;
#49724 = CARTESIAN_POINT ( 'NONE',  ( -2.816281873526473856, 24.12363466993042138, 9.499525473075851096E-16 ) ) ;
#49725 =( LENGTH_UNIT ( ) NAMED_UNIT ( * ) SI_UNIT ( .MILLI., .METRE. ) );
#49726 = EDGE_CURVE ( 'NONE', #93626, #12985, #46214, .T. ) ;
#49727 = B_SPLINE_CURVE_WITH_KNOTS ( 'NONE', 3,
 ( #41359, #49314, #11320, #3836, #33799, #79816 ),
 .UNSPECIFIED., .F., .F.,
 ( 4, 2, 4 ),
 ( 7.944000812428443953E-18, 0.0002626113303185986965, 0.0005252226606371893699 ),
 .UNSPECIFIED. ) ;
#49728 = CARTESIAN_POINT ( 'NONE',  ( 2.791683348922237240, 50.38393115100078035, -7.208316651077763204 ) ) ;
#49729 = CARTESIAN_POINT ( 'NONE',  ( 17.39651004071890128, 29.08210964143323096, -6.499999999999448441 ) ) ;
#49730 = CARTESIAN_POINT ( 'NONE',  ( -0.3689425029237881626, 27.42874883491397142, 10.36894250292379027 ) ) ;
#49731 = CARTESIAN_POINT ( 'NONE',  ( 7.361572987183170547, 37.05059781766744464, 9.846743663894590881 ) ) ;
#49732 = CARTESIAN_POINT ( 'NONE',  ( 6.565887622018943937, 35.16530133659708923, 12.81628187352647430 ) ) ;
#49734 = FACE_OUTER_BOUND ( 'NONE', #44792, .T. ) ;
#49733 = LINE ( 'NONE', #26744, #72410 ) ;
#49735 = CARTESIAN_POINT ( 'NONE',  ( -0.8801773607110991993, 62.85535201082150536, -2.915334737309923874 ) ) ;
#49736 = CARTESIAN_POINT ( 'NONE',  ( 22.81628187352647785, 6.623634669930420493, 6.195893100308588602E-16 ) ) ;
#49737 = CIRCLE ( 'NONE', #16219, 1.000000000000000000 ) ;
#49738 = CARTESIAN_POINT ( 'NONE',  ( 9.876730923139298568, 0.5000000000000004441, -11.28938378619063165 ) ) ;
#49739 = CARTESIAN_POINT ( 'NONE',  ( 10.00000000000000000, 34.75893115100078745, -9.846743663894594434 ) ) ;
#49740 = CARTESIAN_POINT ( 'NONE',  ( 20.88017736071110519, 20.56368534415484106, 2.639326808657452039E-16 ) ) ;
#49741 = CARTESIAN_POINT ( 'NONE',  ( 22.81628187352647785, 31.41530133659709279, 3.434112377981063169 ) ) ;
#49742 = CARTESIAN_POINT ( 'NONE',  ( 1.472469842513823179, 31.42559781766745530, 4.923371831947296329 ) ) ;
#49743 = DIRECTION ( 'NONE',  ( 0.2920631208464272710, 0.8487660001727248549, 0.4407895307198656520 ) ) ;
#49744 = CARTESIAN_POINT ( 'NONE',  ( 18.00000000000000355, 77.07179676972445748, -6.500000000000000888 ) ) ;
#49745 = CARTESIAN_POINT ( 'NONE',  ( 15.44008868035555793, 26.39701867748817321, -9.422509992056140149 ) ) ;
#49746 = VERTEX_POINT ( 'NONE', #72764 ) ;
#49747 = CARTESIAN_POINT ( 'NONE',  ( 10.00000000000000000, 66.81368534415484817, -10.88017736071110342 ) ) ;
#49748 = CARTESIAN_POINT ( 'NONE',  ( 2.035157376598822676, 7.438685344154837509, -7.964842623401177768 ) ) ;
#49750 = CARTESIAN_POINT ( 'NONE',  ( 15.44008868035555793, 26.39701867748817321, -9.422509992056140149 ) ) ;
#49749 = CARTESIAN_POINT ( 'NONE',  ( 19.84674366389459266, 58.30059781766745886, 2.638427012816836559 ) ) ;
#49751 = CARTESIAN_POINT ( 'NONE',  ( 9.399392868737718842, 15.00000000000000000, 11.04089732309479110 ) ) ;
#49752 = CARTESIAN_POINT ( 'NONE',  ( 10.00000000000000178, 44.31368534415484106, 10.88017736071110342 ) ) ;
#49754 = CARTESIAN_POINT ( 'NONE',  ( 20.00000000000001066, 90.58866250142803267, -4.971011743019353446 ) ) ;
#49753 = CARTESIAN_POINT ( 'NONE',  ( 17.96484262340118221, 21.18868534415483396, -7.964842623401177768 ) ) ;
#49755 = CARTESIAN_POINT ( 'NONE',  ( 0.1532563361054082862, 6.217264484334118713, 2.638427012816831674 ) ) ;
#49756 = DIRECTION ( 'NONE',  ( -0.000000000000000000, -0.000000000000000000, 1.000000000000000000 ) ) ;
#49757 = CARTESIAN_POINT ( 'NONE',  ( 2.791683348922240793, 46.63393115100077324, 7.208316651077764092 ) ) ;
#49758 = CARTESIAN_POINT ( 'NONE',  ( 0.000000000000000000, 15.00000000000000000, 0.000000000000000000 ) ) ;
#49760 = FILL_AREA_STYLE ('',( #12261 ) ) ;
#49759 = CARTESIAN_POINT ( 'NONE',  ( 22.26659068614894466, 48.88708216824730357, 7.082119434687054849 ) ) ;
#49761 = PRESENTATION_STYLE_ASSIGNMENT (( #72753 ) ) ;
#49762 = CARTESIAN_POINT ( 'NONE',  ( 24.16423886937409904, 14.09541550158063217, 3.795296366450317205 ) ) ;
#49763 = EDGE_CURVE ( 'NONE', #25641, #35624, #88273, .T. ) ;
#49764 = CARTESIAN_POINT ( 'NONE',  ( 2.917880565312948704, 37.63708216824731068, 12.26659068614894643 ) ) ;
#49765 = STYLED_ITEM ( 'NONE', ( #34521 ), #63828 ) ;
#49766 = CARTESIAN_POINT ( 'NONE',  ( 22.81628187352647785, 6.623634669930420493, 6.195893100308588602E-16 ) ) ;
#49767 = COLOUR_RGB ( '', 0.09019608, 0.27058824, 0.51372549) ;
#49768 = DIRECTION ( 'NONE',  ( -0.000000000000000000, -0.000000000000000000, 1.000000000000000000 ) ) ;
#49769 = VERTEX_POINT ( 'NONE', #44248 ) ;
#49770 = CARTESIAN_POINT ( 'NONE',  ( 13.79529636645030344, 63.26208216824730357, 14.16423886937410614 ) ) ;
#49771 = EDGE_CURVE ( 'NONE', #25131, #48799, #94027, .T. ) ;
#49772 = CARTESIAN_POINT ( 'NONE',  ( 0.1532563361054083140, 31.00893115100078390, 1.131784320476157264E-15 ) ) ;
#49774 = CARTESIAN_POINT ( 'NONE',  ( -9.884188733557275341, 88.99910865660910986, -5.687374854485797826 ) ) ;
#49773 = CARTESIAN_POINT ( 'NONE',  ( -6.715867195167532167, 15.00000000000000000, 12.85095824508320028 ) ) ;
#49775 = CARTESIAN_POINT ( 'NONE',  ( 19.42250999205614548, 65.98035201082151957, -5.440088680355545492 ) ) ;
#49776 = CARTESIAN_POINT ( 'NONE',  ( 11.03499054390001533, 2.041642599432720750, 4.094770669169175648 ) ) ;
#49777 = CARTESIAN_POINT ( 'NONE',  ( 0.5774900079438590739, 27.64701867748817676, -5.440088680355550821 ) ) ;
#49778 = AXIS2_PLACEMENT_3D ( 'NONE', #54267, #75300, #46772 ) ;
#49779 = FACE_OUTER_BOUND ( 'NONE', #68764, .T. ) ;
#49780 = CARTESIAN_POINT ( 'NONE',  ( 22.81628187352648496, 21.83196800326374643, -3.434112377981050290 ) ) ;
#49781 = CARTESIAN_POINT ( 'NONE',  ( 18.52753015748617571, 33.09226448433411605, 4.923371831947298993 ) ) ;
#49782 = ORIENTED_EDGE ( 'NONE', *, *, #95410, .T. ) ;
#49783 = PLANE ( 'NONE',  #87580 ) ;
#49784 = CARTESIAN_POINT ( 'NONE',  ( -0.3689425029237898834, 61.17874883491396076, -10.36894250292378850 ) ) ;
#49785 = CARTESIAN_POINT ( 'NONE',  ( 10.00000000000000178, 33.05374883491396787, 14.16423886937410082 ) ) ;
#49786 = CARTESIAN_POINT ( 'NONE',  ( 10.00000000000000178, 29.31368534415483751, 10.88017736071110342 ) ) ;
#49787 = CARTESIAN_POINT ( 'NONE',  ( 20.88017736071110875, 50.77201867748817676, -2.915334737309920765 ) ) ;
#49788 = DIRECTION ( 'NONE',  ( 0.9981347984218670311, 0.000000000000000000, -0.06104853953485662316 ) ) ;
#49789 = CARTESIAN_POINT ( 'NONE',  ( 8.705944879818165560, -3.115743166029874889, -4.000000000000000888 ) ) ;
#49790 = CARTESIAN_POINT ( 'NONE',  ( 0.1532563361054082862, 11.21726448433411605, 2.638427012816831674 ) ) ;
#49791 = SURFACE_STYLE_FILL_AREA ( #13276 ) ;
#49792 =( NAMED_UNIT ( * ) PLANE_ANGLE_UNIT ( ) SI_UNIT ( $, .RADIAN. ) );
#49793 = TOROIDAL_SURFACE ( 'NONE', #81691, 14.49999999999999822, 0.5000000000000000000 ) ;
#49794 = CARTESIAN_POINT ( 'NONE',  ( 12.63842701281683922, 24.55059781766745175, -9.846743663894590881 ) ) ;
#49795 = CARTESIAN_POINT ( 'NONE',  ( 12.63842701281683922, 54.55059781766745175, -9.846743663894590881 ) ) ;
#49796 = CARTESIAN_POINT ( 'NONE',  ( -1.099225684535947600, 48.70696800326375353, -6.408140936763238038 ) ) ;
#49798 = EDGE_CURVE ( 'NONE', #78252, #49181, #36766, .T. ) ;
#49797 = DIRECTION ( 'NONE',  ( 0.8616291604415301508, 0.000000000000000000, -0.5075383629606968761 ) ) ;
#49799 = CARTESIAN_POINT ( 'NONE',  ( 0.5774900079438607392, 68.48035201082150536, 5.440088680355550821 ) ) ;
#49800 = CARTESIAN_POINT ( 'NONE',  ( 14.92337183194729633, 27.67559781766745530, 8.527530157486181039 ) ) ;
#49802 = CARTESIAN_POINT ( 'NONE',  ( 18.52753015748617571, 23.09226448433411960, 4.923371831947298993 ) ) ;
#49801 = CARTESIAN_POINT ( 'NONE',  ( -4.164238869374099927, 62.01208216824728936, 3.795296366450308767 ) ) ;
#49803 = CARTESIAN_POINT ( 'NONE',  ( -0.1023957841222417897, 60.13377557478297319, 6.340343622311918281 ) ) ;
#49804 = CARTESIAN_POINT ( 'NONE',  ( 12.63842701281683922, 59.55059781766744464, -9.846743663894590881 ) ) ;
#49805 = CARTESIAN_POINT ( 'NONE',  ( 10.00000000000000178, 23.05374883491397142, 14.16423886937410082 ) ) ;
#49806 = CARTESIAN_POINT ( 'NONE',  ( 22.26659068614895176, 29.72041550158063572, -7.082119434687042414 ) ) ;
#49807 = CARTESIAN_POINT ( 'NONE',  ( 7.361572987183169658, 39.96726448433411605, -9.846743663894592657 ) ) ;
#49808 = CARTESIAN_POINT ( 'NONE',  ( 4.555630843329481650, 77.03495325336413657, -9.500000000000000000 ) ) ;
#49809 = CARTESIAN_POINT ( 'NONE',  ( 20.88017736071110875, 30.77201867748816966, -2.915334737309920765 ) ) ;
#49810 = ADVANCED_FACE ( 'NONE', ( #27270 ), #51762, .T. ) ;
#49811 = CARTESIAN_POINT ( 'NONE',  ( 4.559911319644449179, 63.89701867748817676, 9.422509992056141925 ) ) ;
#49812 = ORIENTED_EDGE ( 'NONE', *, *, #61474, .F. ) ;
#49813 = B_SPLINE_CURVE_WITH_KNOTS ( 'NONE', 3,
 ( #9779, #2796, #71752, #93268, #10273, #93761 ),
 .UNSPECIFIED., .F., .F.,
 ( 4, 2, 4 ),
 ( 3.409110551496109007E-05, 0.0004400426677367863006, 0.0008459942299586115924 ),
 .UNSPECIFIED. ) ;
#49814 = CARTESIAN_POINT ( 'NONE',  ( 6.565887622018943937, 40.16530133659708923, 12.81628187352647430 ) ) ;
#49815 = CARTESIAN_POINT ( 'NONE',  ( 4.559911319644449179, 48.89701867748817676, 9.422509992056141925 ) ) ;
#49816 = ORIENTED_EDGE ( 'NONE', *, *, #69112, .F. ) ;
#49817 = CARTESIAN_POINT ( 'NONE',  ( 0.000000000000000000, 0.000000000000000000, 0.000000000000000000 ) ) ;
#49818 = CARTESIAN_POINT ( 'NONE',  ( -0.8801773607111009756, 58.06368534415484106, 1.068504757029289695E-15 ) ) ;
#49819 = ORIENTED_EDGE ( 'NONE', *, *, #35698, .T. ) ;
#49820 = CARTESIAN_POINT ( 'NONE',  ( 19.42250999205614193, 65.14701867748817676, 5.440088680355555262 ) ) ;
#49821 = CARTESIAN_POINT ( 'NONE',  ( 7.084665262690076126, 19.10535201082150181, 10.88017736071109987 ) ) ;
#49822 = LINE ( 'NONE', #80332, #65941 ) ;
#49823 = CARTESIAN_POINT ( 'NONE',  ( 20.25387647958508808, 5.218815989627756379E-14, 6.092576751097550591 ) ) ;
#49824 = CARTESIAN_POINT ( 'NONE',  ( 15.44008868035555260, 9.730352010821505360, 9.422509992056143702 ) ) ;
#49825 = CARTESIAN_POINT ( 'NONE',  ( 1.472469842513823179, 10.59226448433411782, -4.923371831947296329 ) ) ;
#49826 = CARTESIAN_POINT ( 'NONE',  ( 6.204703633549690345, 17.84541550158063217, 14.16423886937410082 ) ) ;
#49827 = CARTESIAN_POINT ( 'NONE',  ( 0.5774900079438590739, 22.64701867748817321, -5.440088680355550821 ) ) ;
#49828 = CARTESIAN_POINT ( 'NONE',  ( 7.361572987183169658, 64.96726448433412315, -9.846743663894592657 ) ) ;
#49829 = ORIENTED_EDGE ( 'NONE', *, *, #81811, .F. ) ;
#49830 = CARTESIAN_POINT ( 'NONE',  ( 10.00000000000000178, 57.25893115100078745, 9.846743663894594434 ) ) ;
#49831 = VERTEX_POINT ( 'NONE', #29248 ) ;
#49832 = CARTESIAN_POINT ( 'NONE',  ( 1.274849032794292736, 47.55509018479936856, -6.499999999999977796 ) ) ;
#49833 =( BOUNDED_SURFACE ( )  B_SPLINE_SURFACE ( 1, 2, ( 
 ( #89402, #7406, #81894, #13405, #14906, #14407, #5914, #50910, #81406, #44878, #12908, #75380, #43405, #31845, #46853, #47836, #39859, #68392, #23887, #30868, #1390, #39375, #77349, #85354, #7892, #70365, #31356, #92361, #62341, #30366, #78339, #38884, #8860, #61857, #53881, #55348, #54353, #47342, #62843, #60872, #17367, #32341, #76861, #84865, #69373, #16374, #85855, #15887, #23396, #1882, #93343, #68887, #69870, #895, #9860, #98913, #38386, #77845, #53370, #61365, #417, #91875, #24865, #92848, #24376, #54841, #8374, #91372, #16868, #84388, #9354, #22898, #83880, #15406, #45889, #76377, #46372, #48332, #71349, #79329, #40847, #71827, #19802, #10347, #64305, #10839, #4328, #2867, #94816, #72791, #78836, #18833, #70860, #34294, #87798, #34800, #33318, #18340, #95817, #42318, #63813, #11319, #26319, #94323, #48820, #57796, #50293, #86836, #41358, #11810, #65290, #25844, #49802, #32830, #63329, #56342, #19316, #3336, #88304, #27297, #33798, #56817, #87315, #49313, #80310, #64791, #79815, #95308, #80806, #57306, #40359, #41838, #72305, #3835, #2375, #26812, #93837, #25363, #55849, #86344, #17847, #96816, #14296, #37297, #4819, #82273, #66789, #51291, #44275, #97308, #6289, #59278, #90767, #35293, #13291, #52277, #58786, #20802, #5315, #67784, #13788, #81776, #65786, #81294, #12790, #98306, #96319, #73295, #44768, #29760, #20305, #88797, #74270, #36291, #29275, #50805, #28780, #5801, #74780, #28292, #43290, #75273, #36792, #6783, #60268, #22292, #43779, #97814, #52765, #82776, #73785, #89777, #35793, #27794, #58279, #66281, #59771, #89292, #21294, #51787, #67286, #12303, #42811, #90264, #21797, #24262, #46264, #8266, #46742, #45270, #93223, #53758, #61734, #76749, #68771, #70250, #38766, #62231, #77730, #75765, #32222, #47227, #91759, #69266, #84276, #786, #1766, #30747, #38278, #16752, #9242, #83768, #31239, #15775, #24747, #83273, #22783, #92738, #68284, #76266, #15291, #53262, #39753, #92252, #23777, #54242, #23282, #62723, #84755, #45773, #16260, #14797, #7286, #37787, #77240, #54726, #8744, #91257, #98805, #7783, #30253, #39265, #60757, #69754, #1282, #31735, #85246, #303, #61254, #79210, #65177, #64189, #17253, #3723, #4212, #87198, #11205, #47729, #18721, #32717, #48707, #33210, #18227, #63215, #10236, #87687, #25253, #93719, #95186, #72194, #63704, #10720, #17740, #34682, #41237, #49203, #95698, #71715, #78226, #56707, #2754, #11701, #55226, #33691, #55738, #64676, #78726, #86229, #48216, #85740, #40729, #71231, #26694, #94709, #94207, #9738, #57190, #79707, #40238, #3227, #41724, #34184, #26214, #70746, #19201 ),
 ( #2262, #25737, #49684, #56229, #72677, #80188, #86723, #42210, #20684, #5688, #74661, #51678, #66165, #82157, #14173, #44153, #6662, #36174, #5193, #43668, #6172, #88676, #35681, #58671, #51178, #36676, #66674, #12679, #29150, #52164, #19694, #97199, #81661, #96698, #59159, #13171, #21176, #74155, #37178, #50181, #28177, #67164, #73666, #89173, #20184, #82657, #28667, #89665, #80691, #96195, #27680, #44657, #12187, #88180, #59657, #75152, #35173, #4711, #13669, #97688, #90148, #65674, #21678, #67671, #27182, #43178, #58165, #57684, #42693, #73172, #50687, #81179, #30625, #84634, #16634, #39141, #30133, #76630, #60639, #52649, #45143, #91140, #16136, #83152, #61132, #8149, #38642, #69631, #92616, #7670, #7161, #1155, #22666, #38161, #98684, #91642, #77609, #68164, #23160, #68647, #62106, #53142, #53635, #31615, #37664, #69143, #29637, #92134, #46622, #24140, #83651, #76144, #54607, #85123, #15166, #671, #84155, #45647, #177, #47109, #9122, #15661, #46144, #39637, #98181, #31121, #8632, #90642, #61616, #23659, #54121, #77120, #60145, #22167, #14677, #75649, #78609, #41612, #72081, #63101, #79595, #62599, #93104, #9618, #49092, #10118, #87575, #95072, #48096, #40616, #63589, #48590, #18599, #94587, #71115, #26102, #57080, #87089, #49564, #79093, #2642, #86606, #11096, #32605, #33096, #94098, #25619, #3607, #10605, #55618, #34068, #26577, #24634, #41119, #56112, #18115, #3120, #71609, #64072, #33578, #80076, #55101, #56598, #64562, #17626, #19087, #93603, #11582, #70126, #1648, #85621, #40119, #70620, #32100, #17138, #47617, #78112, #2145, #25140, #86115, #6409, #67411, #60394, #81911, #97940, #36920, #75395, #28902, #13421, #45392, #37425, #75897, #60888, #91386, #74908, #29892, #22916, #83403, #74406, #21927, #5931, #95580, #89420, #36422, #90891, #27067, #29397, #52406, #82907, #14924, #37919, #51920, #51421, #7422, #66916, #82404, #43906, #59898, #53384, #97437, #90390, #13930, #68408, #59405, #14424, #98930, #89910, #44894, #72562, #67913, #22419, #30385, #21424, #44406, #83894, #42097, #6915, #4096, #34559, #98435, #52893, #65054, #58919, #20933, #39390, #93357, #9876, #7908, #63346, #78356, #23901, #69884, #16388, #8872, #32846, #61870, #69386, #47850, #40375, #15898, #1404, #84881, #55864, #15424, #53893, #24882, #432, #8390, #46389, #84399, #70876, #31858, #54858, #46873, #54370, #2393, #85371, #76875, #62357, #93852, #76392, #25379, #77363, #55366, #92861, #23409, #45905, #38900, #38403, #16882, #91887, #24391, #47358, #77860, #9370, #908, #70380, #39873, #68904, #1899, #30882, #62862, #61379, #32355, #85869 ) ),
 .UNSPECIFIED., .F., .F., .F. ) 
 B_SPLINE_SURFACE_WITH_KNOTS ( ( 2, 2 ),
 ( 3, 2, 2, 2, 2, 2, 2, 2, 2, 2, 2, 2, 2, 2, 2, 2, 2, 2, 2, 2, 2, 2, 2, 2, 2, 2, 2, 2, 2, 2, 2, 2, 2, 2, 2, 2, 2, 2, 2, 2, 2, 2, 2, 2, 2, 2, 2, 2, 2, 2, 2, 2, 2, 2, 2, 2, 2, 2, 2, 2, 2, 2, 2, 2, 2, 2, 2, 2, 2, 2, 2, 2, 2, 2, 2, 2, 2, 2, 2, 2, 2, 2, 2, 2, 2, 2, 2, 2, 2, 2, 2, 2, 2, 2, 2, 2, 2, 2, 2, 2, 2, 2, 2, 2, 2, 2, 2, 2, 2, 2, 2, 2, 2, 2, 2, 2, 2, 2, 2, 2, 2, 2, 2, 2, 2, 2, 2, 2, 2, 2, 2, 2, 2, 2, 2, 2, 2, 2, 2, 2, 2, 2, 2, 2, 2, 2, 2, 2, 2, 2, 2, 2, 2, 2, 2, 2, 2, 2, 2, 2, 2, 2, 3 ),
 ( 0.000000000000000000, 1.000000000000000000 ),
 ( 0.000000000000000000, 0.005952380952380952051, 0.01190476190476190410, 0.01785714285714285615, 0.02380952380952380820, 0.02976190476190476025, 0.03571428571428571230, 0.04166666666666666435, 0.04761904761904761640, 0.05357142857142856845, 0.05952380952380952051, 0.06547619047619047949, 0.07142857142857142461, 0.07738095238095238360, 0.08333333333333332871, 0.08928571428571428770, 0.09523809523809523281, 0.1011904761904761918, 0.1071428571428571369, 0.1130952380952380959, 0.1190476190476190410, 0.1250000000000000000, 0.1309523809523809590, 0.1369047619047619180, 0.1428571428571428492, 0.1488095238095238082, 0.1547619047619047672, 0.1607142857142857262, 0.1666666666666666574, 0.1726190476190476164, 0.1785714285714285754, 0.1845238095238095344, 0.1904761904761904656, 0.1964285714285714246, 0.2023809523809523836, 0.2083333333333333426, 0.2142857142857142738, 0.2202380952380952328, 0.2261904761904761918, 0.2321428571428571508, 0.2380952380952380820, 0.2440476190476190410, 0.2500000000000000000, 0.2559523809523809312, 0.2619047619047619180, 0.2678571428571428492, 0.2738095238095238360, 0.2797619047619047672, 0.2857142857142856984, 0.2916666666666666852, 0.2976190476190476164, 0.3035714285714285476, 0.3095238095238095344, 0.3154761904761904656, 0.3214285714285714524, 0.3273809523809523836, 0.3333333333333333148, 0.3392857142857143016, 0.3452380952380952328, 0.3511904761904761640, 0.3571428571428571508, 0.3630952380952380820, 0.3690476190476190688, 0.3750000000000000000, 0.3809523809523809312, 0.3869047619047619180, 0.3928571428571428492, 0.3988095238095238360, 0.4047619047619047672, 0.4107142857142856984, 0.4166666666666666852, 0.4226190476190476164, 0.4285714285714285476, 0.4345238095238095344, 0.4404761904761904656, 0.4464285714285714524, 0.4523809523809523836, 0.4583333333333333148, 0.4642857142857143016, 0.4702380952380952328, 0.4761904761904761640, 0.4821428571428571508, 0.4880952380952380820, 0.4940476190476190688, 0.5000000000000000000, 0.5059523809523809312, 0.5119047619047618625, 0.5178571428571429047, 0.5238095238095238360, 0.5297619047619047672, 0.5357142857142856984, 0.5416666666666666297, 0.5476190476190476719, 0.5535714285714286031, 0.5595238095238095344, 0.5654761904761904656, 0.5714285714285713969, 0.5773809523809523281, 0.5833333333333333703, 0.5892857142857143016, 0.5952380952380952328, 0.6011904761904761640, 0.6071428571428570953, 0.6130952380952381375, 0.6190476190476190688, 0.6250000000000000000, 0.6309523809523809312, 0.6369047619047618625, 0.6428571428571429047, 0.6488095238095238360, 0.6547619047619047672, 0.6607142857142856984, 0.6666666666666666297, 0.6726190476190476719, 0.6785714285714286031, 0.6845238095238095344, 0.6904761904761904656, 0.6964285714285713969, 0.7023809523809523281, 0.7083333333333333703, 0.7142857142857143016, 0.7202380952380952328, 0.7261904761904761640, 0.7321428571428570953, 0.7380952380952381375, 0.7440476190476190688, 0.7500000000000000000, 0.7559523809523809312, 0.7619047619047618625, 0.7678571428571429047, 0.7738095238095238360, 0.7797619047619047672, 0.7857142857142856984, 0.7916666666666666297, 0.7976190476190476719, 0.8035714285714286031, 0.8095238095238095344, 0.8154761904761904656, 0.8214285714285713969, 0.8273809523809523281, 0.8333333333333333703, 0.8392857142857143016, 0.8452380952380952328, 0.8511904761904761640, 0.8571428571428570953, 0.8630952380952381375, 0.8690476190476190688, 0.8750000000000000000, 0.8809523809523809312, 0.8869047619047618625, 0.8928571428571429047, 0.8988095238095238360, 0.9047619047619047672, 0.9107142857142856984, 0.9166666666666666297, 0.9226190476190476719, 0.9285714285714286031, 0.9345238095238095344, 0.9404761904761904656, 0.9464285714285713969, 0.9523809523809523281, 0.9583333333333333703, 0.9642857142857143016 ),
 .UNSPECIFIED. ) 
 GEOMETRIC_REPRESENTATION_ITEM ( )  RATIONAL_B_SPLINE_SURFACE ( (
 ( 1.000000000000000000, 0.9659258262890683122, 1.000000000000000000, 0.9659258262890683122, 1.000000000000000000, 0.9659258262890683122, 1.000000000000000000, 0.9659258262890683122, 1.000000000000000000, 0.9659258262890683122, 1.000000000000000000, 0.9659258262890683122, 1.000000000000000000, 0.9659258262890683122, 1.000000000000000000, 0.9659258262890683122, 1.000000000000000000, 0.9659258262890683122, 1.000000000000000000, 0.9659258262890683122, 1.000000000000000000, 0.9659258262890683122, 1.000000000000000000, 0.9659258262890683122, 1.000000000000000000, 0.9659258262890683122, 1.000000000000000000, 0.9659258262890683122, 1.000000000000000000, 0.9659258262890683122, 1.000000000000000000, 0.9659258262890683122, 1.000000000000000000, 0.9659258262890683122, 1.000000000000000000, 0.9659258262890683122, 1.000000000000000000, 0.9659258262890683122, 1.000000000000000000, 0.9659258262890683122, 1.000000000000000000, 0.9659258262890683122, 1.000000000000000000, 0.9659258262890683122, 1.000000000000000000, 0.9659258262890683122, 1.000000000000000000, 0.9659258262890683122, 1.000000000000000000, 0.9659258262890683122, 1.000000000000000000, 0.9659258262890683122, 1.000000000000000000, 0.9659258262890683122, 1.000000000000000000, 0.9659258262890683122, 1.000000000000000000, 0.9659258262890683122, 1.000000000000000000, 0.9659258262890683122, 1.000000000000000000, 0.9659258262890683122, 1.000000000000000000, 0.9659258262890683122, 1.000000000000000000, 0.9659258262890683122, 1.000000000000000000, 0.9659258262890683122, 1.000000000000000000, 0.9659258262890683122, 1.000000000000000000, 0.9659258262890683122, 1.000000000000000000, 0.9659258262890683122, 1.000000000000000000, 0.9659258262890683122, 1.000000000000000000, 0.9659258262890683122, 1.000000000000000000, 0.9659258262890683122, 1.000000000000000000, 0.9659258262890683122, 1.000000000000000000, 0.9659258262890683122, 1.000000000000000000, 0.9659258262890683122, 1.000000000000000000, 0.9659258262890683122, 1.000000000000000000, 0.9659258262890683122, 1.000000000000000000, 0.9659258262890683122, 1.000000000000000000, 0.9659258262890683122, 1.000000000000000000, 0.9659258262890683122, 1.000000000000000000, 0.9659258262890683122, 1.000000000000000000, 0.9659258262890683122, 1.000000000000000000, 0.9659258262890683122, 1.000000000000000000, 0.9659258262890683122, 1.000000000000000000, 0.9659258262890683122, 1.000000000000000000, 0.9659258262890683122, 1.000000000000000000, 0.9659258262890683122, 1.000000000000000000, 0.9659258262890683122, 1.000000000000000000, 0.9659258262890683122, 1.000000000000000000, 0.9659258262890683122, 1.000000000000000000, 0.9659258262890683122, 1.000000000000000000, 0.9659258262890683122, 1.000000000000000000, 0.9659258262890683122, 1.000000000000000000, 0.9659258262890683122, 1.000000000000000000, 0.9659258262890683122, 1.000000000000000000, 0.9659258262890683122, 1.000000000000000000, 0.9659258262890683122, 1.000000000000000000, 0.9659258262890683122, 1.000000000000000000, 0.9659258262890683122, 1.000000000000000000, 0.9659258262890683122, 1.000000000000000000, 0.9659258262890683122, 1.000000000000000000, 0.9659258262890683122, 1.000000000000000000, 0.9659258262890683122, 1.000000000000000000, 0.9659258262890683122, 1.000000000000000000, 0.9659258262890683122, 1.000000000000000000, 0.9659258262890683122, 1.000000000000000000, 0.9659258262890683122, 1.000000000000000000, 0.9659258262890683122, 1.000000000000000000, 0.9659258262890683122, 1.000000000000000000, 0.9659258262890683122, 1.000000000000000000, 0.9659258262890683122, 1.000000000000000000, 0.9659258262890683122, 1.000000000000000000, 0.9659258262890683122, 1.000000000000000000, 0.9659258262890683122, 1.000000000000000000, 0.9659258262890683122, 1.000000000000000000, 0.9659258262890683122, 1.000000000000000000, 0.9659258262890683122, 1.000000000000000000, 0.9659258262890683122, 1.000000000000000000, 0.9659258262890683122, 1.000000000000000000, 0.9659258262890683122, 1.000000000000000000, 0.9659258262890683122, 1.000000000000000000, 0.9659258262890683122, 1.000000000000000000, 0.9659258262890683122, 1.000000000000000000, 0.9659258262890683122, 1.000000000000000000, 0.9659258262890683122, 1.000000000000000000, 0.9659258262890683122, 1.000000000000000000, 0.9659258262890683122, 1.000000000000000000, 0.9659258262890683122, 1.000000000000000000, 0.9659258262890683122, 1.000000000000000000, 0.9659258262890683122, 1.000000000000000000, 0.9659258262890683122, 1.000000000000000000, 0.9659258262890683122, 1.000000000000000000, 0.9659258262890683122, 1.000000000000000000, 0.9659258262890683122, 1.000000000000000000, 0.9659258262890683122, 1.000000000000000000, 0.9659258262890683122, 1.000000000000000000, 0.9659258262890683122, 1.000000000000000000, 0.9659258262890683122, 1.000000000000000000, 0.9659258262890683122, 1.000000000000000000, 0.9659258262890683122, 1.000000000000000000, 0.9659258262890683122, 1.000000000000000000, 0.9659258262890683122, 1.000000000000000000, 0.9659258262890683122, 1.000000000000000000, 0.9659258262890683122, 1.000000000000000000, 0.9659258262890683122, 1.000000000000000000, 0.9659258262890683122, 1.000000000000000000, 0.9659258262890683122, 1.000000000000000000, 0.9659258262890683122, 1.000000000000000000, 0.9659258262890683122, 1.000000000000000000, 0.9659258262890683122, 1.000000000000000000, 0.9659258262890683122, 1.000000000000000000, 0.9659258262890683122, 1.000000000000000000, 0.9659258262890683122, 1.000000000000000000, 0.9659258262890683122, 1.000000000000000000, 0.9659258262890683122, 1.000000000000000000, 0.9659258262890683122, 1.000000000000000000, 0.9659258262890683122, 1.000000000000000000, 0.9659258262890683122, 1.000000000000000000, 0.9659258262890683122, 1.000000000000000000, 0.9659258262890683122, 1.000000000000000000, 0.9659258262890683122, 1.000000000000000000, 0.9659258262890683122, 1.000000000000000000, 0.9659258262890683122, 1.000000000000000000, 0.9659258262890683122, 1.000000000000000000, 0.9659258262890683122, 1.000000000000000000, 0.9659258262890683122, 1.000000000000000000, 0.9659258262890683122, 1.000000000000000000, 0.9659258262890683122, 1.000000000000000000, 0.9659258262890683122, 1.000000000000000000, 0.9659258262890683122, 1.000000000000000000, 0.9659258262890683122, 1.000000000000000000, 0.9659258262890683122, 1.000000000000000000, 0.9659258262890683122, 1.000000000000000000, 0.9659258262890683122, 1.000000000000000000, 0.9659258262890683122, 1.000000000000000000, 0.9659258262890683122, 1.000000000000000000, 0.9659258262890683122, 1.000000000000000000, 0.9659258262890683122, 1.000000000000000000, 0.9659258262890683122, 1.000000000000000000, 0.9659258262890683122, 1.000000000000000000, 0.9659258262890683122, 1.000000000000000000, 0.9659258262890683122, 1.000000000000000000, 0.9659258262890683122, 1.000000000000000000, 0.9659258262890683122, 1.000000000000000000, 0.9659258262890683122, 1.000000000000000000, 0.9659258262890683122, 1.000000000000000000, 0.9659258262890683122, 1.000000000000000000, 0.9659258262890683122, 1.000000000000000000, 0.9659258262890683122, 1.000000000000000000, 0.9659258262890683122, 1.000000000000000000, 0.9659258262890683122, 1.000000000000000000, 0.9659258262890683122, 1.000000000000000000, 0.9659258262890683122, 1.000000000000000000, 0.9659258262890683122, 1.000000000000000000),
 ( 1.000000000000000000, 0.9659258262890683122, 1.000000000000000000, 0.9659258262890683122, 1.000000000000000000, 0.9659258262890683122, 1.000000000000000000, 0.9659258262890683122, 1.000000000000000000, 0.9659258262890683122, 1.000000000000000000, 0.9659258262890683122, 1.000000000000000000, 0.9659258262890683122, 1.000000000000000000, 0.9659258262890683122, 1.000000000000000000, 0.9659258262890683122, 1.000000000000000000, 0.9659258262890683122, 1.000000000000000000, 0.9659258262890683122, 1.000000000000000000, 0.9659258262890683122, 1.000000000000000000, 0.9659258262890683122, 1.000000000000000000, 0.9659258262890683122, 1.000000000000000000, 0.9659258262890683122, 1.000000000000000000, 0.9659258262890683122, 1.000000000000000000, 0.9659258262890683122, 1.000000000000000000, 0.9659258262890683122, 1.000000000000000000, 0.9659258262890683122, 1.000000000000000000, 0.9659258262890683122, 1.000000000000000000, 0.9659258262890683122, 1.000000000000000000, 0.9659258262890683122, 1.000000000000000000, 0.9659258262890683122, 1.000000000000000000, 0.9659258262890683122, 1.000000000000000000, 0.9659258262890683122, 1.000000000000000000, 0.9659258262890683122, 1.000000000000000000, 0.9659258262890683122, 1.000000000000000000, 0.9659258262890683122, 1.000000000000000000, 0.9659258262890683122, 1.000000000000000000, 0.9659258262890683122, 1.000000000000000000, 0.9659258262890683122, 1.000000000000000000, 0.9659258262890683122, 1.000000000000000000, 0.9659258262890683122, 1.000000000000000000, 0.9659258262890683122, 1.000000000000000000, 0.9659258262890683122, 1.000000000000000000, 0.9659258262890683122, 1.000000000000000000, 0.9659258262890683122, 1.000000000000000000, 0.9659258262890683122, 1.000000000000000000, 0.9659258262890683122, 1.000000000000000000, 0.9659258262890683122, 1.000000000000000000, 0.9659258262890683122, 1.000000000000000000, 0.9659258262890683122, 1.000000000000000000, 0.9659258262890683122, 1.000000000000000000, 0.9659258262890683122, 1.000000000000000000, 0.9659258262890683122, 1.000000000000000000, 0.9659258262890683122, 1.000000000000000000, 0.9659258262890683122, 1.000000000000000000, 0.9659258262890683122, 1.000000000000000000, 0.9659258262890683122, 1.000000000000000000, 0.9659258262890683122, 1.000000000000000000, 0.9659258262890683122, 1.000000000000000000, 0.9659258262890683122, 1.000000000000000000, 0.9659258262890683122, 1.000000000000000000, 0.9659258262890683122, 1.000000000000000000, 0.9659258262890683122, 1.000000000000000000, 0.9659258262890683122, 1.000000000000000000, 0.9659258262890683122, 1.000000000000000000, 0.9659258262890683122, 1.000000000000000000, 0.9659258262890683122, 1.000000000000000000, 0.9659258262890683122, 1.000000000000000000, 0.9659258262890683122, 1.000000000000000000, 0.9659258262890683122, 1.000000000000000000, 0.9659258262890683122, 1.000000000000000000, 0.9659258262890683122, 1.000000000000000000, 0.9659258262890683122, 1.000000000000000000, 0.9659258262890683122, 1.000000000000000000, 0.9659258262890683122, 1.000000000000000000, 0.9659258262890683122, 1.000000000000000000, 0.9659258262890683122, 1.000000000000000000, 0.9659258262890683122, 1.000000000000000000, 0.9659258262890683122, 1.000000000000000000, 0.9659258262890683122, 1.000000000000000000, 0.9659258262890683122, 1.000000000000000000, 0.9659258262890683122, 1.000000000000000000, 0.9659258262890683122, 1.000000000000000000, 0.9659258262890683122, 1.000000000000000000, 0.9659258262890683122, 1.000000000000000000, 0.9659258262890683122, 1.000000000000000000, 0.9659258262890683122, 1.000000000000000000, 0.9659258262890683122, 1.000000000000000000, 0.9659258262890683122, 1.000000000000000000, 0.9659258262890683122, 1.000000000000000000, 0.9659258262890683122, 1.000000000000000000, 0.9659258262890683122, 1.000000000000000000, 0.9659258262890683122, 1.000000000000000000, 0.9659258262890683122, 1.000000000000000000, 0.9659258262890683122, 1.000000000000000000, 0.9659258262890683122, 1.000000000000000000, 0.9659258262890683122, 1.000000000000000000, 0.9659258262890683122, 1.000000000000000000, 0.9659258262890683122, 1.000000000000000000, 0.9659258262890683122, 1.000000000000000000, 0.9659258262890683122, 1.000000000000000000, 0.9659258262890683122, 1.000000000000000000, 0.9659258262890683122, 1.000000000000000000, 0.9659258262890683122, 1.000000000000000000, 0.9659258262890683122, 1.000000000000000000, 0.9659258262890683122, 1.000000000000000000, 0.9659258262890683122, 1.000000000000000000, 0.9659258262890683122, 1.000000000000000000, 0.9659258262890683122, 1.000000000000000000, 0.9659258262890683122, 1.000000000000000000, 0.9659258262890683122, 1.000000000000000000, 0.9659258262890683122, 1.000000000000000000, 0.9659258262890683122, 1.000000000000000000, 0.9659258262890683122, 1.000000000000000000, 0.9659258262890683122, 1.000000000000000000, 0.9659258262890683122, 1.000000000000000000, 0.9659258262890683122, 1.000000000000000000, 0.9659258262890683122, 1.000000000000000000, 0.9659258262890683122, 1.000000000000000000, 0.9659258262890683122, 1.000000000000000000, 0.9659258262890683122, 1.000000000000000000, 0.9659258262890683122, 1.000000000000000000, 0.9659258262890683122, 1.000000000000000000, 0.9659258262890683122, 1.000000000000000000, 0.9659258262890683122, 1.000000000000000000, 0.9659258262890683122, 1.000000000000000000, 0.9659258262890683122, 1.000000000000000000, 0.9659258262890683122, 1.000000000000000000, 0.9659258262890683122, 1.000000000000000000, 0.9659258262890683122, 1.000000000000000000, 0.9659258262890683122, 1.000000000000000000, 0.9659258262890683122, 1.000000000000000000, 0.9659258262890683122, 1.000000000000000000, 0.9659258262890683122, 1.000000000000000000, 0.9659258262890683122, 1.000000000000000000, 0.9659258262890683122, 1.000000000000000000, 0.9659258262890683122, 1.000000000000000000, 0.9659258262890683122, 1.000000000000000000, 0.9659258262890683122, 1.000000000000000000, 0.9659258262890683122, 1.000000000000000000, 0.9659258262890683122, 1.000000000000000000, 0.9659258262890683122, 1.000000000000000000, 0.9659258262890683122, 1.000000000000000000, 0.9659258262890683122, 1.000000000000000000, 0.9659258262890683122, 1.000000000000000000, 0.9659258262890683122, 1.000000000000000000, 0.9659258262890683122, 1.000000000000000000, 0.9659258262890683122, 1.000000000000000000, 0.9659258262890683122, 1.000000000000000000, 0.9659258262890683122, 1.000000000000000000, 0.9659258262890683122, 1.000000000000000000, 0.9659258262890683122, 1.000000000000000000, 0.9659258262890683122, 1.000000000000000000, 0.9659258262890683122, 1.000000000000000000, 0.9659258262890683122, 1.000000000000000000, 0.9659258262890683122, 1.000000000000000000, 0.9659258262890683122, 1.000000000000000000, 0.9659258262890683122, 1.000000000000000000, 0.9659258262890683122, 1.000000000000000000, 0.9659258262890683122, 1.000000000000000000, 0.9659258262890683122, 1.000000000000000000, 0.9659258262890683122, 1.000000000000000000, 0.9659258262890683122, 1.000000000000000000, 0.9659258262890683122, 1.000000000000000000, 0.9659258262890683122, 1.000000000000000000, 0.9659258262890683122, 1.000000000000000000, 0.9659258262890683122, 1.000000000000000000, 0.9659258262890683122, 1.000000000000000000, 0.9659258262890683122, 1.000000000000000000, 0.9659258262890683122, 1.000000000000000000) ) ) 
 REPRESENTATION_ITEM ( '' )  SURFACE ( )  );
#49834 = CARTESIAN_POINT ( 'NONE',  ( 0.5774900079438590739, 52.64701867748817676, -5.440088680355550821 ) ) ;
#49835 = CARTESIAN_POINT ( 'NONE',  ( 19.84674366389459266, 48.30059781766745175, 2.638427012816836559 ) ) ;
#49836 = CARTESIAN_POINT ( 'NONE',  ( 22.81628187352647785, 41.41530133659708923, 3.434112377981063169 ) ) ;
#49838 = LINE ( 'NONE', #19838, #43092 ) ;
#49837 = CARTESIAN_POINT ( 'NONE',  ( 19.42250999205614193, 10.14701867748816966, 5.440088680355555262 ) ) ;
#49839 = CARTESIAN_POINT ( 'NONE',  ( 10.00000000000000178, 64.31368534415483396, 10.88017736071110342 ) ) ;
#49840 = CARTESIAN_POINT ( 'NONE',  ( -0.8801773607111009756, 8.063685344154837509, 1.068504757029289695E-15 ) ) ;
#49841 = EDGE_CURVE ( 'NONE', #74297, #87937, #59745, .T. ) ;
#49842 = VECTOR ( 'NONE', #18760, 1000.000000000000000 ) ;
#49843 = VERTEX_POINT ( 'NONE', #80283 ) ;
#49844 = CARTESIAN_POINT ( 'NONE',  ( 6.565887622018943937, 45.16530133659708923, 12.81628187352647430 ) ) ;
#49845 = CARTESIAN_POINT ( 'NONE',  ( 10.00000000000000000, 36.81368534415484106, -10.88017736071110342 ) ) ;
#49846 = DIRECTION ( 'NONE',  ( 0.000000000000000000, 0.000000000000000000, -1.000000000000000000 ) ) ;
#49847 = ORIENTED_EDGE ( 'NONE', *, *, #63640, .F. ) ;
#49848 = CARTESIAN_POINT ( 'NONE',  ( 10.00000000000000000, 47.87363466993042493, -12.81628187352647608 ) ) ;
#49849 = CARTESIAN_POINT ( 'NONE',  ( 17.96484262340118221, 29.93868534415484106, 7.964842623401181321 ) ) ;
#49850 = CARTESIAN_POINT ( 'NONE',  ( 5.076628168052703671, 51.84226448433412315, 8.527530157486179263 ) ) ;
#49851 = ORIENTED_EDGE ( 'NONE', *, *, #32507, .F. ) ;
#49852 = VECTOR ( 'NONE', #59542, 999.9999999999998863 ) ;
#49853 = VECTOR ( 'NONE', #30841, 1000.000000000000000 ) ;
#49854 = CARTESIAN_POINT ( 'NONE',  ( 19.84674366389459621, 58.50893115100078745, 7.409399052514197653E-17 ) ) ;
#49856 = CARTESIAN_POINT ( 'NONE',  ( 1.472469842513823179, 45.59226448433412315, -4.923371831947296329 ) ) ;
#49855 = FACE_OUTER_BOUND ( 'NONE', #37692, .T. ) ;
#49857 = CARTESIAN_POINT ( 'NONE',  ( 17.96484262340118221, 26.18868534415483396, -7.964842623401177768 ) ) ;
#49858 = FACE_OUTER_BOUND ( 'NONE', #97906, .T. ) ;
#49859 = DIRECTION ( 'NONE',  ( 0.000000000000000000, 0.000000000000000000, 1.000000000000000000 ) ) ;
#49860 = LINE ( 'NONE', #9916, #86744 ) ;
#49861 = CARTESIAN_POINT ( 'NONE',  ( 7.361572987183169658, 39.96726448433411605, -9.846743663894592657 ) ) ;
#49863 = ORIENTED_EDGE ( 'NONE', *, *, #25425, .F. ) ;
#49862 = CARTESIAN_POINT ( 'NONE',  ( 5.076628168052703671, 56.84226448433412315, 8.527530157486179263 ) ) ;
#49864 = B_SPLINE_CURVE_WITH_KNOTS ( 'NONE', 3,
 ( #34401, #72900, #4919, #18934, #95417, #87903 ),
 .UNSPECIFIED., .F., .F.,
 ( 4, 2, 4 ),
 ( 0.000000000000000000, 0.0002626113303184859395, 0.0005252226606369718789 ),
 .UNSPECIFIED. ) ;
#49865 = CARTESIAN_POINT ( 'NONE',  ( 16.40814093676323893, 35.79030133659708923, 11.09922568453595026 ) ) ;
#49866 = CARTESIAN_POINT ( 'NONE',  ( 19.84674366389459621, 48.50893115100078745, 7.409399052514197653E-17 ) ) ;
#49867 = DIRECTION ( 'NONE',  ( -0.6225146366376236307, 0.000000000000000000, 0.7826081568524105858 ) ) ;
#49868 = CARTESIAN_POINT ( 'NONE',  ( 10.00000000000000178, 63.05374883491396076, 14.16423886937410082 ) ) ;
#49869 = CARTESIAN_POINT ( 'NONE',  ( 5.076628168052704559, 30.17559781766745175, -8.527530157486179263 ) ) ;
#49870 = EDGE_LOOP ( 'NONE', ( #56697, #87223, #37952, #23722 ) ) ;
#49871 = PLANE ( 'NONE',  #7322 ) ;
#49872 = CARTESIAN_POINT ( 'NONE',  ( -4.164238869374099927, 57.01208216824731068, 3.795296366450308767 ) ) ;
#49873 = CARTESIAN_POINT ( 'NONE',  ( 12.67122524790590710, 14.95077488074853456, -7.555537761805753760 ) ) ;
#49874 = CARTESIAN_POINT ( 'NONE',  ( 4.559911319644449179, 8.897018677488173211, 9.422509992056141925 ) ) ;
#49875 = CIRCLE ( 'NONE', #46751, 0.5000000000000004441 ) ;
#49876 = CARTESIAN_POINT ( 'NONE',  ( 17.08211943468705130, 33.47041550158063927, 12.26659068614894998 ) ) ;
#49878 = CARTESIAN_POINT ( 'NONE',  ( 0.2751277870542980231, 10.30223176428831522, 6.500000000000002665 ) ) ;
#49877 = CARTESIAN_POINT ( 'NONE',  ( -0.3689425029237881626, 42.42874883491396787, 10.36894250292379027 ) ) ;
#49879 = CARTESIAN_POINT ( 'NONE',  ( 6.829574850505126804, -88.00372650098204019, 2.750000000000002665 ) ) ;
#49880 = CARTESIAN_POINT ( 'NONE',  ( 12.63842701281683034, 17.46726448433411250, 9.846743663894596210 ) ) ;
#49882 = CARTESIAN_POINT ( 'NONE',  ( 14.92337183194729988, 64.34226448433412315, -8.527530157486177487 ) ) ;
#49881 = CARTESIAN_POINT ( 'NONE',  ( 0.2751277870542967463, 70.00000000000000000, 6.000000000000000000 ) ) ;
#49883 = ORIENTED_EDGE ( 'NONE', *, *, #19548, .F. ) ;
#49884 = CARTESIAN_POINT ( 'NONE',  ( 12.91533473730992121, 49.52201867748817676, 10.88017736071110164 ) ) ;
#49885 = FILL_AREA_STYLE_COLOUR ( '', #75234 ) ;
#49886 = CARTESIAN_POINT ( 'NONE',  ( 12.63842701281683034, 47.46726448433412315, 9.846743663894596210 ) ) ;
#49887 = DIRECTION ( 'NONE',  ( -0.000000000000000000, -0.000000000000000000, -1.000000000000000000 ) ) ;
#49888 = CARTESIAN_POINT ( 'NONE',  ( 17.20831665107776587, 52.88393115100078035, 7.208316651077764980 ) ) ;
#49889 = DIRECTION ( 'NONE',  ( 0.000000000000000000, 0.000000000000000000, 1.000000000000000000 ) ) ;
#49890 = EDGE_CURVE ( 'NONE', #35983, #44442, #4299, .T. ) ;
#49891 = VECTOR ( 'NONE', #84426, 1000.000000000000000 ) ;
#49892 = VERTEX_POINT ( 'NONE', #5288 ) ;
#49893 = CARTESIAN_POINT ( 'NONE',  ( 22.26659068614895176, 24.72041550158063572, -7.082119434687042414 ) ) ;
#49894 = ADVANCED_FACE ( 'NONE', ( #5775 ), #65260, .T. ) ;
#49895 = EDGE_CURVE ( 'NONE', #20729, #16419, #77508, .T. ) ;
#49896 = CARTESIAN_POINT ( 'NONE',  ( -14.09394518620605297, 15.00000000000000000, -3.407449058785551710 ) ) ;
#49898 = CARTESIAN_POINT ( 'NONE',  ( -8.099999999999999645, 80.99999999999994316, 3.000000000000000000 ) ) ;
#49897 = CARTESIAN_POINT ( 'NONE',  ( -3.500000000000000444, 1.019547802438453887, -2.499999999999999556 ) ) ;
#49899 = CARTESIAN_POINT ( 'NONE',  ( 17.96484262340118221, 24.93868534415484461, 7.964842623401181321 ) ) ;
#49900 = CARTESIAN_POINT ( 'NONE',  ( 0.6178305044545838731, 24.74863466993042493, 9.382169495545420901 ) ) ;
#49901 = CARTESIAN_POINT ( 'NONE',  ( -5.963430220938290560, 8.854976035794180689, -10.32896413005679648 ) ) ;
#49902 = CARTESIAN_POINT ( 'NONE',  ( 12.63842701281683034, 7.467264484334118713, 9.846743663894596210 ) ) ;
#49903 = CARTESIAN_POINT ( 'NONE',  ( 3.591859063236763294, 53.29030133659708923, -11.09922568453595026 ) ) ;
#49904 = ORIENTED_EDGE ( 'NONE', *, *, #84212, .T. ) ;
#49905 = CARTESIAN_POINT ( 'NONE',  ( 6.575338752131433040, -50.90849809618014632, -3.750000000000000000 ) ) ;
#49906 = B_SPLINE_CURVE_WITH_KNOTS ( 'NONE', 3,
 ( #12607, #5122, #67098, #6592, #58096, #96625, #90084, #43108, #73595, #51105 ),
 .UNSPECIFIED., .F., .F.,
 ( 4, 3, 3, 4 ),
 ( 5.003707553108401214E-17, 0.0006253016069560650338, 0.001250604074564886812, 0.002501455912506567354 ),
 .UNSPECIFIED. ) ;
#49907 = CARTESIAN_POINT ( 'NONE',  ( 22.26659068614894466, 23.88708216824730357, 7.082119434687054849 ) ) ;
#49908 = CARTESIAN_POINT ( 'NONE',  ( 1.820328553599968036, 0.000000000000000000, -5.140449258537787891 ) ) ;
#49909 = CARTESIAN_POINT ( 'NONE',  ( -6.281451360760613944, -39.80862496263594608, 4.000000000000000000 ) ) ;
#49910 = CARTESIAN_POINT ( 'NONE',  ( 12.91533473730992121, 4.522018677488170546, 10.88017736071110164 ) ) ;
#49911 = DIRECTION ( 'NONE',  ( 0.000000000000000000, -1.000000000000000000, 0.000000000000000000 ) ) ;
#49912 = CARTESIAN_POINT ( 'NONE',  ( -1.326261724323127389, 14.76984959128327901, 14.88164196614432377 ) ) ;
#49913 = CARTESIAN_POINT ( 'NONE',  ( 7.084665262690076126, 37.02201867748817676, -10.88017736071110164 ) ) ;
#49914 = CARTESIAN_POINT ( 'NONE',  ( 20.88017736071110519, 50.56368534415484106, 2.639326808657452039E-16 ) ) ;
#49915 = CARTESIAN_POINT ( 'NONE',  ( -1.099225684535947600, 9.540301336597087456, 6.408140936763237150 ) ) ;
#49916 = DIRECTION ( 'NONE',  ( -0.000000000000000000, -1.000000000000000000, -0.000000000000000000 ) ) ;
#49917 = CARTESIAN_POINT ( 'NONE',  ( 0.5774900079438607392, 3.480352010821504916, 5.440088680355550821 ) ) ;
#49918 = CARTESIAN_POINT ( 'NONE',  ( 19.84674366389459266, 3.717264484334118713, -2.638427012816827677 ) ) ;
#49919 = CARTESIAN_POINT ( 'NONE',  ( 7.084665262690076126, 42.02201867748816966, -10.88017736071110164 ) ) ;
#49920 = AXIS2_PLACEMENT_3D ( 'NONE', #37109, #67605, #98112 ) ;
#49921 = CARTESIAN_POINT ( 'NONE',  ( 22.81628187352647785, 6.623634669930420493, 6.195893100308588602E-16 ) ) ;
#49922 = CARTESIAN_POINT ( 'NONE',  ( 20.88017736071110519, 60.56368534415484106, 2.639326808657452039E-16 ) ) ;
#49923 = CARTESIAN_POINT ( 'NONE',  ( 18.52753015748617571, 23.09226448433411960, 4.923371831947298993 ) ) ;
#49924 = CARTESIAN_POINT ( 'NONE',  ( 21.09922568453595559, 52.04030133659708923, -6.408140936763230044 ) ) ;
#49925 = AXIS2_PLACEMENT_3D ( 'NONE', #86999, #71028, #94008 ) ;
#49927 = CARTESIAN_POINT ( 'NONE',  ( -4.850115630859779259, 14.95077488074853456, 13.93278430610803831 ) ) ;
#49926 = CARTESIAN_POINT ( 'NONE',  ( 14.92337183194729633, 2.675597817667451750, 8.527530157486181039 ) ) ;
#49928 = AXIS2_PLACEMENT_3D ( 'NONE', #28967, #73982, #96010 ) ;
#49929 = ORIENTED_EDGE ( 'NONE', *, *, #10623, .T. ) ;
#49930 = CARTESIAN_POINT ( 'NONE',  ( 1.602071938427517495, 57.02224192338643149, -6.500000000000039080 ) ) ;
#49931 = CARTESIAN_POINT ( 'NONE',  ( 1.274849032794223680, 28.57228050351031001, 6.499999999999884537 ) ) ;
#49932 = CARTESIAN_POINT ( 'NONE',  ( 12.91533473730993009, 21.60535201082150536, -10.88017736071109987 ) ) ;
#49934 = CARTESIAN_POINT ( 'NONE',  ( -4.164238869374099039, 21.80374883491396787, 8.674139862899312516E-16 ) ) ;
#49933 = CARTESIAN_POINT ( 'NONE',  ( 19.38216949554541557, 57.24863466993042493, -9.382169495545420901 ) ) ;
#49935 = ADVANCED_FACE ( 'NONE', ( #42783 ), #16865, .F. ) ;
#49936 = CARTESIAN_POINT ( 'NONE',  ( 1.472469842513823179, 25.59226448433412315, -4.923371831947296329 ) ) ;
#49937 = AXIS2_PLACEMENT_3D ( 'NONE', #7928, #23431, #38425 ) ;
#49938 = CARTESIAN_POINT ( 'NONE',  ( 19.42250999205614193, 20.14701867748817321, 5.440088680355555262 ) ) ;
#49939 = CARTESIAN_POINT ( 'NONE',  ( 12.91533473730993009, 6.605352010821504471, -10.88017736071109987 ) ) ;
#49940 = ORIENTED_EDGE ( 'NONE', *, *, #1410, .F. ) ;
#49941 = AXIS2_PLACEMENT_3D ( 'NONE', #50072, #95579, #27066 ) ;
#49942 = CARTESIAN_POINT ( 'NONE',  ( 4.559911319644449179, 7.230352010821504471, -9.422509992056141925 ) ) ;
#49943 = CARTESIAN_POINT ( 'NONE',  ( 20.88017736071110164, 30.35535201082151247, 2.915334737309930979 ) ) ;
#49944 = ADVANCED_FACE ( 'NONE', ( #96287 ), #66303, .T. ) ;
#49946 = CARTESIAN_POINT ( 'NONE',  ( 0.5774900079438607392, 28.48035201082150891, 5.440088680355550821 ) ) ;
#49945 = CARTESIAN_POINT ( 'NONE',  ( -13.78891971893200186, 0.3640475087720986824, -5.904717858191729007 ) ) ;
#49947 = ORIENTED_EDGE ( 'NONE', *, *, #14472, .T. ) ;
#49948 = CARTESIAN_POINT ( 'NONE',  ( 17.20831665107776587, 64.13393115100079456, -7.208316651077762316 ) ) ;
#49949 = CARTESIAN_POINT ( 'NONE',  ( 0.5774900079438590739, 17.64701867748817321, -5.440088680355550821 ) ) ;
#49950 = CARTESIAN_POINT ( 'NONE',  ( 19.84674366389459266, 63.30059781766745886, 2.638427012816836559 ) ) ;
#49951 = CARTESIAN_POINT ( 'NONE',  ( 8.879999999999991900, 18.00000000000000355, 3.000000000000000000 ) ) ;
#49952 = CARTESIAN_POINT ( 'NONE',  ( -10.58981376305295008, 15.00000000000000000, 9.535111140613638625 ) ) ;
#49953 = CARTESIAN_POINT ( 'NONE',  ( -4.164238869374099927, 27.01208216824730357, 3.795296366450308767 ) ) ;
#49954 = CARTESIAN_POINT ( 'NONE',  ( 20.88017736071110519, 45.56368534415484106, 2.639326808657452039E-16 ) ) ;
#49955 = CARTESIAN_POINT ( 'NONE',  ( 4.559911319644449179, 17.23035201082150536, -9.422509992056141925 ) ) ;
#49956 = CARTESIAN_POINT ( 'NONE',  ( 19.72487221294570858, 9.782175860852373006, 6.500000000000000000 ) ) ;
#49957 = CARTESIAN_POINT ( 'NONE',  ( -11.58474105865894010, -69.55891867961692299, -3.750000000000000444 ) ) ;
#49958 = CARTESIAN_POINT ( 'NONE',  ( 1.472469842513823179, 51.42559781766745886, 4.923371831947296329 ) ) ;
#49959 = AXIS2_PLACEMENT_3D ( 'NONE', #25939, #93445, #24478 ) ;
#49960 = CARTESIAN_POINT ( 'NONE',  ( 19.84674366389459266, 18.71726448433411960, -2.638427012816827677 ) ) ;
#49961 = CARTESIAN_POINT ( 'NONE',  ( -11.09922568453595382, -36.29303199673623936, -6.408140936763226492 ) ) ;
#49962 = CARTESIAN_POINT ( 'NONE',  ( 12.91533473730992121, 14.52201867748817143, 10.88017736071110164 ) ) ;
#49963 = CARTESIAN_POINT ( 'NONE',  ( 1.472469842513823179, 16.42559781766745175, 4.923371831947296329 ) ) ;
#49964 = CARTESIAN_POINT ( 'NONE',  ( 17.96484262340118221, 54.93868534415484106, 7.964842623401181321 ) ) ;
#49966 = CARTESIAN_POINT ( 'NONE',  ( 22.81628187352647785, 61.41530133659709634, 3.434112377981063169 ) ) ;
#49965 = CARTESIAN_POINT ( 'NONE',  ( 15.44008868035555793, 16.39701867748817321, -9.422509992056140149 ) ) ;
#49967 = CARTESIAN_POINT ( 'NONE',  ( 10.00000000000000000, 25.55374883491396787, -14.16423886937410082 ) ) ;
#49968 = CIRCLE ( 'NONE', #40418, 0.5000000000000004441 ) ;
#49969 = DIRECTION ( 'NONE',  ( -0.000000000000000000, -1.000000000000000000, -0.000000000000000000 ) ) ;
#49970 = AXIS2_PLACEMENT_3D ( 'NONE', #15814, #37337, #7820 ) ;
#49971 = CARTESIAN_POINT ( 'NONE',  ( 19.38216949554541557, 62.24863466993041072, -9.382169495545420901 ) ) ;
#49972 = ORIENTED_EDGE ( 'NONE', *, *, #57106, .F. ) ;
#49973 = CARTESIAN_POINT ( 'NONE',  ( 22.81628187352647785, 6.623634669930420493, 6.195893100308588602E-16 ) ) ;
#49974 = CARTESIAN_POINT ( 'NONE',  ( -1.926860441876563801, 14.89664270246084143, 3.195792623639529761 ) ) ;
#49975 = CARTESIAN_POINT ( 'NONE',  ( -0.8801773607111009756, 38.06368534415484106, 1.068504757029289695E-15 ) ) ;
#49976 = CARTESIAN_POINT ( 'NONE',  ( 5.076628168052703671, 56.84226448433412315, 8.527530157486179263 ) ) ;
#49977 = VERTEX_POINT ( 'NONE', #50774 ) ;
#49979 = CARTESIAN_POINT ( 'NONE',  ( -12.60589901313228012, 0.3640475087720979053, 8.129656208641964810 ) ) ;
#49978 = CARTESIAN_POINT ( 'NONE',  ( 5.076628168052703671, 16.84226448433411960, 8.527530157486179263 ) ) ;
#49980 = CARTESIAN_POINT ( 'NONE',  ( 12.63842701281683922, 9.550597817667449974, -9.846743663894590881 ) ) ;
#49981 = CARTESIAN_POINT ( 'NONE',  ( 10.00000000000000000, 19.75893115100078390, -9.846743663894594434 ) ) ;
#49982 = CARTESIAN_POINT ( 'NONE',  ( 10.00000000000000000, 14.75893115100078568, -9.846743663894594434 ) ) ;
#49983 = CARTESIAN_POINT ( 'NONE',  ( 2.791683348922237240, 0.3839311510007847872, -7.208316651077763204 ) ) ;
#49984 = ADVANCED_FACE ( 'NONE', ( #61229, #31213 ), #61709, .T. ) ;
#49986 = DIRECTION ( 'NONE',  ( -0.9953961983671785196, 0.000000000000000000, -0.09584575252022721481 ) ) ;
#49985 = CARTESIAN_POINT ( 'NONE',  ( 20.88017736071110875, 60.77201867748817676, -2.915334737309920765 ) ) ;
#49987 = CARTESIAN_POINT ( 'NONE',  ( 5.076628168052704559, 0.1755978176674514724, -8.527530157486179263 ) ) ;
#49990 = ORIENTED_EDGE ( 'NONE', *, *, #52742, .F. ) ;
#49989 =( GEOMETRIC_REPRESENTATION_CONTEXT ( 3 ) GLOBAL_UNCERTAINTY_ASSIGNED_CONTEXT ( ( #45263 ) ) GLOBAL_UNIT_ASSIGNED_CONTEXT ( ( #11799, #88784, #65277 ) ) REPRESENTATION_CONTEXT ( 'NONE', 'WORKASPACE' ) );
#49988 = CARTESIAN_POINT ( 'NONE',  ( 7.361572987183170547, 22.05059781766745530, 9.846743663894590881 ) ) ;
#49991 = DIRECTION ( 'NONE',  ( -0.9366721892483947931, 0.000000000000000000, -0.3502073812594747038 ) ) ;
#49992 = CARTESIAN_POINT ( 'NONE',  ( -2.816281873526473856, 4.331968003263754419, 3.434112377981055619 ) ) ;
#49993 = ORIENTED_EDGE ( 'NONE', *, *, #61875, .T. ) ;
#49994 = ORIENTED_EDGE ( 'NONE', *, *, #80532, .T. ) ;
#49995 = DIRECTION ( 'NONE',  ( 0.000000000000000000, 0.000000000000000000, 1.000000000000000000 ) ) ;
#49996 = CARTESIAN_POINT ( 'NONE',  ( 24.16423886937409904, 19.09541550158063927, 3.795296366450317205 ) ) ;
#49997 = AXIS2_PLACEMENT_3D ( 'NONE', #50606, #90076, #21602 ) ;
#49998 = AXIS2_PLACEMENT_3D ( 'NONE', #35867, #19392, #81853 ) ;
#49999 = CARTESIAN_POINT ( 'NONE',  ( -10.58981376305295008, 0.000000000000000000, 9.535111140613638625 ) ) ;
#50000 = MECHANICAL_DESIGN_GEOMETRIC_PRESENTATION_REPRESENTATION (  '', ( #6909 ), #5344 ) ;
#50001 = CARTESIAN_POINT ( 'NONE',  ( 17.08211943468705840, 20.13708216824730357, -12.26659068614894466 ) ) ;
#50002 = CARTESIAN_POINT ( 'NONE',  ( 13.79529636645031943, 35.34541550158063927, -14.16423886937409904 ) ) ;
#50003 = PLANE ( 'NONE',  #65776 ) ;
#50004 = CARTESIAN_POINT ( 'NONE',  ( 19.42250999205614548, 35.98035201082151247, -5.440088680355545492 ) ) ;
#50005 = PRESENTATION_STYLE_ASSIGNMENT (( #87510 ) ) ;
#50006 = ORIENTED_EDGE ( 'NONE', *, *, #57583, .T. ) ;
#50008 = VECTOR ( 'NONE', #42859, 1000.000000000000114 ) ;
#50007 = CARTESIAN_POINT ( 'NONE',  ( 5.076628168052703671, 16.84226448433411960, 8.527530157486179263 ) ) ;
#50009 = ADVANCED_FACE ( 'NONE', ( #38251 ), #23256, .F. ) ;
#50011 = CARTESIAN_POINT ( 'NONE',  ( 18.52753015748618282, 13.92559781766745175, -4.923371831947291888 ) ) ;
#50010 = CARTESIAN_POINT ( 'NONE',  ( 12.91533473730993009, 61.60535201082150536, -10.88017736071109987 ) ) ;
#50012 = CARTESIAN_POINT ( 'NONE',  ( 17.96484262340118221, 4.938685344154837509, 7.964842623401181321 ) ) ;
#50013 = CARTESIAN_POINT ( 'NONE',  ( 22.81628187352648496, 51.83196800326376064, -3.434112377981050290 ) ) ;
#50014 = CARTESIAN_POINT ( 'NONE',  ( 1.472469842513823179, 55.59226448433412315, -4.923371831947296329 ) ) ;
#50015 = CARTESIAN_POINT ( 'NONE',  ( -0.1503990784575328643, 25.12777174578613426, 6.262539305110068177 ) ) ;
#50016 = CARTESIAN_POINT ( 'NONE',  ( -1.099225684535947600, 29.54030133659708923, 6.408140936763237150 ) ) ;
#50017 = CARTESIAN_POINT ( 'NONE',  ( 10.36894250292378850, -30.07125116508602858, -10.36894250292379027 ) ) ;
#50018 = CARTESIAN_POINT ( 'NONE',  ( 12.63842701281683922, 44.55059781766745175, -9.846743663894590881 ) ) ;
#50019 = EDGE_CURVE ( 'NONE', #71601, #70379, #83879, .T. ) ;
#50020 = CARTESIAN_POINT ( 'NONE',  ( -4.164238869374098151, 16.59541550158063927, -3.795296366450310543 ) ) ;
#50021 = ORIENTED_EDGE ( 'NONE', *, *, #20687, .F. ) ;
#50022 = DIRECTION ( 'NONE',  ( -0.000000000000000000, -1.000000000000000000, 0.000000000000000000 ) ) ;
#50023 = EDGE_CURVE ( 'NONE', #93536, #93548, #67759, .T. ) ;
#50024 = CARTESIAN_POINT ( 'NONE',  ( 15.44008868035555260, 49.73035201082150536, 9.422509992056143702 ) ) ;
#50025 = CARTESIAN_POINT ( 'NONE',  ( 4.559911319644449179, 52.23035201082151247, -9.422509992056141925 ) ) ;
#50026 = CARTESIAN_POINT ( 'NONE',  ( 2.917880565312950480, 40.97041550158063217, -12.26659068614894821 ) ) ;
#50027 = CARTESIAN_POINT ( 'NONE',  ( 14.92337183194729988, 59.34226448433412315, -8.527530157486177487 ) ) ;
#50028 = CARTESIAN_POINT ( 'NONE',  ( 7.313705784284503686, 0.5000000000000004441, 13.09617149020748705 ) ) ;
#50029 = CARTESIAN_POINT ( 'NONE',  ( 2.035157376598822676, 37.43868534415484106, -7.964842623401177768 ) ) ;
#50030 = CARTESIAN_POINT ( 'NONE',  ( -14.97687855664613465, 14.49999999999999112, -0.8325315005902816923 ) ) ;
#50031 = CARTESIAN_POINT ( 'NONE',  ( 1.472469842513823179, 55.59226448433412315, -4.923371831947296329 ) ) ;
#50032 = CARTESIAN_POINT ( 'NONE',  ( 10.88017736071110164, 20.35535201082150536, 2.915334737309921209 ) ) ;
#50033 = CARTESIAN_POINT ( 'NONE',  ( 20.88017736071110164, 5.355352010821502695, 2.915334737309930979 ) ) ;
#50034 = CARTESIAN_POINT ( 'NONE',  ( 7.084665262690076126, 62.02201867748816966, -10.88017736071110164 ) ) ;
#50035 = TOROIDAL_SURFACE ( 'NONE', #54802, 14.49999999999999822, 0.5000000000000000000 ) ;
#50036 = FACE_OUTER_BOUND ( 'NONE', #12716, .T. ) ;
#50037 = CARTESIAN_POINT ( 'NONE',  ( 2.035157376598822676, 62.43868534415483396, -7.964842623401177768 ) ) ;
#50039 = CARTESIAN_POINT ( 'NONE',  ( 0.1532563361054082862, 1.217264484334117824, 2.638427012816831674 ) ) ;
#50038 = AXIS2_PLACEMENT_3D ( 'NONE', #68941, #61909, #92903 ) ;
#50040 = CARTESIAN_POINT ( 'NONE',  ( 17.87804611792018150, 78.26090218833560641, -4.039389165979423879 ) ) ;
#50042 = B_SPLINE_CURVE_WITH_KNOTS ( 'NONE', 3,
 ( #16111, #8608, #85099, #62576, #9098, #23636 ),
 .UNSPECIFIED., .F., .F.,
 ( 4, 2, 4 ),
 ( 3.409110551496111039E-05, 0.0004400426677367854874, 0.0008459942299586098577 ),
 .UNSPECIFIED. ) ;
#50041 = CARTESIAN_POINT ( 'NONE',  ( 5.076628168052704559, 40.17559781766745175, -8.527530157486179263 ) ) ;
#50043 = CARTESIAN_POINT ( 'NONE',  ( 12.91533473730993009, 26.60535201082150536, -10.88017736071109987 ) ) ;
#50044 = CARTESIAN_POINT ( 'NONE',  ( 3.591859063236763294, 8.290301336597087456, -11.09922568453595026 ) ) ;
#50046 = CARTESIAN_POINT ( 'NONE',  ( -3.627897627657490798, -3.626520239197509987, -3.750000000000000444 ) ) ;
#50045 = CARTESIAN_POINT ( 'NONE',  ( 4.559911319644449179, 33.89701867748817676, 9.422509992056141925 ) ) ;
#50047 = FILL_AREA_STYLE_COLOUR ( '', #75278 ) ;
#50048 = CARTESIAN_POINT ( 'NONE',  ( 13.43411237798105340, 35.58196800326375353, 12.81628187352647963 ) ) ;
#50049 = ORIENTED_EDGE ( 'NONE', *, *, #76418, .F. ) ;
#50050 = CARTESIAN_POINT ( 'NONE',  ( -0.8801773607111009756, 58.06368534415484106, 1.068504757029289695E-15 ) ) ;
#50052 = DIRECTION ( 'NONE',  ( 0.000000000000000000, 0.000000000000000000, 1.000000000000000000 ) ) ;
#50051 = CARTESIAN_POINT ( 'NONE',  ( -2.816281873526473856, 19.12363466993042138, 9.499525473075851096E-16 ) ) ;
#50053 = EDGE_CURVE ( 'NONE', #69049, #59353, #10434, .T. ) ;
#50054 = DIRECTION ( 'NONE',  ( -1.000000000000000000, 0.000000000000000000, 0.000000000000000000 ) ) ;
#50055 = CARTESIAN_POINT ( 'NONE',  ( 20.88017736071110519, 20.56368534415484106, 2.639326808657452039E-16 ) ) ;
#50056 = CARTESIAN_POINT ( 'NONE',  ( -0.3689425029237881626, 67.42874883491396076, 10.36894250292379027 ) ) ;
#50057 = CARTESIAN_POINT ( 'NONE',  ( 19.84674366389459266, 58.30059781766745886, 2.638427012816836559 ) ) ;
#50058 = CARTESIAN_POINT ( 'NONE',  ( -0.8801773607111008646, 68.27201867748817676, 2.915334737309923430 ) ) ;
#50059 = CARTESIAN_POINT ( 'NONE',  ( 19.42250999205614548, 65.98035201082151957, -5.440088680355545492 ) ) ;
#50060 = CARTESIAN_POINT ( 'NONE',  ( -8.375939845167836850, 15.00000000000000000, 11.52849216984293257 ) ) ;
#50061 = CARTESIAN_POINT ( 'NONE',  ( -2.266590686148945544, 36.38708216824730357, -7.082119434687050408 ) ) ;
#50062 = FACE_OUTER_BOUND ( 'NONE', #6536, .T. ) ;
#50063 = ADVANCED_FACE ( 'NONE', ( #39236 ), #39204, .T. ) ;
#50064 = CARTESIAN_POINT ( 'NONE',  ( 13.48255862861927312, 3.989652714533045580E-16, -5.335786055104159153 ) ) ;
#50065 = ORIENTED_EDGE ( 'NONE', *, *, #73587, .T. ) ;
#50066 = ORIENTED_EDGE ( 'NONE', *, *, #28684, .T. ) ;
#50067 = CARTESIAN_POINT ( 'NONE',  ( 13.79529636645030344, 53.26208216824730357, 14.16423886937410614 ) ) ;
#50068 = CARTESIAN_POINT ( 'NONE',  ( -4.164238869374098151, 51.59541550158063217, -3.795296366450310543 ) ) ;
#50069 = CARTESIAN_POINT ( 'NONE',  ( 18.52753015748618282, 13.92559781766745175, -4.923371831947291888 ) ) ;
#50070 = CARTESIAN_POINT ( 'NONE',  ( -13.68576102233676295, 90.96604444080064411, 7.941738159297530686 ) ) ;
#50071 = CARTESIAN_POINT ( 'NONE',  ( -0.1503990784575282014, 42.22266099184918886, -6.262539305110077947 ) ) ;
#50072 = CARTESIAN_POINT ( 'NONE',  ( -3.250000000000000444, 1.019547802438465656, -2.750000000000000000 ) ) ;
#50073 = CARTESIAN_POINT ( 'NONE',  ( 24.16423886937410614, 39.51208216824731068, -3.795296366450302550 ) ) ;
#50074 = VECTOR ( 'NONE', #5613, 1000.000000000000000 ) ;
#50075 = CARTESIAN_POINT ( 'NONE',  ( -4.838527690343426002, 14.49999999999999112, -14.19819177887740302 ) ) ;
#50076 = CARTESIAN_POINT ( 'NONE',  ( 10.00000000000000000, 9.758931151000785675, -9.846743663894594434 ) ) ;
#50077 = VECTOR ( 'NONE', #2503, 1000.000000000000000 ) ;
#50078 = CARTESIAN_POINT ( 'NONE',  ( -4.923371831947292776, 6.842264484334122265, 8.527530157486181039 ) ) ;
#50079 = ORIENTED_EDGE ( 'NONE', *, *, #31963, .F. ) ;
#50080 = CARTESIAN_POINT ( 'NONE',  ( 3.969999999999999751, 10.00000000000000000, 2.500000000000000000 ) ) ;
#50081 = VERTEX_POINT ( 'NONE', #69725 ) ;
#50082 = LINE ( 'NONE', #81071, #82906 ) ;
#50083 = ORIENTED_EDGE ( 'NONE', *, *, #74320, .T. ) ;
#50085 = CARTESIAN_POINT ( 'NONE',  ( -0.8801773607111008646, 23.27201867748817676, 2.915334737309923430 ) ) ;
#50084 = CARTESIAN_POINT ( 'NONE',  ( 0.5774900079438607392, 18.48035201082150536, 5.440088680355550821 ) ) ;
#50087 = CARTESIAN_POINT ( 'NONE',  ( 16.40814093676324603, 22.45696800326375353, -11.09922568453594671 ) ) ;
#50086 = CARTESIAN_POINT ( 'NONE',  ( 19.84674366389459266, 43.30059781766744464, 2.638427012816836559 ) ) ;
#50088 = DIRECTION ( 'NONE',  ( 0.9099612708765425495, 0.000000000000000000, 0.4146932426562403018 ) ) ;
#50089 = B_SPLINE_CURVE_WITH_KNOTS ( 'NONE', 3,
 ( #62950, #32454, #24978, #75989 ),
 .UNSPECIFIED., .F., .F.,
 ( 4, 4 ),
 ( 4.336808689942017736E-19, 0.002562518741975332043 ),
 .UNSPECIFIED. ) ;
#50090 = CARTESIAN_POINT ( 'NONE',  ( -2.816281873526473856, 24.33196800326375353, 3.434112377981055619 ) ) ;
#50091 = EDGE_LOOP ( 'NONE', ( #81553, #50204, #93454, #27312, #65090 ) ) ;
#50092 = CARTESIAN_POINT ( 'NONE',  ( 19.84674366389459266, 28.71726448433411960, -2.638427012816827677 ) ) ;
#50093 = CARTESIAN_POINT ( 'NONE',  ( -2.266590686148945544, 66.38708216824730357, -7.082119434687050408 ) ) ;
#50094 = ORIENTED_EDGE ( 'NONE', *, *, #72602, .F. ) ;
#50095 = CARTESIAN_POINT ( 'NONE',  ( 4.559911319644449179, 3.897018677488171434, 9.422509992056141925 ) ) ;
#50096 = ORIENTED_EDGE ( 'NONE', *, *, #52821, .F. ) ;
#50097 = CARTESIAN_POINT ( 'NONE',  ( -0.8801773607111008646, 38.27201867748816255, 2.915334737309923430 ) ) ;
#50098 = CARTESIAN_POINT ( 'NONE',  ( 12.91533473730992121, 39.52201867748817676, 10.88017736071110164 ) ) ;
#50099 = CARTESIAN_POINT ( 'NONE',  ( 0.5774900079438607392, 53.48035201082151247, 5.440088680355550821 ) ) ;
#50100 = DIRECTION ( 'NONE',  ( -1.000000000000000000, 0.000000000000000000, 0.000000000000000000 ) ) ;
#50101 = CARTESIAN_POINT ( 'NONE',  ( -0.8801773607111009756, 43.06368534415484106, 1.068504757029289695E-15 ) ) ;
#50102 = DIRECTION ( 'NONE',  ( 6.938893903907221278E-15, 1.000000000000000000, 0.000000000000000000 ) ) ;
#50103 = ADVANCED_FACE ( 'NONE', ( #60243 ), #82747, .T. ) ;
#50104 = CARTESIAN_POINT ( 'NONE',  ( 10.19513985507828302, 14.49999999999999112, 11.00268709613230200 ) ) ;
#50105 = CARTESIAN_POINT ( 'NONE',  ( 18.52753015748618282, 13.92559781766745175, -4.923371831947291888 ) ) ;
#50106 = VERTEX_POINT ( 'NONE', #21773 ) ;
#50107 = CARTESIAN_POINT ( 'NONE',  ( 19.84674366389459621, 63.50893115100078745, 7.409399052514197653E-17 ) ) ;
#50108 = CARTESIAN_POINT ( 'NONE',  ( 13.14228782657334804, 0.5000000000000004441, 7.230509711182329546 ) ) ;
#50109 = CARTESIAN_POINT ( 'NONE',  ( -7.127794346849581686, -80.93619716733995517, 2.750000000000000000 ) ) ;
#50110 = VERTEX_POINT ( 'NONE', #31707 ) ;
#50111 = CARTESIAN_POINT ( 'NONE',  ( -4.547378612396795639, 0.000000000000000000, 3.009844244835475635 ) ) ;
#50113 = CARTESIAN_POINT ( 'NONE',  ( 5.076628168052703671, 31.84226448433412315, 8.527530157486179263 ) ) ;
#50112 = CARTESIAN_POINT ( 'NONE',  ( 5.076628168052703671, 66.84226448433412315, 8.527530157486179263 ) ) ;
#50114 = CARTESIAN_POINT ( 'NONE',  ( 24.16423886937410614, 64.51208216824728936, -3.795296366450302550 ) ) ;
#50115 = CARTESIAN_POINT ( 'NONE',  ( 12.25993886608603489, 14.49999999999999112, 8.642563219313760925 ) ) ;
#50116 = ORIENTED_EDGE ( 'NONE', *, *, #98201, .F. ) ;
#50117 = CARTESIAN_POINT ( 'NONE',  ( -7.108715748589260919, 0.04922511925147068923, 12.92719074505362542 ) ) ;
#50118 = CARTESIAN_POINT ( 'NONE',  ( 5.076628168052703671, 26.84226448433411960, 8.527530157486179263 ) ) ;
#50119 = CARTESIAN_POINT ( 'NONE',  ( -2.816281873526471635, 3.915301336597087456, -3.434112377981056508 ) ) ;
#50120 = CARTESIAN_POINT ( 'NONE',  ( 5.076628168052704559, 5.175597817667451750, -8.527530157486179263 ) ) ;
#50121 = DIRECTION ( 'NONE',  ( 0.000000000000000000, 0.000000000000000000, -1.000000000000000000 ) ) ;
#50122 = CARTESIAN_POINT ( 'NONE',  ( 14.92337183194729988, 4.342264484334117824, -8.527530157486177487 ) ) ;
#50123 = CARTESIAN_POINT ( 'NONE',  ( 14.92337183194729988, 64.34226448433412315, -8.527530157486177487 ) ) ;
#50124 = CARTESIAN_POINT ( 'NONE',  ( 11.22915323889580463, 15.00000000000000000, -8.773176023390609757 ) ) ;
#50125 = EDGE_CURVE ( 'NONE', #76878, #5586, #36651, .T. ) ;
#50126 = AXIS2_PLACEMENT_3D ( 'NONE', #86222, #76744, #31729 ) ;
#50127 = VERTEX_POINT ( 'NONE', #90737 ) ;
#50128 = EDGE_CURVE ( 'NONE', #43266, #13075, #45549, .T. ) ;
#50129 = CARTESIAN_POINT ( 'NONE',  ( 12.91533473730993009, 11.60535201082150714, -10.88017736071109987 ) ) ;
#50130 = CARTESIAN_POINT ( 'NONE',  ( 22.26659068614895176, 9.720415501580633943, -7.082119434687042414 ) ) ;
#50131 = CARTESIAN_POINT ( 'NONE',  ( 19.84674366389459621, 8.508931151000785675, 7.409399052514197653E-17 ) ) ;
#50132 = CARTESIAN_POINT ( 'NONE',  ( 17.96484262340118221, 39.93868534415484106, 7.964842623401181321 ) ) ;
#50134 = CARTESIAN_POINT ( 'NONE',  ( 9.508231703811905078, 12.87087484978187746, -6.715038726106763001 ) ) ;
#50133 = CARTESIAN_POINT ( 'NONE',  ( 10.00000000000000178, 20.37363466993042138, 12.81628187352647608 ) ) ;
#50135 = CARTESIAN_POINT ( 'NONE',  ( -8.000000000000000000, 80.99999999999994316, 1.249999999999987121 ) ) ;
#50136 = DIRECTION ( 'NONE',  ( 0.000000000000000000, -1.000000000000000000, 0.000000000000000000 ) ) ;
#50137 = CARTESIAN_POINT ( 'NONE',  ( 3.591859063236761518, -0.04303199673624671928, 11.09922568453594849 ) ) ;
#50138 = CARTESIAN_POINT ( 'NONE',  ( 0.1532563361054082862, 66.21726448433413736, 2.638427012816831674 ) ) ;
#50139 = CARTESIAN_POINT ( 'NONE',  ( 1.472469842513823179, 11.42559781766745175, 4.923371831947296329 ) ) ;
#50140 = CARTESIAN_POINT ( 'NONE',  ( 2.915334737309928315, -25.47798132251181968, 10.88017736071109987 ) ) ;
#50141 = CARTESIAN_POINT ( 'NONE',  ( 6.565887622018943937, 18.08196800326375708, -12.81628187352647608 ) ) ;
#50142 = CARTESIAN_POINT ( 'NONE',  ( -10.53011945866295029, -98.59345040283277228, -3.999999999999994671 ) ) ;
#50143 = CARTESIAN_POINT ( 'NONE',  ( 0.5774900079438590739, 32.64701867748816966, -5.440088680355550821 ) ) ;
#50144 = DIRECTION ( 'NONE',  ( 0.000000000000000000, 0.000000000000000000, 1.000000000000000000 ) ) ;
#50145 = CARTESIAN_POINT ( 'NONE',  ( -0.3689425029237881626, 52.42874883491396076, 10.36894250292379027 ) ) ;
#50146 = CARTESIAN_POINT ( 'NONE',  ( 14.35840480524204388, 14.63606918001612556, -4.340070442838849019 ) ) ;
#50147 = CARTESIAN_POINT ( 'NONE',  ( 10.00000000000000000, 32.87363466993042493, -12.81628187352647608 ) ) ;
#50148 = CARTESIAN_POINT ( 'NONE',  ( -0.8801773607110991993, 32.85535201082151247, -2.915334737309923874 ) ) ;
#50149 = CARTESIAN_POINT ( 'NONE',  ( 18.52753015748618282, 53.92559781766745175, -4.923371831947291888 ) ) ;
#50150 = CARTESIAN_POINT ( 'NONE',  ( 12.91533473730993009, 56.60535201082151247, -10.88017736071109987 ) ) ;
#50151 = B_SPLINE_CURVE_WITH_KNOTS ( 'NONE', 3,
 ( #55580, #39105, #40580, #86078, #17590, #15625 ),
 .UNSPECIFIED., .F., .F.,
 ( 4, 2, 4 ),
 ( 0.000000000000000000, 0.0002565770811491039499, 0.0005131541622982078998 ),
 .UNSPECIFIED. ) ;
#50152 = CARTESIAN_POINT ( 'NONE',  ( 10.00000000000000000, 35.55374883491396787, -14.16423886937410082 ) ) ;
#50153 = DIRECTION ( 'NONE',  ( 0.000000000000000000, -1.000000000000000000, 0.000000000000000000 ) ) ;
#50154 = UNCERTAINTY_MEASURE_WITH_UNIT (LENGTH_MEASURE( 1.000000000000000082E-05 ), #94015, 'distance_accuracy_value', 'NONE');
#50155 = CARTESIAN_POINT ( 'NONE',  ( 0.1532563361054100626, 20.80059781766744464, -2.638427012816831230 ) ) ;
#50156 = CARTESIAN_POINT ( 'NONE',  ( -2.816281873526471635, 58.91530133659707502, -3.434112377981056508 ) ) ;
#50157 = CARTESIAN_POINT ( 'NONE',  ( 0.6178305044545818747, -1.501365330069579951, -9.382169495545419124 ) ) ;
#50158 = ORIENTED_EDGE ( 'NONE', *, *, #97928, .F. ) ;
#50159 = CARTESIAN_POINT ( 'NONE',  ( 21.92686044187657046, 7.396642702460841434, -3.195792623639524432 ) ) ;
#50160 = CARTESIAN_POINT ( 'NONE',  ( 6.533420211785746723, -50.31490269211863620, 3.750000000000001776 ) ) ;
#50161 = CARTESIAN_POINT ( 'NONE',  ( 17.96484262340118221, 14.93868534415484106, 7.964842623401181321 ) ) ;
#50162 = CARTESIAN_POINT ( 'NONE',  ( 24.16423886937410614, 19.51208216824729647, -3.795296366450302550 ) ) ;
#50163 = CARTESIAN_POINT ( 'NONE',  ( 0.1532563361054083140, 11.00893115100078568, 1.131784320476157264E-15 ) ) ;
#50164 = FACE_OUTER_BOUND ( 'NONE', #9257, .T. ) ;
#50165 = CARTESIAN_POINT ( 'NONE',  ( -0.8801773607111009756, 38.06368534415484106, 1.068504757029289695E-15 ) ) ;
#50166 = LINE ( 'NONE', #80675, #8052 ) ;
#50167 = CARTESIAN_POINT ( 'NONE',  ( 7.993154516101047768, 0.04922511925147154271, -12.39982181464614541 ) ) ;
#50168 = VERTEX_POINT ( 'NONE', #84728 ) ;
#50169 = CARTESIAN_POINT ( 'NONE',  ( 0.1532563361054082862, 41.21726448433411605, 2.638427012816831674 ) ) ;
#50170 = ORIENTED_EDGE ( 'NONE', *, *, #21940, .F. ) ;
#50171 = ORIENTED_EDGE ( 'NONE', *, *, #85272, .F. ) ;
#50172 = DIRECTION ( 'NONE',  ( -1.000000000000000000, 0.000000000000000000, 0.000000000000000000 ) ) ;
#50173 = CARTESIAN_POINT ( 'NONE',  ( 22.26659068614895176, 4.720415501580633943, -7.082119434687042414 ) ) ;
#50174 = CARTESIAN_POINT ( 'NONE',  ( 6.204703633549690345, 7.845415501580634832, 14.16423886937410082 ) ) ;
#50175 = CARTESIAN_POINT ( 'NONE',  ( 20.88017736071110164, 45.35535201082149115, 2.915334737309930979 ) ) ;
#50176 = CARTESIAN_POINT ( 'NONE',  ( 2.917880565312948704, 57.63708216824731068, 12.26659068614894643 ) ) ;
#50177 = CARTESIAN_POINT ( 'NONE',  ( 14.92337183194729988, 59.34226448433412315, -8.527530157486177487 ) ) ;
#50178 = CARTESIAN_POINT ( 'NONE',  ( 14.92337183194729633, 32.67559781766745175, 8.527530157486181039 ) ) ;
#50179 = CARTESIAN_POINT ( 'NONE',  ( -10.85644721913293154, -98.10785618599911118, 3.750000000000000000 ) ) ;
#50181 = CARTESIAN_POINT ( 'NONE',  ( 19.38216949554541202, 5.998634669930420493, 9.382169495545424454 ) ) ;
#50180 = CARTESIAN_POINT ( 'NONE',  ( 12.91533473730992121, 39.52201867748817676, 10.88017736071110164 ) ) ;
#50182 = CARTESIAN_POINT ( 'NONE',  ( -4.164238869374099039, 1.803748834913967647, 8.674139862899312516E-16 ) ) ;
#50183 = CARTESIAN_POINT ( 'NONE',  ( 22.26659068614895176, 54.72041550158063217, -7.082119434687042414 ) ) ;
#50184 = CARTESIAN_POINT ( 'NONE',  ( 20.88017736071110875, 10.77201867748817143, -2.915334737309920765 ) ) ;
#50185 = DIRECTION ( 'NONE',  ( 0.000000000000000000, 1.000000000000000000, 0.000000000000000000 ) ) ;
#50186 = CARTESIAN_POINT ( 'NONE',  ( 0.000000000000000000, 70.00000000000000000, 5.000000000000000000 ) ) ;
#50187 = CARTESIAN_POINT ( 'NONE',  ( 7.208316651077764980, -37.11606884899919834, 7.208316651077762316 ) ) ;
#50188 = VERTEX_POINT ( 'NONE', #22265 ) ;
#50189 = CARTESIAN_POINT ( 'NONE',  ( 0.000000000000000000, -97.00000000000000000, 4.000000000000000000 ) ) ;
#50190 = ORIENTED_EDGE ( 'NONE', *, *, #36721, .F. ) ;
#50191 = ORIENTED_EDGE ( 'NONE', *, *, #44949, .T. ) ;
#50192 = CARTESIAN_POINT ( 'NONE',  ( -0.3689425029237881626, 42.42874883491396787, 10.36894250292379027 ) ) ;
#50193 = CARTESIAN_POINT ( 'NONE',  ( 2.791683348922240793, 31.63393115100078745, 7.208316651077764092 ) ) ;
#50194 = CARTESIAN_POINT ( 'NONE',  ( 7.084665262690076126, 62.02201867748816966, -10.88017736071110164 ) ) ;
#50195 = CARTESIAN_POINT ( 'NONE',  ( 20.15039907845753575, 36.74884699246889141, 6.262539305110075283 ) ) ;
#50196 = CARTESIAN_POINT ( 'NONE',  ( 7.084665262690076126, 59.10535201082150536, 10.88017736071109987 ) ) ;
#50197 = AXIS2_PLACEMENT_3D ( 'NONE', #62905, #3401, #71413 ) ;
#50199 = CARTESIAN_POINT ( 'NONE',  ( 3.591859063236763294, 63.29030133659708923, -11.09922568453595026 ) ) ;
#50198 = TOROIDAL_SURFACE ( 'NONE', #45421, 18.93999999999999773, 0.5000000000000000000 ) ;
#50200 = CARTESIAN_POINT ( 'NONE',  ( 12.81628187352647608, 1.623634669930422492, -2.602085213965210642E-15 ) ) ;
#50201 = ORIENTED_EDGE ( 'NONE', *, *, #91343, .F. ) ;
#50202 = CARTESIAN_POINT ( 'NONE',  ( 24.16423886937410614, 19.51208216824729647, -3.795296366450302550 ) ) ;
#50203 = VECTOR ( 'NONE', #9571, 1000.000000000000000 ) ;
#50204 = ORIENTED_EDGE ( 'NONE', *, *, #43080, .T. ) ;
#50205 = CARTESIAN_POINT ( 'NONE',  ( 10.00000000000000178, 50.37363466993042493, 12.81628187352647608 ) ) ;
#50206 = CARTESIAN_POINT ( 'NONE',  ( 20.88017736071110164, 15.35535201082150358, 2.915334737309930979 ) ) ;
#50207 = CARTESIAN_POINT ( 'NONE',  ( 7.361572987183170547, 27.05059781766745175, 9.846743663894590881 ) ) ;
#50208 = CARTESIAN_POINT ( 'NONE',  ( 2.035157376598822676, 17.43868534415483751, -7.964842623401177768 ) ) ;
#50209 = CARTESIAN_POINT ( 'NONE',  ( 13.43411237798106583, 52.66530133659708213, -12.81628187352647252 ) ) ;
#50210 = CARTESIAN_POINT ( 'NONE',  ( -46.59701958359876528, 103.7651961684614861, -6.068442458532171457 ) ) ;
#50211 = CARTESIAN_POINT ( 'NONE',  ( 12.63842701281683034, 37.46726448433411605, 9.846743663894596210 ) ) ;
#50212 = EDGE_CURVE ( 'NONE', #25656, #35357, #4091, .T. ) ;
#50213 = CARTESIAN_POINT ( 'NONE',  ( -12.58848565468362857, 15.00000000000000888, 7.447709424579771031 ) ) ;
#50214 = LINE ( 'NONE', #71271, #32280 ) ;
#50215 = DIRECTION ( 'NONE',  ( 0.000000000000000000, 1.000000000000000000, 0.000000000000000000 ) ) ;
#50216 = CARTESIAN_POINT ( 'NONE',  ( 0.1916775849787259733, 17.25868815902069642, -6.500000000000001776 ) ) ;
#50217 = CARTESIAN_POINT ( 'NONE',  ( 10.00000000000000178, 22.25893115100078745, 9.846743663894594434 ) ) ;
#50218 = CARTESIAN_POINT ( 'NONE',  ( 0.6178305044545838731, 19.74863466993042138, 9.382169495545420901 ) ) ;
#50219 = CARTESIAN_POINT ( 'NONE',  ( 11.39601241150452182, 15.00000000000000000, 11.22534175661874301 ) ) ;
#50220 = CARTESIAN_POINT ( 'NONE',  ( 19.84674366389459621, 43.50893115100078745, 7.409399052514197653E-17 ) ) ;
#50221 = LINE ( 'NONE', #42739, #64954 ) ;
#50222 = CARTESIAN_POINT ( 'NONE',  ( 17.08211943468705840, 15.13708216824730179, -12.26659068614894466 ) ) ;
#50223 = CARTESIAN_POINT ( 'NONE',  ( 19.84674366389459621, 38.50893115100078745, 7.409399052514197653E-17 ) ) ;
#50224 = CARTESIAN_POINT ( 'NONE',  ( 21.09922568453595559, 32.04030133659708923, -6.408140936763230044 ) ) ;
#50225 = CARTESIAN_POINT ( 'NONE',  ( -14.04391541078760675, 4.104531544909319036E-16, -3.608107528143027043 ) ) ;
#50226 = CARTESIAN_POINT ( 'NONE',  ( 2.035157376598824452, 63.68868534415484106, 7.964842623401179544 ) ) ;
#50227 = CARTESIAN_POINT ( 'NONE',  ( 19.38216949554541557, 7.248634669930421381, -9.382169495545420901 ) ) ;
#50228 = FACE_OUTER_BOUND ( 'NONE', #11406, .T. ) ;
#50229 = COLOUR_RGB ( '', 0.66274510, 0.83137255, 0.94901961) ;
#50230 = CARTESIAN_POINT ( 'NONE',  ( 1.472469842513823179, 36.42559781766745175, 4.923371831947296329 ) ) ;
#50231 = CARTESIAN_POINT ( 'NONE',  ( 7.084665262690076126, 24.10535201082150181, 10.88017736071109987 ) ) ;
#50232 = CARTESIAN_POINT ( 'NONE',  ( -1.099225684535947600, 33.70696800326375353, -6.408140936763238038 ) ) ;
#50233 = CARTESIAN_POINT ( 'NONE',  ( 5.076628168052704559, 30.17559781766745175, -8.527530157486179263 ) ) ;
#50234 = SHAPE_DEFINITION_REPRESENTATION ( #21304, #19841 ) ;
#50235 = CARTESIAN_POINT ( 'NONE',  ( -2.393480905993257579, 0.3640475087720981273, 14.80781041047750435 ) ) ;
#50236 = ADVANCED_FACE ( 'NONE', ( #45745 ), #50384, .T. ) ;
#50237 = CARTESIAN_POINT ( 'NONE',  ( 2.035157376598822676, 37.43868534415484106, -7.964842623401177768 ) ) ;
#50238 = ORIENTED_EDGE ( 'NONE', *, *, #59192, .F. ) ;
#50239 = CARTESIAN_POINT ( 'NONE',  ( -11.25000000000000178, 4.909700295649315649, -3.014428414850122806 ) ) ;
#50240 = CARTESIAN_POINT ( 'NONE',  ( 20.88017736071110875, 5.772018677488170546, -2.915334737309920765 ) ) ;
#50242 = CARTESIAN_POINT ( 'NONE',  ( -0.8801773607111008646, 33.27201867748817676, 2.915334737309923430 ) ) ;
#50241 = CARTESIAN_POINT ( 'NONE',  ( 19.84674366389459266, 53.71726448433411605, -2.638427012816827677 ) ) ;
#50243 = CARTESIAN_POINT ( 'NONE',  ( 4.559911319644449179, 57.23035201082150536, -9.422509992056141925 ) ) ;
#50245 = DIRECTION ( 'NONE',  ( 0.000000000000000000, 0.000000000000000000, 1.000000000000000000 ) ) ;
#50244 = CARTESIAN_POINT ( 'NONE',  ( 4.559911319644449179, 28.89701867748817321, 9.422509992056141925 ) ) ;
#50246 = CARTESIAN_POINT ( 'NONE',  ( 14.92337183194729633, 2.675597817667451750, 8.527530157486181039 ) ) ;
#50247 = DIRECTION ( 'NONE',  ( -0.000000000000000000, -1.000000000000000000, -0.000000000000000000 ) ) ;
#50248 = CARTESIAN_POINT ( 'NONE',  ( 2.791683348922240793, 56.63393115100078035, 7.208316651077764092 ) ) ;
#50250 = CARTESIAN_POINT ( 'NONE',  ( 4.380000000000002558, 1.019547802438462547, 3.750000000000000000 ) ) ;
#50249 = CARTESIAN_POINT ( 'NONE',  ( 22.26659068614894466, 58.88708216824729647, 7.082119434687054849 ) ) ;
#50251 = DIRECTION ( 'NONE',  ( 1.000000000000000000, 0.000000000000000000, 0.000000000000000000 ) ) ;
#50252 = CARTESIAN_POINT ( 'NONE',  ( 6.204703633549690345, 2.845415501580634388, 14.16423886937410082 ) ) ;
#50253 = CARTESIAN_POINT ( 'NONE',  ( -0.3689425029237898834, 31.17874883491396787, -10.36894250292378850 ) ) ;
#50254 = CARTESIAN_POINT ( 'NONE',  ( 16.40814093676324603, 7.456968003263754419, -11.09922568453594671 ) ) ;
#50255 = PLANE ( 'NONE',  #7468 ) ;
#50256 = VERTEX_POINT ( 'NONE', #6755 ) ;
#50257 = MECHANICAL_DESIGN_GEOMETRIC_PRESENTATION_REPRESENTATION (  '', ( #67848 ), #56702 ) ;
#50258 = CARTESIAN_POINT ( 'NONE',  ( 7.084665262690076126, 17.02201867748817676, -10.88017736071110164 ) ) ;
#50259 = CARTESIAN_POINT ( 'NONE',  ( 7.361572987183170547, 42.05059781766745886, 9.846743663894590881 ) ) ;
#50260 = CARTESIAN_POINT ( 'NONE',  ( -10.94840535726567943, 89.72140148746872512, -6.176821657850955383 ) ) ;
#50261 = CARTESIAN_POINT ( 'NONE',  ( 20.88017736071110164, 60.35535201082151957, 2.915334737309930979 ) ) ;
#50262 = CARTESIAN_POINT ( 'NONE',  ( 3.115783986955448892, 15.00000000000000000, 14.16128137375397600 ) ) ;
#50263 = VECTOR ( 'NONE', #81478, 1000.000000000000000 ) ;
#50264 = CARTESIAN_POINT ( 'NONE',  ( 21.09922568453595559, 62.04030133659709634, -6.408140936763230044 ) ) ;
#50265 = CARTESIAN_POINT ( 'NONE',  ( 21.09922568453594849, 21.20696800326375353, 6.408140936763242479 ) ) ;
#50266 = CARTESIAN_POINT ( 'NONE',  ( 19.84674366389459621, 33.50893115100078745, 7.409399052514197653E-17 ) ) ;
#50267 = ORIENTED_EDGE ( 'NONE', *, *, #82865, .T. ) ;
#50268 = FACE_BOUND ( 'NONE', #24763, .T. ) ;
#50269 = CARTESIAN_POINT ( 'NONE',  ( -0.8801773607111009756, 3.063685344154838397, 1.068504757029289695E-15 ) ) ;
#50270 = CARTESIAN_POINT ( 'NONE',  ( 10.00000000000000178, 19.31368534415484106, 10.88017736071110342 ) ) ;
#50271 = CARTESIAN_POINT ( 'NONE',  ( 20.36894250292379738, 34.92874883491396076, -10.36894250292379027 ) ) ;
#50272 = CARTESIAN_POINT ( 'NONE',  ( 17.96484262340118221, 34.93868534415482685, 7.964842623401181321 ) ) ;
#50273 = CARTESIAN_POINT ( 'NONE',  ( 2.035157376598824452, 58.68868534415482685, 7.964842623401179544 ) ) ;
#50274 = CARTESIAN_POINT ( 'NONE',  ( -13.61464873478175797, 14.63606918187687000, 6.296136897217746053 ) ) ;
#50275 = EDGE_CURVE ( 'NONE', #77529, #97699, #45242, .T. ) ;
#50276 = CARTESIAN_POINT ( 'NONE',  ( 10.76917535773492141, -96.07946373138615570, -4.000000000000000000 ) ) ;
#50277 = CARTESIAN_POINT ( 'NONE',  ( 10.00000000000000000, 9.758931151000785675, -9.846743663894594434 ) ) ;
#50278 = CARTESIAN_POINT ( 'NONE',  ( 19.88701968852512536, 21.79427333184091964, 6.480634945678691139 ) ) ;
#50279 = CARTESIAN_POINT ( 'NONE',  ( 10.00000000000000000, 9.758931151000785675, -9.846743663894594434 ) ) ;
#50280 = SURFACE_STYLE_FILL_AREA ( #95807 ) ;
#50281 = CARTESIAN_POINT ( 'NONE',  ( 17.20831665107776587, 37.88393115100078745, 7.208316651077764980 ) ) ;
#50282 = CARTESIAN_POINT ( 'NONE',  ( 6.565887622018943937, 0.1653013365970866511, 12.81628187352647430 ) ) ;
#50283 = ADVANCED_FACE ( 'NONE', ( #83741 ), #76241, .F. ) ;
#50284 = CARTESIAN_POINT ( 'NONE',  ( 15.44008868035555793, 26.39701867748817321, -9.422509992056140149 ) ) ;
#50285 = UNCERTAINTY_MEASURE_WITH_UNIT (LENGTH_MEASURE( 1.000000000000000082E-05 ), #76156, 'distance_accuracy_value', 'NONE');
#50286 = VERTEX_POINT ( 'NONE', #15264 ) ;
#50287 = CARTESIAN_POINT ( 'NONE',  ( 3.591859063236761518, 39.95696800326375353, 11.09922568453594849 ) ) ;
#50288 = AXIS2_PLACEMENT_3D ( 'NONE', #85950, #86441, #17460 ) ;
#50289 = DIRECTION ( 'NONE',  ( 1.257568779154408793E-17, 1.000000000000000000, -0.000000000000000000 ) ) ;
#50290 = CARTESIAN_POINT ( 'NONE',  ( 12.91533473730992121, 59.52201867748816966, 10.88017736071110164 ) ) ;
#50291 = CARTESIAN_POINT ( 'NONE',  ( -2.816281873526471635, 43.91530133659708923, -3.434112377981056508 ) ) ;
#50293 = CARTESIAN_POINT ( 'NONE',  ( 5.076628168052703671, 21.84226448433411960, 8.527530157486179263 ) ) ;
#50292 = CARTESIAN_POINT ( 'NONE',  ( -0.3689425029237881626, 57.42874883491397497, 10.36894250292379027 ) ) ;
#50294 = CARTESIAN_POINT ( 'NONE',  ( 0.2751277870542911397, 50.30223176428831522, 6.499999999999992006 ) ) ;
#50295 = CARTESIAN_POINT ( 'NONE',  ( 10.00000000000000178, 62.25893115100078745, 9.846743663894594434 ) ) ;
#50296 = CARTESIAN_POINT ( 'NONE',  ( 2.917880565312950480, 30.97041550158063572, -12.26659068614894821 ) ) ;
#50297 = CARTESIAN_POINT ( 'NONE',  ( 17.20831665107776587, 47.88393115100078745, 7.208316651077764980 ) ) ;
#50298 = CARTESIAN_POINT ( 'NONE',  ( 31.00000000000000000, -1.803764545938971194E-15, 7.000000000000000000 ) ) ;
#50299 = CARTESIAN_POINT ( 'NONE',  ( 4.559911319644449179, 23.89701867748817321, 9.422509992056141925 ) ) ;
#50300 = CARTESIAN_POINT ( 'NONE',  ( 20.88017736071110519, 60.56368534415484106, 2.639326808657452039E-16 ) ) ;
#50301 = CARTESIAN_POINT ( 'NONE',  ( 0.000000000000000000, -97.00000000000000000, -3.750000000000000000 ) ) ;
#50302 = VERTEX_POINT ( 'NONE', #85712 ) ;
#50303 = CARTESIAN_POINT ( 'NONE',  ( 6.565887622018943937, 48.08196800326375353, -12.81628187352647608 ) ) ;
#50304 = CARTESIAN_POINT ( 'NONE',  ( 2.035157376598824452, 53.68868534415484817, 7.964842623401179544 ) ) ;
#50305 = ORIENTED_EDGE ( 'NONE', *, *, #19506, .T. ) ;
#50306 = SURFACE_STYLE_FILL_AREA ( #93490 ) ;
#50307 = DIRECTION ( 'NONE',  ( -0.000000000000000000, -1.000000000000000000, -0.000000000000000000 ) ) ;
#50308 = CYLINDRICAL_SURFACE ( 'NONE', #13812, 0.2500000000000002220 ) ;
#50309 = ORIENTED_EDGE ( 'NONE', *, *, #39176, .T. ) ;
#50310 = CARTESIAN_POINT ( 'NONE',  ( 0.5774900079438607392, 63.48035201082149825, 5.440088680355550821 ) ) ;
#50311 = CARTESIAN_POINT ( 'NONE',  ( 15.44008868035555260, 9.730352010821505360, 9.422509992056143702 ) ) ;
#50312 = DIRECTION ( 'NONE',  ( 0.000000000000000000, 1.000000000000000000, 0.000000000000000000 ) ) ;
#50313 = SURFACE_STYLE_FILL_AREA ( #84169 ) ;
#50314 = CARTESIAN_POINT ( 'NONE',  ( 20.88017736071110875, 5.772018677488170546, -2.915334737309920765 ) ) ;
#50315 = CARTESIAN_POINT ( 'NONE',  ( 20.36894250292379382, 13.67874883491396965, 10.36894250292379205 ) ) ;
#50316 = CARTESIAN_POINT ( 'NONE',  ( 20.88017736071110875, 20.77201867748816611, -2.915334737309920765 ) ) ;
#50317 = CARTESIAN_POINT ( 'NONE',  ( 18.52753015748617571, 58.09226448433411605, 4.923371831947298993 ) ) ;
#50318 = ORIENTED_EDGE ( 'NONE', *, *, #44271, .T. ) ;
#50319 = CARTESIAN_POINT ( 'NONE',  ( 5.076628168052703671, 61.84226448433412315, 8.527530157486179263 ) ) ;
#50320 = ORIENTED_EDGE ( 'NONE', *, *, #76910, .T. ) ;
#50321 = AXIS2_PLACEMENT_3D ( 'NONE', #98095, #53052, #84060 ) ;
#50322 = AXIS2_PLACEMENT_3D ( 'NONE', #1320, #15812, #39788 ) ;
#50323 = CARTESIAN_POINT ( 'NONE',  ( 0.5774900079438590739, 57.64701867748817676, -5.440088680355550821 ) ) ;
#50324 = CARTESIAN_POINT ( 'NONE',  ( 5.076628168052703671, 66.84226448433412315, 8.527530157486179263 ) ) ;
#50325 = CARTESIAN_POINT ( 'NONE',  ( 16.40814093676323893, 35.79030133659708923, 11.09922568453595026 ) ) ;
#50327 = LINE ( 'NONE', #33834, #44668 ) ;
#50326 = CARTESIAN_POINT ( 'NONE',  ( 12.91533473730992121, 4.522018677488169658, 10.88017736071110164 ) ) ;
#50328 = CARTESIAN_POINT ( 'NONE',  ( 19.42250999205614193, 60.14701867748817676, 5.440088680355555262 ) ) ;
#50329 = CARTESIAN_POINT ( 'NONE',  ( 10.00000000000000000, 16.81368534415483751, -10.88017736071110342 ) ) ;
#50330 = ADVANCED_FACE ( 'NONE', ( #87167 ), #62200, .F. ) ;
#50331 = B_SPLINE_CURVE_WITH_KNOTS ( 'NONE', 3,
 ( #14993, #83472, #68967, #91951, #37492, #29961 ),
 .UNSPECIFIED., .F., .F.,
 ( 4, 2, 4 ),
 ( 3.409110551494637202E-05, 0.0004400426677367925347, 0.0008459942299586386974 ),
 .UNSPECIFIED. ) ;
#50332 = CARTESIAN_POINT ( 'NONE',  ( 3.591859063236763294, 53.29030133659708923, -11.09922568453595026 ) ) ;
#50333 = CARTESIAN_POINT ( 'NONE',  ( 2.035157376598824452, 23.68868534415484461, 7.964842623401179544 ) ) ;
#50334 = CARTESIAN_POINT ( 'NONE',  ( -8.209432707284950226, 0.5000000000000004441, 12.55409154915480485 ) ) ;
#50335 = EDGE_CURVE ( 'NONE', #49345, #65924, #42485, .T. ) ;
#50336 = AXIS2_PLACEMENT_3D ( 'NONE', #45829, #22345, #16807 ) ;
#50337 = CARTESIAN_POINT ( 'NONE',  ( -2.816281873526473856, 39.33196800326374643, 3.434112377981055619 ) ) ;
#50338 = CARTESIAN_POINT ( 'NONE',  ( 19.42250999205614548, 30.98035201082150536, -5.440088680355545492 ) ) ;
#50339 = CARTESIAN_POINT ( 'NONE',  ( 0.1532563361054082862, 61.21726448433412315, 2.638427012816831674 ) ) ;
#50340 = ORIENTED_EDGE ( 'NONE', *, *, #42064, .F. ) ;
#50341 = DIRECTION ( 'NONE',  ( 0.000000000000000000, 1.000000000000000000, 0.000000000000000000 ) ) ;
#50342 = CARTESIAN_POINT ( 'NONE',  ( 19.84674366389459621, 8.508931151000785675, 7.409399052514197653E-17 ) ) ;
#50343 = CARTESIAN_POINT ( 'NONE',  ( 0.1532563361054082862, 66.21726448433413736, 2.638427012816831674 ) ) ;
#50345 = CARTESIAN_POINT ( 'NONE',  ( 10.00000000000000178, 47.25893115100078745, 9.846743663894594434 ) ) ;
#50344 = CARTESIAN_POINT ( 'NONE',  ( -13.78092363094822304, 90.91979277574868945, -7.864123332961985291 ) ) ;
#50346 = CARTESIAN_POINT ( 'NONE',  ( 4.559911319644449179, 18.89701867748817321, 9.422509992056141925 ) ) ;
#50347 = DIRECTION ( 'NONE',  ( 0.000000000000000000, 0.000000000000000000, 1.000000000000000000 ) ) ;
#50348 = CARTESIAN_POINT ( 'NONE',  ( 12.63842701281683922, 34.55059781766745886, -9.846743663894590881 ) ) ;
#50349 = CARTESIAN_POINT ( 'NONE',  ( 9.876730923139357188, 14.49999999999999112, -11.28938378619066363 ) ) ;
#50350 = FILL_AREA_STYLE ('',( #52331 ) ) ;
#50352 = CARTESIAN_POINT ( 'NONE',  ( 12.63842701281683922, 4.550597817667451750, -9.846743663894590881 ) ) ;
#50351 = CARTESIAN_POINT ( 'NONE',  ( 14.92337183194729988, 44.34226448433412315, -8.527530157486177487 ) ) ;
#50353 = CARTESIAN_POINT ( 'NONE',  ( -20.19000000000000838, 92.00000000000000000, -9.500000000000000000 ) ) ;
#50355 = ORIENTED_EDGE ( 'NONE', *, *, #60315, .F. ) ;
#50354 = CARTESIAN_POINT ( 'NONE',  ( 19.84674366389459621, 58.50893115100078745, 7.409399052514197653E-17 ) ) ;
#50356 = DIRECTION ( 'NONE',  ( 1.000000000000000000, 0.000000000000000000, 0.000000000000000000 ) ) ;
#50357 = CARTESIAN_POINT ( 'NONE',  ( 22.81628187352648496, 36.83196800326376064, -3.434112377981050290 ) ) ;
#50358 = AXIS2_PLACEMENT_3D ( 'NONE', #56201, #77702, #32690 ) ;
#50359 = EDGE_CURVE ( 'NONE', #39257, #63305, #11175, .T. ) ;
#50360 = CARTESIAN_POINT ( 'NONE',  ( 14.92337183194729988, 49.34226448433411605, -8.527530157486177487 ) ) ;
#50361 = DIRECTION ( 'NONE',  ( -0.7385627893568607050, 0.6741846973770715401, 0.000000000000000000 ) ) ;
#50362 = CARTESIAN_POINT ( 'NONE',  ( 24.16423886937410614, 59.30374883491397497, 8.672049930838204340E-16 ) ) ;
#50363 = CARTESIAN_POINT ( 'NONE',  ( 14.92337183194729988, 34.34226448433411605, -8.527530157486177487 ) ) ;
#50364 = CARTESIAN_POINT ( 'NONE',  ( -0.3289641300568005855, 40.10497603579417358, 5.963430220938281678 ) ) ;
#50365 = EDGE_CURVE ( 'NONE', #85655, #4847, #60360, .T. ) ;
#50366 = CARTESIAN_POINT ( 'NONE',  ( 24.16423886937410614, 54.51208216824730357, -3.795296366450302550 ) ) ;
#50367 = CARTESIAN_POINT ( 'NONE',  ( -42.60666666666668334, 92.50000000000000000, 9.500000000000000000 ) ) ;
#50368 = CARTESIAN_POINT ( 'NONE',  ( 10.00000000000000178, 14.31368534415483929, 10.88017736071110342 ) ) ;
#50369 = CARTESIAN_POINT ( 'NONE',  ( 24.16423886937410614, 39.30374883491396787, 8.672049930838204340E-16 ) ) ;
#50371 = CARTESIAN_POINT ( 'NONE',  ( -2.933660812630105141, 15.00000000000000000, 15.72485391577587954 ) ) ;
#50370 = CARTESIAN_POINT ( 'NONE',  ( 22.26659068614894466, 58.88708216824729647, 7.082119434687054849 ) ) ;
#50372 = CARTESIAN_POINT ( 'NONE',  ( 0.2751277870542967463, 69.50000000000000000, 6.500000000000000888 ) ) ;
#50373 = CARTESIAN_POINT ( 'NONE',  ( 12.63842701281683034, 7.467264484334118713, 9.846743663894596210 ) ) ;
#50374 = CARTESIAN_POINT ( 'NONE',  ( 7.361572987183170547, 67.05059781766746596, 9.846743663894590881 ) ) ;
#50375 = VERTEX_POINT ( 'NONE', #63675 ) ;
#50376 = CARTESIAN_POINT ( 'NONE',  ( 10.00000000000000000, 46.81368534415484106, -10.88017736071110342 ) ) ;
#50377 = VECTOR ( 'NONE', #83718, 1000.000000000000114 ) ;
#50378 = CARTESIAN_POINT ( 'NONE',  ( -0.8801773607111009756, 18.27201867748817321, 2.915334737309923874 ) ) ;
#50379 = CARTESIAN_POINT ( 'NONE',  ( 0.000000000000000000, 0.000000000000000000, 0.000000000000000000 ) ) ;
#50380 = B_SPLINE_CURVE_WITH_KNOTS ( 'NONE', 3,
 ( #27132, #34134, #88131, #88624, #44102, #19643 ),
 .UNSPECIFIED., .F., .F.,
 ( 4, 2, 4 ),
 ( 0.000000000000000000, 0.0002701661927229229761, 0.0005403323854458459523 ),
 .UNSPECIFIED. ) ;
#50381 = CARTESIAN_POINT ( 'NONE',  ( 0.1532563361054083140, 51.00893115100078745, 1.131784320476157264E-15 ) ) ;
#50382 = CARTESIAN_POINT ( 'NONE',  ( -0.3093388210927672244, 0.3640475087720984049, 14.99680997725066867 ) ) ;
#50383 = ORIENTED_EDGE ( 'NONE', *, *, #91679, .T. ) ;
#50384 = TOROIDAL_SURFACE ( 'NONE', #12068, 14.49999999999999822, 0.5000000000000000000 ) ;
#50385 = CARTESIAN_POINT ( 'NONE',  ( 2.917880565312948704, 27.63708216824730357, 12.26659068614894643 ) ) ;
#50386 = DIRECTION ( 'NONE',  ( 0.000000000000000000, 1.000000000000000000, 0.000000000000000000 ) ) ;
#50388 = CARTESIAN_POINT ( 'NONE',  ( 0.000000000000000000, 0.000000000000000000, 0.000000000000000000 ) ) ;
#50387 = CARTESIAN_POINT ( 'NONE',  ( -6.866255446112624838, -80.67934795256483937, -2.500000000000000000 ) ) ;
#50389 = CARTESIAN_POINT ( 'NONE',  ( 10.00000000000000178, 19.31368534415484106, 10.88017736071110342 ) ) ;
#50390 = CARTESIAN_POINT ( 'NONE',  ( -2.816281873526473856, 44.33196800326375353, 3.434112377981055619 ) ) ;
#50391 = CARTESIAN_POINT ( 'NONE',  ( -8.731067818237036704, 9.063309369127512838, -8.731067818237033151 ) ) ;
#50392 = CARTESIAN_POINT ( 'NONE',  ( 5.076628168052704559, 10.17559781766745175, -8.527530157486179263 ) ) ;
#50393 = CARTESIAN_POINT ( 'NONE',  ( 6.565887622018943937, 60.16530133659707502, 12.81628187352647430 ) ) ;
#50394 = EDGE_LOOP ( 'NONE', ( #93264, #74581, #76260, #27939 ) ) ;
#50395 = FACE_OUTER_BOUND ( 'NONE', #19813, .T. ) ;
#50396 = CARTESIAN_POINT ( 'NONE',  ( -4.164238869374099039, 31.80374883491396432, 8.674139862899312516E-16 ) ) ;
#50397 = FILL_AREA_STYLE_COLOUR ( '', #31467 ) ;
#50398 = CARTESIAN_POINT ( 'NONE',  ( -7.287667432647796595, -86.26780665046146623, 4.000000000000000000 ) ) ;
#50399 = CARTESIAN_POINT ( 'NONE',  ( 10.00000000000000178, 29.31368534415483751, 10.88017736071110342 ) ) ;
#50400 = DIRECTION ( 'NONE',  ( 0.000000000000000000, 0.000000000000000000, -1.000000000000000000 ) ) ;
#50401 = CARTESIAN_POINT ( 'NONE',  ( 8.209432707284861408, 15.00000000000000000, -12.55409154915486170 ) ) ;
#50402 = CARTESIAN_POINT ( 'NONE',  ( 12.91533473730993009, 46.60535201082150536, -10.88017736071109987 ) ) ;
#50403 = CARTESIAN_POINT ( 'NONE',  ( -0.8801773607110991993, 47.85535201082150536, -2.915334737309923874 ) ) ;
#50404 = CARTESIAN_POINT ( 'NONE',  ( 3.591859063236761518, 19.95696800326375353, 11.09922568453594849 ) ) ;
#50405 = CARTESIAN_POINT ( 'NONE',  ( 19.84674366389459621, 63.50893115100078745, 7.409399052514197653E-17 ) ) ;
#50406 = CARTESIAN_POINT ( 'NONE',  ( 1.282179089048214760, 0.8662784883469558661, 6.500000000000002665 ) ) ;
#50407 = CARTESIAN_POINT ( 'NONE',  ( 19.84674366389459266, 28.71726448433411960, -2.638427012816827677 ) ) ;
#50408 = PRESENTATION_STYLE_ASSIGNMENT (( #19917 ) ) ;
#50409 = CARTESIAN_POINT ( 'NONE',  ( -0.8801773607111008646, 43.27201867748817676, 2.915334737309923430 ) ) ;
#50410 = ADVANCED_FACE ( 'NONE', ( #41209 ), #71689, .F. ) ;
#50411 = AXIS2_PLACEMENT_3D ( 'NONE', #4400, #34868, #27371 ) ;
#50412 = CARTESIAN_POINT ( 'NONE',  ( 3.591859063236761518, 4.956968003263753531, 11.09922568453594849 ) ) ;
#50413 = CARTESIAN_POINT ( 'NONE',  ( 10.00000000000000178, 59.31368534415484106, 10.88017736071110342 ) ) ;
#50414 = AXIS2_PLACEMENT_3D ( 'NONE', #28994, #44000, #98533 ) ;
#50415 = CARTESIAN_POINT ( 'NONE',  ( 7.361572987183170547, 27.05059781766745175, 9.846743663894590881 ) ) ;
#50416 = CARTESIAN_POINT ( 'NONE',  ( 22.81628187352648496, 51.83196800326376064, -3.434112377981050290 ) ) ;
#50418 =( NAMED_UNIT ( * ) PLANE_ANGLE_UNIT ( ) SI_UNIT ( $, .RADIAN. ) );
#50417 = CARTESIAN_POINT ( 'NONE',  ( 5.076628168052704559, 10.17559781766745175, -8.527530157486179263 ) ) ;
#50419 = EDGE_LOOP ( 'NONE', ( #22597, #47913, #53559 ) ) ;
#50420 = CARTESIAN_POINT ( 'NONE',  ( 14.99999999999997691, 80.32179676972448590, -4.000000000000000000 ) ) ;
#50421 = CARTESIAN_POINT ( 'NONE',  ( 0.1532563361054083140, 36.00893115100078745, 1.131784320476157264E-15 ) ) ;
#50422 = CARTESIAN_POINT ( 'NONE',  ( 19.42250999205614548, 25.98035201082150891, -5.440088680355545492 ) ) ;
#50424 = CARTESIAN_POINT ( 'NONE',  ( 2.917880565312950480, 20.97041550158063217, -12.26659068614894821 ) ) ;
#50423 = CARTESIAN_POINT ( 'NONE',  ( 22.81628187352647785, 56.62363466993042493, 6.195893100308588602E-16 ) ) ;
#50425 = CARTESIAN_POINT ( 'NONE',  ( 14.92337183194729633, 27.67559781766745530, 8.527530157486181039 ) ) ;
#50426 = CARTESIAN_POINT ( 'NONE',  ( -0.8801773607111008646, 18.27201867748817321, 2.915334737309923430 ) ) ;
#50427 = CARTESIAN_POINT ( 'NONE',  ( 24.16423886937410614, 64.51208216824728936, -3.795296366450302550 ) ) ;
#50428 = ORIENTED_EDGE ( 'NONE', *, *, #55560, .F. ) ;
#50429 = CARTESIAN_POINT ( 'NONE',  ( 19.42250999205614193, 15.14701867748817143, 5.440088680355555262 ) ) ;
#50430 = CARTESIAN_POINT ( 'NONE',  ( 10.00000000000000178, 29.31368534415483751, 10.88017736071110342 ) ) ;
#50431 = CARTESIAN_POINT ( 'NONE',  ( 7.084665262690076126, 37.02201867748817676, -10.88017736071110164 ) ) ;
#50432 = ORIENTED_EDGE ( 'NONE', *, *, #94928, .F. ) ;
#50433 = CARTESIAN_POINT ( 'NONE',  ( -4.250000000000000000, 10.25000000000000000, -4.000000000000000000 ) ) ;
#50434 = CARTESIAN_POINT ( 'NONE',  ( 20.88017736071110164, 20.35535201082150891, 2.915334737309930979 ) ) ;
#50435 = CARTESIAN_POINT ( 'NONE',  ( 17.20831665107776587, 64.13393115100079456, -7.208316651077762316 ) ) ;
#50436 = CIRCLE ( 'NONE', #80774, 15.00000000000000000 ) ;
#50437 = CARTESIAN_POINT ( 'NONE',  ( -8.502626202121433607, 14.95077488074853456, 12.05617882333531554 ) ) ;
#50438 = LINE ( 'NONE', #35929, #22854 ) ;
#50439 = CARTESIAN_POINT ( 'NONE',  ( -5.149999999999996803, 98.49999999999998579, -8.525133428036873795 ) ) ;
#50440 = CARTESIAN_POINT ( 'NONE',  ( 10.00000000000000178, 38.05374883491396787, 14.16423886937410082 ) ) ;
#50441 = CARTESIAN_POINT ( 'NONE',  ( 20.88017736071110164, 35.35535201082150536, 2.915334737309930979 ) ) ;
#50442 = CARTESIAN_POINT ( 'NONE',  ( 15.44008868035555260, 29.73035201082150891, 9.422509992056143702 ) ) ;
#50443 = CARTESIAN_POINT ( 'NONE',  ( 1.472469842513823179, 65.59226448433412315, -4.923371831947296329 ) ) ;
#50444 = FACE_OUTER_BOUND ( 'NONE', #83401, .T. ) ;
#50446 = EDGE_CURVE ( 'NONE', #27786, #4847, #41695, .T. ) ;
#50445 = CARTESIAN_POINT ( 'NONE',  ( 2.791683348922237240, 45.38393115100079456, -7.208316651077763204 ) ) ;
#50447 = CARTESIAN_POINT ( 'NONE',  ( 0.1532563361054100626, 20.80059781766744464, -2.638427012816831230 ) ) ;
#50448 = CARTESIAN_POINT ( 'NONE',  ( -3.434112377981067610, -26.91803199673625002, -12.81628187352647252 ) ) ;
#50449 = CARTESIAN_POINT ( 'NONE',  ( -0.8801773607111009756, 8.063685344154837509, 1.068504757029289695E-15 ) ) ;
#50450 = CARTESIAN_POINT ( 'NONE',  ( 14.92337183194729988, 29.34226448433411960, -8.527530157486177487 ) ) ;
#50451 = CARTESIAN_POINT ( 'NONE',  ( 22.81628187352647785, 6.623634669930420493, 6.195893100308588602E-16 ) ) ;
#50453 = CARTESIAN_POINT ( 'NONE',  ( 19.42250999205614193, 50.14701867748817676, 5.440088680355555262 ) ) ;
#50452 = CARTESIAN_POINT ( 'NONE',  ( 20.88017736071110164, 55.35535201082149825, 2.915334737309930979 ) ) ;
#50455 = CARTESIAN_POINT ( 'NONE',  ( 0.6178305044545838731, 59.74863466993041783, 9.382169495545420901 ) ) ;
#50454 = CARTESIAN_POINT ( 'NONE',  ( 20.88017736071110875, 20.77201867748816611, -2.915334737309920765 ) ) ;
#50456 = CARTESIAN_POINT ( 'NONE',  ( -2.266590686148945544, 31.38708216824730002, -7.082119434687050408 ) ) ;
#50457 =( GEOMETRIC_REPRESENTATION_CONTEXT ( 3 ) GLOBAL_UNCERTAINTY_ASSIGNED_CONTEXT ( ( #78333 ) ) GLOBAL_UNIT_ASSIGNED_CONTEXT ( ( #14258, #83735, #53724 ) ) REPRESENTATION_CONTEXT ( 'NONE', 'WORKASPACE' ) );
#50458 = EDGE_CURVE ( 'NONE', #77048, #65600, #59951, .T. ) ;
#50459 = EDGE_CURVE ( 'NONE', #43985, #76019, #66383, .T. ) ;
#50460 = CARTESIAN_POINT ( 'NONE',  ( 20.32896413005680714, 35.57879003517447103, -5.963430220938276349 ) ) ;
#50461 = EDGE_CURVE ( 'NONE', #87279, #49892, #24233, .T. ) ;
#50462 = ORIENTED_EDGE ( 'NONE', *, *, #17647, .T. ) ;
#50463 = CARTESIAN_POINT ( 'NONE',  ( 19.38216949554541202, 0.9986346699304200492, 9.382169495545424454 ) ) ;
#50464 = FACE_OUTER_BOUND ( 'NONE', #6069, .T. ) ;
#50465 = CARTESIAN_POINT ( 'NONE',  ( 20.88017736071110519, 30.56368534415484106, 2.639326808657452039E-16 ) ) ;
#50466 = CARTESIAN_POINT ( 'NONE',  ( 18.52753015748617571, 58.09226448433411605, 4.923371831947298993 ) ) ;
#50467 = ORIENTED_EDGE ( 'NONE', *, *, #17959, .T. ) ;
#50468 = CARTESIAN_POINT ( 'NONE',  ( 19.84674366389459266, 13.71726448433411782, -2.638427012816827677 ) ) ;
#50469 = CARTESIAN_POINT ( 'NONE',  ( 5.963430220938279902, 8.021642702460848540, -10.32896413005680181 ) ) ;
#50470 = CARTESIAN_POINT ( 'NONE',  ( 2.791683348922237240, 25.38393115100078390, -7.208316651077763204 ) ) ;
#50471 = CARTESIAN_POINT ( 'NONE',  ( 7.361572987183170547, 7.050597817667451750, 9.846743663894590881 ) ) ;
#50472 = MECHANICAL_DESIGN_GEOMETRIC_PRESENTATION_REPRESENTATION (  '', ( #28134 ), #60104 ) ;
#50473 = CARTESIAN_POINT ( 'NONE',  ( 19.84674366389459621, 3.508931151000785231, 7.409399052514197653E-17 ) ) ;
#50474 = DIRECTION ( 'NONE',  ( 0.000000000000000000, 0.000000000000000000, 1.000000000000000000 ) ) ;
#50476 = LINE ( 'NONE', #80980, #85081 ) ;
#50475 = CARTESIAN_POINT ( 'NONE',  ( 10.00000000000000178, 69.31368534415484817, 10.88017736071110342 ) ) ;
#50477 = CARTESIAN_POINT ( 'NONE',  ( 19.84674366389459621, 3.508931151000785231, 7.409399052514197653E-17 ) ) ;
#50478 = CIRCLE ( 'NONE', #55263, 15.00000000000000000 ) ;
#50480 = ORIENTED_EDGE ( 'NONE', *, *, #96429, .T. ) ;
#50479 = CARTESIAN_POINT ( 'NONE',  ( 7.361572987183169658, 19.96726448433411960, -9.846743663894592657 ) ) ;
#50481 = AXIS2_PLACEMENT_3D ( 'NONE', #40306, #70315, #31795 ) ;
#50482 = LINE ( 'NONE', #80985, #56564 ) ;
#50484 = EDGE_CURVE ( 'NONE', #27552, #12702, #70220, .T. ) ;
#50483 = CARTESIAN_POINT ( 'NONE',  ( 13.43411237798106583, 2.665301336597086568, -12.81628187352647252 ) ) ;
#50485 = B_SPLINE_CURVE_WITH_KNOTS ( 'NONE', 3,
 ( #24431, #8911, #17902, #23936 ),
 .UNSPECIFIED., .F., .F.,
 ( 4, 4 ),
 ( 0.000000000000000000, 0.001036303429213384589 ),
 .UNSPECIFIED. ) ;
#50486 = VERTEX_POINT ( 'NONE', #79182 ) ;
#50487 = CARTESIAN_POINT ( 'NONE',  ( 20.88017736071110519, 5.563685344154837509, 2.639326808657452039E-16 ) ) ;
#50488 = VECTOR ( 'NONE', #59689, 1000.000000000000000 ) ;
#50489 = CARTESIAN_POINT ( 'NONE',  ( -0.3689425029237881626, 17.42874883491397142, 10.36894250292379027 ) ) ;
#50490 = UNCERTAINTY_MEASURE_WITH_UNIT (LENGTH_MEASURE( 1.000000000000000082E-05 ), #65354, 'distance_accuracy_value', 'NONE');
#50491 = DIRECTION ( 'NONE',  ( 0.000000000000000000, 1.000000000000000000, 0.000000000000000000 ) ) ;
#50492 = EDGE_CURVE ( 'NONE', #59916, #37810, #33664, .T. ) ;
#50493 = CARTESIAN_POINT ( 'NONE',  ( 24.16423886937409904, 19.09541550158063927, 3.795296366450317205 ) ) ;
#50494 = CARTESIAN_POINT ( 'NONE',  ( -0.3689425029237898834, 31.17874883491396787, -10.36894250292378850 ) ) ;
#50496 = CARTESIAN_POINT ( 'NONE',  ( 10.00000000000000178, 69.31368534415484817, 10.88017736071110342 ) ) ;
#50495 = CARTESIAN_POINT ( 'NONE',  ( -4.164238869374098151, 16.59541550158063927, -3.795296366450310543 ) ) ;
#50497 = CARTESIAN_POINT ( 'NONE',  ( 15.44008868035555793, 31.39701867748817676, -9.422509992056140149 ) ) ;
#50498 = CARTESIAN_POINT ( 'NONE',  ( -11.49638213510188756, 14.95077488074853456, 9.245501498401852203 ) ) ;
#50499 = ORIENTED_EDGE ( 'NONE', *, *, #12228, .F. ) ;
#50500 = CARTESIAN_POINT ( 'NONE',  ( 0.1532563361054100626, 20.80059781766744464, -2.638427012816831230 ) ) ;
#50502 = CARTESIAN_POINT ( 'NONE',  ( 10.00000000000000000, 34.75893115100078745, -9.846743663894594434 ) ) ;
#50501 = CARTESIAN_POINT ( 'NONE',  ( 2.035157376598824452, 53.68868534415484817, 7.964842623401179544 ) ) ;
#50503 = CARTESIAN_POINT ( 'NONE',  ( 19.42250999205614193, 5.147018677488171434, 5.440088680355555262 ) ) ;
#50504 = CARTESIAN_POINT ( 'NONE',  ( 6.565887622018943937, 45.16530133659708923, 12.81628187352647430 ) ) ;
#50505 = CARTESIAN_POINT ( 'NONE',  ( 7.361572987183170547, 57.05059781766744464, 9.846743663894590881 ) ) ;
#50506 = CARTESIAN_POINT ( 'NONE',  ( 14.43100913237647731, 15.00000000000000000, -1.412789942450803027 ) ) ;
#50508 = CARTESIAN_POINT ( 'NONE',  ( 0.6178305044545818747, 48.49863466993042493, -9.382169495545419124 ) ) ;
#50507 = AXIS2_PLACEMENT_3D ( 'NONE', #32166, #78172, #24204 ) ;
#50509 = CARTESIAN_POINT ( 'NONE',  ( -12.26659068614894110, -27.77958449841936073, 7.082119434687058401 ) ) ;
#50510 = PRESENTATION_LAYER_ASSIGNMENT (  '', '', ( #95248 ) ) ;
#50511 = CARTESIAN_POINT ( 'NONE',  ( 18.52753015748617571, 43.09226448433412315, 4.923371831947298993 ) ) ;
#50512 = CARTESIAN_POINT ( 'NONE',  ( 6.204703633549690345, 25.76208216824730712, -14.16423886937410259 ) ) ;
#50513 = ORIENTED_EDGE ( 'NONE', *, *, #6804, .F. ) ;
#50514 = CARTESIAN_POINT ( 'NONE',  ( 8.375939845167756914, -0.03417435944610275333, -11.52849216984298941 ) ) ;
#50515 = CARTESIAN_POINT ( 'NONE',  ( 0.5774900079438590739, 47.64701867748817676, -5.440088680355550821 ) ) ;
#50516 = CARTESIAN_POINT ( 'NONE',  ( 4.559911319644449179, 48.89701867748817676, 9.422509992056141925 ) ) ;
#50517 = CARTESIAN_POINT ( 'NONE',  ( -2.266590686148945544, 51.38708216824730357, -7.082119434687050408 ) ) ;
#50518 = CARTESIAN_POINT ( 'NONE',  ( 12.63842701281683034, 62.46726448433410894, 9.846743663894596210 ) ) ;
#50519 = LINE ( 'NONE', #13006, #24159 ) ;
#50520 = CARTESIAN_POINT ( 'NONE',  ( 20.88017736071110875, 40.77201867748818387, -2.915334737309920765 ) ) ;
#50521 = CARTESIAN_POINT ( 'NONE',  ( -6.767445849361333643, 0.5000000000000004441, 13.38662304974491946 ) ) ;
#50522 = CARTESIAN_POINT ( 'NONE',  ( 0.6178305044545838731, 24.74863466993042493, 9.382169495545420901 ) ) ;
#50523 = CARTESIAN_POINT ( 'NONE',  ( 10.00000000000000000, 49.75893115100078745, -9.846743663894594434 ) ) ;
#50524 = CARTESIAN_POINT ( 'NONE',  ( 3.469446951953614189E-15, 9.313685344154846391, 10.88017736071110342 ) ) ;
#50525 = FACE_OUTER_BOUND ( 'NONE', #15608, .T. ) ;
#50526 = CARTESIAN_POINT ( 'NONE',  ( 17.96484262340118221, 61.18868534415482685, -7.964842623401177768 ) ) ;
#50527 = ORIENTED_EDGE ( 'NONE', *, *, #10881, .T. ) ;
#50528 = VECTOR ( 'NONE', #72964, 1000.000000000000227 ) ;
#50529 = CARTESIAN_POINT ( 'NONE',  ( 2.035157376598822676, 2.438685344154837953, -7.964842623401177768 ) ) ;
#50530 = DIRECTION ( 'NONE',  ( 1.563194018672220156E-13, 0.000000000000000000, 1.000000000000000000 ) ) ;
#50531 = CARTESIAN_POINT ( 'NONE',  ( 15.44008868035555793, 66.39701867748817676, -9.422509992056140149 ) ) ;
#50532 = CARTESIAN_POINT ( 'NONE',  ( 10.00000000000000000, 4.758931151000784787, -9.846743663894594434 ) ) ;
#50533 = CARTESIAN_POINT ( 'NONE',  ( 18.00000000000000000, 77.35022402049111179, -4.131279366365265382 ) ) ;
#50534 = CARTESIAN_POINT ( 'NONE',  ( 17.20831665107776587, 29.13393115100078390, -7.208316651077762316 ) ) ;
#50535 = CARTESIAN_POINT ( 'NONE',  ( 4.559911319644449179, 17.23035201082150536, -9.422509992056141925 ) ) ;
#50536 = MECHANICAL_DESIGN_GEOMETRIC_PRESENTATION_REPRESENTATION (  '', ( #45776 ), #47315 ) ;
#50537 = CARTESIAN_POINT ( 'NONE',  ( 0.6178305044545818747, 3.498634669930420049, -9.382169495545419124 ) ) ;
#50539 = DIRECTION ( 'NONE',  ( -0.7826081568524105858, 0.000000000000000000, -0.6225146366376238527 ) ) ;
#50538 = CARTESIAN_POINT ( 'NONE',  ( 20.88017736071110519, 35.56368534415484106, 2.639326808657452039E-16 ) ) ;
#50540 = DIRECTION ( 'NONE',  ( 0.000000000000000000, 0.000000000000000000, -1.000000000000000000 ) ) ;
#50541 = CARTESIAN_POINT ( 'NONE',  ( 19.38216949554541557, 42.24863466993041783, -9.382169495545420901 ) ) ;
#50542 = VERTEX_POINT ( 'NONE', #9214 ) ;
#50543 = CARTESIAN_POINT ( 'NONE',  ( 19.42250999205614548, 60.98035201082151247, -5.440088680355545492 ) ) ;
#50545 = CARTESIAN_POINT ( 'NONE',  ( 0.000000000000000000, 0.5000000000000004441, 0.000000000000000000 ) ) ;
#50544 = CARTESIAN_POINT ( 'NONE',  ( 19.38216949554541202, 15.99863466993042138, 9.382169495545424454 ) ) ;
#50546 = CARTESIAN_POINT ( 'NONE',  ( 19.42250999205614193, 45.14701867748817676, 5.440088680355555262 ) ) ;
#50547 = CARTESIAN_POINT ( 'NONE',  ( 0.1532563361054082862, 61.21726448433412315, 2.638427012816831674 ) ) ;
#50548 = CARTESIAN_POINT ( 'NONE',  ( 20.36894250292379382, 58.67874883491396076, 10.36894250292379205 ) ) ;
#50549 = CARTESIAN_POINT ( 'NONE',  ( 12.63842701281683034, 57.46726448433411605, 9.846743663894596210 ) ) ;
#50550 = CARTESIAN_POINT ( 'NONE',  ( -0.8801773607110991993, 67.85535201082151957, -2.915334737309923874 ) ) ;
#50551 = CARTESIAN_POINT ( 'NONE',  ( 7.084665262690076126, 64.10535201082150536, 10.88017736071109987 ) ) ;
#50552 = FACE_OUTER_BOUND ( 'NONE', #40374, .T. ) ;
#50553 = CARTESIAN_POINT ( 'NONE',  ( -0.3689425029237898834, 31.17874883491396787, -10.36894250292378850 ) ) ;
#50554 = COLOUR_RGB ( '', 0.08235294, 0.09019608, 0.10196078) ;
#50555 = CARTESIAN_POINT ( 'NONE',  ( 11.20711848508407016, -56.83082008004717522, -3.750000000000000000 ) ) ;
#50556 = CARTESIAN_POINT ( 'NONE',  ( -4.021995598253403692, -6.415937870592102854, -4.000000000000000000 ) ) ;
#50557 = MECHANICAL_DESIGN_GEOMETRIC_PRESENTATION_REPRESENTATION (  '', ( #37808 ), #45711 ) ;
#50558 = VERTEX_POINT ( 'NONE', #39727 ) ;
#50559 = VERTEX_POINT ( 'NONE', #3692 ) ;
#50560 = CARTESIAN_POINT ( 'NONE',  ( -2.266590686148945544, 62.22041550158063927, 7.082119434687048631 ) ) ;
#50561 = CARTESIAN_POINT ( 'NONE',  ( 24.16423886937410614, 44.51208216824730357, -3.795296366450302550 ) ) ;
#50562 = CARTESIAN_POINT ( 'NONE',  ( 17.20831665107776587, 29.13393115100078390, -7.208316651077762316 ) ) ;
#50563 = CARTESIAN_POINT ( 'NONE',  ( 16.40814093676323893, 25.79030133659708923, 11.09922568453595026 ) ) ;
#50564 = CARTESIAN_POINT ( 'NONE',  ( -7.750000000000000000, 83.99999999999994316, 4.000000000000000000 ) ) ;
#50565 = CARTESIAN_POINT ( 'NONE',  ( 4.559911319644449179, 67.23035201082150536, -9.422509992056141925 ) ) ;
#50566 = CARTESIAN_POINT ( 'NONE',  ( 13.79529636645030344, 43.26208216824730357, 14.16423886937410614 ) ) ;
#50567 = AXIS2_PLACEMENT_3D ( 'NONE', #9657, #32637, #18148 ) ;
#50568 =( BOUNDED_CURVE ( )  B_SPLINE_CURVE ( 2, ( #68472, #8447, #13589, #30445, #98499, #60945, #22981, #29954, #53948, #966, #60459, #90949, #15481 ),
 .UNSPECIFIED., .F., .T. ) 
 B_SPLINE_CURVE_WITH_KNOTS ( ( 3, 2, 2, 2, 2, 2, 3 ),
 ( 0.6666666666666666297, 0.6722222222222222765, 0.6777777777777778123, 0.6833333333333333481, 0.6888888888888888840, 0.6944444444444444198, 0.6999999999999999556 ),
 .UNSPECIFIED. ) 
 CURVE ( )  GEOMETRIC_REPRESENTATION_ITEM ( )  RATIONAL_B_SPLINE_CURVE ( ( 1.000000000000000000, 0.9659258262890684232, 1.000000000000000000, 0.9659258262890684232, 1.000000000000000000, 0.9659258262890684232, 1.000000000000000000, 0.9659258262890684232, 1.000000000000000000, 0.9659258262890684232, 1.000000000000000000, 0.9659258262890684232, 1.000000000000000000 ) ) 
 REPRESENTATION_ITEM ( '' )  );
#50569 = CARTESIAN_POINT ( 'NONE',  ( -4.838527690343427778, 14.63606918327098327, -14.19819177887737638 ) ) ;
#50570 = CARTESIAN_POINT ( 'NONE',  ( 17.20831665107776587, 7.883931151000784787, 7.208316651077764980 ) ) ;
#50571 = CARTESIAN_POINT ( 'NONE',  ( -14.62617646268096827, 14.49999999999999112, 3.327906561566773558 ) ) ;
#50572 = CARTESIAN_POINT ( 'NONE',  ( 4.923371831947301658, -2.324402182332541145, 8.527530157486175710 ) ) ;
#50573 = ORIENTED_EDGE ( 'NONE', *, *, #88343, .F. ) ;
#50574 = ORIENTED_EDGE ( 'NONE', *, *, #48327, .T. ) ;
#50576 = EDGE_CURVE ( 'NONE', #24815, #80599, #78197, .T. ) ;
#50575 =( NAMED_UNIT ( * ) PLANE_ANGLE_UNIT ( ) SI_UNIT ( $, .RADIAN. ) );
#50577 = ORIENTED_EDGE ( 'NONE', *, *, #16669, .F. ) ;
#50578 = CARTESIAN_POINT ( 'NONE',  ( -2.266590686148945544, 11.38708216824730179, -7.082119434687050408 ) ) ;
#50580 = CARTESIAN_POINT ( 'NONE',  ( 10.00000000000000000, 26.81368534415484106, -10.88017736071110342 ) ) ;
#50579 = CARTESIAN_POINT ( 'NONE',  ( 0.5774900079438590739, 22.64701867748817321, -5.440088680355550821 ) ) ;
#50582 = CARTESIAN_POINT ( 'NONE',  ( 22.81628187352647785, 16.62363466993042138, 6.195893100308588602E-16 ) ) ;
#50581 = CARTESIAN_POINT ( 'NONE',  ( 19.84674366389459266, 53.30059781766744464, 2.638427012816836559 ) ) ;
#50583 =( GEOMETRIC_REPRESENTATION_CONTEXT ( 3 ) GLOBAL_UNCERTAINTY_ASSIGNED_CONTEXT ( ( #34286 ) ) GLOBAL_UNIT_ASSIGNED_CONTEXT ( ( #74458, #58470, #12975 ) ) REPRESENTATION_CONTEXT ( 'NONE', 'WORKASPACE' ) );
#50584 = VECTOR ( 'NONE', #35547, 1000.000000000000000 ) ;
#50585 = EDGE_CURVE ( 'NONE', #47609, #18352, #53535, .T. ) ;
#50586 = AXIS2_PLACEMENT_3D ( 'NONE', #28497, #13497, #74479 ) ;
#50587 = CARTESIAN_POINT ( 'NONE',  ( 10.00000000000000000, 27.87363466993042138, -12.81628187352647608 ) ) ;
#50588 = EDGE_CURVE ( 'NONE', #27809, #98371, #43713, .T. ) ;
#50589 = ORIENTED_EDGE ( 'NONE', *, *, #35057, .T. ) ;
#50590 = CARTESIAN_POINT ( 'NONE',  ( 7.361572987183170547, 32.05059781766745175, 9.846743663894590881 ) ) ;
#50591 = CARTESIAN_POINT ( 'NONE',  ( 17.08211943468705130, 63.47041550158063927, 12.26659068614894998 ) ) ;
#50592 = ORIENTED_EDGE ( 'NONE', *, *, #82133, .F. ) ;
#50593 = CARTESIAN_POINT ( 'NONE',  ( 15.44008868035555260, 4.730352010821505360, 9.422509992056143702 ) ) ;
#50594 = ORIENTED_EDGE ( 'NONE', *, *, #53716, .F. ) ;
#50595 = CARTESIAN_POINT ( 'NONE',  ( 2.035157376598822676, 42.43868534415483396, -7.964842623401177768 ) ) ;
#50596 = CARTESIAN_POINT ( 'NONE',  ( 20.88017736071110164, 40.35535201082150536, 2.915334737309930979 ) ) ;
#50597 = CARTESIAN_POINT ( 'NONE',  ( 15.44008868035555793, 46.39701867748817676, -9.422509992056140149 ) ) ;
#50598 = FILL_AREA_STYLE ('',( #11122 ) ) ;
#50599 = CARTESIAN_POINT ( 'NONE',  ( 15.44008868035555793, 36.39701867748816966, -9.422509992056140149 ) ) ;
#50600 = LINE ( 'NONE', #88588, #26721 ) ;
#50602 = VERTEX_POINT ( 'NONE', #27647 ) ;
#50601 = DIRECTION ( 'NONE',  ( -1.000000000000000000, 0.000000000000000000, 0.000000000000000000 ) ) ;
#50603 = CARTESIAN_POINT ( 'NONE',  ( 19.84674366389459266, 28.30059781766745886, 2.638427012816836559 ) ) ;
#50604 = ORIENTED_EDGE ( 'NONE', *, *, #85750, .F. ) ;
#50605 = CARTESIAN_POINT ( 'NONE',  ( 17.20831665107776587, 57.88393115100078745, 7.208316651077764980 ) ) ;
#50606 = CARTESIAN_POINT ( 'NONE',  ( 0.000000000000000000, 14.49999999999999822, 0.000000000000000000 ) ) ;
#50607 = COLOUR_RGB ( '', 0.72549020, 0.75294118, 0.79215686) ;
#50608 = EDGE_CURVE ( 'NONE', #11604, #28932, #65641, .T. ) ;
#50609 = DIRECTION ( 'NONE',  ( 0.000000000000000000, 1.000000000000000000, 0.000000000000000000 ) ) ;
#50610 = CARTESIAN_POINT ( 'NONE',  ( -11.57731665747925831, 12.81546821322845986, 0.2203853198082409703 ) ) ;
#50611 = DIRECTION ( 'NONE',  ( 0.3007057995042701770, 0.000000000000000000, 0.9537169507482278208 ) ) ;
#50613 = CARTESIAN_POINT ( 'NONE',  ( 19.84674366389459266, 38.71726448433412315, -2.638427012816827677 ) ) ;
#50612 = CARTESIAN_POINT ( 'NONE',  ( -3.270351084886603310, 0.04962888917231444985, -14.38617789677966385 ) ) ;
#50614 = CARTESIAN_POINT ( 'NONE',  ( 2.917880565312948704, 57.63708216824731068, 12.26659068614894643 ) ) ;
#50615 = CARTESIAN_POINT ( 'NONE',  ( 6.767445849361153343, 15.00000000000000000, 13.38662304974501360 ) ) ;
#50616 = ORIENTED_EDGE ( 'NONE', *, *, #50458, .F. ) ;
#50617 = DIRECTION ( 'NONE',  ( 0.000000000000000000, 1.000000000000000000, 0.000000000000000000 ) ) ;
#50618 = CARTESIAN_POINT ( 'NONE',  ( 5.076628168052703671, 31.84226448433412315, 8.527530157486179263 ) ) ;
#50619 = DIRECTION ( 'NONE',  ( -0.7826081568524232424, -0.000000000000000000, 0.6225146366376079765 ) ) ;
#50620 = CARTESIAN_POINT ( 'NONE',  ( 3.591859063236761518, 4.956968003263753531, 11.09922568453594849 ) ) ;
#50621 = CARTESIAN_POINT ( 'NONE',  ( 19.84674366389459266, 8.717264484334116048, -2.638427012816827677 ) ) ;
#50622 = CARTESIAN_POINT ( 'NONE',  ( 0.000000000000000000, 15.00000000000000000, 0.000000000000000000 ) ) ;
#50623 = CARTESIAN_POINT ( 'NONE',  ( 10.00000000000000000, 9.758931151000785675, -9.846743663894594434 ) ) ;
#50624 = CARTESIAN_POINT ( 'NONE',  ( 18.52753015748618282, 53.92559781766745175, -4.923371831947291888 ) ) ;
#50625 = FACE_OUTER_BOUND ( 'NONE', #55214, .T. ) ;
#50626 = VECTOR ( 'NONE', #92061, 1000.000000000000114 ) ;
#50627 = EDGE_LOOP ( 'NONE', ( #69778, #83643, #47520, #48615 ) ) ;
#50628 = CARTESIAN_POINT ( 'NONE',  ( 12.91533473730993009, 6.605352010821504471, -10.88017736071109987 ) ) ;
#50629 = CARTESIAN_POINT ( 'NONE',  ( 6.204703633549690345, 5.762082168247301794, -14.16423886937410259 ) ) ;
#50630 = CARTESIAN_POINT ( 'NONE',  ( 5.076628168052703671, 11.84226448433411960, 8.527530157486179263 ) ) ;
#50631 = CARTESIAN_POINT ( 'NONE',  ( -0.8801773607111008646, 53.27201867748816966, 2.915334737309923430 ) ) ;
#50633 = CARTESIAN_POINT ( 'NONE',  ( -5.112373461513591621, -25.53775085953292390, -3.750000000000000000 ) ) ;
#50632 = CARTESIAN_POINT ( 'NONE',  ( 21.09922568453595559, 27.04030133659708568, -6.408140936763230044 ) ) ;
#50634 = CARTESIAN_POINT ( 'NONE',  ( 17.96484262340118221, 6.188685344154836621, -7.964842623401177768 ) ) ;
#50635 = DIRECTION ( 'NONE',  ( 1.000000000000000000, 0.000000000000000000, -0.000000000000000000 ) ) ;
#50636 = CARTESIAN_POINT ( 'NONE',  ( 20.05723567505238947, 0.1676365378933190875, -6.413539670616452248 ) ) ;
#50637 = AXIS2_PLACEMENT_3D ( 'NONE', #12105, #25288, #34591 ) ;
#50638 = CARTESIAN_POINT ( 'NONE',  ( 16.40814093676323893, 0.7903013365970867898, 11.09922568453595026 ) ) ;
#50639 = CARTESIAN_POINT ( 'NONE',  ( 2.791683348922237240, 65.38393115100078035, -7.208316651077763204 ) ) ;
#50640 = CARTESIAN_POINT ( 'NONE',  ( 19.84674366389459621, 13.50893115100078568, 7.409399052514197653E-17 ) ) ;
#50641 = CARTESIAN_POINT ( 'NONE',  ( 9.422509992056141925, -29.01964798917849109, -5.440088680355554374 ) ) ;
#50642 = CARTESIAN_POINT ( 'NONE',  ( 21.09922568453594849, 16.20696800326375353, 6.408140936763242479 ) ) ;
#50643 = CARTESIAN_POINT ( 'NONE',  ( -11.62646502397220871, -81.99905065409890881, -4.000000000003602452 ) ) ;
#50645 = CARTESIAN_POINT ( 'NONE',  ( -0.9082943533608713871, 15.00000000000000000, -14.47152380946376660 ) ) ;
#50644 = CARTESIAN_POINT ( 'NONE',  ( -0.8801773607110991993, 27.85535201082150181, -2.915334737309923874 ) ) ;
#50646 = CARTESIAN_POINT ( 'NONE',  ( 12.50534872682730914, 15.00000000000000000, -7.339363270777500503 ) ) ;
#50647 = CARTESIAN_POINT ( 'NONE',  ( 17.08211943468705130, 53.47041550158063217, 12.26659068614894998 ) ) ;
#50648 = AXIS2_PLACEMENT_3D ( 'NONE', #27846, #73346, #23208 ) ;
#50649 = CARTESIAN_POINT ( 'NONE',  ( 0.000000000000000000, 15.00000000000000000, 0.000000000000000000 ) ) ;
#50650 = AXIS2_PLACEMENT_3D ( 'NONE', #60016, #20556, #13041 ) ;
#50651 = CARTESIAN_POINT ( 'NONE',  ( 2.035157376598822676, 27.43868534415483396, -7.964842623401177768 ) ) ;
#50652 = CARTESIAN_POINT ( 'NONE',  ( 2.791683348922237240, 45.38393115100079456, -7.208316651077763204 ) ) ;
#50653 = CARTESIAN_POINT ( 'NONE',  ( 0.5774900079438607392, 58.48035201082151247, 5.440088680355550821 ) ) ;
#50654 = CARTESIAN_POINT ( 'NONE',  ( -4.164238869374098151, 31.59541550158063927, -3.795296366450310543 ) ) ;
#50655 = DIRECTION ( 'NONE',  ( 0.8141155183563107967, 0.000000000000000000, 0.5807029557109515405 ) ) ;
#50656 = CARTESIAN_POINT ( 'NONE',  ( 14.92337183194729633, 37.67559781766745175, 8.527530157486181039 ) ) ;
#50657 = CARTESIAN_POINT ( 'NONE',  ( 6.565887622018943937, 65.16530133659709634, 12.81628187352647430 ) ) ;
#50658 = CARTESIAN_POINT ( 'NONE',  ( 5.076628168052703671, 66.84226448433412315, 8.527530157486179263 ) ) ;
#50659 = ORIENTED_EDGE ( 'NONE', *, *, #60997, .F. ) ;
#50660 = CARTESIAN_POINT ( 'NONE',  ( 19.42250999205614548, 30.98035201082150536, -5.440088680355545492 ) ) ;
#50661 = LINE ( 'NONE', #87663, #38148 ) ;
#50662 = CARTESIAN_POINT ( 'NONE',  ( 14.49999999999999822, 11.50000000000000000, -5.000000000000000000 ) ) ;
#50663 = CARTESIAN_POINT ( 'NONE',  ( 10.00000000000000178, 9.313685344154839285, 10.88017736071110342 ) ) ;
#50664 = CARTESIAN_POINT ( 'NONE',  ( 17.96484262340118221, 66.18868534415483396, -7.964842623401177768 ) ) ;
#50665 = CARTESIAN_POINT ( 'NONE',  ( -2.266590686148945544, 26.38708216824730357, -7.082119434687050408 ) ) ;
#50666 = EDGE_CURVE ( 'NONE', #45674, #36088, #81143, .T. ) ;
#50667 = CARTESIAN_POINT ( 'NONE',  ( 10.00000000000000000, 9.758931151000785675, -9.846743663894594434 ) ) ;
#50668 = CARTESIAN_POINT ( 'NONE',  ( 5.076628168052704559, 60.17559781766745175, -8.527530157486179263 ) ) ;
#50669 = CARTESIAN_POINT ( 'NONE',  ( 2.035157376598822676, 32.43868534415483396, -7.964842623401177768 ) ) ;
#50670 = CARTESIAN_POINT ( 'NONE',  ( 19.05914839598885280, 64.96693863883976405, 6.499999999999962697 ) ) ;
#50671 = PLANE ( 'NONE',  #82506 ) ;
#50672 = EDGE_CURVE ( 'NONE', #61531, #27349, #20150, .T. ) ;
#50673 = VERTEX_POINT ( 'NONE', #74123 ) ;
#50674 = DIRECTION ( 'NONE',  ( 1.000000000000000000, -0.000000000000000000, -0.000000000000000000 ) ) ;
#50675 = CARTESIAN_POINT ( 'NONE',  ( 7.361572987183170547, 47.05059781766745175, 9.846743663894590881 ) ) ;
#50676 = ORIENTED_EDGE ( 'NONE', *, *, #31276, .F. ) ;
#50677 = VERTEX_POINT ( 'NONE', #58133 ) ;
#50678 = CARTESIAN_POINT ( 'NONE',  ( 3.014428414850134796, 9.380135511184867880, 11.24999999999999822 ) ) ;
#50679 = CARTESIAN_POINT ( 'NONE',  ( 22.26659068614894466, 13.88708216824730179, 7.082119434687054849 ) ) ;
#50680 = CARTESIAN_POINT ( 'NONE',  ( 2.917880565312950480, 5.970415501580634832, -12.26659068614894821 ) ) ;
#50681 = CARTESIAN_POINT ( 'NONE',  ( 4.559911319644449179, 53.89701867748817676, 9.422509992056141925 ) ) ;
#50682 = CARTESIAN_POINT ( 'NONE',  ( 10.00000000000000000, 55.55374883491396787, -14.16423886937410082 ) ) ;
#50683 = CARTESIAN_POINT ( 'NONE',  ( 3.591859063236763294, 3.290301336597087012, -11.09922568453595026 ) ) ;
#50684 = CARTESIAN_POINT ( 'NONE',  ( 2.791683348922240793, 31.63393115100078745, 7.208316651077764092 ) ) ;
#50685 = CARTESIAN_POINT ( 'NONE',  ( -10.95094547707107502, -94.44763431416964750, 4.000000000000000000 ) ) ;
#50687 = CARTESIAN_POINT ( 'NONE',  ( 16.40814093676324603, 12.45696800326375353, -11.09922568453594671 ) ) ;
#50686 = CARTESIAN_POINT ( 'NONE',  ( 2.035157376598822676, 27.43868534415483396, -7.964842623401177768 ) ) ;
#50688 = CARTESIAN_POINT ( 'NONE',  ( 17.08211943468705130, 3.470415501580634388, 12.26659068614894998 ) ) ;
#50689 = CARTESIAN_POINT ( 'NONE',  ( 20.88017736071110164, 15.35535201082150358, 2.915334737309930979 ) ) ;
#50690 = CARTESIAN_POINT ( 'NONE',  ( -1.926860441876562247, 67.45379003517449235, -3.195792623639530650 ) ) ;
#50691 = LINE ( 'NONE', #66170, #82694 ) ;
#50692 = CARTESIAN_POINT ( 'NONE',  ( -0.8801773607111008646, 38.27201867748816255, 2.915334737309923430 ) ) ;
#50693 = CARTESIAN_POINT ( 'NONE',  ( 9.846743663894590881, -36.28273551566587685, -2.638427012816833894 ) ) ;
#50694 = VERTEX_POINT ( 'NONE', #88644 ) ;
#50695 = DIRECTION ( 'NONE',  ( -0.000000000000000000, -1.000000000000000000, -0.000000000000000000 ) ) ;
#50696 = EDGE_LOOP ( 'NONE', ( #12120, #65685, #82086, #9630 ) ) ;
#50697 = EDGE_LOOP ( 'NONE', ( #10712, #37168, #76986, #82289 ) ) ;
#50698 = CARTESIAN_POINT ( 'NONE',  ( 10.00000000000000178, 48.05374883491396787, 14.16423886937410082 ) ) ;
#50699 = CARTESIAN_POINT ( 'NONE',  ( 17.20831665107776587, 52.88393115100078035, 7.208316651077764980 ) ) ;
#50700 = CARTESIAN_POINT ( 'NONE',  ( 20.88017736071110875, 55.77201867748816966, -2.915334737309920765 ) ) ;
#50701 = VECTOR ( 'NONE', #44093, 1000.000000000000114 ) ;
#50702 = DIRECTION ( 'NONE',  ( -0.000000000000000000, -1.000000000000000000, -0.000000000000000000 ) ) ;
#50703 = AXIS2_PLACEMENT_3D ( 'NONE', #282, #59752, #60251 ) ;
#50704 = CARTESIAN_POINT ( 'NONE',  ( 0.5774900079438607392, 58.48035201082151247, 5.440088680355550821 ) ) ;
#50705 = ADVANCED_FACE ( 'NONE', ( #26667 ), #19172, .F. ) ;
#50706 = CARTESIAN_POINT ( 'NONE',  ( -2.816281873526473856, 59.33196800326374643, 3.434112377981055619 ) ) ;
#50707 = CARTESIAN_POINT ( 'NONE',  ( -9.382169495545422677, 8.498634669930423158, -9.382169495545417348 ) ) ;
#50708 = ADVANCED_FACE ( 'NONE', ( #43144 ), #31185, .T. ) ;
#50709 = EDGE_LOOP ( 'NONE', ( #93979, #20281, #22374, #63506, #66564 ) ) ;
#50710 = CARTESIAN_POINT ( 'NONE',  ( 15.44008868035555260, 49.73035201082150536, 9.422509992056143702 ) ) ;
#50711 = CARTESIAN_POINT ( 'NONE',  ( 2.917880565312950480, 20.97041550158063217, -12.26659068614894821 ) ) ;
#50712 = CARTESIAN_POINT ( 'NONE',  ( 10.00000000000000000, 27.87363466993042138, -12.81628187352647608 ) ) ;
#50713 = ORIENTED_EDGE ( 'NONE', *, *, #19665, .F. ) ;
#50714 = CARTESIAN_POINT ( 'NONE',  ( 3.591859063236761518, 44.95696800326376064, 11.09922568453594849 ) ) ;
#50715 = CIRCLE ( 'NONE', #45936, 0.2500000000000002220 ) ;
#50716 = CARTESIAN_POINT ( 'NONE',  ( 10.00000000000000178, 32.25893115100078745, 9.846743663894594434 ) ) ;
#50717 = CARTESIAN_POINT ( 'NONE',  ( 2.035157376598824452, 8.688685344154839285, 7.964842623401179544 ) ) ;
#50718 = CARTESIAN_POINT ( 'NONE',  ( 3.591859063236761518, 49.95696800326375353, 11.09922568453594849 ) ) ;
#50719 = DIRECTION ( 'NONE',  ( 0.2334453638559155775, 0.000000000000000000, -0.9723699203976741146 ) ) ;
#50720 = CARTESIAN_POINT ( 'NONE',  ( 2.791683348922237240, 45.38393115100079456, -7.208316651077763204 ) ) ;
#50721 = AXIS2_PLACEMENT_3D ( 'NONE', #38844, #6862, #860 ) ;
#50722 = MECHANICAL_DESIGN_GEOMETRIC_PRESENTATION_REPRESENTATION (  '', ( #71513 ), #34793 ) ;
#50723 = AXIS2_PLACEMENT_3D ( 'NONE', #74031, #97559, #81534 ) ;
#50725 = ORIENTED_EDGE ( 'NONE', *, *, #25344, .T. ) ;
#50724 = CARTESIAN_POINT ( 'NONE',  ( -0.8801773607110991993, 67.85535201082151957, -2.915334737309923874 ) ) ;
#50727 = EDGE_CURVE ( 'NONE', #20156, #47721, #43957, .T. ) ;
#50726 = CARTESIAN_POINT ( 'NONE',  ( 0.000000000000000000, 15.00000000000000000, 0.000000000000000000 ) ) ;
#50728 = CARTESIAN_POINT ( 'NONE',  ( 0.000000000000000000, 15.00000000000000000, 0.000000000000000000 ) ) ;
#50729 = EDGE_CURVE ( 'NONE', #35322, #46560, #66134, .T. ) ;
#50730 = CARTESIAN_POINT ( 'NONE',  ( 10.58981376305288613, 0.000000000000000000, -9.535111140613709679 ) ) ;
#50731 = CARTESIAN_POINT ( 'NONE',  ( 19.84674366389459266, 23.71726448433412315, -2.638427012816827677 ) ) ;
#50732 = CARTESIAN_POINT ( 'NONE',  ( 6.565887622018943937, 25.16530133659708213, 12.81628187352647430 ) ) ;
#50733 = PLANE ( 'NONE',  #40386 ) ;
#50734 = EDGE_CURVE ( 'NONE', #77766, #50974, #58057, .T. ) ;
#50735 = EDGE_LOOP ( 'NONE', ( #70035, #69781, #50592, #60022 ) ) ;
#50736 = DIRECTION ( 'NONE',  ( -0.000000000000000000, -0.000000000000000000, -1.000000000000000000 ) ) ;
#50737 = CARTESIAN_POINT ( 'NONE',  ( 24.16423886937410614, 24.30374883491396787, 8.672049930838204340E-16 ) ) ;
#50738 = CARTESIAN_POINT ( 'NONE',  ( 17.20831665107776587, 39.13393115100079456, -7.208316651077762316 ) ) ;
#50739 = CARTESIAN_POINT ( 'NONE',  ( 16.40814093676323893, 45.79030133659708923, 11.09922568453595026 ) ) ;
#50741 = LINE ( 'NONE', #28223, #38521 ) ;
#50740 = CARTESIAN_POINT ( 'NONE',  ( -14.94699059465099822, 14.49999999999999822, -1.259949270175015013 ) ) ;
#50742 = CARTESIAN_POINT ( 'NONE',  ( 12.91533473730993009, 61.60535201082150536, -10.88017736071109987 ) ) ;
#50743 = CARTESIAN_POINT ( 'NONE',  ( -1.099225684535947600, 14.54030133659708568, 6.408140936763237150 ) ) ;
#50744 = DIRECTION ( 'NONE',  ( 0.000000000000000000, 0.000000000000000000, 1.000000000000000000 ) ) ;
#50745 = CARTESIAN_POINT ( 'NONE',  ( 1.472469842513823179, 40.59226448433411605, -4.923371831947296329 ) ) ;
#50746 = CARTESIAN_POINT ( 'NONE',  ( 15.44008868035555260, 34.73035201082151247, 9.422509992056143702 ) ) ;
#50747 = CARTESIAN_POINT ( 'NONE',  ( -2.816281873526473856, 44.12363466993042493, 9.499525473075851096E-16 ) ) ;
#50748 = CARTESIAN_POINT ( 'NONE',  ( 0.1532563361054083140, 31.00893115100078390, 1.131784320476157264E-15 ) ) ;
#50749 = DIRECTION ( 'NONE',  ( -0.7319527173941134945, -0.4481680578296335371, -0.5132159501034501137 ) ) ;
#50750 = CARTESIAN_POINT ( 'NONE',  ( 14.93928340878672500, 14.76930270348881180, 0.2363597353050709837 ) ) ;
#50751 = CARTESIAN_POINT ( 'NONE',  ( 19.42250999205614193, 35.14701867748816966, 5.440088680355555262 ) ) ;
#50752 = ORIENTED_EDGE ( 'NONE', *, *, #40035, .T. ) ;
#50753 = CYLINDRICAL_SURFACE ( 'NONE', #39391, 7.000000000000006217 ) ;
#50754 = CARTESIAN_POINT ( 'NONE',  ( 20.88017736071110875, 10.77201867748817143, -2.915334737309920765 ) ) ;
#50756 = CARTESIAN_POINT ( 'NONE',  ( 12.91533473730992121, 34.52201867748817676, 10.88017736071110164 ) ) ;
#50755 = CARTESIAN_POINT ( 'NONE',  ( 2.791683348922237240, 55.38393115100078745, -7.208316651077763204 ) ) ;
#50757 = LINE ( 'NONE', #26764, #21714 ) ;
#50758 = CARTESIAN_POINT ( 'NONE',  ( 0.5774900079438590739, 57.64701867748817676, -5.440088680355550821 ) ) ;
#50759 = CARTESIAN_POINT ( 'NONE',  ( 20.88017736071110519, 25.56368534415483751, 2.639326808657452039E-16 ) ) ;
#50760 = CARTESIAN_POINT ( 'NONE',  ( 14.92337183194729988, 24.34226448433411960, -8.527530157486177487 ) ) ;
#50761 = CARTESIAN_POINT ( 'NONE',  ( 0.000000000000000000, 15.00000000000000000, 0.000000000000000000 ) ) ;
#50762 = CARTESIAN_POINT ( 'NONE',  ( -14.16423886937410437, 1.595415501580629503, -3.795296366450299885 ) ) ;
#50763 = CARTESIAN_POINT ( 'NONE',  ( 14.92337183194729633, 52.67559781766745175, 8.527530157486181039 ) ) ;
#50765 = CARTESIAN_POINT ( 'NONE',  ( -11.75209714983983567, 0.04922511925149412187, 8.918201205061931702 ) ) ;
#50764 = CARTESIAN_POINT ( 'NONE',  ( -4.164238869374099927, 57.01208216824731068, 3.795296366450308767 ) ) ;
#50766 = CARTESIAN_POINT ( 'NONE',  ( 10.00000000000000178, 8.053748834913967869, 14.16423886937410082 ) ) ;
#50767 = CARTESIAN_POINT ( 'NONE',  ( 20.36894250292379382, 33.67874883491396076, 10.36894250292379205 ) ) ;
#50768 = AXIS2_PLACEMENT_3D ( 'NONE', #32697, #93699, #25234 ) ;
#50769 = CARTESIAN_POINT ( 'NONE',  ( 0.6178305044545838731, -0.2513653300695798953, 9.382169495545420901 ) ) ;
#50770 = ORIENTED_EDGE ( 'NONE', *, *, #16284, .T. ) ;
#50771 = CARTESIAN_POINT ( 'NONE',  ( 2.035157376598822676, 17.43868534415483751, -7.964842623401177768 ) ) ;
#50772 = CARTESIAN_POINT ( 'NONE',  ( 7.361572987183169658, 39.96726448433411605, -9.846743663894592657 ) ) ;
#50773 = CARTESIAN_POINT ( 'NONE',  ( -13.83909701985791152, 90.94176541299273708, -7.900788997805661573 ) ) ;
#50774 = CARTESIAN_POINT ( 'NONE',  ( 14.26139399674455710, 4.125707382711286748E-16, 2.619664342929903356 ) ) ;
#50775 = CARTESIAN_POINT ( 'NONE',  ( -11.48952521350009448, 15.00000000000000000, -8.845383562533896793 ) ) ;
#50776 = CARTESIAN_POINT ( 'NONE',  ( -1.099225684535947600, 23.70696800326375708, -6.408140936763238038 ) ) ;
#50777 = CARTESIAN_POINT ( 'NONE',  ( 2.791683348922240793, 26.63393115100078745, 7.208316651077764092 ) ) ;
#50778 = ORIENTED_EDGE ( 'NONE', *, *, #60374, .F. ) ;
#50779 = CARTESIAN_POINT ( 'NONE',  ( 17.20831665107776587, 4.133931151000785675, -7.208316651077762316 ) ) ;
#50780 = B_SPLINE_CURVE_WITH_KNOTS ( 'NONE', 3,
 ( #81845, #29335, #51854, #83339 ),
 .UNSPECIFIED., .F., .F.,
 ( 4, 4 ),
 ( 2.523187944655234921E-17, 0.002562518741975313395 ),
 .UNSPECIFIED. ) ;
#50781 = DIRECTION ( 'NONE',  ( -0.5519369853120501546, 0.000000000000000000, -0.8338858220671735433 ) ) ;
#50782 = CARTESIAN_POINT ( 'NONE',  ( 19.42250999205614193, 5.147018677488171434, 5.440088680355555262 ) ) ;
#50783 = CARTESIAN_POINT ( 'NONE',  ( 0.5774900079438590739, 17.64701867748817321, -5.440088680355550821 ) ) ;
#50784 = CARTESIAN_POINT ( 'NONE',  ( -2.266590686148945544, 37.22041550158063217, 7.082119434687048631 ) ) ;
#50785 = CARTESIAN_POINT ( 'NONE',  ( 4.559911319644449179, 27.23035201082150536, -9.422509992056141925 ) ) ;
#50786 = VECTOR ( 'NONE', #44078, 1000.000000000000114 ) ;
#50787 = CARTESIAN_POINT ( 'NONE',  ( 19.42250999205614193, 65.14701867748817676, 5.440088680355555262 ) ) ;
#50788 = DIRECTION ( 'NONE',  ( -0.000000000000000000, -1.000000000000000000, -0.000000000000000000 ) ) ;
#50789 = CARTESIAN_POINT ( 'NONE',  ( 14.19749592853504438, -0.03417435944610275333, -7.369430493279943484 ) ) ;
#50790 = CARTESIAN_POINT ( 'NONE',  ( 12.63842701281683034, 17.46726448433411250, 9.846743663894596210 ) ) ;
#50791 = CARTESIAN_POINT ( 'NONE',  ( 17.20831665107776587, 4.133931151000785675, -7.208316651077762316 ) ) ;
#50792 = CARTESIAN_POINT ( 'NONE',  ( -11.48952521350030587, 15.00000000000000000, 8.845383562533664090 ) ) ;
#50793 = CARTESIAN_POINT ( 'NONE',  ( 7.361572987183170547, 42.05059781766745886, 9.846743663894590881 ) ) ;
#50794 = CARTESIAN_POINT ( 'NONE',  ( 14.92337183194729633, 62.67559781766745886, 8.527530157486181039 ) ) ;
#50795 = EDGE_CURVE ( 'NONE', #88686, #10324, #58643, .T. ) ;
#50796 = CARTESIAN_POINT ( 'NONE',  ( -0.8801773607111008646, 38.27201867748816255, 2.915334737309923430 ) ) ;
#50797 = VECTOR ( 'NONE', #2609, 1000.000000000000114 ) ;
#50798 = CIRCLE ( 'NONE', #25276, 15.00000000000000000 ) ;
#50799 = ORIENTED_EDGE ( 'NONE', *, *, #94629, .F. ) ;
#50800 = CARTESIAN_POINT ( 'NONE',  ( 16.40814093676324603, 47.45696800326375353, -11.09922568453594671 ) ) ;
#50801 = DIRECTION ( 'NONE',  ( -1.000000000000000000, 1.257568779154408793E-17, 0.000000000000000000 ) ) ;
#50802 = CARTESIAN_POINT ( 'NONE',  ( 7.084665262690076126, 62.02201867748816966, -10.88017736071110164 ) ) ;
#50803 = CARTESIAN_POINT ( 'NONE',  ( -2.816281873526473856, 44.33196800326375353, 3.434112377981055619 ) ) ;
#50805 = CARTESIAN_POINT ( 'NONE',  ( 0.1532563361054082862, 36.21726448433410894, 2.638427012816831674 ) ) ;
#50804 = CARTESIAN_POINT ( 'NONE',  ( 17.08211943468705130, 58.47041550158063927, 12.26659068614894998 ) ) ;
#50806 = CARTESIAN_POINT ( 'NONE',  ( 19.72487221294571569, 20.71833443783938122, -6.499999999999990230 ) ) ;
#50807 = CARTESIAN_POINT ( 'NONE',  ( 14.92337183194729988, 64.34226448433412315, -8.527530157486177487 ) ) ;
#50808 = CARTESIAN_POINT ( 'NONE',  ( 6.204703633549690345, 25.76208216824730712, -14.16423886937410259 ) ) ;
#50809 = CARTESIAN_POINT ( 'NONE',  ( 17.20831665107776587, 44.13393115100078745, -7.208316651077762316 ) ) ;
#50810 = CARTESIAN_POINT ( 'NONE',  ( -8.564643372776465924, 14.49999999999999112, -12.31449893000758955 ) ) ;
#50811 = CARTESIAN_POINT ( 'NONE',  ( 10.00000000000000000, 31.81368534415483751, -10.88017736071110342 ) ) ;
#50812 = CARTESIAN_POINT ( 'NONE',  ( 0.5774900079438590739, 52.64701867748817676, -5.440088680355550821 ) ) ;
#50813 = VERTEX_POINT ( 'NONE', #13139 ) ;
#50814 = CARTESIAN_POINT ( 'NONE',  ( -1.099225684535947600, 43.70696800326375353, -6.408140936763238038 ) ) ;
#50815 = ORIENTED_EDGE ( 'NONE', *, *, #82984, .F. ) ;
#50816 = CARTESIAN_POINT ( 'NONE',  ( 19.84674366389459266, 3.300597817667451750, 2.638427012816836559 ) ) ;
#50817 = ORIENTED_EDGE ( 'NONE', *, *, #79658, .T. ) ;
#50818 = CARTESIAN_POINT ( 'NONE',  ( 17.08211943468705840, 5.137082168247300906, -12.26659068614894466 ) ) ;
#50819 = CARTESIAN_POINT ( 'NONE',  ( 10.00000000000000178, 2.258931151000784787, 9.846743663894594434 ) ) ;
#50820 = CARTESIAN_POINT ( 'NONE',  ( 2.599899806584774264, 0.4361964623231012195, -6.495912400107028084 ) ) ;
#50821 = ORIENTED_EDGE ( 'NONE', *, *, #84582, .F. ) ;
#50822 = FACE_OUTER_BOUND ( 'NONE', #84765, .T. ) ;
#50823 = CARTESIAN_POINT ( 'NONE',  ( 12.91533473730993009, 11.60535201082150536, -10.88017736071109987 ) ) ;
#50824 = ADVANCED_FACE ( 'NONE', ( #12158 ), #69538, .T. ) ;
#50825 = DIRECTION ( 'NONE',  ( -1.000000000000000000, -0.000000000000000000, -0.000000000000000000 ) ) ;
#50826 = CARTESIAN_POINT ( 'NONE',  ( 10.00000000000000000, 20.55374883491396787, -14.16423886937410082 ) ) ;
#50827 = ADVANCED_FACE ( 'NONE', ( #73139 ), #95158, .F. ) ;
#50828 = CARTESIAN_POINT ( 'NONE',  ( 20.88017736071110164, 25.35535201082150891, 2.915334737309930979 ) ) ;
#50829 = CARTESIAN_POINT ( 'NONE',  ( 19.84674366389459266, 53.30059781766744464, 2.638427012816836559 ) ) ;
#50830 = ORIENTED_EDGE ( 'NONE', *, *, #43941, .F. ) ;
#50831 = CARTESIAN_POINT ( 'NONE',  ( 0.1532563361054082862, 61.21726448433412315, 2.638427012816831674 ) ) ;
#50832 = EDGE_LOOP ( 'NONE', ( #44286, #71241, #13563, #81684, #97679 ) ) ;
#50833 = CARTESIAN_POINT ( 'NONE',  ( 19.42250999205614193, 60.14701867748817676, 5.440088680355555262 ) ) ;
#50834 = CARTESIAN_POINT ( 'NONE',  ( 1.472469842513823179, 66.42559781766745175, 4.923371831947296329 ) ) ;
#50835 = CARTESIAN_POINT ( 'NONE',  ( 0.6178305044545838731, 34.74863466993042493, 9.382169495545420901 ) ) ;
#50837 = DIRECTION ( 'NONE',  ( 0.9862856015372297724, 0.000000000000000000, 0.1650476058606878682 ) ) ;
#50836 = CARTESIAN_POINT ( 'NONE',  ( 15.44008868035555260, 4.730352010821504471, 9.422509992056143702 ) ) ;
#50838 = CARTESIAN_POINT ( 'NONE',  ( 10.00000000000000000, 4.758931151000784787, -9.846743663894594434 ) ) ;
#50839 = CARTESIAN_POINT ( 'NONE',  ( 15.44008868035555793, 21.39701867748817321, -9.422509992056140149 ) ) ;
#50840 = ORIENTED_EDGE ( 'NONE', *, *, #71792, .T. ) ;
#50841 = CARTESIAN_POINT ( 'NONE',  ( 13.43411237798106583, 57.66530133659708923, -12.81628187352647252 ) ) ;
#50842 = CARTESIAN_POINT ( 'NONE',  ( 15.44008868035555260, 24.73035201082150891, 9.422509992056143702 ) ) ;
#50843 = DIRECTION ( 'NONE',  ( -0.000000000000000000, 1.000000000000000000, 0.000000000000000000 ) ) ;
#50844 = CARTESIAN_POINT ( 'NONE',  ( 21.09922568453594849, 46.20696800326376064, 6.408140936763242479 ) ) ;
#50845 = CARTESIAN_POINT ( 'NONE',  ( 20.88017736071110875, 45.77201867748816966, -2.915334737309920765 ) ) ;
#50846 = CARTESIAN_POINT ( 'NONE',  ( 1.472469842513823179, 55.59226448433412315, -4.923371831947296329 ) ) ;
#50847 = ORIENTED_EDGE ( 'NONE', *, *, #17533, .F. ) ;
#50848 = AXIS2_PLACEMENT_3D ( 'NONE', #25435, #40921, #40430 ) ;
#50849 = CARTESIAN_POINT ( 'NONE',  ( 0.1532563361054100626, 20.80059781766744464, -2.638427012816831230 ) ) ;
#50850 = CARTESIAN_POINT ( 'NONE',  ( 3.591859063236761518, -0.04303199673624671928, 11.09922568453594849 ) ) ;
#50852 = CARTESIAN_POINT ( 'NONE',  ( -6.898461952320517732, 15.00000000000000000, 12.75387089053304557 ) ) ;
#50851 = LINE ( 'NONE', #42371, #50008 ) ;
#50853 = CARTESIAN_POINT ( 'NONE',  ( -0.8801773607111008646, 18.27201867748817321, 2.915334737309923430 ) ) ;
#50854 = CARTESIAN_POINT ( 'NONE',  ( 17.20831665107776587, 54.13393115100079456, -7.208316651077762316 ) ) ;
#50855 = FACE_OUTER_BOUND ( 'NONE', #54976, .T. ) ;
#50856 = ADVANCED_FACE ( 'NONE', ( #80160, #24377 ), #9861, .F. ) ;
#50857 = CARTESIAN_POINT ( 'NONE',  ( 7.361572987183169658, 9.967264484334119601, -9.846743663894592657 ) ) ;
#50859 = ORIENTED_EDGE ( 'NONE', *, *, #80288, .F. ) ;
#50858 = CARTESIAN_POINT ( 'NONE',  ( 19.38216949554541202, 0.9986346699304200492, 9.382169495545424454 ) ) ;
#50860 = AXIS2_PLACEMENT_3D ( 'NONE', #54990, #54500, #16529 ) ;
#50861 = CARTESIAN_POINT ( 'NONE',  ( 9.323033696084937816, 14.95037104545395046, 11.43408728005520203 ) ) ;
#50862 = CARTESIAN_POINT ( 'NONE',  ( 6.879999999999995453, 43.00000000000000000, 6.250000000000000000 ) ) ;
#50863 = CARTESIAN_POINT ( 'NONE',  ( 19.38216949554541557, 37.24863466993041783, -9.382169495545420901 ) ) ;
#50864 = CARTESIAN_POINT ( 'NONE',  ( 12.63842701281683034, 37.46726448433411605, 9.846743663894596210 ) ) ;
#50865 = CARTESIAN_POINT ( 'NONE',  ( 14.82269085861168811, 0.5000000000000004441, -2.299529454046961519 ) ) ;
#50866 = CARTESIAN_POINT ( 'NONE',  ( -0.3689425029237881626, 62.42874883491396787, 10.36894250292379027 ) ) ;
#50867 = CARTESIAN_POINT ( 'NONE',  ( 18.52753015748618282, 28.92559781766745175, -4.923371831947291888 ) ) ;
#50868 = CARTESIAN_POINT ( 'NONE',  ( -0.2418659066527655277, 39.26028685723174050, -6.114288769123055189 ) ) ;
#50869 = CARTESIAN_POINT ( 'NONE',  ( 13.79529636645030344, 53.26208216824730357, 14.16423886937410614 ) ) ;
#50870 = CARTESIAN_POINT ( 'NONE',  ( -7.754989057094395122, 84.52548903604052555, -4.000000000000000000 ) ) ;
#50871 = CARTESIAN_POINT ( 'NONE',  ( 15.44008868035555260, 24.73035201082150891, 9.422509992056143702 ) ) ;
#50872 = CARTESIAN_POINT ( 'NONE',  ( -0.3689425029237881626, 42.42874883491396787, 10.36894250292379027 ) ) ;
#50873 = CARTESIAN_POINT ( 'NONE',  ( 20.36894250292379382, 58.67874883491396076, 10.36894250292379205 ) ) ;
#50874 = CYLINDRICAL_SURFACE ( 'NONE', #8469, 0.5000000000000004441 ) ;
#50875 = CARTESIAN_POINT ( 'NONE',  ( 18.52753015748617571, 8.092264484334117824, 4.923371831947298993 ) ) ;
#50876 = CARTESIAN_POINT ( 'NONE',  ( 3.591859063236763294, -1.709698663402913210, -11.09922568453595026 ) ) ;
#50877 = CARTESIAN_POINT ( 'NONE',  ( 17.84635730667655906, 13.63791097397318985, 6.500000000000019540 ) ) ;
#50878 = VERTEX_POINT ( 'NONE', #92849 ) ;
#50879 = CARTESIAN_POINT ( 'NONE',  ( 20.88017736071110875, 50.77201867748817676, -2.915334737309920765 ) ) ;
#50880 = CARTESIAN_POINT ( 'NONE',  ( 14.29730467489533652, 3.971653163193037558E-16, -2.416004766803220516 ) ) ;
#50881 = CARTESIAN_POINT ( 'NONE',  ( 0.1532563361054083140, 51.00893115100078745, 1.131784320476157264E-15 ) ) ;
#50882 = CARTESIAN_POINT ( 'NONE',  ( -3.749999999999999112, 78.07179676972445748, -4.250000000000000000 ) ) ;
#50883 = CARTESIAN_POINT ( 'NONE',  ( 3.969999999999999751, 36.75000000000000000, -2.750000000000000000 ) ) ;
#50884 = ORIENTED_EDGE ( 'NONE', *, *, #34358, .T. ) ;
#50885 = CARTESIAN_POINT ( 'NONE',  ( -4.164238869374099927, 47.01208216824729647, 3.795296366450308767 ) ) ;
#50887 = LINE ( 'NONE', #35879, #808 ) ;
#50886 = DIRECTION ( 'NONE',  ( 0.000000000000000000, 0.000000000000000000, 1.000000000000000000 ) ) ;
#50888 = CARTESIAN_POINT ( 'NONE',  ( 7.084665262690076126, 17.02201867748817676, -10.88017736071110164 ) ) ;
#50889 = CARTESIAN_POINT ( 'NONE',  ( -1.099225684535947600, 44.54030133659708923, 6.408140936763237150 ) ) ;
#50890 = CARTESIAN_POINT ( 'NONE',  ( -3.195792623639522212, 10.72997603579417536, 11.92686044187656691 ) ) ;
#50891 = CARTESIAN_POINT ( 'NONE',  ( -2.816281873526473856, 19.12363466993042138, 9.499525473075851096E-16 ) ) ;
#50892 = DIRECTION ( 'NONE',  ( 0.000000000000000000, 0.000000000000000000, 1.000000000000000000 ) ) ;
#50893 = ORIENTED_EDGE ( 'NONE', *, *, #14032, .T. ) ;
#50894 = CARTESIAN_POINT ( 'NONE',  ( -10.60841941975015601, -98.07601481626471696, -4.000000000000000000 ) ) ;
#50895 = CARTESIAN_POINT ( 'NONE',  ( -0.3689425029237881626, 27.42874883491397142, 10.36894250292379027 ) ) ;
#50896 = CARTESIAN_POINT ( 'NONE',  ( 6.204703633549690345, 0.7620821682473009062, -14.16423886937410259 ) ) ;
#50897 = CARTESIAN_POINT ( 'NONE',  ( -3.772056942336352581, -0.8420495280537244609, 4.000000000000000000 ) ) ;
#50898 = CARTESIAN_POINT ( 'NONE',  ( 7.084665262690076126, 22.02201867748817321, -10.88017736071110164 ) ) ;
#50899 = PLANE ( 'NONE',  #11119 ) ;
#50900 = DIRECTION ( 'NONE',  ( 0.000000000000000000, -1.000000000000000000, 0.000000000000000000 ) ) ;
#50901 = CARTESIAN_POINT ( 'NONE',  ( 4.559911319644449179, 47.23035201082150536, -9.422509992056141925 ) ) ;
#50902 = CARTESIAN_POINT ( 'NONE',  ( 12.91533473730992121, 54.52201867748816255, 10.88017736071110164 ) ) ;
#50903 = CARTESIAN_POINT ( 'NONE',  ( 3.591859063236763294, 8.290301336597087456, -11.09922568453595026 ) ) ;
#50904 = CARTESIAN_POINT ( 'NONE',  ( 14.88232117145530786, 14.49999999999999822, -1.875237731503139438 ) ) ;
#50905 = CARTESIAN_POINT ( 'NONE',  ( 1.274849032794102888, 3.572280503510291361, 6.499999999999721112 ) ) ;
#50906 = CARTESIAN_POINT ( 'NONE',  ( 18.52753015748617571, 18.09226448433411960, 4.923371831947298993 ) ) ;
#50907 = CARTESIAN_POINT ( 'NONE',  ( 15.44008868035555260, 39.73035201082150536, 9.422509992056143702 ) ) ;
#50908 = ADVANCED_FACE ( 'NONE', ( #55850 ), #24866, .F. ) ;
#50909 = CARTESIAN_POINT ( 'NONE',  ( 19.38216949554541557, 2.248634669930420049, -9.382169495545420901 ) ) ;
#50910 = CARTESIAN_POINT ( 'NONE',  ( 0.1532563361054082862, 1.217264484334117824, 2.638427012816831674 ) ) ;
#50911 = CARTESIAN_POINT ( 'NONE',  ( 5.076628168052704559, 20.17559781766745175, -8.527530157486179263 ) ) ;
#50912 = CARTESIAN_POINT ( 'NONE',  ( -2.816281873526471635, 53.91530133659709634, -3.434112377981056508 ) ) ;
#50913 = CARTESIAN_POINT ( 'NONE',  ( 2.791683348922240793, 6.633931151000785675, 7.208316651077764092 ) ) ;
#50914 = ORIENTED_EDGE ( 'NONE', *, *, #40282, .T. ) ;
#50915 = DIRECTION ( 'NONE',  ( 0.000000000000000000, 0.000000000000000000, 1.000000000000000000 ) ) ;
#50916 = DIRECTION ( 'NONE',  ( 1.000000000000000000, -0.000000000000000000, -0.000000000000000000 ) ) ;
#50917 = CARTESIAN_POINT ( 'NONE',  ( 20.88017736071110519, 20.56368534415484106, 2.639326808657452039E-16 ) ) ;
#50919 = CARTESIAN_POINT ( 'NONE',  ( 6.204703633549690345, 30.76208216824730357, -14.16423886937410259 ) ) ;
#50918 = PLANE ( 'NONE',  #83972 ) ;
#50920 = CARTESIAN_POINT ( 'NONE',  ( 0.1532563361054100626, 30.80059781766744820, -2.638427012816831230 ) ) ;
#50921 = MECHANICAL_DESIGN_GEOMETRIC_PRESENTATION_REPRESENTATION (  '', ( #14244 ), #20598 ) ;
#50922 = CARTESIAN_POINT ( 'NONE',  ( 17.96484262340118221, 21.18868534415483396, -7.964842623401177768 ) ) ;
#50923 = CARTESIAN_POINT ( 'NONE',  ( 0.5774900079438607392, 8.480352010821505360, 5.440088680355550821 ) ) ;
#50924 = EDGE_LOOP ( 'NONE', ( #21307, #88524, #88966, #8883, #86248, #69040 ) ) ;
#50925 = CARTESIAN_POINT ( 'NONE',  ( -0.8801773607110991993, 32.85535201082151247, -2.915334737309923874 ) ) ;
#50926 = AXIS2_PLACEMENT_3D ( 'NONE', #46157, #5333, #60157 ) ;
#50927 = CARTESIAN_POINT ( 'NONE',  ( 17.96484262340118221, 41.18868534415484106, -7.964842623401177768 ) ) ;
#50929 = CARTESIAN_POINT ( 'NONE',  ( 2.035157376598824452, 43.68868534415484106, 7.964842623401179544 ) ) ;
#50928 = FACE_OUTER_BOUND ( 'NONE', #46649, .T. ) ;
#50930 = AXIS2_PLACEMENT_3D ( 'NONE', #82419, #81925, #35441 ) ;
#50931 = ORIENTED_EDGE ( 'NONE', *, *, #71792, .F. ) ;
#50932 = CARTESIAN_POINT ( 'NONE',  ( 19.84674366389459621, 63.50893115100078745, 7.409399052514197653E-17 ) ) ;
#50933 = CARTESIAN_POINT ( 'NONE',  ( 17.96484262340118221, 39.93868534415484106, 7.964842623401181321 ) ) ;
#50934 = DIRECTION ( 'NONE',  ( -1.257568779154408793E-17, -1.000000000000000000, 0.000000000000000000 ) ) ;
#50935 = EDGE_CURVE ( 'NONE', #31636, #81215, #87805, .T. ) ;
#50936 = CARTESIAN_POINT ( 'NONE',  ( -2.816281873526473856, 64.33196800326376774, 3.434112377981055619 ) ) ;
#50937 = LINE ( 'NONE', #51431, #4534 ) ;
#50938 = CARTESIAN_POINT ( 'NONE',  ( 10.00000000000000000, 35.55374883491396787, -14.16423886937410082 ) ) ;
#50939 = CARTESIAN_POINT ( 'NONE',  ( 7.084665262690076126, 47.02201867748818387, -10.88017736071110164 ) ) ;
#50940 = CARTESIAN_POINT ( 'NONE',  ( 10.00000000000000178, 67.25893115100079456, 9.846743663894594434 ) ) ;
#50941 = DIRECTION ( 'NONE',  ( -0.000000000000000000, 1.000000000000000000, -0.000000000000000000 ) ) ;
#50942 = CARTESIAN_POINT ( 'NONE',  ( 5.076628168052703671, 46.84226448433412315, 8.527530157486179263 ) ) ;
#50943 = EDGE_CURVE ( 'NONE', #14583, #31163, #53604, .T. ) ;
#50944 = VERTEX_POINT ( 'NONE', #47343 ) ;
#50945 = CARTESIAN_POINT ( 'NONE',  ( -9.399392868737642459, 15.00000000000000000, -11.04089732309485861 ) ) ;
#50946 = CARTESIAN_POINT ( 'NONE',  ( 7.361572987183170547, 17.05059781766745530, 9.846743663894590881 ) ) ;
#50947 = CARTESIAN_POINT ( 'NONE',  ( 12.81628187352647252, -13.16803199673624825, -3.434112377981059172 ) ) ;
#50948 = CARTESIAN_POINT ( 'NONE',  ( 2.035157376598824452, 8.688685344154839285, 7.964842623401179544 ) ) ;
#50949 = CARTESIAN_POINT ( 'NONE',  ( 0.1532563361054083140, 31.00893115100078390, 1.131784320476157264E-15 ) ) ;
#50950 = CARTESIAN_POINT ( 'NONE',  ( 19.38216949554541202, 10.99863466993042138, 9.382169495545424454 ) ) ;
#50951 = CARTESIAN_POINT ( 'NONE',  ( -0.8801773607111009756, 58.06368534415484106, 1.068504757029289695E-15 ) ) ;
#50953 = CARTESIAN_POINT ( 'NONE',  ( -1.099225684535947600, 58.70696800326375353, -6.408140936763238038 ) ) ;
#50952 = CARTESIAN_POINT ( 'NONE',  ( 0.5774900079438590739, 32.64701867748816966, -5.440088680355550821 ) ) ;
#50954 = CARTESIAN_POINT ( 'NONE',  ( 13.79529636645030344, 43.26208216824730357, 14.16423886937410614 ) ) ;
#50955 = CARTESIAN_POINT ( 'NONE',  ( -13.07661834287492120, -3.167479706257454935E-15, 6.550615570651588726 ) ) ;
#50956 = ORIENTED_EDGE ( 'NONE', *, *, #17779, .T. ) ;
#50957 = CARTESIAN_POINT ( 'NONE',  ( 22.81628187352647785, 1.623634669930420271, 6.195893100308588602E-16 ) ) ;
#50958 = CARTESIAN_POINT ( 'NONE',  ( 2.035157376598824452, 3.688685344154837953, 7.964842623401179544 ) ) ;
#50959 = CARTESIAN_POINT ( 'NONE',  ( 20.88017736071110875, 40.77201867748818387, -2.915334737309920765 ) ) ;
#50960 = CARTESIAN_POINT ( 'NONE',  ( 10.00000000000000178, 62.25893115100078745, 9.846743663894594434 ) ) ;
#50961 = B_SPLINE_CURVE_WITH_KNOTS ( 'NONE', 3,
 ( #82963, #45957, #89477, #7961, #29448, #37975, #14482, #66974, #44952, #13482 ),
 .UNSPECIFIED., .F., .F.,
 ( 4, 3, 3, 4 ),
 ( 7.573910767901059648E-18, 0.0006253016069560859589, 0.001250604074564941890, 0.002501455912506543935 ),
 .UNSPECIFIED. ) ;
#50962 = ORIENTED_EDGE ( 'NONE', *, *, #40419, .F. ) ;
#50963 = CARTESIAN_POINT ( 'NONE',  ( 0.1532563361054100626, 15.80059781766745353, -2.638427012816831230 ) ) ;
#50964 = CARTESIAN_POINT ( 'NONE',  ( 19.84674366389459621, 13.50893115100078568, 7.409399052514197653E-17 ) ) ;
#50965 = CARTESIAN_POINT ( 'NONE',  ( 1.472469842513823179, 26.42559781766745175, 4.923371831947296329 ) ) ;
#50966 = CARTESIAN_POINT ( 'NONE',  ( 12.63842701281683922, 14.55059781766744997, -9.846743663894590881 ) ) ;
#50967 =( NAMED_UNIT ( * ) PLANE_ANGLE_UNIT ( ) SI_UNIT ( $, .RADIAN. ) );
#50968 = CARTESIAN_POINT ( 'NONE',  ( -7.072497013479695838, -84.40007040885043921, 2.500000000001209255 ) ) ;
#50969 = ADVANCED_FACE ( 'NONE', ( #25364 ), #55349, .F. ) ;
#50971 = CYLINDRICAL_SURFACE ( 'NONE', #41987, 2.000000000000000000 ) ;
#50970 = CARTESIAN_POINT ( 'NONE',  ( 10.00000000000000178, 7.258931151000785675, 9.846743663894594434 ) ) ;
#50972 = CARTESIAN_POINT ( 'NONE',  ( 10.00000000000000000, 9.758931151000785675, -9.846743663894594434 ) ) ;
#50974 = VERTEX_POINT ( 'NONE', #40360 ) ;
#50973 = CARTESIAN_POINT ( 'NONE',  ( 0.1532563361054082862, 21.21726448433412315, 2.638427012816831674 ) ) ;
#50975 = CARTESIAN_POINT ( 'NONE',  ( 0.2078314800211761848, 0.04962894115304285203, 14.75174957775520213 ) ) ;
#50976 = CARTESIAN_POINT ( 'NONE',  ( 12.63842701281683922, 64.55059781766745175, -9.846743663894590881 ) ) ;
#50977 = ORIENTED_EDGE ( 'NONE', *, *, #5834, .F. ) ;
#50978 = CARTESIAN_POINT ( 'NONE',  ( 6.204703633549690345, 17.84541550158063217, 14.16423886937410082 ) ) ;
#50979 = CARTESIAN_POINT ( 'NONE',  ( 2.913501739333762774, 15.00000000000000000, -14.20427779279532565 ) ) ;
#50980 = CARTESIAN_POINT ( 'NONE',  ( -4.164238869374099039, 16.80374883491396787, 8.674139862899312516E-16 ) ) ;
#50981 = EDGE_CURVE ( 'NONE', #765, #61749, #23889, .T. ) ;
#50982 = CARTESIAN_POINT ( 'NONE',  ( -0.3689425029237881626, 47.42874883491396787, 10.36894250292379027 ) ) ;
#50983 = DIRECTION ( 'NONE',  ( 0.000000000000000000, 1.000000000000000000, 0.000000000000000000 ) ) ;
#50985 = CARTESIAN_POINT ( 'NONE',  ( 20.88017736071110164, 65.35535201082150536, 2.915334737309930979 ) ) ;
#50984 = CARTESIAN_POINT ( 'NONE',  ( 22.26659068614895176, 14.72041550158063572, -7.082119434687042414 ) ) ;
#50986 = CARTESIAN_POINT ( 'NONE',  ( 12.91533473730993009, 36.60535201082151247, -10.88017736071109987 ) ) ;
#50987 = DIRECTION ( 'NONE',  ( -0.000000000000000000, 0.000000000000000000, 1.000000000000000000 ) ) ;
#50988 = CARTESIAN_POINT ( 'NONE',  ( 0.1532563361054082862, 26.21726448433411605, 2.638427012816831674 ) ) ;
#50990 = CARTESIAN_POINT ( 'NONE',  ( 1.472469842513823179, 35.59226448433412315, -4.923371831947296329 ) ) ;
#50989 = CARTESIAN_POINT ( 'NONE',  ( 17.96484262340118221, 51.18868534415483396, -7.964842623401177768 ) ) ;
#50991 = CARTESIAN_POINT ( 'NONE',  ( 20.88017736071110875, 10.77201867748817143, -2.915334737309920765 ) ) ;
#50992 = CARTESIAN_POINT ( 'NONE',  ( 16.40814093676323893, 55.79030133659708923, 11.09922568453595026 ) ) ;
#50993 = CARTESIAN_POINT ( 'NONE',  ( 10.00000000000000178, 57.25893115100078745, 9.846743663894594434 ) ) ;
#50994 = DIRECTION ( 'NONE',  ( 0.000000000000000000, 1.000000000000000000, 0.000000000000000000 ) ) ;
#50995 = CARTESIAN_POINT ( 'NONE',  ( 13.43411237798105340, 40.58196800326375353, 12.81628187352647963 ) ) ;
#50996 = CARTESIAN_POINT ( 'NONE',  ( -3.795296366450300773, -22.15458449841936073, 14.16423886937410437 ) ) ;
#50997 = CARTESIAN_POINT ( 'NONE',  ( -0.8801773607111009756, 48.06368534415484817, 1.068504757029289695E-15 ) ) ;
#50998 = CARTESIAN_POINT ( 'NONE',  ( 12.63842701281683922, 39.55059781766744464, -9.846743663894590881 ) ) ;
#50999 = CARTESIAN_POINT ( 'NONE',  ( 10.00000000000000178, 33.05374883491396787, 14.16423886937410082 ) ) ;
#51000 = VERTEX_POINT ( 'NONE', #86345 ) ;
#51001 = CARTESIAN_POINT ( 'NONE',  ( 10.00000000000000000, 0.5537488349139675359, -14.16423886937410082 ) ) ;
#51002 = CARTESIAN_POINT ( 'NONE',  ( 19.42250999205614548, 55.98035201082150536, -5.440088680355545492 ) ) ;
#51003 = CARTESIAN_POINT ( 'NONE',  ( 4.559911319644449179, 68.89701867748817676, 9.422509992056141925 ) ) ;
#51004 = CARTESIAN_POINT ( 'NONE',  ( -4.164238869374099927, 52.01208216824729647, 3.795296366450308767 ) ) ;
#51005 = CARTESIAN_POINT ( 'NONE',  ( 13.43411237798105340, 0.5819680032637533085, 12.81628187352647963 ) ) ;
#51006 = CARTESIAN_POINT ( 'NONE',  ( 19.38216949554541202, 60.99863466993042493, 9.382169495545424454 ) ) ;
#51007 = CARTESIAN_POINT ( 'NONE',  ( 7.084665262690076126, 44.10535201082151247, 10.88017736071109987 ) ) ;
#51008 = CARTESIAN_POINT ( 'NONE',  ( -3.271887613349915735, -0.8417457659429951056, -2.500000000000000444 ) ) ;
#51009 = VECTOR ( 'NONE', #8649, 1000.000000000000000 ) ;
#51010 = CARTESIAN_POINT ( 'NONE',  ( -2.816281873526471635, 23.91530133659708568, -3.434112377981056508 ) ) ;
#51011 = CARTESIAN_POINT ( 'NONE',  ( 5.076628168052703671, 51.84226448433412315, 8.527530157486179263 ) ) ;
#51012 = CARTESIAN_POINT ( 'NONE',  ( -9.422509992056145478, 17.64701867748817676, -5.440088680355541939 ) ) ;
#51013 = CARTESIAN_POINT ( 'NONE',  ( 10.00000000000000000, 1.813685344154837731, -10.88017736071110342 ) ) ;
#51014 = CARTESIAN_POINT ( 'NONE',  ( 0.5774900079438590739, 17.64701867748817321, -5.440088680355550821 ) ) ;
#51015 = DIRECTION ( 'NONE',  ( 1.000000000000000000, -3.469446951953623261E-15, 0.000000000000000000 ) ) ;
#51016 = ORIENTED_EDGE ( 'NONE', *, *, #74405, .F. ) ;
#51017 = CARTESIAN_POINT ( 'NONE',  ( 2.035157376598822676, 7.438685344154837509, -7.964842623401177768 ) ) ;
#51018 = EDGE_CURVE ( 'NONE', #91827, #3599, #93838, .T. ) ;
#51019 = DIRECTION ( 'NONE',  ( 0.000000000000000000, 0.000000000000000000, 1.000000000000000000 ) ) ;
#51020 = CARTESIAN_POINT ( 'NONE',  ( 10.00000000000000000, 66.81368534415484817, -10.88017736071110342 ) ) ;
#51021 = CARTESIAN_POINT ( 'NONE',  ( 1.472469842513823179, 0.5922644843341181575, -4.923371831947296329 ) ) ;
#51022 = CARTESIAN_POINT ( 'NONE',  ( 1.472469842513823179, 36.42559781766745175, 4.923371831947296329 ) ) ;
#51023 = EDGE_CURVE ( 'NONE', #1044, #42348, #1391, .T. ) ;
#51024 = CARTESIAN_POINT ( 'NONE',  ( 2.035157376598822676, 27.43868534415483396, -7.964842623401177768 ) ) ;
#51025 = CARTESIAN_POINT ( 'NONE',  ( 6.565887622018943937, 5.165301336597086568, 12.81628187352647430 ) ) ;
#51027 = DIRECTION ( 'NONE',  ( 0.000000000000000000, 0.000000000000000000, -1.000000000000000000 ) ) ;
#51026 = CARTESIAN_POINT ( 'NONE',  ( 0.5774900079438590739, 32.64701867748816966, -5.440088680355550821 ) ) ;
#51028 = SURFACE_STYLE_FILL_AREA ( #35533 ) ;
#51029 = CARTESIAN_POINT ( 'NONE',  ( 6.565887622018943937, 38.08196800326376064, -12.81628187352647608 ) ) ;
#51030 = ORIENTED_EDGE ( 'NONE', *, *, #83876, .T. ) ;
#51031 = CARTESIAN_POINT ( 'NONE',  ( 20.88017736071110164, 65.35535201082150536, 2.915334737309930979 ) ) ;
#51033 = CARTESIAN_POINT ( 'NONE',  ( 22.26659068614894466, 3.887082168247300906, 7.082119434687054849 ) ) ;
#51032 = CARTESIAN_POINT ( 'NONE',  ( 0.6178305044545818747, 28.49863466993041783, -9.382169495545419124 ) ) ;
#51034 = CARTESIAN_POINT ( 'NONE',  ( 21.92686044187657046, 32.39664270246083788, -3.195792623639524432 ) ) ;
#51035 = CARTESIAN_POINT ( 'NONE',  ( 0.5774900079438590739, 37.64701867748817676, -5.440088680355550821 ) ) ;
#51036 = CARTESIAN_POINT ( 'NONE',  ( 1.472469842513823179, 65.59226448433412315, -4.923371831947296329 ) ) ;
#51037 = CARTESIAN_POINT ( 'NONE',  ( 10.00000000000000000, 1.813685344154838175, -10.88017736071110342 ) ) ;
#51038 = CARTESIAN_POINT ( 'NONE',  ( 14.92337183194729633, 52.67559781766745175, 8.527530157486181039 ) ) ;
#51039 = CARTESIAN_POINT ( 'NONE',  ( 18.52753015748617571, 8.092264484334117824, 4.923371831947298993 ) ) ;
#51040 = CARTESIAN_POINT ( 'NONE',  ( -0.8801773607111009756, 68.06368534415484817, 1.068504757029289695E-15 ) ) ;
#51041 = DIRECTION ( 'NONE',  ( 0.000000000000000000, 0.000000000000000000, -1.000000000000000000 ) ) ;
#51042 = CARTESIAN_POINT ( 'NONE',  ( 22.26659068614894466, 28.88708216824730357, 7.082119434687054849 ) ) ;
#51043 = ADVANCED_FACE ( 'NONE', ( #78837 ), #16869, .F. ) ;
#51044 = CIRCLE ( 'NONE', #44621, 0.5000000000000004441 ) ;
#51045 = FILL_AREA_STYLE_COLOUR ( '', #2557 ) ;
#51046 = VERTEX_POINT ( 'NONE', #84866 ) ;
#51047 = EDGE_LOOP ( 'NONE', ( #90436, #32881, #62891, #96205 ) ) ;
#51048 = CARTESIAN_POINT ( 'NONE',  ( 17.08211943468705130, 63.47041550158063927, 12.26659068614894998 ) ) ;
#51049 = CARTESIAN_POINT ( 'NONE',  ( 24.16423886937409904, 54.09541550158063217, 3.795296366450317205 ) ) ;
#51050 = CARTESIAN_POINT ( 'NONE',  ( 2.791683348922237240, 25.38393115100078390, -7.208316651077763204 ) ) ;
#51051 = CARTESIAN_POINT ( 'NONE',  ( -2.816281873526471635, 23.91530133659708568, -3.434112377981056508 ) ) ;
#51052 = CARTESIAN_POINT ( 'NONE',  ( 4.431036607602561794, 0.5000000000000004441, -14.33059365769911153 ) ) ;
#51053 = DIRECTION ( 'NONE',  ( -0.8320502943378437211, 0.5547001962252290364, 0.000000000000000000 ) ) ;
#51054 = CARTESIAN_POINT ( 'NONE',  ( 15.44008868035555793, 16.39701867748817321, -9.422509992056140149 ) ) ;
#51055 = CARTESIAN_POINT ( 'NONE',  ( 24.16423886937409904, 54.09541550158063217, 3.795296366450317205 ) ) ;
#51056 = CARTESIAN_POINT ( 'NONE',  ( 10.00000000000000178, 27.25893115100078390, 9.846743663894594434 ) ) ;
#51057 = DIRECTION ( 'NONE',  ( 0.000000000000000000, 0.000000000000000000, 1.000000000000000000 ) ) ;
#51058 = CARTESIAN_POINT ( 'NONE',  ( 19.84674366389459266, 13.30059781766745353, 2.638427012816836559 ) ) ;
#51059 = EDGE_CURVE ( 'NONE', #74593, #96688, #750, .T. ) ;
#51060 = CARTESIAN_POINT ( 'NONE',  ( 12.34086200392826882, 0.000000000000000000, -7.124999999999971578 ) ) ;
#51061 = CARTESIAN_POINT ( 'NONE',  ( 9.846743663894594434, 8.508931151000792781, -2.168404344971008868E-15 ) ) ;
#51062 = ORIENTED_EDGE ( 'NONE', *, *, #69537, .T. ) ;
#51063 = ORIENTED_EDGE ( 'NONE', *, *, #58713, .F. ) ;
#51064 =( NAMED_UNIT ( * ) PLANE_ANGLE_UNIT ( ) SI_UNIT ( $, .RADIAN. ) );
#51065 = ORIENTED_EDGE ( 'NONE', *, *, #82436, .F. ) ;
#51066 = CARTESIAN_POINT ( 'NONE',  ( 17.08211943468705840, 15.13708216824730179, -12.26659068614894466 ) ) ;
#51068 = CARTESIAN_POINT ( 'NONE',  ( 19.42250999205614193, 30.14701867748817321, 5.440088680355555262 ) ) ;
#51067 = CARTESIAN_POINT ( 'NONE',  ( 0.5774900079438607392, 13.48035201082150358, 5.440088680355550821 ) ) ;
#51070 = CARTESIAN_POINT ( 'NONE',  ( 0.6178305044545818747, 13.49863466993041783, -9.382169495545419124 ) ) ;
#51069 = CARTESIAN_POINT ( 'NONE',  ( 14.92337183194729988, 54.34226448433412315, -8.527530157486177487 ) ) ;
#51071 = CARTESIAN_POINT ( 'NONE',  ( 17.08211943468705840, 5.137082168247300906, -12.26659068614894466 ) ) ;
#51072 = CARTESIAN_POINT ( 'NONE',  ( 19.84674366389459266, 43.71726448433411605, -2.638427012816827677 ) ) ;
#51073 = B_SPLINE_CURVE_WITH_KNOTS ( 'NONE', 3,
 ( #98067, #90530, #22064, #52537 ),
 .UNSPECIFIED., .F., .F.,
 ( 4, 4 ),
 ( 3.469446951953614189E-18, 0.001060528352562002848 ),
 .UNSPECIFIED. ) ;
#51074 = CARTESIAN_POINT ( 'NONE',  ( 0.6178305044545838731, 34.74863466993042493, 9.382169495545420901 ) ) ;
#51076 = ORIENTED_EDGE ( 'NONE', *, *, #20955, .T. ) ;
#51075 = CARTESIAN_POINT ( 'NONE',  ( 10.00000000000000000, -0.2410688489992152128, -9.846743663894594434 ) ) ;
#51077 = CARTESIAN_POINT ( 'NONE',  ( 2.791683348922240793, 26.63393115100078745, 7.208316651077764092 ) ) ;
#51078 = CARTESIAN_POINT ( 'NONE',  ( -4.164238869374099927, 57.01208216824731068, 3.795296366450308767 ) ) ;
#51079 = ORIENTED_EDGE ( 'NONE', *, *, #41939, .F. ) ;
#51080 = CARTESIAN_POINT ( 'NONE',  ( 4.559911319644449179, 2.230352010821504916, -9.422509992056141925 ) ) ;
#51081 = ORIENTED_EDGE ( 'NONE', *, *, #81450, .T. ) ;
#51082 = CARTESIAN_POINT ( 'NONE',  ( 10.00000000000000178, 49.31368534415484106, 10.88017736071110342 ) ) ;
#51083 = AXIS2_PLACEMENT_3D ( 'NONE', #66387, #72902, #43393 ) ;
#51084 = CARTESIAN_POINT ( 'NONE',  ( 10.00000000000000178, 44.31368534415484106, 10.88017736071110342 ) ) ;
#51085 = CARTESIAN_POINT ( 'NONE',  ( 19.42250999205614193, 50.14701867748817676, 5.440088680355555262 ) ) ;
#51086 = CARTESIAN_POINT ( 'NONE',  ( 18.00000000000000711, 77.36199599866324661, -4.193285603388146043 ) ) ;
#51087 = CARTESIAN_POINT ( 'NONE',  ( 20.88017736071110519, 35.56368534415484106, 2.639326808657452039E-16 ) ) ;
#51088 = CARTESIAN_POINT ( 'NONE',  ( 1.236355250167264774, 0.04962892728884438220, 14.70131747622448337 ) ) ;
#51089 = AXIS2_PLACEMENT_3D ( 'NONE', #44884, #14414, #85733 ) ;
#51090 = EDGE_CURVE ( 'NONE', #93614, #62473, #8707, .T. ) ;
#51092 = ORIENTED_EDGE ( 'NONE', *, *, #60105, .F. ) ;
#51091 = DIRECTION ( 'NONE',  ( 0.000000000000000000, -0.000000000000000000, 1.000000000000000000 ) ) ;
#51094 = B_SPLINE_CURVE_WITH_KNOTS ( 'NONE', 3,
 ( #33433, #40481, #26437, #49429, #70978, #25957 ),
 .UNSPECIFIED., .F., .F.,
 ( 4, 2, 4 ),
 ( 0.0002800001862105926565, 0.0006862054174524929908, 0.001092410648694393163 ),
 .UNSPECIFIED. ) ;
#51093 = CARTESIAN_POINT ( 'NONE',  ( 0.1532563361054083140, 26.00893115100078745, 1.131784320476157264E-15 ) ) ;
#51095 = EDGE_LOOP ( 'NONE', ( #87662, #8768, #25611, #29058, #92157, #31187 ) ) ;
#51096 = CARTESIAN_POINT ( 'NONE',  ( 17.20831665107776587, 62.88393115100078745, 7.208316651077764980 ) ) ;
#51097 = CARTESIAN_POINT ( 'NONE',  ( 14.42571047809459195, 14.76930270348883134, -3.890621016587847869 ) ) ;
#51098 = CARTESIAN_POINT ( 'NONE',  ( 10.00000000000000000, 10.55374883491396787, -14.16423886937410082 ) ) ;
#51099 = AXIS2_PLACEMENT_3D ( 'NONE', #5757, #59227, #28737 ) ;
#51100 = DIRECTION ( 'NONE',  ( 1.000000000000000000, 0.000000000000000000, 0.000000000000000000 ) ) ;
#51101 = CARTESIAN_POINT ( 'NONE',  ( 19.72487221294570858, 46.86607318730077054, 6.500000000000000888 ) ) ;
#51103 = CARTESIAN_POINT ( 'NONE',  ( 0.1532563361054083140, 36.00893115100078745, 1.131784320476157264E-15 ) ) ;
#51102 = CARTESIAN_POINT ( 'NONE',  ( 1.274849032794231007, 43.57228050351031357, 6.499999999999895195 ) ) ;
#51104 = CARTESIAN_POINT ( 'NONE',  ( 6.204703633549690345, 55.76208216824730357, -14.16423886937410259 ) ) ;
#51105 = CARTESIAN_POINT ( 'NONE',  ( 17.39651004071838614, 62.93575266056827644, 6.500000000000032863 ) ) ;
#51106 = ORIENTED_EDGE ( 'NONE', *, *, #31963, .T. ) ;
#51107 = CARTESIAN_POINT ( 'NONE',  ( -16.94000000000001194, 92.00000000000000000, 9.500000000000000000 ) ) ;
#51108 = CARTESIAN_POINT ( 'NONE',  ( 1.472469842513823179, 51.42559781766745886, 4.923371831947296329 ) ) ;
#51109 = PLANE ( 'NONE',  #94604 ) ;
#51110 = CARTESIAN_POINT ( 'NONE',  ( -2.816281873526473856, 9.123634669930421381, 9.499525473075851096E-16 ) ) ;
#51111 = CARTESIAN_POINT ( 'NONE',  ( 12.63842701281683922, 14.55059781766744997, -9.846743663894590881 ) ) ;
#51112 = CARTESIAN_POINT ( 'NONE',  ( 0.000000000000000000, 0.000000000000000000, 0.000000000000000000 ) ) ;
#51113 = CARTESIAN_POINT ( 'NONE',  ( 5.076628168052703671, 11.84226448433411960, 8.527530157486179263 ) ) ;
#51114 = CARTESIAN_POINT ( 'NONE',  ( 0.6178305044545818747, 8.498634669930421381, -9.382169495545419124 ) ) ;
#51115 = LINE ( 'NONE', #81603, #2603 ) ;
#51116 = VERTEX_POINT ( 'NONE', #39376 ) ;
#51117 = CARTESIAN_POINT ( 'NONE',  ( 20.88017736071110164, 15.35535201082150358, 2.915334737309930979 ) ) ;
#51118 = CARTESIAN_POINT ( 'NONE',  ( 2.917880565312950480, 0.9704155015806342766, -12.26659068614894821 ) ) ;
#51119 = CARTESIAN_POINT ( 'NONE',  ( 0.1532563361054083140, 31.00893115100078390, 1.131784320476157264E-15 ) ) ;
#51120 = CARTESIAN_POINT ( 'NONE',  ( 15.44008868035555793, 56.39701867748817676, -9.422509992056140149 ) ) ;
#51122 = FILL_AREA_STYLE ('',( #21129 ) ) ;
#51121 = CARTESIAN_POINT ( 'NONE',  ( 16.40814093676324603, 32.45696800326375353, -11.09922568453594671 ) ) ;
#51123 = CARTESIAN_POINT ( 'NONE',  ( 20.88017736071110519, 5.563685344154837509, 2.639326808657452039E-16 ) ) ;
#51124 = CARTESIAN_POINT ( 'NONE',  ( -1.926860441876564023, 57.87045670184114954, 3.195792623639529761 ) ) ;
#51125 = PRESENTATION_STYLE_ASSIGNMENT (( #11156 ) ) ;
#51126 = CARTESIAN_POINT ( 'NONE',  ( 19.38216949554541557, 2.248634669930420049, -9.382169495545420901 ) ) ;
#51127 = CARTESIAN_POINT ( 'NONE',  ( -2.816281873526473856, -0.8763653300695799508, 9.499525473075851096E-16 ) ) ;
#51128 = CARTESIAN_POINT ( 'NONE',  ( 1.472469842513823179, 15.59226448433411960, -4.923371831947296329 ) ) ;
#51129 = CARTESIAN_POINT ( 'NONE',  ( 3.469446951953614189E-15, -25.68631465584515894, 10.88017736071110342 ) ) ;
#51130 = CARTESIAN_POINT ( 'NONE',  ( -2.816281873526473856, 24.33196800326375353, 3.434112377981055619 ) ) ;
#51131 = CARTESIAN_POINT ( 'NONE',  ( -11.07532115247915883, -96.02567358739618442, -3.999999999999774403 ) ) ;
#51133 = CARTESIAN_POINT ( 'NONE',  ( 2.930023131210769627, 0.000000000000000000, -4.599215049682158885 ) ) ;
#51132 = CARTESIAN_POINT ( 'NONE',  ( 17.96484262340118221, 36.18868534415484106, -7.964842623401177768 ) ) ;
#51134 = CARTESIAN_POINT ( 'NONE',  ( 32.06412365047463453, 14.00000000000001421, -9.500000000000000000 ) ) ;
#51135 = CYLINDRICAL_SURFACE ( 'NONE', #96113, 0.2500000000000002220 ) ;
#51136 = EDGE_CURVE ( 'NONE', #55108, #32731, #78944, .T. ) ;
#51137 = CARTESIAN_POINT ( 'NONE',  ( 19.42250999205614548, 20.98035201082150891, -5.440088680355545492 ) ) ;
#51138 = VECTOR ( 'NONE', #56691, 1000.000000000000227 ) ;
#51139 = EDGE_CURVE ( 'NONE', #61703, #93127, #2868, .T. ) ;
#51140 = CARTESIAN_POINT ( 'NONE',  ( 7.361572987183170547, 52.05059781766745175, 9.846743663894590881 ) ) ;
#51141 = CARTESIAN_POINT ( 'NONE',  ( 4.559911319644449179, 53.89701867748817676, 9.422509992056141925 ) ) ;
#51142 = CARTESIAN_POINT ( 'NONE',  ( -4.164238869374099039, 36.80374883491396787, 8.674139862899312516E-16 ) ) ;
#51144 = EDGE_CURVE ( 'NONE', #23745, #11622, #45615, .T. ) ;
#51143 = DIRECTION ( 'NONE',  ( 0.8526401643540847397, 0.000000000000000000, 0.5224985647159611224 ) ) ;
#51145 = EDGE_CURVE ( 'NONE', #20172, #35060, #87135, .T. ) ;
#51146 = UNCERTAINTY_MEASURE_WITH_UNIT (LENGTH_MEASURE( 1.000000000000000082E-05 ), #47184, 'distance_accuracy_value', 'NONE');
#51147 = CARTESIAN_POINT ( 'NONE',  ( 17.20831665107776587, 44.13393115100078745, -7.208316651077762316 ) ) ;
#51148 = CARTESIAN_POINT ( 'NONE',  ( 13.43411237798105340, 60.58196800326376064, 12.81628187352647963 ) ) ;
#51149 = AXIS2_PLACEMENT_3D ( 'NONE', #9957, #68986, #76965 ) ;
#51150 = CARTESIAN_POINT ( 'NONE',  ( 19.38216949554541557, 2.248634669930420049, -9.382169495545420901 ) ) ;
#51151 = ORIENTED_EDGE ( 'NONE', *, *, #33090, .T. ) ;
#51152 = CARTESIAN_POINT ( 'NONE',  ( 0.5774900079438607392, 28.48035201082150891, 5.440088680355550821 ) ) ;
#51153 = CARTESIAN_POINT ( 'NONE',  ( 21.92686044187656691, 7.188309369127508397, 4.562052436263911564E-16 ) ) ;
#51154 = CARTESIAN_POINT ( 'NONE',  ( 19.42250999205614548, 5.980352010821504471, -5.440088680355545492 ) ) ;
#51155 = CARTESIAN_POINT ( 'NONE',  ( -0.8801773607110991993, 17.85535201082150536, -2.915334737309923874 ) ) ;
#51156 = CARTESIAN_POINT ( 'NONE',  ( 0.5774900079438590739, 62.64701867748817676, -5.440088680355550821 ) ) ;
#51157 = CARTESIAN_POINT ( 'NONE',  ( 2.917880565312948704, 27.63708216824730357, 12.26659068614894643 ) ) ;
#51158 = CARTESIAN_POINT ( 'NONE',  ( 7.361572987183169658, 19.96726448433411960, -9.846743663894592657 ) ) ;
#51159 = CARTESIAN_POINT ( 'NONE',  ( 17.20831665107776587, 59.13393115100078745, -7.208316651077762316 ) ) ;
#51160 = CARTESIAN_POINT ( 'NONE',  ( 10.00000000000000178, 29.31368534415483751, 10.88017736071110342 ) ) ;
#51161 = CYLINDRICAL_SURFACE ( 'NONE', #20820, 15.00000000000000000 ) ;
#51162 = CARTESIAN_POINT ( 'NONE',  ( -7.750000000000000000, 80.07179676972448590, 6.250000000000000000 ) ) ;
#51163 = AXIS2_PLACEMENT_3D ( 'NONE', #90181, #45183, #60672 ) ;
#51164 = ORIENTED_EDGE ( 'NONE', *, *, #83547, .T. ) ;
#51165 = CARTESIAN_POINT ( 'NONE',  ( 4.145753578648191606, -0.8370341202481567100, 2.499999999999999556 ) ) ;
#51166 = CARTESIAN_POINT ( 'NONE',  ( 19.84674366389459266, 43.71726448433410894, -2.638427012816827677 ) ) ;
#51167 = ORIENTED_EDGE ( 'NONE', *, *, #82402, .T. ) ;
#51168 = EDGE_LOOP ( 'NONE', ( #57356, #10203, #6566, #88086 ) ) ;
#51169 = CARTESIAN_POINT ( 'NONE',  ( -5.428133280998936883, 0.000000000000000000, -0.5226697871168243248 ) ) ;
#51170 = CARTESIAN_POINT ( 'NONE',  ( 17.08211943468705130, 23.47041550158063572, 12.26659068614894998 ) ) ;
#51171 = CARTESIAN_POINT ( 'NONE',  ( 20.36894250292379382, 8.678748834913967869, 10.36894250292379205 ) ) ;
#51172 = CARTESIAN_POINT ( 'NONE',  ( 17.96484262340118221, 54.93868534415484106, 7.964842623401181321 ) ) ;
#51173 = CARTESIAN_POINT ( 'NONE',  ( 24.16423886937410614, 54.51208216824730357, -3.795296366450302550 ) ) ;
#51174 = CARTESIAN_POINT ( 'NONE',  ( -1.099225684535947600, -1.293031996736246469, -6.408140936763238038 ) ) ;
#51175 = CARTESIAN_POINT ( 'NONE',  ( 12.63842701281683034, 52.46726448433413026, 9.846743663894596210 ) ) ;
#51176 = CARTESIAN_POINT ( 'NONE',  ( -11.07542066933276992, -96.02453755662239132, 3.750000000000000000 ) ) ;
#51178 = CARTESIAN_POINT ( 'NONE',  ( 10.00000000000000000, 2.873634669930420049, -12.81628187352647608 ) ) ;
#51177 = CARTESIAN_POINT ( 'NONE',  ( 0.5774900079438590739, 37.64701867748817676, -5.440088680355550821 ) ) ;
#51179 = CARTESIAN_POINT ( 'NONE',  ( 2.917880565312948704, 12.63708216824730179, 12.26659068614894643 ) ) ;
#51180 = CARTESIAN_POINT ( 'NONE',  ( 24.16423886937410614, 54.30374883491396787, 8.672049930838204340E-16 ) ) ;
#51181 = CARTESIAN_POINT ( 'NONE',  ( 19.42250999205614193, 15.14701867748817143, 5.440088680355555262 ) ) ;
#51182 = CARTESIAN_POINT ( 'NONE',  ( 19.72487221294571569, 14.78217586085237656, 6.499999999999995559 ) ) ;
#51183 = CARTESIAN_POINT ( 'NONE',  ( 10.00000000000000000, 46.81368534415484106, -10.88017736071110342 ) ) ;
#51184 = EDGE_CURVE ( 'NONE', #60118, #2137, #69374, .T. ) ;
#51185 = CARTESIAN_POINT ( 'NONE',  ( -8.527530157486182816, -34.40773551566587685, -4.923371831947288335 ) ) ;
#51186 = EDGE_LOOP ( 'NONE', ( #9658, #76291, #6447, #38040, #9270, #45488, #20592 ) ) ;
#51187 = CARTESIAN_POINT ( 'NONE',  ( -11.64999999999999680, 98.49999999999998579, 8.000000000000000000 ) ) ;
#51188 = VERTEX_POINT ( 'NONE', #16375 ) ;
#51189 = ORIENTED_EDGE ( 'NONE', *, *, #30160, .F. ) ;
#51190 = CARTESIAN_POINT ( 'NONE',  ( 24.16423886937410614, 49.30374883491396787, 8.672049930838204340E-16 ) ) ;
#51191 = CARTESIAN_POINT ( 'NONE',  ( 10.00000000000000000, 44.75893115100078745, -9.846743663894594434 ) ) ;
#51192 = CARTESIAN_POINT ( 'NONE',  ( 10.00000000000000000, 56.81368534415484106, -10.88017736071110342 ) ) ;
#51193 = DIRECTION ( 'NONE',  ( -1.776356839400250780E-14, 0.000000000000000000, 1.000000000000000000 ) ) ;
#51194 = EDGE_CURVE ( 'NONE', #24774, #51686, #35794, .T. ) ;
#51195 = CARTESIAN_POINT ( 'NONE',  ( 12.91533473730993009, 56.60535201082151247, -10.88017736071109987 ) ) ;
#51196 = CIRCLE ( 'NONE', #63950, 0.5000000000000004441 ) ;
#51197 = CARTESIAN_POINT ( 'NONE',  ( -1.099225684535947600, 58.70696800326375353, -6.408140936763238038 ) ) ;
#51198 = CARTESIAN_POINT ( 'NONE',  ( 11.09922568453594671, 12.04030133659709456, -6.408140936763241591 ) ) ;
#51199 = VERTEX_POINT ( 'NONE', #50806 ) ;
#51200 = CARTESIAN_POINT ( 'NONE',  ( 6.204703633549690345, 25.76208216824730712, -14.16423886937410259 ) ) ;
#51201 = ORIENTED_EDGE ( 'NONE', *, *, #57354, .T. ) ;
#51202 = CARTESIAN_POINT ( 'NONE',  ( 21.09922568453595559, 22.04030133659708923, -6.408140936763230044 ) ) ;
#51203 = VERTEX_POINT ( 'NONE', #34801 ) ;
#51204 = CARTESIAN_POINT ( 'NONE',  ( 6.565887622018943937, 43.08196800326374643, -12.81628187352647608 ) ) ;
#51205 = CARTESIAN_POINT ( 'NONE',  ( 19.42250999205614193, 15.14701867748817143, 5.440088680355555262 ) ) ;
#51206 = CARTESIAN_POINT ( 'NONE',  ( 14.92337183194729633, 32.67559781766745175, 8.527530157486181039 ) ) ;
#51207 = CARTESIAN_POINT ( 'NONE',  ( 12.91533473730992121, 14.52201867748817143, 10.88017736071110164 ) ) ;
#51208 = CARTESIAN_POINT ( 'NONE',  ( 19.38216949554541557, 57.24863466993042493, -9.382169495545420901 ) ) ;
#51209 = DIRECTION ( 'NONE',  ( -0.000000000000000000, -0.000000000000000000, 1.000000000000000000 ) ) ;
#51210 = CARTESIAN_POINT ( 'NONE',  ( 2.791683348922240793, 41.63393115100078745, 7.208316651077764092 ) ) ;
#51212 = TOROIDAL_SURFACE ( 'NONE', #25678, 14.49999999999999822, 0.5000000000000000000 ) ;
#51211 = CARTESIAN_POINT ( 'NONE',  ( 13.34343830728403724, 14.49999999999999112, 6.852200678592740068 ) ) ;
#51213 = DIRECTION ( 'NONE',  ( -1.000000000000000000, 0.000000000000000000, 0.000000000000000000 ) ) ;
#51214 = DIRECTION ( 'NONE',  ( 0.000000000000000000, 0.000000000000000000, 1.000000000000000000 ) ) ;
#51215 = CARTESIAN_POINT ( 'NONE',  ( -12.25993886608611660, 0.5000000000000004441, 8.642563219313529999 ) ) ;
#51216 = CARTESIAN_POINT ( 'NONE',  ( 1.472469842513823179, 16.42559781766745175, 4.923371831947296329 ) ) ;
#51217 = CARTESIAN_POINT ( 'NONE',  ( 22.81628187352648496, 26.83196800326374998, -3.434112377981050290 ) ) ;
#51218 = AXIS2_PLACEMENT_3D ( 'NONE', #33069, #61239, #71585 ) ;
#51219 = AXIS2_PLACEMENT_3D ( 'NONE', #46486, #39978, #92963 ) ;
#51220 = VERTEX_POINT ( 'NONE', #72306 ) ;
#51221 = CARTESIAN_POINT ( 'NONE',  ( 5.076628168052704559, 60.17559781766745175, -8.527530157486179263 ) ) ;
#51222 = CARTESIAN_POINT ( 'NONE',  ( 0.8060400322138880913, 0.000000000000000000, 5.393339789881745894 ) ) ;
#51223 = CARTESIAN_POINT ( 'NONE',  ( -4.164238869374098151, 21.59541550158063217, -3.795296366450310543 ) ) ;
#51224 = CARTESIAN_POINT ( 'NONE',  ( 18.52753015748617571, 43.09226448433412315, 4.923371831947298993 ) ) ;
#51225 = CARTESIAN_POINT ( 'NONE',  ( 0.6178305044545818747, 43.49863466993042493, -9.382169495545419124 ) ) ;
#51227 = CARTESIAN_POINT ( 'NONE',  ( 69.60148758828984228, -4.049828892140921146E-15, 10.00000000000000000 ) ) ;
#51226 = CARTESIAN_POINT ( 'NONE',  ( 14.24131928502211686, 15.00000000000000000, -0.4973178280105898241 ) ) ;
#51228 = CARTESIAN_POINT ( 'NONE',  ( 20.88017736071110519, 60.56368534415484106, 2.639326808657452039E-16 ) ) ;
#51229 = CIRCLE ( 'NONE', #17497, 1.000000000000000000 ) ;
#51230 = EDGE_CURVE ( 'NONE', #35164, #7679, #18280, .T. ) ;
#51231 = CARTESIAN_POINT ( 'NONE',  ( 2.791683348922240793, 31.63393115100078745, 7.208316651077764092 ) ) ;
#51232 = CARTESIAN_POINT ( 'NONE',  ( 2.035157376598824452, 43.68868534415484106, 7.964842623401179544 ) ) ;
#51233 = CARTESIAN_POINT ( 'NONE',  ( 21.09922568453594849, 46.20696800326376064, 6.408140936763242479 ) ) ;
#51234 = CARTESIAN_POINT ( 'NONE',  ( -12.74305857943755882, 15.00000000000000178, 7.177950183686771624 ) ) ;
#51235 = CARTESIAN_POINT ( 'NONE',  ( 20.88017736071110875, 40.77201867748818387, -2.915334737309920765 ) ) ;
#51236 = ORIENTED_EDGE ( 'NONE', *, *, #37081, .F. ) ;
#51237 = DIRECTION ( 'NONE',  ( 0.000000000000000000, 1.000000000000000000, 0.000000000000000000 ) ) ;
#51238 = CARTESIAN_POINT ( 'NONE',  ( 15.44008868035555793, 16.39701867748817321, -9.422509992056140149 ) ) ;
#51240 = CARTESIAN_POINT ( 'NONE',  ( 4.559911319644449179, 43.89701867748816966, 9.422509992056141925 ) ) ;
#51239 = CARTESIAN_POINT ( 'NONE',  ( 17.20831665107776587, 62.88393115100078745, 7.208316651077764980 ) ) ;
#51241 = CARTESIAN_POINT ( 'NONE',  ( 15.44008868035555260, 59.73035201082151247, 9.422509992056143702 ) ) ;
#51243 = CARTESIAN_POINT ( 'NONE',  ( -0.000000000000000000, 76.91853713602722564, -7.561724626172516395 ) ) ;
#51242 = CARTESIAN_POINT ( 'NONE',  ( 0.5774900079438607392, 28.48035201082150891, 5.440088680355550821 ) ) ;
#51244 = CARTESIAN_POINT ( 'NONE',  ( 19.39235739573469530, 49.87576471608600315, 6.499999999999993783 ) ) ;
#51245 = CARTESIAN_POINT ( 'NONE',  ( 12.63842701281683034, 27.46726448433411250, 9.846743663894596210 ) ) ;
#51246 = CARTESIAN_POINT ( 'NONE',  ( -46.30928139467842897, 104.0823827281712255, -5.529860068218142466 ) ) ;
#51247 = CARTESIAN_POINT ( 'NONE',  ( -10.36894250292379205, 11.17874883491397675, -10.36894250292378672 ) ) ;
#51248 = CARTESIAN_POINT ( 'NONE',  ( 0.1532563361054083140, 51.00893115100078745, 1.131784320476157264E-15 ) ) ;
#51249 = B_SPLINE_CURVE_WITH_KNOTS ( 'NONE', 3,
 ( #59198, #7204, #97238, #36214 ),
 .UNSPECIFIED., .F., .F.,
 ( 4, 4 ),
 ( 0.000000000000000000, 0.001036303429213363990 ),
 .UNSPECIFIED. ) ;
#51251 = CARTESIAN_POINT ( 'NONE',  ( 15.00000000000000178, 73.00000000000000000, 4.000000000000000000 ) ) ;
#51250 = CARTESIAN_POINT ( 'NONE',  ( 6.204703633549690345, 50.76208216824730357, -14.16423886937410259 ) ) ;
#51252 = CARTESIAN_POINT ( 'NONE',  ( 1.821708436314909640, 61.66792564121894316, -6.499999999999922728 ) ) ;
#51253 = CARTESIAN_POINT ( 'NONE',  ( 10.00000000000000178, 13.05374883491396787, 14.16423886937410082 ) ) ;
#51254 = CARTESIAN_POINT ( 'NONE',  ( 22.26659068614895176, 39.72041550158063217, -7.082119434687042414 ) ) ;
#51255 = CARTESIAN_POINT ( 'NONE',  ( 13.43411237798105340, 0.5819680032637533085, 12.81628187352647963 ) ) ;
#51256 = EDGE_CURVE ( 'NONE', #54489, #41784, #87799, .T. ) ;
#51257 = VECTOR ( 'NONE', #72398, 1000.000000000000000 ) ;
#51258 = EDGE_LOOP ( 'NONE', ( #42895, #76499, #1362, #94405 ) ) ;
#51259 = CARTESIAN_POINT ( 'NONE',  ( -0.8801773607110991993, 7.855352010821506248, -2.915334737309923874 ) ) ;
#51260 = CARTESIAN_POINT ( 'NONE',  ( 18.52753015748617571, 43.09226448433412315, 4.923371831947298993 ) ) ;
#51262 = CARTESIAN_POINT ( 'NONE',  ( 8.880000000000000782, 1.116573172248542834E-15, 6.250000000000000000 ) ) ;
#51261 = FACE_OUTER_BOUND ( 'NONE', #65424, .T. ) ;
#51263 = SURFACE_SIDE_STYLE ('',( #96787 ) ) ;
#51264 = EDGE_CURVE ( 'NONE', #23770, #2388, #49727, .T. ) ;
#51265 = CARTESIAN_POINT ( 'NONE',  ( 0.1532563361054100626, 0.8005978176674514168, -2.638427012816831230 ) ) ;
#51266 = CARTESIAN_POINT ( 'NONE',  ( 3.591859063236763294, 28.29030133659708568, -11.09922568453595026 ) ) ;
#51267 = CARTESIAN_POINT ( 'NONE',  ( 5.076628168052703671, 31.84226448433412315, 8.527530157486179263 ) ) ;
#51268 = VERTEX_POINT ( 'NONE', #3337 ) ;
#51269 = CARTESIAN_POINT ( 'NONE',  ( 7.361572987183170547, 2.050597817667451750, 9.846743663894590881 ) ) ;
#51270 = CARTESIAN_POINT ( 'NONE',  ( -11.10175276307583658, 0.04962894967561114201, -9.716398248524834358 ) ) ;
#51271 = PLANE ( 'NONE',  #50703 ) ;
#51272 = CARTESIAN_POINT ( 'NONE',  ( 12.91533473730993009, 16.60535201082150891, -10.88017736071109987 ) ) ;
#51273 = CARTESIAN_POINT ( 'NONE',  ( 17.08211943468705840, 40.13708216824731068, -12.26659068614894466 ) ) ;
#51274 = CARTESIAN_POINT ( 'NONE',  ( -0.8801773607110991993, 47.85535201082150536, -2.915334737309923874 ) ) ;
#51275 = CARTESIAN_POINT ( 'NONE',  ( 0.5774900079438590739, 67.64701867748817676, -5.440088680355550821 ) ) ;
#51276 = CARTESIAN_POINT ( 'NONE',  ( -7.750000000000000000, 79.82179676972448590, 6.500000000000000888 ) ) ;
#51277 = CARTESIAN_POINT ( 'NONE',  ( 0.2751277870542876980, 48.21833443783936701, 6.499999999999984901 ) ) ;
#51278 = CARTESIAN_POINT ( 'NONE',  ( 12.63842701281683922, 29.55059781766745175, -9.846743663894590881 ) ) ;
#51279 = SURFACE_SIDE_STYLE ('',( #66268 ) ) ;
#51280 = CARTESIAN_POINT ( 'NONE',  ( 12.63842701281683034, 2.467264484334118269, 9.846743663894596210 ) ) ;
#51281 = CARTESIAN_POINT ( 'NONE',  ( 19.84674366389459266, 33.30059781766744464, 2.638427012816836559 ) ) ;
#51282 = CARTESIAN_POINT ( 'NONE',  ( 10.00000000000000000, 59.75893115100078745, -9.846743663894594434 ) ) ;
#51283 = CARTESIAN_POINT ( 'NONE',  ( 20.88017736071110164, 35.35535201082150536, 2.915334737309930979 ) ) ;
#51284 = UNCERTAINTY_MEASURE_WITH_UNIT (LENGTH_MEASURE( 1.000000000000000082E-05 ), #1583, 'distance_accuracy_value', 'NONE');
#51285 = AXIS2_PLACEMENT_3D ( 'NONE', #28999, #67515, #22517 ) ;
#51286 = ORIENTED_EDGE ( 'NONE', *, *, #56268, .T. ) ;
#51287 = CARTESIAN_POINT ( 'NONE',  ( -1.099225684535947600, 53.70696800326376064, -6.408140936763238038 ) ) ;
#51288 = CARTESIAN_POINT ( 'NONE',  ( 4.559911319644449179, 67.23035201082150536, -9.422509992056141925 ) ) ;
#51289 = CARTESIAN_POINT ( 'NONE',  ( 21.09922568453595559, 42.04030133659708213, -6.408140936763230044 ) ) ;
#51291 = CARTESIAN_POINT ( 'NONE',  ( 2.791683348922237240, 30.38393115100078390, -7.208316651077763204 ) ) ;
#51290 = CARTESIAN_POINT ( 'NONE',  ( 6.204703633549690345, 57.84541550158063927, 14.16423886937410082 ) ) ;
#51292 = DIRECTION ( 'NONE',  ( 0.000000000000000000, 1.000000000000000000, 0.000000000000000000 ) ) ;
#51293 = DIRECTION ( 'NONE',  ( 0.000000000000000000, 0.000000000000000000, 1.000000000000000000 ) ) ;
#51294 = CARTESIAN_POINT ( 'NONE',  ( 17.08211943468705130, 38.47041550158063217, 12.26659068614894998 ) ) ;
#51295 = CARTESIAN_POINT ( 'NONE',  ( 1.472469842513823179, 45.59226448433412315, -4.923371831947296329 ) ) ;
#51296 = CIRCLE ( 'NONE', #40161, 14.49999999999999822 ) ;
#51297 = CARTESIAN_POINT ( 'NONE',  ( -14.43100913236851568, 4.866596497322921311E-16, 1.412789942453065883 ) ) ;
#51298 = CARTESIAN_POINT ( 'NONE',  ( -0.8801773607111008646, 33.27201867748817676, 2.915334737309923430 ) ) ;
#51299 = EDGE_CURVE ( 'NONE', #58998, #58863, #71173, .T. ) ;
#51300 = CARTESIAN_POINT ( 'NONE',  ( 2.035157376598822676, 57.43868534415484106, -7.964842623401177768 ) ) ;
#51301 =( NAMED_UNIT ( * ) SI_UNIT ( $, .STERADIAN. ) SOLID_ANGLE_UNIT ( ) );
#51302 = ORIENTED_EDGE ( 'NONE', *, *, #841, .F. ) ;
#51303 = CARTESIAN_POINT ( 'NONE',  ( -2.816281873526473856, 49.33196800326374643, 3.434112377981055619 ) ) ;
#51304 = STYLED_ITEM ( 'NONE', ( #49082 ), #74465 ) ;
#51305 = CARTESIAN_POINT ( 'NONE',  ( 7.084665262690076126, 69.10535201082151957, 10.88017736071109987 ) ) ;
#51306 = ORIENTED_EDGE ( 'NONE', *, *, #5216, .T. ) ;
#51307 = CARTESIAN_POINT ( 'NONE',  ( 2.917880565312948704, 7.637082168247301794, 12.26659068614894643 ) ) ;
#51308 = CARTESIAN_POINT ( 'NONE',  ( 5.076628168052703671, 1.842264484334118047, 8.527530157486179263 ) ) ;
#51309 = CARTESIAN_POINT ( 'NONE',  ( 1.420647316330978072, 0.04189720826290899841, -6.202995698450457063 ) ) ;
#51310 = EDGE_LOOP ( 'NONE', ( #19448, #75087, #38693, #76667 ) ) ;
#51311 = CARTESIAN_POINT ( 'NONE',  ( -0.8801773607111009756, 8.063685344154837509, 1.068504757029289695E-15 ) ) ;
#51312 = DIRECTION ( 'NONE',  ( 0.000000000000000000, 1.000000000000000000, 0.000000000000000000 ) ) ;
#51313 = CARTESIAN_POINT ( 'NONE',  ( 2.917880565312948704, 22.63708216824730002, 12.26659068614894643 ) ) ;
#51314 = EDGE_LOOP ( 'NONE', ( #36074, #2665, #25410, #59168 ) ) ;
#51315 = CARTESIAN_POINT ( 'NONE',  ( 15.44008868035555793, 26.39701867748817321, -9.422509992056140149 ) ) ;
#51316 = CARTESIAN_POINT ( 'NONE',  ( 18.52753015748618282, 63.92559781766745886, -4.923371831947291888 ) ) ;
#51317 = ORIENTED_EDGE ( 'NONE', *, *, #75291, .F. ) ;
#51318 = CARTESIAN_POINT ( 'NONE',  ( 7.361572987183169658, 59.96726448433410894, -9.846743663894592657 ) ) ;
#51319 = ORIENTED_EDGE ( 'NONE', *, *, #77114, .F. ) ;
#51320 = CARTESIAN_POINT ( 'NONE',  ( 0.5774900079438590739, 67.64701867748817676, -5.440088680355550821 ) ) ;
#51321 = CARTESIAN_POINT ( 'NONE',  ( 3.541595367958687568, 0.000000000000000000, -4.146675399920591865 ) ) ;
#51322 = CARTESIAN_POINT ( 'NONE',  ( 10.00000000000000000, 37.87363466993041783, -12.81628187352647608 ) ) ;
#51324 = PLANE ( 'NONE',  #52661 ) ;
#51323 = CARTESIAN_POINT ( 'NONE',  ( 10.00000000000000000, 1.813685344154837731, -10.88017736071110342 ) ) ;
#51325 = CARTESIAN_POINT ( 'NONE',  ( 19.84674366389459266, 8.300597817667451750, 2.638427012816836559 ) ) ;
#51326 = CARTESIAN_POINT ( 'NONE',  ( 17.96484262340118221, 16.18868534415483396, -7.964842623401177768 ) ) ;
#51327 = AXIS2_PLACEMENT_3D ( 'NONE', #30829, #98878, #31805 ) ;
#51328 = B_SPLINE_CURVE_WITH_KNOTS ( 'NONE', 3,
 ( #86569, #87050, #95541, #27031, #57530, #88024 ),
 .UNSPECIFIED., .F., .F.,
 ( 4, 2, 4 ),
 ( 0.0002800086601590408698, 0.0006862139742845935111, 0.001092419288410146315 ),
 .UNSPECIFIED. ) ;
#51329 =( BOUNDED_CURVE ( )  B_SPLINE_CURVE ( 2, ( #63045, #4038, #42042, #57510, #55555, #12017, #27012, #71551, #87024 ),
 .UNSPECIFIED., .F., .F. ) 
 B_SPLINE_CURVE_WITH_KNOTS ( ( 3, 2, 2, 2, 3 ),
 ( 0.8310855930462679453, 0.8333333333333333703, 0.8392857142857143016, 0.8452380952380952328, 0.8474858355251606579 ),
 .UNSPECIFIED. ) 
 CURVE ( )  GEOMETRIC_REPRESENTATION_ITEM ( )  RATIONAL_B_SPLINE_CURVE ( ( 0.9839835555609424134, 0.9871328979762477029, 1.000000000000000000, 0.9659258262890683122, 1.000000000000000000, 0.9659258262890683122, 1.000000000000000000, 0.9871328979762474809, 0.9839835555609424134 ) ) 
 REPRESENTATION_ITEM ( '' )  );
#51330 = VECTOR ( 'NONE', #7885, 1000.000000000000227 ) ;
#51331 = ORIENTED_EDGE ( 'NONE', *, *, #41586, .F. ) ;
#51332 = CARTESIAN_POINT ( 'NONE',  ( 6.565887622018943937, 58.08196800326376064, -12.81628187352647608 ) ) ;
#51333 = CARTESIAN_POINT ( 'NONE',  ( 2.035157376598822676, 37.43868534415484106, -7.964842623401177768 ) ) ;
#51334 = CARTESIAN_POINT ( 'NONE',  ( -0.1503990784575328643, 70.00000000000000000, -6.262539305110068177 ) ) ;
#51335 = CARTESIAN_POINT ( 'NONE',  ( 10.00000000000000178, 35.37363466993042493, 12.81628187352647608 ) ) ;
#51336 = CARTESIAN_POINT ( 'NONE',  ( 10.00000000000000000, 46.81368534415484106, -10.88017736071110342 ) ) ;
#51337 = CARTESIAN_POINT ( 'NONE',  ( 10.00000000000000000, 59.75893115100078745, -9.846743663894594434 ) ) ;
#51338 = CARTESIAN_POINT ( 'NONE',  ( 0.000000000000000000, 0.5000000000000004441, 0.000000000000000000 ) ) ;
#51339 = CARTESIAN_POINT ( 'NONE',  ( 12.63842701281683034, 12.46726448433411782, 9.846743663894596210 ) ) ;
#51340 = CARTESIAN_POINT ( 'NONE',  ( 10.00000000000000000, 12.87363466993042138, -12.81628187352647608 ) ) ;
#51342 = CYLINDRICAL_SURFACE ( 'NONE', #76901, 0.5000000000000004441 ) ;
#51341 = DIRECTION ( 'NONE',  ( -3.996802888650562914E-14, 0.000000000000000000, 1.000000000000000000 ) ) ;
#51343 = CARTESIAN_POINT ( 'NONE',  ( 0.5774900079438607392, 18.48035201082150536, 5.440088680355550821 ) ) ;
#51344 = CARTESIAN_POINT ( 'NONE',  ( 5.076628168052703671, 51.84226448433412315, 8.527530157486179263 ) ) ;
#51345 = DIRECTION ( 'NONE',  ( 0.000000000000000000, 0.000000000000000000, 1.000000000000000000 ) ) ;
#51346 = DIRECTION ( 'NONE',  ( 0.4461978131098069400, 0.000000000000000000, -0.8949343616020258851 ) ) ;
#51347 = EDGE_CURVE ( 'NONE', #20694, #80255, #56825, .T. ) ;
#51348 = CARTESIAN_POINT ( 'NONE',  ( 7.361572987183170547, 12.05059781766744997, 9.846743663894590881 ) ) ;
#51349 = CARTESIAN_POINT ( 'NONE',  ( 19.84674366389459621, 28.50893115100078745, 7.409399052514197653E-17 ) ) ;
#51351 = ORIENTED_EDGE ( 'NONE', *, *, #55912, .T. ) ;
#51350 = CARTESIAN_POINT ( 'NONE',  ( 22.81628187352648496, 6.831968003263753531, -3.434112377981050290 ) ) ;
#51352 = AXIS2_PLACEMENT_3D ( 'NONE', #37036, #68026, #8506 ) ;
#51353 = AXIS2_PLACEMENT_3D ( 'NONE', #46795, #85296, #38819 ) ;
#51354 = CARTESIAN_POINT ( 'NONE',  ( 16.40814093676324603, 42.45696800326375353, -11.09922568453594671 ) ) ;
#51355 = CARTESIAN_POINT ( 'NONE',  ( 0.1532563361054083140, 31.00893115100078390, 1.131784320476157264E-15 ) ) ;
#51356 = CARTESIAN_POINT ( 'NONE',  ( 17.08211943468705840, 55.13708216824731068, -12.26659068614894466 ) ) ;
#51357 = CARTESIAN_POINT ( 'NONE',  ( 2.791683348922237240, 35.38393115100079456, -7.208316651077763204 ) ) ;
#51358 = STYLED_ITEM ( 'NONE', ( #85375 ), #47285 ) ;
#51359 = CARTESIAN_POINT ( 'NONE',  ( 0.9413316022086175572, 18.45508385108958649, 6.499999999999973355 ) ) ;
#51360 = CARTESIAN_POINT ( 'NONE',  ( 17.96484262340118221, 9.938685344154839285, 7.964842623401181321 ) ) ;
#51361 = CARTESIAN_POINT ( 'NONE',  ( 0.1532563361054082862, 66.21726448433413736, 2.638427012816831674 ) ) ;
#51362 = CARTESIAN_POINT ( 'NONE',  ( -0.8801773607111009756, 23.06368534415484106, 1.068504757029289695E-15 ) ) ;
#51363 = CARTESIAN_POINT ( 'NONE',  ( 22.26659068614895176, 44.72041550158063927, -7.082119434687042414 ) ) ;
#51365 = CARTESIAN_POINT ( 'NONE',  ( -10.82361996477984789, 0.04962893104176982484, 10.02529603627126953 ) ) ;
#51364 = CARTESIAN_POINT ( 'NONE',  ( 13.79529636645030344, 48.26208216824728936, 14.16423886937410614 ) ) ;
#51366 =( NAMED_UNIT ( * ) SI_UNIT ( $, .STERADIAN. ) SOLID_ANGLE_UNIT ( ) );
#51367 = AXIS2_PLACEMENT_3D ( 'NONE', #30558, #16069, #1086 ) ;
#51368 = CARTESIAN_POINT ( 'NONE',  ( 7.361572987183170547, 17.05059781766745530, 9.846743663894590881 ) ) ;
#51369 = CARTESIAN_POINT ( 'NONE',  ( 3.591859063236761518, -0.04303199673624671928, 11.09922568453594849 ) ) ;
#51370 = ORIENTED_EDGE ( 'NONE', *, *, #31556, .F. ) ;
#51371 = CARTESIAN_POINT ( 'NONE',  ( 2.035157376598824452, 43.68868534415484106, 7.964842623401179544 ) ) ;
#51372 = DIRECTION ( 'NONE',  ( 0.000000000000000000, 1.000000000000000000, -0.000000000000000000 ) ) ;
#51373 = CARTESIAN_POINT ( 'NONE',  ( 12.63842701281683922, 64.55059781766745175, -9.846743663894590881 ) ) ;
#51374 = CARTESIAN_POINT ( 'NONE',  ( 19.84674366389459266, 28.30059781766745886, 2.638427012816836559 ) ) ;
#51375 = EDGE_CURVE ( 'NONE', #79612, #1475, #43814, .T. ) ;
#51376 = DIRECTION ( 'NONE',  ( -0.4924235601034707144, 0.000000000000000000, 0.8703556959398975890 ) ) ;
#51377 = VERTEX_POINT ( 'NONE', #42319 ) ;
#51378 = CARTESIAN_POINT ( 'NONE',  ( 24.16423886937410614, 44.51208216824730357, -3.795296366450302550 ) ) ;
#51379 = B_SPLINE_SURFACE_WITH_KNOTS ( 'NONE', 3, 1, ( 
 ( #97503, #43480 ),
 ( #67479, #97011 ),
 ( #42509, #4523 ),
 ( #27495, #89485 ),
 ( #57988, #88493 ),
 ( #20996, #51483 ),
 ( #83955, #24451 ),
 ( #44961, #37485 ),
 ( #52954, #46447 ),
 ( #83465, #16449 ),
 ( #22479, #54429 ),
 ( #91944, #46927 ),
 ( #1463, #23475 ),
 ( #14986, #31914 ),
 ( #84938, #77419 ),
 ( #69446, #91455 ),
 ( #45457, #68959 ),
 ( #7485, #53446 ) ),
 .UNSPECIFIED., .F., .F., .F.,
 ( 4, 2, 2, 2, 2, 2, 2, 2, 4 ),
 ( 2, 2 ),
 ( 0.1401766717507622051, 0.2499999999999989453, 0.3749999999999986122, 0.4374999999999986677, 0.4999999999999986677, 0.7499999999999992228, 0.8749999999999996669, 0.9374999999999997780, 1.000000000000000000 ),
 ( 0.000000000000000000, 1.000000000000000000 ),
 .UNSPECIFIED. ) ;
#51380 = CARTESIAN_POINT ( 'NONE',  ( 0.1532563361054082862, 1.217264484334117824, 2.638427012816831674 ) ) ;
#51382 = DIRECTION ( 'NONE',  ( -1.000000000000000000, 0.000000000000000000, 0.000000000000000000 ) ) ;
#51381 = CARTESIAN_POINT ( 'NONE',  ( 12.34086200392826882, -0.03417435944610275333, -7.124999999999971578 ) ) ;
#51383 = CARTESIAN_POINT ( 'NONE',  ( 0.5774900079438590739, 32.64701867748816966, -5.440088680355550821 ) ) ;
#51384 = CARTESIAN_POINT ( 'NONE',  ( 21.09922568453594849, 41.20696800326375353, 6.408140936763242479 ) ) ;
#51385 = EDGE_CURVE ( 'NONE', #5021, #20454, #15311, .T. ) ;
#51386 = CARTESIAN_POINT ( 'NONE',  ( 19.42250999205614548, 10.98035201082150358, -5.440088680355545492 ) ) ;
#51387 = CARTESIAN_POINT ( 'NONE',  ( 22.81628187352647785, 41.41530133659708923, 3.434112377981063169 ) ) ;
#51388 = CARTESIAN_POINT ( 'NONE',  ( 13.43411237798105340, 55.58196800326374643, 12.81628187352647963 ) ) ;
#51389 = VERTEX_POINT ( 'NONE', #73786 ) ;
#51390 = FACE_OUTER_BOUND ( 'NONE', #78480, .T. ) ;
#51391 = CARTESIAN_POINT ( 'NONE',  ( -10.54707717933094813, -44.61285707880912810, -4.000000000000000000 ) ) ;
#51392 = CARTESIAN_POINT ( 'NONE',  ( 6.204703633549690345, 22.84541550158062861, 14.16423886937410082 ) ) ;
#51393 = CARTESIAN_POINT ( 'NONE',  ( -4.164238869374099039, 6.803748834913967869, 8.674139862899312516E-16 ) ) ;
#51394 = CARTESIAN_POINT ( 'NONE',  ( 7.084665262690076126, 12.02201867748817143, -10.88017736071110164 ) ) ;
#51395 = CARTESIAN_POINT ( 'NONE',  ( 17.96484262340118221, 19.93868534415484106, 7.964842623401181321 ) ) ;
#51396 = DIRECTION ( 'NONE',  ( -1.000000000000000000, -0.000000000000000000, -0.000000000000000000 ) ) ;
#51397 = LINE ( 'NONE', #82376, #57569 ) ;
#51398 = CARTESIAN_POINT ( 'NONE',  ( 0.5774900079438590739, 52.64701867748817676, -5.440088680355550821 ) ) ;
#51399 = CARTESIAN_POINT ( 'NONE',  ( 7.084665262690076126, 52.02201867748816255, -10.88017736071110164 ) ) ;
#51400 = CARTESIAN_POINT ( 'NONE',  ( 21.09922568453595559, 17.04030133659708923, -6.408140936763230044 ) ) ;
#51401 = CARTESIAN_POINT ( 'NONE',  ( 6.880000000000009663, 40.99999999999999289, 6.250000000000000000 ) ) ;
#51402 = CARTESIAN_POINT ( 'NONE',  ( 0.000000000000000000, 0.000000000000000000, 0.000000000000000000 ) ) ;
#51403 = CARTESIAN_POINT ( 'NONE',  ( 0.1532563361054083140, 21.00893115100078745, 1.131784320476157264E-15 ) ) ;
#51404 = CARTESIAN_POINT ( 'NONE',  ( 20.88017736071110164, 40.35535201082150536, 2.915334737309930979 ) ) ;
#51405 = CIRCLE ( 'NONE', #53040, 0.2500000000000002220 ) ;
#51406 = CARTESIAN_POINT ( 'NONE',  ( 6.565887622018943937, 15.16530133659708568, 12.81628187352647430 ) ) ;
#51407 = CARTESIAN_POINT ( 'NONE',  ( 2.148416515056676523, 27.23726573380435667, 6.499999999999981348 ) ) ;
#51408 = CARTESIAN_POINT ( 'NONE',  ( 19.84674366389459621, 23.50893115100078390, 7.409399052514197653E-17 ) ) ;
#51409 = CARTESIAN_POINT ( 'NONE',  ( 21.09922568453595559, 47.04030133659708923, -6.408140936763230044 ) ) ;
#51410 = CARTESIAN_POINT ( 'NONE',  ( 7.361572987183170547, 22.05059781766745530, 9.846743663894590881 ) ) ;
#51411 =( BOUNDED_SURFACE ( )  B_SPLINE_SURFACE ( 3, 2, ( 
 ( #33214, #23781, #76754 ),
 ( #48222, #38769, #61740 ),
 ( #24754, #86234, #54247 ),
 ( #1287, #1771, #63709 ),
 ( #24267, #9743, #84759 ),
 ( #94212, #84280, #25743 ),
 ( #31244, #85252, #32228 ),
 ( #9247, #62728, #40244 ) ),
 .UNSPECIFIED., .F., .F., .F. ) 
 B_SPLINE_SURFACE_WITH_KNOTS ( ( 4, 2, 2, 4 ),
 ( 3, 3 ),
 ( 0.000000000000000000, 0.0004516266542298917803, 0.0009032533084597835606, 0.001806506616919567121 ),
 ( 0.000000000000000000, 1.000000000000000000 ),
 .UNSPECIFIED. ) 
 GEOMETRIC_REPRESENTATION_ITEM ( )  RATIONAL_B_SPLINE_SURFACE ( (
 ( 1.000000000000000000, 0.7071067811865475727, 1.000000000000000000),
 ( 1.000000000000000000, 0.7557133596827383393, 1.000000000000000000),
 ( 1.000000000000000000, 0.7976722695483360326, 1.000000000000000000),
 ( 1.000000000000000000, 0.8702934545469085403, 1.000000000000000000),
 ( 1.000000000000000000, 0.9009816261292108441, 1.000000000000000000),
 ( 1.000000000000000000, 0.9749059260391067516, 1.000000000000000000),
 ( 1.000000000000000000, 1.000014990205005949, 1.000000000000000000),
 ( 1.000000000000000000, 1.000000000000000000, 1.000000000000000000) ) ) 
 REPRESENTATION_ITEM ( '' )  SURFACE ( )  );
#51412 = VERTEX_POINT ( 'NONE', #27298 ) ;
#51413 = CARTESIAN_POINT ( 'NONE',  ( 13.64884605730314426, -0.03417435944610275333, -8.341846182955777067 ) ) ;
#51414 = CARTESIAN_POINT ( 'NONE',  ( 10.00000000000000000, 21.81368534415484106, -10.88017736071110342 ) ) ;
#51415 = CARTESIAN_POINT ( 'NONE',  ( 17.08211943468705130, 33.47041550158063927, 12.26659068614894998 ) ) ;
#51416 = CARTESIAN_POINT ( 'NONE',  ( 17.20831665107776587, 29.13393115100078390, -7.208316651077762316 ) ) ;
#51417 = CARTESIAN_POINT ( 'NONE',  ( -0.8801773607111009756, 23.06368534415484106, 1.068504757029289695E-15 ) ) ;
#51418 = CARTESIAN_POINT ( 'NONE',  ( 12.91533473730993009, 16.60535201082150891, -10.88017736071109987 ) ) ;
#51419 = ORIENTED_EDGE ( 'NONE', *, *, #8542, .T. ) ;
#51420 = CARTESIAN_POINT ( 'NONE',  ( 19.42250999205614548, 20.98035201082150891, -5.440088680355545492 ) ) ;
#51421 = CARTESIAN_POINT ( 'NONE',  ( 21.09922568453594849, 46.20696800326376064, 6.408140936763242479 ) ) ;
#51422 = CARTESIAN_POINT ( 'NONE',  ( 12.91533473730992121, 39.52201867748817676, 10.88017736071110164 ) ) ;
#51424 = CARTESIAN_POINT ( 'NONE',  ( 15.44008868035555793, 36.39701867748816966, -9.422509992056140149 ) ) ;
#51423 = CARTESIAN_POINT ( 'NONE',  ( 13.99999999999999822, 60.50000000000000711, -6.000000000000000000 ) ) ;
#51425 = COLOUR_RGB ( '', 0.40784314, 0.44705882, 0.49803922) ;
#51426 = EDGE_LOOP ( 'NONE', ( #34603, #24002, #45503, #66842 ) ) ;
#51427 = CARTESIAN_POINT ( 'NONE',  ( 19.84674366389459621, 53.50893115100078745, 7.409399052514197653E-17 ) ) ;
#51428 = CARTESIAN_POINT ( 'NONE',  ( 7.084665262690076126, 42.02201867748816966, -10.88017736071110164 ) ) ;
#51429 = CARTESIAN_POINT ( 'NONE',  ( 10.00000000000000178, 67.25893115100079456, 9.846743663894594434 ) ) ;
#51430 = CARTESIAN_POINT ( 'NONE',  ( 21.09922568453595559, 62.04030133659709634, -6.408140936763230044 ) ) ;
#51431 = CARTESIAN_POINT ( 'NONE',  ( 32.56412365047463453, 26.99999999999998224, -9.500000000000000000 ) ) ;
#51432 = CARTESIAN_POINT ( 'NONE',  ( -4.164238869374099927, 52.01208216824729647, 3.795296366450308767 ) ) ;
#51433 = CARTESIAN_POINT ( 'NONE',  ( 12.91533473730993009, 51.60535201082149825, -10.88017736071109987 ) ) ;
#51434 = CARTESIAN_POINT ( 'NONE',  ( 0.5600000000000083800, 105.0000000000000000, 5.000000000000000000 ) ) ;
#51435 = CARTESIAN_POINT ( 'NONE',  ( 19.84674366389459266, 43.30059781766744464, 2.638427012816836559 ) ) ;
#51436 = AXIS2_PLACEMENT_3D ( 'NONE', #29791, #60303, #90796 ) ;
#51437 = CARTESIAN_POINT ( 'NONE',  ( 10.00000000000000000, 4.758931151000784787, -9.846743663894594434 ) ) ;
#51438 = CARTESIAN_POINT ( 'NONE',  ( 18.52753015748618282, 23.92559781766745530, -4.923371831947291888 ) ) ;
#51439 = EDGE_LOOP ( 'NONE', ( #93043, #64603, #42440, #63830, #44422, #98315 ) ) ;
#51440 = VECTOR ( 'NONE', #74041, 1000.000000000000000 ) ;
#51441 = CARTESIAN_POINT ( 'NONE',  ( 14.92337183194729988, 19.34226448433411960, -8.527530157486177487 ) ) ;
#51442 = CARTESIAN_POINT ( 'NONE',  ( -6.408140936763232709, -15.04303199673624469, 11.09922568453595026 ) ) ;
#51443 = VECTOR ( 'NONE', #74360, 1000.000000000000000 ) ;
#51444 = CARTESIAN_POINT ( 'NONE',  ( 2.035157376598822676, 32.43868534415483396, -7.964842623401177768 ) ) ;
#51445 = CARTESIAN_POINT ( 'NONE',  ( 18.52753015748618282, 18.92559781766745175, -4.923371831947291888 ) ) ;
#51446 = CARTESIAN_POINT ( 'NONE',  ( 21.09922568453595559, 12.04030133659708746, -6.408140936763230044 ) ) ;
#51448 = CARTESIAN_POINT ( 'NONE',  ( 20.88017736071110164, 50.35535201082151247, 2.915334737309930979 ) ) ;
#51447 = CARTESIAN_POINT ( 'NONE',  ( 15.44008868035555260, 64.73035201082151957, 9.422509992056143702 ) ) ;
#51450 = CARTESIAN_POINT ( 'NONE',  ( 0.6178305044545818747, 53.49863466993041072, -9.382169495545419124 ) ) ;
#51449 = CARTESIAN_POINT ( 'NONE',  ( 4.559911319644449179, 33.89701867748817676, 9.422509992056141925 ) ) ;
#51451 = CARTESIAN_POINT ( 'NONE',  ( 24.16423886937410614, 39.30374883491396787, 8.672049930838204340E-16 ) ) ;
#51452 = CARTESIAN_POINT ( 'NONE',  ( -43.81448451332931882, 106.0682908843177614, 5.149235002859532173 ) ) ;
#51453 = ORIENTED_EDGE ( 'NONE', *, *, #58506, .T. ) ;
#51454 = CARTESIAN_POINT ( 'NONE',  ( 22.81628187352648496, 1.831968003263753753, -3.434112377981050290 ) ) ;
#51455 = CARTESIAN_POINT ( 'NONE',  ( 10.00000000000000178, 14.31368534415483751, 10.88017736071110342 ) ) ;
#51456 = CARTESIAN_POINT ( 'NONE',  ( -0.8801773607110991993, 42.85535201082150536, -2.915334737309923874 ) ) ;
#51457 = CARTESIAN_POINT ( 'NONE',  ( 12.50465990577749409, 56.99999999999999289, 2.900000000000000355 ) ) ;
#51458 = ORIENTED_EDGE ( 'NONE', *, *, #7907, .T. ) ;
#51459 = CARTESIAN_POINT ( 'NONE',  ( 7.361572987183170547, 22.05059781766745530, 9.846743663894590881 ) ) ;
#51460 = CARTESIAN_POINT ( 'NONE',  ( 12.91533473730992121, 64.52201867748817676, 10.88017736071110164 ) ) ;
#51461 = CARTESIAN_POINT ( 'NONE',  ( 5.076628168052704559, 35.17559781766745175, -8.527530157486179263 ) ) ;
#51462 = CARTESIAN_POINT ( 'NONE',  ( 12.63842701281683034, 27.46726448433411250, 9.846743663894596210 ) ) ;
#51463 = CARTESIAN_POINT ( 'NONE',  ( 5.076628168052704559, 10.17559781766745175, -8.527530157486179263 ) ) ;
#51464 = CARTESIAN_POINT ( 'NONE',  ( 14.82269085861167390, 14.49999999999999822, 2.299529454047062327 ) ) ;
#51465 = ADVANCED_FACE ( 'NONE', ( #80311 ), #81295, .T. ) ;
#51467 = DIRECTION ( 'NONE',  ( -0.000000000000000000, -0.000000000000000000, 1.000000000000000000 ) ) ;
#51466 = CARTESIAN_POINT ( 'NONE',  ( 10.00000000000000178, 2.258931151000784787, 9.846743663894594434 ) ) ;
#51468 = CARTESIAN_POINT ( 'NONE',  ( 11.04805072354886875, -95.57913125337492488, 4.000000000000000000 ) ) ;
#51470 = ORIENTED_EDGE ( 'NONE', *, *, #8291, .T. ) ;
#51469 = CARTESIAN_POINT ( 'NONE',  ( 12.63842701281683034, 37.46726448433411605, 9.846743663894596210 ) ) ;
#51471 = CARTESIAN_POINT ( 'NONE',  ( 0.000000000000000000, 0.000000000000000000, 0.000000000000000000 ) ) ;
#51472 = CARTESIAN_POINT ( 'NONE',  ( 0.1532563361054100626, 65.80059781766745175, -2.638427012816831230 ) ) ;
#51473 = CARTESIAN_POINT ( 'NONE',  ( -0.8801773607110991993, 2.855352010821504471, -2.915334737309923874 ) ) ;
#51474 = CARTESIAN_POINT ( 'NONE',  ( 10.00000000000000178, 23.05374883491397142, 14.16423886937410082 ) ) ;
#51475 = UNCERTAINTY_MEASURE_WITH_UNIT (LENGTH_MEASURE( 1.000000000000000082E-05 ), #67841, 'distance_accuracy_value', 'NONE');
#51476 = CARTESIAN_POINT ( 'NONE',  ( 11.49638213510176499, 0.04922511925147023820, 9.245501498402024509 ) ) ;
#51477 = CARTESIAN_POINT ( 'NONE',  ( 6.204703633549690345, 22.84541550158062861, 14.16423886937410082 ) ) ;
#51478 = CARTESIAN_POINT ( 'NONE',  ( 24.16423886937410614, 39.51208216824731068, -3.795296366450302550 ) ) ;
#51479 = CARTESIAN_POINT ( 'NONE',  ( 6.204703633549690345, 10.76208216824729824, -14.16423886937410259 ) ) ;
#51481 = FACE_BOUND ( 'NONE', #95591, .T. ) ;
#51480 = CARTESIAN_POINT ( 'NONE',  ( 13.79529636645030344, 8.262082168247300018, 14.16423886937410614 ) ) ;
#51482 = CARTESIAN_POINT ( 'NONE',  ( 2.035157376598824452, 53.68868534415484817, 7.964842623401179544 ) ) ;
#51483 = CARTESIAN_POINT ( 'NONE',  ( 6.732888861736110009, -58.30752899003807954, -3.750000000000000888 ) ) ;
#51484 = ORIENTED_EDGE ( 'NONE', *, *, #47080, .F. ) ;
#51485 = CARTESIAN_POINT ( 'NONE',  ( 1.472469842513823179, 30.59226448433411960, -4.923371831947296329 ) ) ;
#51487 = CARTESIAN_POINT ( 'NONE',  ( 5.076628168052703671, 31.84226448433412315, 8.527530157486179263 ) ) ;
#51486 = CARTESIAN_POINT ( 'NONE',  ( 5.240416992896808068, 0.04922511925147525502, -13.79072622793301761 ) ) ;
#51488 = CARTESIAN_POINT ( 'NONE',  ( 20.88017736071110519, 10.56368534415483929, 2.639326808657452039E-16 ) ) ;
#51489 = CARTESIAN_POINT ( 'NONE',  ( -1.099225684535947600, 58.70696800326375353, -6.408140936763238038 ) ) ;
#51490 = CARTESIAN_POINT ( 'NONE',  ( 1.472469842513823179, 50.59226448433411605, -4.923371831947296329 ) ) ;
#51491 = CARTESIAN_POINT ( 'NONE',  ( 8.630000000000000782, 1.085138116723527427E-15, 3.750000000000000000 ) ) ;
#51492 = CARTESIAN_POINT ( 'NONE',  ( 19.84674366389459266, 33.30059781766744464, 2.638427012816836559 ) ) ;
#51493 = CARTESIAN_POINT ( 'NONE',  ( 22.81628187352647785, 36.41530133659707502, 3.434112377981063169 ) ) ;
#51494 = CARTESIAN_POINT ( 'NONE',  ( 3.795296366450306547, -19.65458449841936428, -14.16423886937410259 ) ) ;
#51495 = CARTESIAN_POINT ( 'NONE',  ( -0.8801773607110991993, 47.85535201082150536, -2.915334737309923874 ) ) ;
#51496 = CARTESIAN_POINT ( 'NONE',  ( 19.84674366389459621, 33.50893115100078745, 7.409399052514197653E-17 ) ) ;
#51497 = CARTESIAN_POINT ( 'NONE',  ( 13.79529636645030344, 23.26208216824730002, 14.16423886937410614 ) ) ;
#51498 = EDGE_CURVE ( 'NONE', #63997, #30159, #16288, .T. ) ;
#51499 = ORIENTED_EDGE ( 'NONE', *, *, #63790, .F. ) ;
#51500 = DIRECTION ( 'NONE',  ( -0.08715574274765112983, -0.9961946980917461003, -0.000000000000000000 ) ) ;
#51501 = CARTESIAN_POINT ( 'NONE',  ( 20.88017736071110164, 50.35535201082151247, 2.915334737309930979 ) ) ;
#51502 = CARTESIAN_POINT ( 'NONE',  ( 10.93781366033343083, 14.49999999999999112, 10.26470809774079029 ) ) ;
#51503 = CARTESIAN_POINT ( 'NONE',  ( -4.164238869374099039, 51.80374883491396787, 8.674139862899312516E-16 ) ) ;
#51504 = CARTESIAN_POINT ( 'NONE',  ( -1.099225684535947600, -1.293031996736246469, -6.408140936763238038 ) ) ;
#51505 =( GEOMETRIC_REPRESENTATION_CONTEXT ( 3 ) GLOBAL_UNCERTAINTY_ASSIGNED_CONTEXT ( ( #6282 ) ) GLOBAL_UNIT_ASSIGNED_CONTEXT ( ( #74854, #66356, #51366 ) ) REPRESENTATION_CONTEXT ( 'NONE', 'WORKASPACE' ) );
#51506 = CARTESIAN_POINT ( 'NONE',  ( 0.000000000000000000, 0.5000000000000004441, 0.000000000000000000 ) ) ;
#51507 = CARTESIAN_POINT ( 'NONE',  ( 17.96484262340118221, 49.93868534415484106, 7.964842623401181321 ) ) ;
#51508 = CARTESIAN_POINT ( 'NONE',  ( -0.04068437667224029941, 27.21974360917721114, -6.396802510829693311 ) ) ;
#51509 = CARTESIAN_POINT ( 'NONE',  ( 21.09922568453594849, 21.20696800326375353, 6.408140936763242479 ) ) ;
#51510 = CARTESIAN_POINT ( 'NONE',  ( 0.6178305044545818747, 3.498634669930420049, -9.382169495545419124 ) ) ;
#51511 = LINE ( 'NONE', #82003, #85459 ) ;
#51512 = CARTESIAN_POINT ( 'NONE',  ( 15.44008868035555260, 19.73035201082150536, 9.422509992056143702 ) ) ;
#51513 = CARTESIAN_POINT ( 'NONE',  ( 4.559911319644449179, 8.897018677488173211, 9.422509992056141925 ) ) ;
#51514 = CARTESIAN_POINT ( 'NONE',  ( 0.1532563361054082862, 46.21726448433411605, 2.638427012816831674 ) ) ;
#51515 = CARTESIAN_POINT ( 'NONE',  ( -14.43063482171897149, -2.270048298641522937E-16, 2.386446184882927035 ) ) ;
#51516 = EDGE_LOOP ( 'NONE', ( #9764, #25959, #65414, #77359, #51317, #39178 ) ) ;
#51517 = CARTESIAN_POINT ( 'NONE',  ( 2.035157376598824452, 3.688685344154837953, 7.964842623401179544 ) ) ;
#51518 = CARTESIAN_POINT ( 'NONE',  ( -1.099225684535947600, 3.706968003263753531, -6.408140936763238038 ) ) ;
#51519 = SURFACE_STYLE_FILL_AREA ( #21028 ) ;
#51520 = VECTOR ( 'NONE', #80266, 1000.000000000000000 ) ;
#51521 = CARTESIAN_POINT ( 'NONE',  ( 0.1532563361054100626, 15.80059781766745353, -2.638427012816831230 ) ) ;
#51522 = CARTESIAN_POINT ( 'NONE',  ( 1.472469842513823179, 35.59226448433412315, -4.923371831947296329 ) ) ;
#51523 = CARTESIAN_POINT ( 'NONE',  ( 12.91533473730993009, 41.60535201082149825, -10.88017736071109987 ) ) ;
#51524 = CARTESIAN_POINT ( 'NONE',  ( 16.40814093676324603, 12.45696800326375353, -11.09922568453594671 ) ) ;
#51526 = CARTESIAN_POINT ( 'NONE',  ( 5.129999999999995453, 43.00000000000000000, -6.500000000000000888 ) ) ;
#51525 = CARTESIAN_POINT ( 'NONE',  ( 12.91533473730992121, 54.52201867748816255, 10.88017736071110164 ) ) ;
#51527 = DIRECTION ( 'NONE',  ( -3.819167204710539130E-14, 0.000000000000000000, 1.000000000000000000 ) ) ;
#51528 = CARTESIAN_POINT ( 'NONE',  ( 10.00000000000000178, 50.37363466993042493, 12.81628187352647608 ) ) ;
#51529 = ORIENTED_EDGE ( 'NONE', *, *, #66975, .F. ) ;
#51530 = CARTESIAN_POINT ( 'NONE',  ( 15.44008868035555260, 64.73035201082151957, 9.422509992056143702 ) ) ;
#51532 = CARTESIAN_POINT ( 'NONE',  ( 6.204703633549690345, 0.7620821682473009062, -14.16423886937410259 ) ) ;
#51531 = CARTESIAN_POINT ( 'NONE',  ( 21.09922568453594849, 36.20696800326375353, 6.408140936763242479 ) ) ;
#51533 = CARTESIAN_POINT ( 'NONE',  ( 2.791683348922240793, 1.633931151000784565, 7.208316651077764092 ) ) ;
#51534 = CARTESIAN_POINT ( 'NONE',  ( -0.8801773607111008646, 43.27201867748817676, 2.915334737309923430 ) ) ;
#51535 = CARTESIAN_POINT ( 'NONE',  ( 1.472469842513823179, 61.42559781766745175, 4.923371831947296329 ) ) ;
#51536 = AXIS2_PLACEMENT_3D ( 'NONE', #73528, #21539, #50054 ) ;
#51537 = CARTESIAN_POINT ( 'NONE',  ( 12.63842701281683922, 59.55059781766744464, -9.846743663894590881 ) ) ;
#51538 = CARTESIAN_POINT ( 'NONE',  ( 2.791683348922237240, 15.38393115100078212, -7.208316651077763204 ) ) ;
#51539 = EDGE_CURVE ( 'NONE', #97117, #83990, #83945, .T. ) ;
#51540 = CARTESIAN_POINT ( 'NONE',  ( 10.00000000000000000, 61.81368534415484106, -10.88017736071110342 ) ) ;
#51541 = CARTESIAN_POINT ( 'NONE',  ( -7.750000000000000000, 79.82179676972448590, -6.250000000000000000 ) ) ;
#51542 = CARTESIAN_POINT ( 'NONE',  ( -4.164238869374098151, 26.59541550158063217, -3.795296366450310543 ) ) ;
#51543 = FACE_OUTER_BOUND ( 'NONE', #57009, .T. ) ;
#51544 = EDGE_CURVE ( 'NONE', #92036, #65098, #69385, .T. ) ;
#51545 = CARTESIAN_POINT ( 'NONE',  ( 11.10711265426551897, -52.69644047981464041, -3.750000000000001776 ) ) ;
#51546 = CARTESIAN_POINT ( 'NONE',  ( -4.182615635448454938, 26.60017725333986149, 9.500000000000000000 ) ) ;
#51547 = ORIENTED_EDGE ( 'NONE', *, *, #6464, .F. ) ;
#51548 = VECTOR ( 'NONE', #35207, 1000.000000000000000 ) ;
#51549 = CARTESIAN_POINT ( 'NONE',  ( 22.26659068614894466, 58.88708216824729647, 7.082119434687054849 ) ) ;
#51550 = CARTESIAN_POINT ( 'NONE',  ( 24.16423886937409904, 59.09541550158063217, 3.795296366450317205 ) ) ;
#51551 = CARTESIAN_POINT ( 'NONE',  ( 7.361572987183169658, 34.96726448433411605, -9.846743663894592657 ) ) ;
#51552 = B_SPLINE_CURVE_WITH_KNOTS ( 'NONE', 3,
 ( #65743, #58229, #20754, #65244, #27746, #88749, #20259, #51243, #81247, #57751, #95770, #34249, #12746, #97267, #35747, #66235, #81730, #13245 ),
 .UNSPECIFIED., .F., .F.,
 ( 4, 2, 2, 2, 2, 2, 2, 2, 4 ),
 ( 1.551583845779545699E-17, 0.0005964982550586688404, 0.001192996510117322285, 0.002385993020234661918, 0.003578989530352000899, 0.004771986040469341182, 0.007157979060703985319, 0.008350975570821308688, 0.009543972080938632058 ),
 .UNSPECIFIED. ) ;
#51553 = CARTESIAN_POINT ( 'NONE',  ( 22.81628187352647785, 31.62363466993042138, 6.195893100308588602E-16 ) ) ;
#51554 = SURFACE_STYLE_FILL_AREA ( #90522 ) ;
#51555 =( LENGTH_UNIT ( ) NAMED_UNIT ( * ) SI_UNIT ( .MILLI., .METRE. ) );
#51556 = CARTESIAN_POINT ( 'NONE',  ( 17.96484262340118221, 9.938685344154837509, 7.964842623401181321 ) ) ;
#51557 = CARTESIAN_POINT ( 'NONE',  ( 10.00000000000000000, 60.55374883491397497, -14.16423886937410082 ) ) ;
#51558 = CARTESIAN_POINT ( 'NONE',  ( 0.1532563361054083140, 26.00893115100078745, 1.131784320476157264E-15 ) ) ;
#51559 = B_SPLINE_CURVE_WITH_KNOTS ( 'NONE', 3,
 ( #57715, #58706, #88216, #19723, #50213, #12219 ),
 .UNSPECIFIED., .F., .F.,
 ( 4, 2, 4 ),
 ( 3.409110551494643978E-05, 0.0004400426677367937273, 0.0008459942299586410827 ),
 .UNSPECIFIED. ) ;
#51560 = CARTESIAN_POINT ( 'NONE',  ( -13.21236992757677164, 15.00000000000000000, 5.338143956176621074 ) ) ;
#51561 = CARTESIAN_POINT ( 'NONE',  ( 7.361572987183169658, 9.967264484334119601, -9.846743663894592657 ) ) ;
#51562 = EDGE_CURVE ( 'NONE', #53168, #42200, #96147, .T. ) ;
#51563 = CARTESIAN_POINT ( 'NONE',  ( 38.04706783004212411, -2.213315012455880539E-15, -7.000000000000000000 ) ) ;
#51564 = CARTESIAN_POINT ( 'NONE',  ( -9.846743663894596210, 15.80059781766745353, -2.638427012816824124 ) ) ;
#51565 = ORIENTED_EDGE ( 'NONE', *, *, #46291, .F. ) ;
#51566 = ORIENTED_EDGE ( 'NONE', *, *, #6348, .F. ) ;
#51567 = LINE ( 'NONE', #38056, #43005 ) ;
#51568 = VERTEX_POINT ( 'NONE', #65787 ) ;
#51569 = CARTESIAN_POINT ( 'NONE',  ( 0.1532563361054082862, 41.21726448433411605, 2.638427012816831674 ) ) ;
#51570 = CARTESIAN_POINT ( 'NONE',  ( -4.164238869374098151, 16.59541550158063927, -3.795296366450310543 ) ) ;
#51572 = CARTESIAN_POINT ( 'NONE',  ( 19.42250999205614193, 25.14701867748817321, 5.440088680355555262 ) ) ;
#51571 = CARTESIAN_POINT ( 'NONE',  ( 19.42250999205614193, 25.14701867748817321, 5.440088680355555262 ) ) ;
#51574 = CARTESIAN_POINT ( 'NONE',  ( 21.09922568453595559, 22.04030133659708923, -6.408140936763230044 ) ) ;
#51573 = CARTESIAN_POINT ( 'NONE',  ( 19.84674366389459266, 58.71726448433411605, -2.638427012816827677 ) ) ;
#51575 = CARTESIAN_POINT ( 'NONE',  ( 13.79529636645031943, 5.345415501580634832, -14.16423886937409904 ) ) ;
#51576 = CARTESIAN_POINT ( 'NONE',  ( 13.43411237798105340, 35.58196800326375353, 12.81628187352647963 ) ) ;
#51577 = ORIENTED_EDGE ( 'NONE', *, *, #14714, .T. ) ;
#51578 = CARTESIAN_POINT ( 'NONE',  ( 2.791683348922237240, 30.38393115100078390, -7.208316651077763204 ) ) ;
#51579 = MECHANICAL_DESIGN_GEOMETRIC_PRESENTATION_REPRESENTATION (  '', ( #19596 ), #51505 ) ;
#51580 = CARTESIAN_POINT ( 'NONE',  ( 17.96484262340118221, 4.938685344154837509, 7.964842623401181321 ) ) ;
#51581 = VERTEX_POINT ( 'NONE', #27795 ) ;
#51582 = CIRCLE ( 'NONE', #83564, 2.999999999999999112 ) ;
#51583 = CARTESIAN_POINT ( 'NONE',  ( -2.266590686148945544, 67.22041550158063217, 7.082119434687048631 ) ) ;
#51584 = EDGE_LOOP ( 'NONE', ( #28760, #54857, #80677, #49084 ) ) ;
#51585 = CARTESIAN_POINT ( 'NONE',  ( 7.084665262690076126, 47.02201867748818387, -10.88017736071110164 ) ) ;
#51586 = CARTESIAN_POINT ( 'NONE',  ( 4.559911319644449179, 63.89701867748817676, 9.422509992056141925 ) ) ;
#51587 = CARTESIAN_POINT ( 'NONE',  ( 12.91533473730993009, 56.60535201082151247, -10.88017736071109987 ) ) ;
#51588 = PRESENTATION_LAYER_ASSIGNMENT (  '', '', ( #77132 ) ) ;
#51589 =( NAMED_UNIT ( * ) PLANE_ANGLE_UNIT ( ) SI_UNIT ( $, .RADIAN. ) );
#51590 = B_SPLINE_CURVE_WITH_KNOTS ( 'NONE', 3,
 ( #37041, #36549, #44528, #98559, #61007, #91008 ),
 .UNSPECIFIED., .F., .F.,
 ( 4, 2, 4 ),
 ( 0.0002800858945027140997, 0.0006862919646584248693, 0.001092498034814135639 ),
 .UNSPECIFIED. ) ;
#51591 = CARTESIAN_POINT ( 'NONE',  ( 2.035157376598824452, 58.68868534415482685, 7.964842623401179544 ) ) ;
#51592 = CARTESIAN_POINT ( 'NONE',  ( 19.72487221294570858, 70.00000000000000000, -6.000000000000000000 ) ) ;
#51593 = EDGE_CURVE ( 'NONE', #16419, #53779, #91723, .T. ) ;
#51595 = ORIENTED_EDGE ( 'NONE', *, *, #90184, .T. ) ;
#51594 = DIRECTION ( 'NONE',  ( -0.000000000000000000, -0.000000000000000000, -1.000000000000000000 ) ) ;
#51596 = CARTESIAN_POINT ( 'NONE',  ( 12.63842701281683922, 24.55059781766745175, -9.846743663894590881 ) ) ;
#51597 = ORIENTED_EDGE ( 'NONE', *, *, #31761, .T. ) ;
#51598 = CARTESIAN_POINT ( 'NONE',  ( 14.92337183194729633, 57.67559781766745886, 8.527530157486181039 ) ) ;
#51599 = ADVANCED_FACE ( 'NONE', ( #87316 ), #89778, .T. ) ;
#51600 = LINE ( 'NONE', #66595, #6970 ) ;
#51601 = CARTESIAN_POINT ( 'NONE',  ( 20.36894250292379738, 9.928748834913966093, -10.36894250292379027 ) ) ;
#51602 = EDGE_LOOP ( 'NONE', ( #64540, #19480, #780, #49440 ) ) ;
#51603 = FACE_OUTER_BOUND ( 'NONE', #94228, .T. ) ;
#51604 = CARTESIAN_POINT ( 'NONE',  ( -5.329638162525626832, -28.67157456369669788, 3.750000000000001332 ) ) ;
#51605 = CARTESIAN_POINT ( 'NONE',  ( 10.00000000000000178, 37.25893115100078745, 9.846743663894594434 ) ) ;
#51606 = CARTESIAN_POINT ( 'NONE',  ( 10.00000000000000178, 68.05374883491397497, 14.16423886937410082 ) ) ;
#51607 = CARTESIAN_POINT ( 'NONE',  ( 14.47650479471822216, 0.5000000000000004441, -3.928206833722012625 ) ) ;
#51608 = ORIENTED_EDGE ( 'NONE', *, *, #44718, .F. ) ;
#51609 =( BOUNDED_SURFACE ( )  B_SPLINE_SURFACE ( 3, 2, ( 
 ( #41163, #26143, #9667 ),
 ( #25664, #70669, #95620 ),
 ( #25182, #18643, #11133 ),
 ( #94136, #27109, #64604 ) ),
 .UNSPECIFIED., .F., .F., .F. ) 
 B_SPLINE_SURFACE_WITH_KNOTS ( ( 4, 4 ),
 ( 3, 3 ),
 ( -2.168404344971008868E-19, 0.0006068291151710580476 ),
 ( 0.000000000000000000, 1.000000000000000000 ),
 .UNSPECIFIED. ) 
 GEOMETRIC_REPRESENTATION_ITEM ( )  RATIONAL_B_SPLINE_SURFACE ( (
 ( 1.000000000000000000, 0.8414823709351009207, 1.000000000000000000),
 ( 1.000000000000000000, 0.8336435218270028535, 1.000000000000000000),
 ( 1.000000000000000000, 0.8260591074388748956, 1.000000000000000000),
 ( 1.000000000000000000, 0.8188293140827598293, 1.000000000000000000) ) ) 
 REPRESENTATION_ITEM ( '' )  SURFACE ( )  );
#51610 = DIRECTION ( 'NONE',  ( 0.000000000000000000, 1.000000000000000000, -1.734723475976805517E-15 ) ) ;
#51611 = CARTESIAN_POINT ( 'NONE',  ( 5.076628168052704559, 45.17559781766745175, -8.527530157486179263 ) ) ;
#51612 = CARTESIAN_POINT ( 'NONE',  ( 0.2751277870542967463, 70.00000000000000000, -6.000000000000000000 ) ) ;
#51613 = CARTESIAN_POINT ( 'NONE',  ( -2.816281873526473856, 19.12363466993042138, 9.499525473075851096E-16 ) ) ;
#51614 = CARTESIAN_POINT ( 'NONE',  ( 0.1532563361054083140, 11.00893115100078568, 1.131784320476157264E-15 ) ) ;
#51615 = CARTESIAN_POINT ( 'NONE',  ( 2.603489959281614308, 36.58210964143329136, 6.500000000000031086 ) ) ;
#51616 = CARTESIAN_POINT ( 'NONE',  ( 14.92337183194729633, 17.67559781766745175, 8.527530157486181039 ) ) ;
#51617 = CARTESIAN_POINT ( 'NONE',  ( 3.591859063236761518, -0.04303199673624671928, 11.09922568453594849 ) ) ;
#51618 =( BOUNDED_SURFACE ( )  B_SPLINE_SURFACE ( 1, 2, ( 
 ( #75363, #92828, #53351, #84368, #76358, #68376, #69848, #7873, #61834, #77327, #6878, #31824, #37882, #14890, #31334, #23867, #46352, #62321, #30347, #98895, #16352, #24357, #45359, #76840, #83859, #82874, #14388, #7386, #37389, #8354, #38862, #69351, #60854, #67879, #54330, #84845, #98400, #29856, #90854, #91353, #22880, #10323, #72283, #16845, #34269, #55827, #64281, #40825, #17345, #56795, #56318, #24842, #25821, #32317, #2844, #71325, #87290, #33298, #18810, #47319, #71806, #93320, #63789, #77819, #3311, #3813, #86814, #10815, #9334, #18318, #62821, #48307, #32808, #17826, #55324, #9835, #49293, #85830, #47815, #94793, #33774, #63304, #78815, #78315, #64771, #94298, #48798, #95285, #79307, #39836, #41334, #2352, #11296, #54820, #26295, #40336, #79794, #41816, #85331, #70342, #1860, #70839, #93813, #25343, #86321, #73271, #36769, #28759, #89265, #11787, #20280, #28266, #20776, #5291, #6264, #97285, #67261, #43757, #19778, #59251, #96790, #35768, #80287, #65765, #44252, #74246, #34777, #4303, #88769, #50777, #5778, #65263, #81269, #12769, #58761, #12279, #95792, #89751, #43265, #21268, #73760, #27273, #58253, #13265, #74755, #66762, #26786, #66256, #51765, #57284, #72767, #88277, #36267, #42295, #51267, #81751, #82249, #13764, #87778, #19294, #49781, #57772, #50266, #96292, #80782, #42786, #4792, #35269, #27769, #76726, #38742, #52254, #45245, #91738, #37274, #76245, #29251, #23259, #46240, #92228, #29737, #75741, #54214, #764, #60247, #68746, #22758, #6760, #7263, #16237, #77217, #37764, #68261, #69243, #31217, #90740, #8245, #90244, #21775, #67763, #61712, #98781, #46717, #23754, #30229, #60733, #84731, #53734, #15268, #8722, #39240, #91234, #97788, #61232, #59747, #7761, #53240, #45749, #15755, #22268, #83745, #38254, #278, #82750, #30725, #83250, #98282, #14271, #84253, #44745, #75248, #52741, #14772, #25231, #63678, #17718, #49180, #62205, #70720, #10700, #17230, #78201, #62698, #26190, #40705, #9713, #24237, #39730, #70224, #56682, #40213, #2731, #55710, #94183, #48191, #79681, #92711, #2236, #41214, #47707, #32694, #93199, #87173, #71209, #63191, #54704, #1743, #32197, #18696, #85225, #93696, #11179, #86698, #77706, #47205, #86207, #78704, #18204, #9218, #10213, #33186, #25712, #55201, #24725, #71692, #56205, #64164, #48683, #85715, #79186, #3204, #69728, #33667, #1255, #94682, #31710, #16728, #87661, #4185, #58646, #95163, #73145, #20155, #81147, #13143, #81635, #59129, #73637, #58138, #72650, #80666, #42186, #4682, #19175, #57657, #80165, #20655, #43640, #26669, #88155, #35651, #11676, #50658, #72170, #66137 ),
 ( #34656, #74125, #89144, #50157, #35145, #65151, #21149, #65644, #5165, #82130, #96168, #34158, #43149, #19668, #97172, #89638, #12651, #95670, #27651, #5662, #96669, #51150, #28149, #36144, #27156, #66648, #28639, #12161, #51650, #41699, #3697, #57164, #88647, #64650, #49655, #42666, #92106, #84125, #54096, #30604, #6633, #15637, #83627, #22638, #46120, #37638, #8124, #60616, #82631, #45116, #155, #31099, #53608, #61593, #75624, #38618, #13639, #59628, #75127, #61109, #67136, #7136, #91115, #53119, #76607, #69119, #23637, #45621, #30110, #44631, #52624, #14147, #68135, #90123, #29612, #52136, #91618, #650, #97660, #60117, #7647, #37149, #15143, #44124, #38138, #23135, #74634, #67645, #90616, #6146, #36648, #98154, #76118, #98662, #21651, #22140, #29127, #83125, #14652, #68625, #56088, #86580, #77583, #94074, #77097, #8609, #24116, #63566, #93081, #3098, #10579, #62577, #55078, #41089, #40592, #2121, #71586, #33552, #24611, #84611, #48070, #64050, #93577, #85597, #32580, #2615, #47087, #17111, #47594, #9591, #33070, #63076, #70102, #54585, #16113, #78088, #94562, #40095, #70595, #17600, #25112, #78583, #55594, #26080, #39117, #86089, #25595, #32076, #10094, #9099, #46598, #71089, #18089, #69607, #85100, #16609, #1128, #31590, #48564, #62085, #79065, #92592, #39613, #1627, #80551, #73523, #95047, #12047, #19552, #88537, #42075, #26554, #97056, #5051, #49542, #58525, #27537, #65530, #35534, #57051, #89033, #50048, #42548, #20039, #18575, #66529, #27043, #35028, #73032, #72536, #43524, #4566, #66027, #51029, #49068, #5549, #11555, #87553, #96555, #28030, #96053, #74020, #4070, #34533, #20544, #81522, #19063, #58030, #57541, #56574, #87065, #80052, #79571, #50541, #81035, #12542, #65027, #13030, #43043, #36027, #11070, #41591, #72058, #3585, #95554, #34043, #64539, #88040, #8011, #29498, #38020, #83016, #90013, #30492, #29998, #97548, #98546, #6037, #75509, #14533, #60991, #45004, #91502, #89529, #45502, #67026, #7023, #21038, #76002, #76498, #60505, #83512, #51528, #90995, #36537, #22035, #6519, #90500, #29010, #82519, #23022, #59519, #21533, #68513, #7530, #37029, #52509, #52026, #38509, #37529, #22525, #69007, #68019, #82020, #52998, #75014, #84003, #28529, #15030, #14036, #43, #53493, #15527, #46008, #59023, #13531, #44515, #44014, #74517, #67525, #98042, #60006, #62962, #84499, #92966, #2002, #93467, #77970, #78954, #70980, #85482, #39001, #63458, #24498, #39980, #85978, #24994, #32467, #47470, #69496, #54960, #17971, #61484, #10465, #1514, #9978, #16991, #61977, #2501, #55477, #1012, #70481, #76985, #9477, #17489 ) ),
 .UNSPECIFIED., .F., .F., .F. ) 
 B_SPLINE_SURFACE_WITH_KNOTS ( ( 2, 2 ),
 ( 3, 2, 2, 2, 2, 2, 2, 2, 2, 2, 2, 2, 2, 2, 2, 2, 2, 2, 2, 2, 2, 2, 2, 2, 2, 2, 2, 2, 2, 2, 2, 2, 2, 2, 2, 2, 2, 2, 2, 2, 2, 2, 2, 2, 2, 2, 2, 2, 2, 2, 2, 2, 2, 2, 2, 2, 2, 2, 2, 2, 2, 2, 2, 2, 2, 2, 2, 2, 2, 2, 2, 2, 2, 2, 2, 2, 2, 2, 2, 2, 2, 2, 2, 2, 2, 2, 2, 2, 2, 2, 2, 2, 2, 2, 2, 2, 2, 2, 2, 2, 2, 2, 2, 2, 2, 2, 2, 2, 2, 2, 2, 2, 2, 2, 2, 2, 2, 2, 2, 2, 2, 2, 2, 2, 2, 2, 2, 2, 2, 2, 2, 2, 2, 2, 2, 2, 2, 2, 2, 2, 2, 2, 2, 2, 2, 2, 2, 2, 2, 2, 2, 2, 2, 2, 2, 2, 2, 2, 2, 2, 2, 2, 3 ),
 ( 0.000000000000000000, 1.000000000000000000 ),
 ( 0.000000000000000000, 0.005952380952380952051, 0.01190476190476190410, 0.01785714285714285615, 0.02380952380952380820, 0.02976190476190476025, 0.03571428571428571230, 0.04166666666666666435, 0.04761904761904761640, 0.05357142857142856845, 0.05952380952380952051, 0.06547619047619047949, 0.07142857142857142461, 0.07738095238095238360, 0.08333333333333332871, 0.08928571428571428770, 0.09523809523809523281, 0.1011904761904761918, 0.1071428571428571369, 0.1130952380952380959, 0.1190476190476190410, 0.1250000000000000000, 0.1309523809523809590, 0.1369047619047619180, 0.1428571428571428492, 0.1488095238095238082, 0.1547619047619047672, 0.1607142857142857262, 0.1666666666666666574, 0.1726190476190476164, 0.1785714285714285754, 0.1845238095238095344, 0.1904761904761904656, 0.1964285714285714246, 0.2023809523809523836, 0.2083333333333333426, 0.2142857142857142738, 0.2202380952380952328, 0.2261904761904761918, 0.2321428571428571508, 0.2380952380952380820, 0.2440476190476190410, 0.2500000000000000000, 0.2559523809523809312, 0.2619047619047619180, 0.2678571428571428492, 0.2738095238095238360, 0.2797619047619047672, 0.2857142857142856984, 0.2916666666666666852, 0.2976190476190476164, 0.3035714285714285476, 0.3095238095238095344, 0.3154761904761904656, 0.3214285714285714524, 0.3273809523809523836, 0.3333333333333333148, 0.3392857142857143016, 0.3452380952380952328, 0.3511904761904761640, 0.3571428571428571508, 0.3630952380952380820, 0.3690476190476190688, 0.3750000000000000000, 0.3809523809523809312, 0.3869047619047619180, 0.3928571428571428492, 0.3988095238095238360, 0.4047619047619047672, 0.4107142857142856984, 0.4166666666666666852, 0.4226190476190476164, 0.4285714285714285476, 0.4345238095238095344, 0.4404761904761904656, 0.4464285714285714524, 0.4523809523809523836, 0.4583333333333333148, 0.4642857142857143016, 0.4702380952380952328, 0.4761904761904761640, 0.4821428571428571508, 0.4880952380952380820, 0.4940476190476190688, 0.5000000000000000000, 0.5059523809523809312, 0.5119047619047618625, 0.5178571428571429047, 0.5238095238095238360, 0.5297619047619047672, 0.5357142857142856984, 0.5416666666666666297, 0.5476190476190476719, 0.5535714285714286031, 0.5595238095238095344, 0.5654761904761904656, 0.5714285714285713969, 0.5773809523809523281, 0.5833333333333333703, 0.5892857142857143016, 0.5952380952380952328, 0.6011904761904761640, 0.6071428571428570953, 0.6130952380952381375, 0.6190476190476190688, 0.6250000000000000000, 0.6309523809523809312, 0.6369047619047618625, 0.6428571428571429047, 0.6488095238095238360, 0.6547619047619047672, 0.6607142857142856984, 0.6666666666666666297, 0.6726190476190476719, 0.6785714285714286031, 0.6845238095238095344, 0.6904761904761904656, 0.6964285714285713969, 0.7023809523809523281, 0.7083333333333333703, 0.7142857142857143016, 0.7202380952380952328, 0.7261904761904761640, 0.7321428571428570953, 0.7380952380952381375, 0.7440476190476190688, 0.7500000000000000000, 0.7559523809523809312, 0.7619047619047618625, 0.7678571428571429047, 0.7738095238095238360, 0.7797619047619047672, 0.7857142857142856984, 0.7916666666666666297, 0.7976190476190476719, 0.8035714285714286031, 0.8095238095238095344, 0.8154761904761904656, 0.8214285714285713969, 0.8273809523809523281, 0.8333333333333333703, 0.8392857142857143016, 0.8452380952380952328, 0.8511904761904761640, 0.8571428571428570953, 0.8630952380952381375, 0.8690476190476190688, 0.8750000000000000000, 0.8809523809523809312, 0.8869047619047618625, 0.8928571428571429047, 0.8988095238095238360, 0.9047619047619047672, 0.9107142857142856984, 0.9166666666666666297, 0.9226190476190476719, 0.9285714285714286031, 0.9345238095238095344, 0.9404761904761904656, 0.9464285714285713969, 0.9523809523809523281, 0.9583333333333333703, 0.9642857142857143016 ),
 .UNSPECIFIED. ) 
 GEOMETRIC_REPRESENTATION_ITEM ( )  RATIONAL_B_SPLINE_SURFACE ( (
 ( 1.000000000000000000, 0.9659258262890683122, 1.000000000000000000, 0.9659258262890683122, 1.000000000000000000, 0.9659258262890683122, 1.000000000000000000, 0.9659258262890683122, 1.000000000000000000, 0.9659258262890683122, 1.000000000000000000, 0.9659258262890683122, 1.000000000000000000, 0.9659258262890683122, 1.000000000000000000, 0.9659258262890683122, 1.000000000000000000, 0.9659258262890683122, 1.000000000000000000, 0.9659258262890683122, 1.000000000000000000, 0.9659258262890683122, 1.000000000000000000, 0.9659258262890683122, 1.000000000000000000, 0.9659258262890683122, 1.000000000000000000, 0.9659258262890683122, 1.000000000000000000, 0.9659258262890683122, 1.000000000000000000, 0.9659258262890683122, 1.000000000000000000, 0.9659258262890683122, 1.000000000000000000, 0.9659258262890683122, 1.000000000000000000, 0.9659258262890683122, 1.000000000000000000, 0.9659258262890683122, 1.000000000000000000, 0.9659258262890683122, 1.000000000000000000, 0.9659258262890683122, 1.000000000000000000, 0.9659258262890683122, 1.000000000000000000, 0.9659258262890683122, 1.000000000000000000, 0.9659258262890683122, 1.000000000000000000, 0.9659258262890683122, 1.000000000000000000, 0.9659258262890683122, 1.000000000000000000, 0.9659258262890683122, 1.000000000000000000, 0.9659258262890683122, 1.000000000000000000, 0.9659258262890683122, 1.000000000000000000, 0.9659258262890683122, 1.000000000000000000, 0.9659258262890683122, 1.000000000000000000, 0.9659258262890683122, 1.000000000000000000, 0.9659258262890683122, 1.000000000000000000, 0.9659258262890683122, 1.000000000000000000, 0.9659258262890683122, 1.000000000000000000, 0.9659258262890683122, 1.000000000000000000, 0.9659258262890683122, 1.000000000000000000, 0.9659258262890683122, 1.000000000000000000, 0.9659258262890683122, 1.000000000000000000, 0.9659258262890683122, 1.000000000000000000, 0.9659258262890683122, 1.000000000000000000, 0.9659258262890683122, 1.000000000000000000, 0.9659258262890683122, 1.000000000000000000, 0.9659258262890683122, 1.000000000000000000, 0.9659258262890683122, 1.000000000000000000, 0.9659258262890683122, 1.000000000000000000, 0.9659258262890683122, 1.000000000000000000, 0.9659258262890683122, 1.000000000000000000, 0.9659258262890683122, 1.000000000000000000, 0.9659258262890683122, 1.000000000000000000, 0.9659258262890683122, 1.000000000000000000, 0.9659258262890683122, 1.000000000000000000, 0.9659258262890683122, 1.000000000000000000, 0.9659258262890683122, 1.000000000000000000, 0.9659258262890683122, 1.000000000000000000, 0.9659258262890683122, 1.000000000000000000, 0.9659258262890683122, 1.000000000000000000, 0.9659258262890683122, 1.000000000000000000, 0.9659258262890683122, 1.000000000000000000, 0.9659258262890683122, 1.000000000000000000, 0.9659258262890683122, 1.000000000000000000, 0.9659258262890683122, 1.000000000000000000, 0.9659258262890683122, 1.000000000000000000, 0.9659258262890683122, 1.000000000000000000, 0.9659258262890683122, 1.000000000000000000, 0.9659258262890683122, 1.000000000000000000, 0.9659258262890683122, 1.000000000000000000, 0.9659258262890683122, 1.000000000000000000, 0.9659258262890683122, 1.000000000000000000, 0.9659258262890683122, 1.000000000000000000, 0.9659258262890683122, 1.000000000000000000, 0.9659258262890683122, 1.000000000000000000, 0.9659258262890683122, 1.000000000000000000, 0.9659258262890683122, 1.000000000000000000, 0.9659258262890683122, 1.000000000000000000, 0.9659258262890683122, 1.000000000000000000, 0.9659258262890683122, 1.000000000000000000, 0.9659258262890683122, 1.000000000000000000, 0.9659258262890683122, 1.000000000000000000, 0.9659258262890683122, 1.000000000000000000, 0.9659258262890683122, 1.000000000000000000, 0.9659258262890683122, 1.000000000000000000, 0.9659258262890683122, 1.000000000000000000, 0.9659258262890683122, 1.000000000000000000, 0.9659258262890683122, 1.000000000000000000, 0.9659258262890683122, 1.000000000000000000, 0.9659258262890683122, 1.000000000000000000, 0.9659258262890683122, 1.000000000000000000, 0.9659258262890683122, 1.000000000000000000, 0.9659258262890683122, 1.000000000000000000, 0.9659258262890683122, 1.000000000000000000, 0.9659258262890683122, 1.000000000000000000, 0.9659258262890683122, 1.000000000000000000, 0.9659258262890683122, 1.000000000000000000, 0.9659258262890683122, 1.000000000000000000, 0.9659258262890683122, 1.000000000000000000, 0.9659258262890683122, 1.000000000000000000, 0.9659258262890683122, 1.000000000000000000, 0.9659258262890683122, 1.000000000000000000, 0.9659258262890683122, 1.000000000000000000, 0.9659258262890683122, 1.000000000000000000, 0.9659258262890683122, 1.000000000000000000, 0.9659258262890683122, 1.000000000000000000, 0.9659258262890683122, 1.000000000000000000, 0.9659258262890683122, 1.000000000000000000, 0.9659258262890683122, 1.000000000000000000, 0.9659258262890683122, 1.000000000000000000, 0.9659258262890683122, 1.000000000000000000, 0.9659258262890683122, 1.000000000000000000, 0.9659258262890683122, 1.000000000000000000, 0.9659258262890683122, 1.000000000000000000, 0.9659258262890683122, 1.000000000000000000, 0.9659258262890683122, 1.000000000000000000, 0.9659258262890683122, 1.000000000000000000, 0.9659258262890683122, 1.000000000000000000, 0.9659258262890683122, 1.000000000000000000, 0.9659258262890683122, 1.000000000000000000, 0.9659258262890683122, 1.000000000000000000, 0.9659258262890683122, 1.000000000000000000, 0.9659258262890683122, 1.000000000000000000, 0.9659258262890683122, 1.000000000000000000, 0.9659258262890683122, 1.000000000000000000, 0.9659258262890683122, 1.000000000000000000, 0.9659258262890683122, 1.000000000000000000, 0.9659258262890683122, 1.000000000000000000, 0.9659258262890683122, 1.000000000000000000, 0.9659258262890683122, 1.000000000000000000, 0.9659258262890683122, 1.000000000000000000, 0.9659258262890683122, 1.000000000000000000, 0.9659258262890683122, 1.000000000000000000, 0.9659258262890683122, 1.000000000000000000, 0.9659258262890683122, 1.000000000000000000, 0.9659258262890683122, 1.000000000000000000, 0.9659258262890683122, 1.000000000000000000, 0.9659258262890683122, 1.000000000000000000, 0.9659258262890683122, 1.000000000000000000, 0.9659258262890683122, 1.000000000000000000, 0.9659258262890683122, 1.000000000000000000, 0.9659258262890683122, 1.000000000000000000, 0.9659258262890683122, 1.000000000000000000, 0.9659258262890683122, 1.000000000000000000, 0.9659258262890683122, 1.000000000000000000, 0.9659258262890683122, 1.000000000000000000, 0.9659258262890683122, 1.000000000000000000, 0.9659258262890683122, 1.000000000000000000, 0.9659258262890683122, 1.000000000000000000, 0.9659258262890683122, 1.000000000000000000, 0.9659258262890683122, 1.000000000000000000, 0.9659258262890683122, 1.000000000000000000, 0.9659258262890683122, 1.000000000000000000, 0.9659258262890683122, 1.000000000000000000, 0.9659258262890683122, 1.000000000000000000, 0.9659258262890683122, 1.000000000000000000, 0.9659258262890683122, 1.000000000000000000, 0.9659258262890683122, 1.000000000000000000, 0.9659258262890683122, 1.000000000000000000, 0.9659258262890683122, 1.000000000000000000, 0.9659258262890683122, 1.000000000000000000, 0.9659258262890683122, 1.000000000000000000, 0.9659258262890683122, 1.000000000000000000, 0.9659258262890683122, 1.000000000000000000),
 ( 1.000000000000000000, 0.9659258262890683122, 1.000000000000000000, 0.9659258262890683122, 1.000000000000000000, 0.9659258262890683122, 1.000000000000000000, 0.9659258262890683122, 1.000000000000000000, 0.9659258262890683122, 1.000000000000000000, 0.9659258262890683122, 1.000000000000000000, 0.9659258262890683122, 1.000000000000000000, 0.9659258262890683122, 1.000000000000000000, 0.9659258262890683122, 1.000000000000000000, 0.9659258262890683122, 1.000000000000000000, 0.9659258262890683122, 1.000000000000000000, 0.9659258262890683122, 1.000000000000000000, 0.9659258262890683122, 1.000000000000000000, 0.9659258262890683122, 1.000000000000000000, 0.9659258262890683122, 1.000000000000000000, 0.9659258262890683122, 1.000000000000000000, 0.9659258262890683122, 1.000000000000000000, 0.9659258262890683122, 1.000000000000000000, 0.9659258262890683122, 1.000000000000000000, 0.9659258262890683122, 1.000000000000000000, 0.9659258262890683122, 1.000000000000000000, 0.9659258262890683122, 1.000000000000000000, 0.9659258262890683122, 1.000000000000000000, 0.9659258262890683122, 1.000000000000000000, 0.9659258262890683122, 1.000000000000000000, 0.9659258262890683122, 1.000000000000000000, 0.9659258262890683122, 1.000000000000000000, 0.9659258262890683122, 1.000000000000000000, 0.9659258262890683122, 1.000000000000000000, 0.9659258262890683122, 1.000000000000000000, 0.9659258262890683122, 1.000000000000000000, 0.9659258262890683122, 1.000000000000000000, 0.9659258262890683122, 1.000000000000000000, 0.9659258262890683122, 1.000000000000000000, 0.9659258262890683122, 1.000000000000000000, 0.9659258262890683122, 1.000000000000000000, 0.9659258262890683122, 1.000000000000000000, 0.9659258262890683122, 1.000000000000000000, 0.9659258262890683122, 1.000000000000000000, 0.9659258262890683122, 1.000000000000000000, 0.9659258262890683122, 1.000000000000000000, 0.9659258262890683122, 1.000000000000000000, 0.9659258262890683122, 1.000000000000000000, 0.9659258262890683122, 1.000000000000000000, 0.9659258262890683122, 1.000000000000000000, 0.9659258262890683122, 1.000000000000000000, 0.9659258262890683122, 1.000000000000000000, 0.9659258262890683122, 1.000000000000000000, 0.9659258262890683122, 1.000000000000000000, 0.9659258262890683122, 1.000000000000000000, 0.9659258262890683122, 1.000000000000000000, 0.9659258262890683122, 1.000000000000000000, 0.9659258262890683122, 1.000000000000000000, 0.9659258262890683122, 1.000000000000000000, 0.9659258262890683122, 1.000000000000000000, 0.9659258262890683122, 1.000000000000000000, 0.9659258262890683122, 1.000000000000000000, 0.9659258262890683122, 1.000000000000000000, 0.9659258262890683122, 1.000000000000000000, 0.9659258262890683122, 1.000000000000000000, 0.9659258262890683122, 1.000000000000000000, 0.9659258262890683122, 1.000000000000000000, 0.9659258262890683122, 1.000000000000000000, 0.9659258262890683122, 1.000000000000000000, 0.9659258262890683122, 1.000000000000000000, 0.9659258262890683122, 1.000000000000000000, 0.9659258262890683122, 1.000000000000000000, 0.9659258262890683122, 1.000000000000000000, 0.9659258262890683122, 1.000000000000000000, 0.9659258262890683122, 1.000000000000000000, 0.9659258262890683122, 1.000000000000000000, 0.9659258262890683122, 1.000000000000000000, 0.9659258262890683122, 1.000000000000000000, 0.9659258262890683122, 1.000000000000000000, 0.9659258262890683122, 1.000000000000000000, 0.9659258262890683122, 1.000000000000000000, 0.9659258262890683122, 1.000000000000000000, 0.9659258262890683122, 1.000000000000000000, 0.9659258262890683122, 1.000000000000000000, 0.9659258262890683122, 1.000000000000000000, 0.9659258262890683122, 1.000000000000000000, 0.9659258262890683122, 1.000000000000000000, 0.9659258262890683122, 1.000000000000000000, 0.9659258262890683122, 1.000000000000000000, 0.9659258262890683122, 1.000000000000000000, 0.9659258262890683122, 1.000000000000000000, 0.9659258262890683122, 1.000000000000000000, 0.9659258262890683122, 1.000000000000000000, 0.9659258262890683122, 1.000000000000000000, 0.9659258262890683122, 1.000000000000000000, 0.9659258262890683122, 1.000000000000000000, 0.9659258262890683122, 1.000000000000000000, 0.9659258262890683122, 1.000000000000000000, 0.9659258262890683122, 1.000000000000000000, 0.9659258262890683122, 1.000000000000000000, 0.9659258262890683122, 1.000000000000000000, 0.9659258262890683122, 1.000000000000000000, 0.9659258262890683122, 1.000000000000000000, 0.9659258262890683122, 1.000000000000000000, 0.9659258262890683122, 1.000000000000000000, 0.9659258262890683122, 1.000000000000000000, 0.9659258262890683122, 1.000000000000000000, 0.9659258262890683122, 1.000000000000000000, 0.9659258262890683122, 1.000000000000000000, 0.9659258262890683122, 1.000000000000000000, 0.9659258262890683122, 1.000000000000000000, 0.9659258262890683122, 1.000000000000000000, 0.9659258262890683122, 1.000000000000000000, 0.9659258262890683122, 1.000000000000000000, 0.9659258262890683122, 1.000000000000000000, 0.9659258262890683122, 1.000000000000000000, 0.9659258262890683122, 1.000000000000000000, 0.9659258262890683122, 1.000000000000000000, 0.9659258262890683122, 1.000000000000000000, 0.9659258262890683122, 1.000000000000000000, 0.9659258262890683122, 1.000000000000000000, 0.9659258262890683122, 1.000000000000000000, 0.9659258262890683122, 1.000000000000000000, 0.9659258262890683122, 1.000000000000000000, 0.9659258262890683122, 1.000000000000000000, 0.9659258262890683122, 1.000000000000000000, 0.9659258262890683122, 1.000000000000000000, 0.9659258262890683122, 1.000000000000000000, 0.9659258262890683122, 1.000000000000000000, 0.9659258262890683122, 1.000000000000000000, 0.9659258262890683122, 1.000000000000000000, 0.9659258262890683122, 1.000000000000000000, 0.9659258262890683122, 1.000000000000000000, 0.9659258262890683122, 1.000000000000000000, 0.9659258262890683122, 1.000000000000000000, 0.9659258262890683122, 1.000000000000000000, 0.9659258262890683122, 1.000000000000000000, 0.9659258262890683122, 1.000000000000000000, 0.9659258262890683122, 1.000000000000000000, 0.9659258262890683122, 1.000000000000000000, 0.9659258262890683122, 1.000000000000000000, 0.9659258262890683122, 1.000000000000000000, 0.9659258262890683122, 1.000000000000000000, 0.9659258262890683122, 1.000000000000000000, 0.9659258262890683122, 1.000000000000000000, 0.9659258262890683122, 1.000000000000000000, 0.9659258262890683122, 1.000000000000000000, 0.9659258262890683122, 1.000000000000000000, 0.9659258262890683122, 1.000000000000000000, 0.9659258262890683122, 1.000000000000000000, 0.9659258262890683122, 1.000000000000000000, 0.9659258262890683122, 1.000000000000000000, 0.9659258262890683122, 1.000000000000000000, 0.9659258262890683122, 1.000000000000000000, 0.9659258262890683122, 1.000000000000000000, 0.9659258262890683122, 1.000000000000000000, 0.9659258262890683122, 1.000000000000000000, 0.9659258262890683122, 1.000000000000000000, 0.9659258262890683122, 1.000000000000000000, 0.9659258262890683122, 1.000000000000000000, 0.9659258262890683122, 1.000000000000000000, 0.9659258262890683122, 1.000000000000000000, 0.9659258262890683122, 1.000000000000000000, 0.9659258262890683122, 1.000000000000000000, 0.9659258262890683122, 1.000000000000000000, 0.9659258262890683122, 1.000000000000000000, 0.9659258262890683122, 1.000000000000000000) ) ) 
 REPRESENTATION_ITEM ( '' )  SURFACE ( )  );
#51619 = CARTESIAN_POINT ( 'NONE',  ( 0.000000000000000000, 0.000000000000000000, 0.000000000000000000 ) ) ;
#51620 = AXIS2_PLACEMENT_3D ( 'NONE', #64108, #2182, #24670 ) ;
#51621 = ADVANCED_FACE ( 'NONE', ( #38279 ), #59279, .F. ) ;
#51622 = ORIENTED_EDGE ( 'NONE', *, *, #87940, .F. ) ;
#51623 = CARTESIAN_POINT ( 'NONE',  ( 0.5774900079438607392, 13.48035201082150358, 5.440088680355550821 ) ) ;
#51624 = CARTESIAN_POINT ( 'NONE',  ( 20.36894250292379382, 3.678748834913967869, 10.36894250292379205 ) ) ;
#51625 = CARTESIAN_POINT ( 'NONE',  ( 10.00000000000000178, 32.25893115100078745, 9.846743663894594434 ) ) ;
#51626 = CARTESIAN_POINT ( 'NONE',  ( 10.00000000000000178, 49.31368534415484106, 10.88017736071110342 ) ) ;
#51628 = FACE_BOUND ( 'NONE', #97700, .T. ) ;
#51627 = CARTESIAN_POINT ( 'NONE',  ( 3.591859063236761518, 24.95696800326375353, 11.09922568453594849 ) ) ;
#51629 = CARTESIAN_POINT ( 'NONE',  ( 12.91533473730992121, 14.52201867748817143, 10.88017736071110164 ) ) ;
#51630 = EDGE_CURVE ( 'NONE', #63243, #55430, #40634, .T. ) ;
#51631 = CARTESIAN_POINT ( 'NONE',  ( 12.60589901313221439, 0.5000000000000004441, -8.129656208642048298 ) ) ;
#51632 = DIRECTION ( 'NONE',  ( 0.000000000000000000, 0.000000000000000000, -1.000000000000000000 ) ) ;
#51633 = CARTESIAN_POINT ( 'NONE',  ( -1.099225684535947600, 4.540301336597087456, 6.408140936763237150 ) ) ;
#51634 = CARTESIAN_POINT ( 'NONE',  ( 12.63842701281683922, 64.55059781766745175, -9.846743663894590881 ) ) ;
#51635 = CARTESIAN_POINT ( 'NONE',  ( 0.1532563361054100626, 25.80059781766744820, -2.638427012816831230 ) ) ;
#51636 = CARTESIAN_POINT ( 'NONE',  ( -7.964842623401179544, -12.56131465584515894, -7.964842623401174215 ) ) ;
#51637 = CARTESIAN_POINT ( 'NONE',  ( 10.00000000000000178, 40.37363466993042493, 12.81628187352647608 ) ) ;
#51639 = CARTESIAN_POINT ( 'NONE',  ( 14.61146088927472420, 2.439454888092384977E-16, 0.6660010753335569023 ) ) ;
#51638 = CARTESIAN_POINT ( 'NONE',  ( 2.035157376598824452, 38.68868534415483396, 7.964842623401179544 ) ) ;
#51640 = CYLINDRICAL_SURFACE ( 'NONE', #27364, 11.92686044187656513 ) ;
#51641 = CARTESIAN_POINT ( 'NONE',  ( 7.084665262690076126, 22.02201867748817321, -10.88017736071110164 ) ) ;
#51642 = CARTESIAN_POINT ( 'NONE',  ( 20.88017736071110164, 35.35535201082150536, 2.915334737309930979 ) ) ;
#51643 = CARTESIAN_POINT ( 'NONE',  ( 19.84674366389459266, 53.71726448433411605, -2.638427012816827677 ) ) ;
#51644 = CARTESIAN_POINT ( 'NONE',  ( -0.8801773607110991993, 57.85535201082149825, -2.915334737309923874 ) ) ;
#51645 = AXIS2_PLACEMENT_3D ( 'NONE', #61836, #1862, #93815 ) ;
#51646 = CARTESIAN_POINT ( 'NONE',  ( 24.16423886937410614, 34.30374883491396787, 8.672049930838204340E-16 ) ) ;
#51647 = TOROIDAL_SURFACE ( 'NONE', #24470, 20.49999999999999645, 0.5000000000000000000 ) ;
#51648 = CARTESIAN_POINT ( 'NONE',  ( 0.1532563361054082862, 41.21726448433411605, 2.638427012816831674 ) ) ;
#51649 = CARTESIAN_POINT ( 'NONE',  ( -2.816281873526473856, 64.12363466993042493, 9.499525473075851096E-16 ) ) ;
#51650 = CARTESIAN_POINT ( 'NONE',  ( -1.099225684535947600, 3.706968003263753531, -6.408140936763238038 ) ) ;
#51651 = VERTEX_POINT ( 'NONE', #14798 ) ;
#51652 = CARTESIAN_POINT ( 'NONE',  ( 4.559911319644449179, 23.89701867748817321, 9.422509992056141925 ) ) ;
#51653 = MECHANICAL_DESIGN_GEOMETRIC_PRESENTATION_REPRESENTATION (  '', ( #70869 ), #43643 ) ;
#51654 = CYLINDRICAL_SURFACE ( 'NONE', #11078, 15.00000000000000000 ) ;
#51655 = CARTESIAN_POINT ( 'NONE',  ( 7.084665262690076126, 19.10535201082150181, 10.88017736071109987 ) ) ;
#51656 = CARTESIAN_POINT ( 'NONE',  ( 20.88017736071110519, 65.56368534415483396, 2.639326808657452039E-16 ) ) ;
#51657 = CARTESIAN_POINT ( 'NONE',  ( 22.26659068614894466, 23.88708216824730357, 7.082119434687054849 ) ) ;
#51658 = CARTESIAN_POINT ( 'NONE',  ( 19.84674366389459266, 18.30059781766745175, 2.638427012816836559 ) ) ;
#51659 = CARTESIAN_POINT ( 'NONE',  ( -14.26139399674453578, 3.905478766663822759E-16, -2.619664342929995282 ) ) ;
#51660 = CARTESIAN_POINT ( 'NONE',  ( 15.44008868035555260, 49.73035201082150536, 9.422509992056143702 ) ) ;
#51661 = AXIS2_PLACEMENT_3D ( 'NONE', #78275, #31782, #24314 ) ;
#51662 = CARTESIAN_POINT ( 'NONE',  ( -0.1503990784575242878, 34.24884699246889141, -6.262539305110083276 ) ) ;
#51663 = CARTESIAN_POINT ( 'NONE',  ( -42.83893681340153847, 106.9585622934581721, -5.000000000000000888 ) ) ;
#51664 = EDGE_CURVE ( 'NONE', #43937, #29028, #46040, .T. ) ;
#51665 = ORIENTED_EDGE ( 'NONE', *, *, #72713, .T. ) ;
#51666 = CARTESIAN_POINT ( 'NONE',  ( 4.406177045959971394, -8.255047197857166452, 2.500000000000000000 ) ) ;
#51667 = CARTESIAN_POINT ( 'NONE',  ( 2.791683348922240793, 41.63393115100078745, 7.208316651077764092 ) ) ;
#51668 = ORIENTED_EDGE ( 'NONE', *, *, #21004, .F. ) ;
#51669 = ORIENTED_EDGE ( 'NONE', *, *, #89716, .F. ) ;
#51670 = CARTESIAN_POINT ( 'NONE',  ( 12.98685442714199390, 3.839196892837649736E-16, -6.449155920600954772 ) ) ;
#51671 = CARTESIAN_POINT ( 'NONE',  ( -2.266590686148945544, 17.22041550158063572, 7.082119434687048631 ) ) ;
#51672 = CARTESIAN_POINT ( 'NONE',  ( -4.164238869374098151, 26.59541550158063217, -3.795296366450310543 ) ) ;
#51673 = CARTESIAN_POINT ( 'NONE',  ( 12.91533473730993009, 56.60535201082151247, -10.88017736071109987 ) ) ;
#51674 = CARTESIAN_POINT ( 'NONE',  ( 2.917880565312948704, 62.63708216824730357, 12.26659068614894643 ) ) ;
#51675 = CARTESIAN_POINT ( 'NONE',  ( 3.591859063236763294, -1.709698663402913210, -11.09922568453595026 ) ) ;
#51676 = CARTESIAN_POINT ( 'NONE',  ( 7.361572987183170547, 47.05059781766745175, 9.846743663894590881 ) ) ;
#51678 = CARTESIAN_POINT ( 'NONE',  ( 6.565887622018943937, 0.1653013365970866511, 12.81628187352647430 ) ) ;
#51677 = CARTESIAN_POINT ( 'NONE',  ( 4.559911319644449179, 43.89701867748816966, 9.422509992056141925 ) ) ;
#51679 = CARTESIAN_POINT ( 'NONE',  ( 10.00000000000000178, 23.05374883491397142, 14.16423886937410082 ) ) ;
#51680 = CARTESIAN_POINT ( 'NONE',  ( -2.266590686148945544, 47.22041550158063927, 7.082119434687048631 ) ) ;
#51681 = CARTESIAN_POINT ( 'NONE',  ( 2.035157376598822676, 22.43868534415483396, -7.964842623401177768 ) ) ;
#51682 = CARTESIAN_POINT ( 'NONE',  ( -1.926860441876563801, 2.662123368507804511, 1.004413902775740978E-15 ) ) ;
#51683 = CARTESIAN_POINT ( 'NONE',  ( -0.8801773607110991993, 37.85535201082151247, -2.915334737309923874 ) ) ;
#51684 = CARTESIAN_POINT ( 'NONE',  ( 6.565887622018943937, 53.08196800326374643, -12.81628187352647608 ) ) ;
#51685 = CARTESIAN_POINT ( 'NONE',  ( 9.846743663894594434, -26.49106884899921255, -2.168404344971008868E-15 ) ) ;
#51686 = VERTEX_POINT ( 'NONE', #90768 ) ;
#51687 = CARTESIAN_POINT ( 'NONE',  ( 13.34989199099675439, 0.04962897297196695173, 6.279943681065537575 ) ) ;
#51688 = VERTEX_POINT ( 'NONE', #97309 ) ;
#51689 = ORIENTED_EDGE ( 'NONE', *, *, #65283, .F. ) ;
#51690 = CARTESIAN_POINT ( 'NONE',  ( -0.3689425029237898834, 46.17874883491397497, -10.36894250292378850 ) ) ;
#51692 = CARTESIAN_POINT ( 'NONE',  ( 2.791683348922237240, 45.38393115100079456, -7.208316651077763204 ) ) ;
#51691 = CARTESIAN_POINT ( 'NONE',  ( 19.84674366389459266, 18.71726448433411960, -2.638427012816827677 ) ) ;
#51693 = CARTESIAN_POINT ( 'NONE',  ( 15.44008868035555793, 66.39701867748817676, -9.422509992056140149 ) ) ;
#51694 = CARTESIAN_POINT ( 'NONE',  ( -0.1503990784575328643, 55.12777174578612716, 6.262539305110068177 ) ) ;
#51695 = SHAPE_REPRESENTATION ( '1.0 Fixed Jaw', ( #27931 ), #34259 ) ;
#51696 = CARTESIAN_POINT ( 'NONE',  ( -0.8801773607110991993, 57.85535201082149825, -2.915334737309923874 ) ) ;
#51697 = CARTESIAN_POINT ( 'NONE',  ( -1.099225684535947600, 53.70696800326376064, -6.408140936763238038 ) ) ;
#51698 = CARTESIAN_POINT ( 'NONE',  ( 6.408140936763236262, 12.45696800326375531, -11.09922568453595026 ) ) ;
#51699 = EDGE_LOOP ( 'NONE', ( #19189, #59580, #66175, #25281, #87607, #59993, #54995, #88552 ) ) ;
#51700 = EDGE_CURVE ( 'NONE', #33002, #71459, #7784, .T. ) ;
#51701 = CARTESIAN_POINT ( 'NONE',  ( 13.79529636645031943, 35.34541550158063927, -14.16423886937409904 ) ) ;
#51702 = CARTESIAN_POINT ( 'NONE',  ( 21.09922568453595559, 27.04030133659708568, -6.408140936763230044 ) ) ;
#51703 = ORIENTED_EDGE ( 'NONE', *, *, #90341, .T. ) ;
#51704 = CARTESIAN_POINT ( 'NONE',  ( 13.43411237798106583, 42.66530133659707502, -12.81628187352647252 ) ) ;
#51705 = CARTESIAN_POINT ( 'NONE',  ( 10.00000000000000000, 34.75893115100078745, -9.846743663894594434 ) ) ;
#51706 = CARTESIAN_POINT ( 'NONE',  ( 20.88017736071110875, 15.77201867748817143, -2.915334737309920765 ) ) ;
#51707 = PLANE ( 'NONE',  #38773 ) ;
#51708 = DIRECTION ( 'NONE',  ( 0.000000000000000000, -1.000000000000000000, 0.000000000000000000 ) ) ;
#51709 = CARTESIAN_POINT ( 'NONE',  ( 1.472469842513823179, 45.59226448433412315, -4.923371831947296329 ) ) ;
#51710 = CARTESIAN_POINT ( 'NONE',  ( 10.00000000000000178, 47.25893115100078745, 9.846743663894594434 ) ) ;
#51712 = VERTEX_POINT ( 'NONE', #15292 ) ;
#51711 = PLANE ( 'NONE',  #23322 ) ;
#51713 = DIRECTION ( 'NONE',  ( 0.000000000000000000, 0.000000000000000000, 1.000000000000000000 ) ) ;
#51714 = VECTOR ( 'NONE', #27173, 1000.000000000000000 ) ;
#51715 = CARTESIAN_POINT ( 'NONE',  ( -15.94000000000001371, 93.50000000000000000, -10.09898361729590199 ) ) ;
#51716 = CARTESIAN_POINT ( 'NONE',  ( 0.2751277870543045734, 27.28217586085238011, -6.500000000000012434 ) ) ;
#51717 = EDGE_CURVE ( 'NONE', #16296, #88170, #45271, .T. ) ;
#51718 = DIRECTION ( 'NONE',  ( -0.07626964003977219908, 0.9970872288863213972, 0.000000000000000000 ) ) ;
#51719 = CARTESIAN_POINT ( 'NONE',  ( 19.84674366389459621, 13.50893115100078568, 7.409399052514197653E-17 ) ) ;
#51720 = EDGE_CURVE ( 'NONE', #37917, #67494, #60758, .T. ) ;
#51721 = CARTESIAN_POINT ( 'NONE',  ( 21.09922568453594849, 41.20696800326375353, 6.408140936763242479 ) ) ;
#51723 = FACE_OUTER_BOUND ( 'NONE', #79979, .T. ) ;
#51722 = VECTOR ( 'NONE', #59608, 1000.000000000000000 ) ;
#51724 = ORIENTED_EDGE ( 'NONE', *, *, #96791, .T. ) ;
#51725 = CARTESIAN_POINT ( 'NONE',  ( 17.20831665107776587, 59.13393115100078745, -7.208316651077762316 ) ) ;
#51726 = DIRECTION ( 'NONE',  ( -0.9890158633619177131, 0.000000000000000000, 0.1478094111296046342 ) ) ;
#51727 = CARTESIAN_POINT ( 'NONE',  ( 2.917880565312950480, 15.97041550158063217, -12.26659068614894821 ) ) ;
#51728 = CARTESIAN_POINT ( 'NONE',  ( 10.00000000000000178, 52.25893115100078745, 9.846743663894594434 ) ) ;
#51729 = CARTESIAN_POINT ( 'NONE',  ( 21.09922568453595559, 42.04030133659708213, -6.408140936763230044 ) ) ;
#51731 = FILL_AREA_STYLE_COLOUR ( '', #33703 ) ;
#51730 = CARTESIAN_POINT ( 'NONE',  ( -4.431036607602684363, 14.63606876205412632, 14.33059365769911508 ) ) ;
#51732 = CARTESIAN_POINT ( 'NONE',  ( 1.472469842513823179, 11.42559781766745175, 4.923371831947296329 ) ) ;
#51733 = CARTESIAN_POINT ( 'NONE',  ( 0.1916775849787265840, 67.25868815902069286, -6.499999999999991118 ) ) ;
#51734 = CARTESIAN_POINT ( 'NONE',  ( 12.63842701281683034, 52.46726448433413026, 9.846743663894596210 ) ) ;
#51735 = CARTESIAN_POINT ( 'NONE',  ( 12.91533473730992121, 39.52201867748817676, 10.88017736071110164 ) ) ;
#51736 = APPLICATION_PROTOCOL_DEFINITION ( 'draft international standard', 'automotive_design', 1998, #52544 ) ;
#51737 = CARTESIAN_POINT ( 'NONE',  ( 19.80448550324506840, 31.82703681773341131, 6.500000000002799538 ) ) ;
#51738 = CARTESIAN_POINT ( 'NONE',  ( 20.88017736071110164, 40.35535201082150536, 2.915334737309930979 ) ) ;
#51739 = VERTEX_POINT ( 'NONE', #76267 ) ;
#51740 = CARTESIAN_POINT ( 'NONE',  ( 2.035157376598824452, 18.68868534415484106, 7.964842623401179544 ) ) ;
#51742 = CARTESIAN_POINT ( 'NONE',  ( -0.8801773607111009756, 38.06368534415484106, 1.068504757029289695E-15 ) ) ;
#51741 = CARTESIAN_POINT ( 'NONE',  ( 17.20831665107776587, 54.13393115100079456, -7.208316651077762316 ) ) ;
#51743 = CARTESIAN_POINT ( 'NONE',  ( 0.000000000000000000, 15.00000000000000000, -14.25000000000000000 ) ) ;
#51744 = EDGE_CURVE ( 'NONE', #56319, #85753, #10289, .T. ) ;
#51745 = CARTESIAN_POINT ( 'NONE',  ( 20.88017736071110519, 55.56368534415484817, 2.639326808657452039E-16 ) ) ;
#51747 = CARTESIAN_POINT ( 'NONE',  ( -46.94000000000001194, 103.0000000000000000, 5.000000000000000000 ) ) ;
#51746 = CARTESIAN_POINT ( 'NONE',  ( 20.88017736071110164, 20.35535201082150891, 2.915334737309930979 ) ) ;
#51748 = CARTESIAN_POINT ( 'NONE',  ( 2.791683348922237240, 5.383931151000785675, -7.208316651077763204 ) ) ;
#51749 = CARTESIAN_POINT ( 'NONE',  ( 18.52753015748617571, 28.09226448433411960, 4.923371831947298993 ) ) ;
#51750 = CARTESIAN_POINT ( 'NONE',  ( 14.16423886937410437, 4.095415501580630391, 3.795296366450304770 ) ) ;
#51751 = CARTESIAN_POINT ( 'NONE',  ( 1.472469842513823179, 66.42559781766745175, 4.923371831947296329 ) ) ;
#51752 = CARTESIAN_POINT ( 'NONE',  ( 4.559911319644449179, 3.897018677488171434, 9.422509992056141925 ) ) ;
#51753 = LINE ( 'NONE', #74231, #88079 ) ;
#51754 = CARTESIAN_POINT ( 'NONE',  ( 6.204703633549690345, 5.762082168247301794, -14.16423886937410259 ) ) ;
#51755 = CARTESIAN_POINT ( 'NONE',  ( 13.79529636645031943, 50.34541550158064638, -14.16423886937409904 ) ) ;
#51756 = CARTESIAN_POINT ( 'NONE',  ( -2.816281873526473856, 9.123634669930421381, 9.499525473075851096E-16 ) ) ;
#51757 = VERTEX_POINT ( 'NONE', #74781 ) ;
#51758 = CARTESIAN_POINT ( 'NONE',  ( 7.084665262690076126, 9.105352010821503583, 10.88017736071109987 ) ) ;
#51759 = CARTESIAN_POINT ( 'NONE',  ( 5.076628168052703671, 51.84226448433412315, 8.527530157486179263 ) ) ;
#51761 = LINE ( 'NONE', #43754, #69434 ) ;
#51760 = FILL_AREA_STYLE ('',( #28260 ) ) ;
#51762 = PLANE ( 'NONE',  #20060 ) ;
#51763 = CARTESIAN_POINT ( 'NONE',  ( 1.472469842513823179, 0.5922644843341181575, -4.923371831947296329 ) ) ;
#51764 = CARTESIAN_POINT ( 'NONE',  ( 0.6178305044545838731, 19.74863466993042138, 9.382169495545420901 ) ) ;
#51765 = CARTESIAN_POINT ( 'NONE',  ( 1.472469842513823179, 30.59226448433411960, -4.923371831947296329 ) ) ;
#51766 = ORIENTED_EDGE ( 'NONE', *, *, #75792, .T. ) ;
#51767 = CARTESIAN_POINT ( 'NONE',  ( 1.472469842513823179, 11.42559781766745175, 4.923371831947296329 ) ) ;
#51768 = CARTESIAN_POINT ( 'NONE',  ( 11.10647200087231568, -65.08385396170790216, -4.000000000000000000 ) ) ;
#51769 = CARTESIAN_POINT ( 'NONE',  ( -1.114591949024815731, 15.00000000000000000, -14.45709807627963350 ) ) ;
#51770 = CARTESIAN_POINT ( 'NONE',  ( 4.559911319644449179, 18.89701867748817321, 9.422509992056141925 ) ) ;
#51771 = CARTESIAN_POINT ( 'NONE',  ( 22.26659068614894466, 38.88708216824731068, 7.082119434687054849 ) ) ;
#51772 = CARTESIAN_POINT ( 'NONE',  ( 10.00000000000000178, 44.31368534415484106, 10.88017736071110342 ) ) ;
#51773 = CARTESIAN_POINT ( 'NONE',  ( 12.91533473730993009, 56.60535201082151247, -10.88017736071109987 ) ) ;
#51774 = CARTESIAN_POINT ( 'NONE',  ( -12.03768810259491140, -3.868822986584015221E-15, 8.306778944023246680 ) ) ;
#51775 = CARTESIAN_POINT ( 'NONE',  ( 14.92337183194729988, 24.34226448433411960, -8.527530157486177487 ) ) ;
#51776 = CARTESIAN_POINT ( 'NONE',  ( 6.879999999999995453, 43.00000000000000000, -4.000000000000000000 ) ) ;
#51777 = CARTESIAN_POINT ( 'NONE',  ( 17.20831665107776587, 2.883931151000785231, 7.208316651077764980 ) ) ;
#51778 = CARTESIAN_POINT ( 'NONE',  ( 19.84674366389459266, 33.71726448433410894, -2.638427012816827677 ) ) ;
#51779 = CARTESIAN_POINT ( 'NONE',  ( 0.5774900079438590739, 32.64701867748816966, -5.440088680355550821 ) ) ;
#51780 = EDGE_CURVE ( 'NONE', #89049, #87399, #6290, .T. ) ;
#51781 = VERTEX_POINT ( 'NONE', #77731 ) ;
#51782 = CARTESIAN_POINT ( 'NONE',  ( -2.816281873526473856, 54.33196800326376064, 3.434112377981055619 ) ) ;
#51783 = LINE ( 'NONE', #53754, #30077 ) ;
#51784 = CARTESIAN_POINT ( 'NONE',  ( 12.63842701281683922, 14.55059781766744997, -9.846743663894590881 ) ) ;
#51785 = CARTESIAN_POINT ( 'NONE',  ( 0.6178305044545838731, 49.74863466993041072, 9.382169495545420901 ) ) ;
#51787 = CARTESIAN_POINT ( 'NONE',  ( 0.1532563361054082862, 41.21726448433411605, 2.638427012816831674 ) ) ;
#51786 = CARTESIAN_POINT ( 'NONE',  ( 4.559911319644449179, 2.230352010821504916, -9.422509992056141925 ) ) ;
#51788 = CARTESIAN_POINT ( 'NONE',  ( 14.92337183194729633, 2.675597817667451750, 8.527530157486181039 ) ) ;
#51789 = CARTESIAN_POINT ( 'NONE',  ( 20.36894250292379738, 19.92874883491396787, -10.36894250292379027 ) ) ;
#51790 = CARTESIAN_POINT ( 'NONE',  ( 22.26659068614895176, 44.72041550158063927, -7.082119434687042414 ) ) ;
#51791 = CARTESIAN_POINT ( 'NONE',  ( 10.00000000000000000, 44.75893115100078745, -9.846743663894594434 ) ) ;
#51792 = CARTESIAN_POINT ( 'NONE',  ( 0.000000000000000000, 15.00000000000000000, 0.000000000000000000 ) ) ;
#51793 = CARTESIAN_POINT ( 'NONE',  ( 12.91533473730992121, 44.52201867748816966, 10.88017736071110164 ) ) ;
#51794 = AXIS2_PLACEMENT_3D ( 'NONE', #9453, #85955, #76961 ) ;
#51795 = CARTESIAN_POINT ( 'NONE',  ( 12.63842701281683034, 7.467264484334118713, 9.846743663894596210 ) ) ;
#51796 = CARTESIAN_POINT ( 'NONE',  ( -3.878348535191012303, -3.630205232349507760, 4.000000000000000000 ) ) ;
#51797 = EDGE_LOOP ( 'NONE', ( #75215, #37689, #53537, #87010 ) ) ;
#51798 = CARTESIAN_POINT ( 'NONE',  ( 0.6178305044545838731, 64.74863466993043914, 9.382169495545420901 ) ) ;
#51799 = ORIENTED_EDGE ( 'NONE', *, *, #51956, .F. ) ;
#51800 = CARTESIAN_POINT ( 'NONE',  ( 15.44008868035555793, 61.39701867748817676, -9.422509992056140149 ) ) ;
#51801 = ORIENTED_EDGE ( 'NONE', *, *, #45088, .T. ) ;
#51802 = ADVANCED_FACE ( 'NONE', ( #2755 ), #24748, .F. ) ;
#51803 = CARTESIAN_POINT ( 'NONE',  ( 6.204703633549690345, 5.762082168247301794, -14.16423886937410259 ) ) ;
#51804 = CARTESIAN_POINT ( 'NONE',  ( 17.20831665107776587, 4.133931151000785675, -7.208316651077762316 ) ) ;
#51805 = CARTESIAN_POINT ( 'NONE',  ( 0.000000000000000000, 0.000000000000000000, 0.000000000000000000 ) ) ;
#51806 = EDGE_LOOP ( 'NONE', ( #93593, #68672, #81054, #64474 ) ) ;
#51807 = CARTESIAN_POINT ( 'NONE',  ( -0.8801773607111008646, 13.27201867748817143, 2.915334737309923430 ) ) ;
#51808 = ORIENTED_EDGE ( 'NONE', *, *, #86071, .F. ) ;
#51809 = CARTESIAN_POINT ( 'NONE',  ( 12.91533473730992121, 34.52201867748817676, 10.88017736071110164 ) ) ;
#51810 = CARTESIAN_POINT ( 'NONE',  ( 14.92337183194729988, 59.34226448433412315, -8.527530157486177487 ) ) ;
#51811 = ORIENTED_EDGE ( 'NONE', *, *, #55220, .F. ) ;
#51812 = CARTESIAN_POINT ( 'NONE',  ( 0.1532563361054082862, 56.21726448433411605, 2.638427012816831674 ) ) ;
#51813 = ORIENTED_EDGE ( 'NONE', *, *, #39123, .F. ) ;
#51814 = CARTESIAN_POINT ( 'NONE',  ( -0.8801773607110991993, 62.85535201082150536, -2.915334737309923874 ) ) ;
#51815 = CARTESIAN_POINT ( 'NONE',  ( 2.791683348922237240, 65.38393115100078035, -7.208316651077763204 ) ) ;
#51816 = EDGE_CURVE ( 'NONE', #5586, #47253, #51822, .T. ) ;
#51817 = CARTESIAN_POINT ( 'NONE',  ( 3.591859063236761518, 34.95696800326375353, 11.09922568453594849 ) ) ;
#51819 = DIRECTION ( 'NONE',  ( -0.000000000000000000, 1.000000000000000000, -0.000000000000000000 ) ) ;
#51818 = CARTESIAN_POINT ( 'NONE',  ( 12.91533473730993009, 21.60535201082150536, -10.88017736071109987 ) ) ;
#51820 = CARTESIAN_POINT ( 'NONE',  ( 19.84674366389459621, 8.508931151000785675, 7.409399052514197653E-17 ) ) ;
#51821 = CARTESIAN_POINT ( 'NONE',  ( 2.035157376598824452, 13.68868534415483751, 7.964842623401179544 ) ) ;
#51822 = CIRCLE ( 'NONE', #5514, 15.00000000000000000 ) ;
#51823 = ADVANCED_FACE ( 'NONE', ( #77241 ), #90132, .T. ) ;
#51824 = ORIENTED_EDGE ( 'NONE', *, *, #90290, .T. ) ;
#51825 = CARTESIAN_POINT ( 'NONE',  ( -1.099225684535947600, 49.54030133659708923, 6.408140936763237150 ) ) ;
#51826 = CARTESIAN_POINT ( 'NONE',  ( 0.5774900079438607392, 43.48035201082151247, 5.440088680355550821 ) ) ;
#51827 = CARTESIAN_POINT ( 'NONE',  ( -46.94000000000001194, 101.9887809004034267, -6.851115700664164088 ) ) ;
#51828 = CARTESIAN_POINT ( 'NONE',  ( 16.40814093676323893, 60.79030133659709634, 11.09922568453595026 ) ) ;
#51829 = CARTESIAN_POINT ( 'NONE',  ( 0.5774900079438607392, 43.48035201082151247, 5.440088680355550821 ) ) ;
#51830 = EDGE_CURVE ( 'NONE', #5117, #39559, #85247, .T. ) ;
#51831 = CARTESIAN_POINT ( 'NONE',  ( 12.63842701281683034, 62.46726448433410894, 9.846743663894596210 ) ) ;
#51832 = PLANE ( 'NONE',  #91399 ) ;
#51833 = CARTESIAN_POINT ( 'NONE',  ( 14.92337183194729988, 24.34226448433411960, -8.527530157486177487 ) ) ;
#51834 = CARTESIAN_POINT ( 'NONE',  ( -2.816281873526471635, 8.915301336597083903, -3.434112377981056508 ) ) ;
#51836 = CARTESIAN_POINT ( 'NONE',  ( 14.92337183194729633, 62.67559781766745886, 8.527530157486181039 ) ) ;
#51835 = DIRECTION ( 'NONE',  ( 0.9170600743851183845, 0.000000000000000000, 0.3987490689252592979 ) ) ;
#51837 = CARTESIAN_POINT ( 'NONE',  ( -0.8801773607111008646, 38.27201867748816255, 2.915334737309923430 ) ) ;
#51838 = CARTESIAN_POINT ( 'NONE',  ( 18.52753015748618282, 48.92559781766745886, -4.923371831947291888 ) ) ;
#51839 = PRESENTATION_STYLE_ASSIGNMENT (( #82326 ) ) ;
#51840 = CARTESIAN_POINT ( 'NONE',  ( 0.1532563361054082862, 26.21726448433411605, 2.638427012816831674 ) ) ;
#51841 = CARTESIAN_POINT ( 'NONE',  ( 19.84674366389459266, 8.717264484334116048, -2.638427012816827677 ) ) ;
#51843 = ORIENTED_EDGE ( 'NONE', *, *, #35665, .F. ) ;
#51842 = CARTESIAN_POINT ( 'NONE',  ( 0.6178305044545818747, 8.498634669930421381, -9.382169495545419124 ) ) ;
#51844 = CARTESIAN_POINT ( 'NONE',  ( 0.2751277870542910842, 63.21833443783937412, 6.499999999999992006 ) ) ;
#51845 = FACE_OUTER_BOUND ( 'NONE', #279, .T. ) ;
#51846 = CARTESIAN_POINT ( 'NONE',  ( 21.09922568453594849, 36.20696800326375353, 6.408140936763242479 ) ) ;
#51847 = CARTESIAN_POINT ( 'NONE',  ( 14.92337183194729988, 34.34226448433411605, -8.527530157486177487 ) ) ;
#51848 = COLOUR_RGB ( '', 0.72549020, 0.75294118, 0.79215686) ;
#51849 = LINE ( 'NONE', #57372, #82385 ) ;
#51850 = CARTESIAN_POINT ( 'NONE',  ( 15.44008868035555260, 9.730352010821505360, 9.422509992056143702 ) ) ;
#51851 = CARTESIAN_POINT ( 'NONE',  ( 7.361572987183169658, 29.96726448433411960, -9.846743663894592657 ) ) ;
#51852 = AXIS2_PLACEMENT_3D ( 'NONE', #17939, #39468, #55446 ) ;
#51853 = ORIENTED_EDGE ( 'NONE', *, *, #90191, .T. ) ;
#51854 = CARTESIAN_POINT ( 'NONE',  ( 1.042145700049383228, 24.74216108172002038, -6.499999999999826805 ) ) ;
#51855 = TOROIDAL_SURFACE ( 'NONE', #8753, 0.5000000000000000000, 0.2500000000000000000 ) ;
#51856 = CARTESIAN_POINT ( 'NONE',  ( 15.44008868035555793, 6.397018677488171434, -9.422509992056140149 ) ) ;
#51857 = CARTESIAN_POINT ( 'NONE',  ( -42.93999999999999773, 92.00000000000000000, 9.292893218813452094 ) ) ;
#51858 = ADVANCED_FACE ( 'NONE', ( #70251 ), #3942, .T. ) ;
#51859 = CARTESIAN_POINT ( 'NONE',  ( 2.035157376598824452, 13.68868534415483751, 7.964842623401179544 ) ) ;
#51860 = CARTESIAN_POINT ( 'NONE',  ( 13.79529636645030344, 48.26208216824728936, 14.16423886937410614 ) ) ;
#51862 = DIRECTION ( 'NONE',  ( -0.5075383629607084224, 0.000000000000000000, 0.8616291604415231564 ) ) ;
#51861 = CARTESIAN_POINT ( 'NONE',  ( -2.266590686148945544, 56.38708216824731068, -7.082119434687050408 ) ) ;
#51863 = CARTESIAN_POINT ( 'NONE',  ( 64.56412365047461321, -3.756725070333740926E-15, 0.000000000000000000 ) ) ;
#51864 = VECTOR ( 'NONE', #33746, 1000.000000000000000 ) ;
#51865 = CARTESIAN_POINT ( 'NONE',  ( 10.00000000000000178, 12.25893115100078568, 9.846743663894594434 ) ) ;
#51866 = CARTESIAN_POINT ( 'NONE',  ( 13.43411237798105340, 0.5819680032637533085, 12.81628187352647963 ) ) ;
#51867 = ORIENTED_EDGE ( 'NONE', *, *, #25686, .T. ) ;
#51868 = FACE_OUTER_BOUND ( 'NONE', #86175, .T. ) ;
#51869 = CARTESIAN_POINT ( 'NONE',  ( 2.791683348922240793, 61.63393115100079456, 7.208316651077764092 ) ) ;
#51870 = DIRECTION ( 'NONE',  ( 0.000000000000000000, 0.000000000000000000, 1.000000000000000000 ) ) ;
#51871 = EDGE_CURVE ( 'NONE', #9609, #79224, #22122, .T. ) ;
#51872 = CARTESIAN_POINT ( 'NONE',  ( 18.52753015748617571, 63.09226448433412315, 4.923371831947298993 ) ) ;
#51873 = CARTESIAN_POINT ( 'NONE',  ( 10.00000000000000178, 13.05374883491396787, 14.16423886937410082 ) ) ;
#51874 = CARTESIAN_POINT ( 'NONE',  ( 5.076628168052703671, 21.84226448433411960, 8.527530157486179263 ) ) ;
#51875 = LINE ( 'NONE', #90845, #88002 ) ;
#51876 = ORIENTED_EDGE ( 'NONE', *, *, #61286, .T. ) ;
#51877 = AXIS2_PLACEMENT_3D ( 'NONE', #16346, #92821, #76352 ) ;
#51878 = CARTESIAN_POINT ( 'NONE',  ( 24.16423886937410614, 44.30374883491397497, 8.672049930838204340E-16 ) ) ;
#51879 = CARTESIAN_POINT ( 'NONE',  ( 5.076628168052703671, 6.842264484334118713, 8.527530157486179263 ) ) ;
#51881 = LINE ( 'NONE', #97900, #53436 ) ;
#51880 = DIRECTION ( 'NONE',  ( 1.000000000000000000, 1.636349903325072848E-16, 0.000000000000000000 ) ) ;
#51882 = CARTESIAN_POINT ( 'NONE',  ( 2.035157376598822676, 37.43868534415484106, -7.964842623401177768 ) ) ;
#51883 = CARTESIAN_POINT ( 'NONE',  ( 19.38216949554541557, 37.24863466993041783, -9.382169495545420901 ) ) ;
#51884 = CARTESIAN_POINT ( 'NONE',  ( 4.559911319644449179, 3.897018677488170990, 9.422509992056141925 ) ) ;
#51885 = CARTESIAN_POINT ( 'NONE',  ( 3.591859063236763294, 33.29030133659708213, -11.09922568453595026 ) ) ;
#51886 = CARTESIAN_POINT ( 'NONE',  ( -2.816281873526473856, 64.33196800326376774, 3.434112377981055619 ) ) ;
#51887 = EDGE_LOOP ( 'NONE', ( #62548, #34307, #79129, #52677 ) ) ;
#51888 = LINE ( 'NONE', #89878, #11083 ) ;
#51889 = CARTESIAN_POINT ( 'NONE',  ( 22.26659068614895176, 39.72041550158063217, -7.082119434687042414 ) ) ;
#51890 = FACE_OUTER_BOUND ( 'NONE', #20336, .T. ) ;
#51891 = CARTESIAN_POINT ( 'NONE',  ( 20.88017736071110519, 5.563685344154837509, 2.639326808657452039E-16 ) ) ;
#51892 = CARTESIAN_POINT ( 'NONE',  ( 17.96484262340118221, 21.18868534415483396, -7.964842623401177768 ) ) ;
#51893 = DIRECTION ( 'NONE',  ( -0.000000000000000000, 1.000000000000000000, 0.000000000000000000 ) ) ;
#51894 = SURFACE_SIDE_STYLE ('',( #7394 ) ) ;
#51895 = CARTESIAN_POINT ( 'NONE',  ( 10.00000000000000000, 51.81368534415484106, -10.88017736071110342 ) ) ;
#51896 = CARTESIAN_POINT ( 'NONE',  ( 19.42250999205614548, 50.98035201082151247, -5.440088680355545492 ) ) ;
#51897 = CARTESIAN_POINT ( 'NONE',  ( 22.81628187352648496, 31.83196800326375353, -3.434112377981050290 ) ) ;
#51898 = CARTESIAN_POINT ( 'NONE',  ( -2.913501739333854701, 4.099883984707052505E-16, 14.20427779279533098 ) ) ;
#51899 = CARTESIAN_POINT ( 'NONE',  ( -10.32896413005679470, 3.078790035174472361, 5.963430220938290560 ) ) ;
#51900 = CARTESIAN_POINT ( 'NONE',  ( 2.791683348922240793, 26.63393115100078745, 7.208316651077764092 ) ) ;
#51901 = CIRCLE ( 'NONE', #26334, 15.00000000000000000 ) ;
#51902 = CARTESIAN_POINT ( 'NONE',  ( 2.035157376598824452, 63.68868534415484106, 7.964842623401179544 ) ) ;
#51903 = CARTESIAN_POINT ( 'NONE',  ( -1.099225684535947600, 18.70696800326375353, -6.408140936763238038 ) ) ;
#51904 = CARTESIAN_POINT ( 'NONE',  ( 9.240973841163533820, 15.00000000000000000, 11.17382667070378943 ) ) ;
#51905 = CARTESIAN_POINT ( 'NONE',  ( 7.084665262690076126, 14.10535201082150358, 10.88017736071109987 ) ) ;
#51906 = CARTESIAN_POINT ( 'NONE',  ( 5.076628168052703671, 41.84226448433411605, 8.527530157486179263 ) ) ;
#51907 = CARTESIAN_POINT ( 'NONE',  ( -2.816281873526471635, 48.91530133659708213, -3.434112377981056508 ) ) ;
#51908 = CARTESIAN_POINT ( 'NONE',  ( 14.92337183194729633, 17.67559781766745175, 8.527530157486181039 ) ) ;
#51909 = CARTESIAN_POINT ( 'NONE',  ( 6.204703633549690345, 5.762082168247301794, -14.16423886937410259 ) ) ;
#51910 = CARTESIAN_POINT ( 'NONE',  ( 0.1532563361054082862, 36.21726448433410894, 2.638427012816831674 ) ) ;
#51911 = CARTESIAN_POINT ( 'NONE',  ( 19.42250999205614193, 15.14701867748817143, 5.440088680355555262 ) ) ;
#51912 = DIRECTION ( 'NONE',  ( 0.000000000000000000, -1.000000000000000000, -0.000000000000000000 ) ) ;
#51913 = CARTESIAN_POINT ( 'NONE',  ( 14.92337183194729633, 42.67559781766745886, 8.527530157486181039 ) ) ;
#51914 = CARTESIAN_POINT ( 'NONE',  ( 2.035157376598822676, 32.43868534415483396, -7.964842623401177768 ) ) ;
#51915 = EDGE_CURVE ( 'NONE', #44442, #66734, #80593, .T. ) ;
#51916 = CARTESIAN_POINT ( 'NONE',  ( 19.42250999205614548, 10.98035201082150536, -5.440088680355545492 ) ) ;
#51917 = ORIENTED_EDGE ( 'NONE', *, *, #34321, .F. ) ;
#51918 = CARTESIAN_POINT ( 'NONE',  ( 7.084665262690076126, 22.02201867748817321, -10.88017736071110164 ) ) ;
#51919 = EDGE_CURVE ( 'NONE', #6963, #8562, #21551, .T. ) ;
#51920 = CARTESIAN_POINT ( 'NONE',  ( 19.38216949554541202, 45.99863466993041072, 9.382169495545424454 ) ) ;
#51921 = CARTESIAN_POINT ( 'NONE',  ( 0.5774900079438607392, 28.48035201082150891, 5.440088680355550821 ) ) ;
#51923 = CARTESIAN_POINT ( 'NONE',  ( 2.035157376598824452, 33.68868534415484106, 7.964842623401179544 ) ) ;
#51922 = CARTESIAN_POINT ( 'NONE',  ( 1.959929470562281395, 45.51528370094808196, -5.767676674365853629 ) ) ;
#51924 = EDGE_LOOP ( 'NONE', ( #48721, #39393, #8084, #95438 ) ) ;
#51925 = CARTESIAN_POINT ( 'NONE',  ( 2.791683348922237240, 55.38393115100078745, -7.208316651077763204 ) ) ;
#51926 = CARTESIAN_POINT ( 'NONE',  ( 4.559911319644449179, 38.89701867748817676, 9.422509992056141925 ) ) ;
#51927 = CARTESIAN_POINT ( 'NONE',  ( 4.691428608706885051, -2.693193260553968127, 4.000000000000000000 ) ) ;
#51928 = B_SPLINE_CURVE_WITH_KNOTS ( 'NONE', 3,
 ( #10208, #40701, #2727, #16724 ),
 .UNSPECIFIED., .F., .F.,
 ( 4, 4 ),
 ( 5.204893179191170684E-17, 0.002562518741975298216 ),
 .UNSPECIFIED. ) ;
#51929 = FILL_AREA_STYLE_COLOUR ( '', #27603 ) ;
#51930 = CARTESIAN_POINT ( 'NONE',  ( 2.313926553644108641E-17, 1.840000000000001412, 0.000000000000000000 ) ) ;
#51931 = CARTESIAN_POINT ( 'NONE',  ( 10.00000000000000178, 43.05374883491397497, 14.16423886937410082 ) ) ;
#51932 = CARTESIAN_POINT ( 'NONE',  ( 4.559911319644449179, 57.23035201082150536, -9.422509992056141925 ) ) ;
#51933 = DIRECTION ( 'NONE',  ( 0.000000000000000000, 0.000000000000000000, 1.000000000000000000 ) ) ;
#51934 = PRESENTATION_LAYER_ASSIGNMENT (  '', '', ( #10389 ) ) ;
#51935 = LINE ( 'NONE', #75412, #55650 ) ;
#51936 = CARTESIAN_POINT ( 'NONE',  ( 0.1532563361054083140, 66.00893115100079456, 1.131784320476157264E-15 ) ) ;
#51937 = PRESENTATION_STYLE_ASSIGNMENT (( #26111 ) ) ;
#51938 = CARTESIAN_POINT ( 'NONE',  ( 0.1532563361054083140, 26.00893115100078745, 1.131784320476157264E-15 ) ) ;
#51939 = ORIENTED_EDGE ( 'NONE', *, *, #31843, .T. ) ;
#51940 = CARTESIAN_POINT ( 'NONE',  ( 12.63842701281683034, 22.46726448433411605, 9.846743663894596210 ) ) ;
#51941 = CARTESIAN_POINT ( 'NONE',  ( 12.81628187352647252, -18.16803199673624292, -3.434112377981059172 ) ) ;
#51942 = CARTESIAN_POINT ( 'NONE',  ( 12.91533473730993009, 31.60535201082150891, -10.88017736071109987 ) ) ;
#51943 = CARTESIAN_POINT ( 'NONE',  ( 19.84674366389459266, 18.71726448433411960, -2.638427012816827677 ) ) ;
#51944 = CARTESIAN_POINT ( 'NONE',  ( -1.099225684535947600, 14.54030133659708568, 6.408140936763237150 ) ) ;
#51946 = CARTESIAN_POINT ( 'NONE',  ( 4.559911319644449179, 62.23035201082150536, -9.422509992056141925 ) ) ;
#51945 = CARTESIAN_POINT ( 'NONE',  ( 0.000000000000000000, 15.00000000000000000, 0.000000000000000000 ) ) ;
#51948 = CARTESIAN_POINT ( 'NONE',  ( 16.40814093676323893, 60.79030133659709634, 11.09922568453595026 ) ) ;
#51947 = CARTESIAN_POINT ( 'NONE',  ( 2.035157376598822676, 32.43868534415483396, -7.964842623401177768 ) ) ;
#51949 = CARTESIAN_POINT ( 'NONE',  ( 6.204703633549690345, 42.84541550158063217, 14.16423886937410082 ) ) ;
#51950 = EDGE_CURVE ( 'NONE', #74051, #46208, #66220, .T. ) ;
#51951 = AXIS2_PLACEMENT_3D ( 'NONE', #41527, #71530, #78521 ) ;
#51952 = CARTESIAN_POINT ( 'NONE',  ( 6.432108699068925795, -88.20011490510430008, -3.750000000000000000 ) ) ;
#51953 = EDGE_LOOP ( 'NONE', ( #46872, #24424, #34669, #42975, #29138 ) ) ;
#51954 = CARTESIAN_POINT ( 'NONE',  ( 6.565887622018943937, 10.16530133659708746, 12.81628187352647430 ) ) ;
#51955 = CARTESIAN_POINT ( 'NONE',  ( 19.42250999205614193, 5.147018677488171434, 5.440088680355555262 ) ) ;
#51956 = EDGE_CURVE ( 'NONE', #59823, #32731, #82215, .T. ) ;
#51957 = CARTESIAN_POINT ( 'NONE',  ( 15.44008868035555260, 49.73035201082150536, 9.422509992056143702 ) ) ;
#51958 = DIRECTION ( 'NONE',  ( -0.08715574274765112983, -0.9961946980917461003, -0.000000000000000000 ) ) ;
#51959 = EDGE_LOOP ( 'NONE', ( #85832, #22655, #66185, #17130 ) ) ;
#51960 = CARTESIAN_POINT ( 'NONE',  ( -0.8801773607111009756, 63.06368534415484106, 1.068504757029289695E-15 ) ) ;
#51961 =( REPRESENTATION_RELATIONSHIP ('NONE','NONE', #61309, #19841 ) REPRESENTATION_RELATIONSHIP_WITH_TRANSFORMATION ( #60213 )SHAPE_REPRESENTATION_RELATIONSHIP( ) );
#51962 = CARTESIAN_POINT ( 'NONE',  ( 18.52753015748618282, 38.92559781766745175, -4.923371831947291888 ) ) ;
#51963 = CARTESIAN_POINT ( 'NONE',  ( 5.076628168052704559, 30.17559781766745175, -8.527530157486179263 ) ) ;
#51964 = CARTESIAN_POINT ( 'NONE',  ( 0.1532563361054100626, 20.80059781766744464, -2.638427012816831230 ) ) ;
#51965 = VECTOR ( 'NONE', #93789, 1000.000000000000000 ) ;
#51966 = CARTESIAN_POINT ( 'NONE',  ( -6.606690058644155705, -50.93246948813188624, 2.500000000001612044 ) ) ;
#51968 = CARTESIAN_POINT ( 'NONE',  ( 5.500000000000000000, 11.00000000000000000, 5.000000000000000000 ) ) ;
#51967 = CARTESIAN_POINT ( 'NONE',  ( 2.791683348922237240, 5.383931151000785675, -7.208316651077763204 ) ) ;
#51969 = CARTESIAN_POINT ( 'NONE',  ( 9.511407825468095822, -15.49433182432920120, 4.000000000000000000 ) ) ;
#51971 = ORIENTED_EDGE ( 'NONE', *, *, #20069, .T. ) ;
#51970 = CARTESIAN_POINT ( 'NONE',  ( 18.52753015748617571, 38.09226448433412315, 4.923371831947298993 ) ) ;
#51972 = CARTESIAN_POINT ( 'NONE',  ( 10.00000000000000000, 57.87363466993042493, -12.81628187352647608 ) ) ;
#51973 = CARTESIAN_POINT ( 'NONE',  ( 18.29284471827481440, 55.40189080397284016, -6.499999999999946709 ) ) ;
#51974 = CARTESIAN_POINT ( 'NONE',  ( 0.6178305044545818747, 3.498634669930420049, -9.382169495545419124 ) ) ;
#51975 = AXIS2_PLACEMENT_3D ( 'NONE', #63814, #8375, #48333 ) ;
#51976 = CARTESIAN_POINT ( 'NONE',  ( 4.559911319644449179, 12.23035201082150536, -9.422509992056141925 ) ) ;
#51977 = EDGE_CURVE ( 'NONE', #19380, #80716, #80555, .T. ) ;
#51978 = CARTESIAN_POINT ( 'NONE',  ( 17.08211943468705130, 33.47041550158063927, 12.26659068614894998 ) ) ;
#51979 = CARTESIAN_POINT ( 'NONE',  ( 11.62719953690058539, 0.3640475087720986269, 9.476720473301883274 ) ) ;
#51980 = CARTESIAN_POINT ( 'NONE',  ( 24.16423886937410614, 24.51208216824730002, -3.795296366450302550 ) ) ;
#51981 = CARTESIAN_POINT ( 'NONE',  ( 10.00000000000000178, 48.05374883491396787, 14.16423886937410082 ) ) ;
#51982 = CARTESIAN_POINT ( 'NONE',  ( -4.164238869374099927, 7.012082168247302683, 3.795296366450308767 ) ) ;
#51983 = CARTESIAN_POINT ( 'NONE',  ( 17.08211943468705130, 13.47041550158063572, 12.26659068614894998 ) ) ;
#51984 = CARTESIAN_POINT ( 'NONE',  ( -0.8801773607111009756, 48.06368534415484817, 1.068504757029289695E-15 ) ) ;
#51985 = DIRECTION ( 'NONE',  ( 0.000000000000000000, 0.000000000000000000, 1.000000000000000000 ) ) ;
#51986 = VERTEX_POINT ( 'NONE', #15776 ) ;
#51987 = CARTESIAN_POINT ( 'NONE',  ( 17.20831665107776587, 34.13393115100078745, -7.208316651077762316 ) ) ;
#51989 = CARTESIAN_POINT ( 'NONE',  ( 19.84674366389459621, 23.50893115100078390, 7.409399052514197653E-17 ) ) ;
#51988 = CARTESIAN_POINT ( 'NONE',  ( 19.42250999205614193, 65.14701867748817676, 5.440088680355555262 ) ) ;
#51990 = CARTESIAN_POINT ( 'NONE',  ( 17.96484262340118221, 16.18868534415483396, -7.964842623401177768 ) ) ;
#51991 = CARTESIAN_POINT ( 'NONE',  ( 0.6178305044545838731, 59.74863466993041783, 9.382169495545420901 ) ) ;
#51992 = CARTESIAN_POINT ( 'NONE',  ( 17.20831665107776587, 54.13393115100079456, -7.208316651077762316 ) ) ;
#51993 = CARTESIAN_POINT ( 'NONE',  ( 18.00000000000000000, 78.50170875210521615, 3.769097870606325174 ) ) ;
#51994 = CARTESIAN_POINT ( 'NONE',  ( 17.20831665107776587, 29.13393115100078390, -7.208316651077762316 ) ) ;
#51995 = CARTESIAN_POINT ( 'NONE',  ( 22.81628187352647785, 46.62363466993041783, 6.195893100308588602E-16 ) ) ;
#51996 = CARTESIAN_POINT ( 'NONE',  ( -3.795296366450322534, -19.23791783175269998, -14.16423886937409904 ) ) ;
#51997 = CARTESIAN_POINT ( 'NONE',  ( 10.00000000000000000, 36.81368534415484106, -10.88017736071110342 ) ) ;
#51998 = CARTESIAN_POINT ( 'NONE',  ( 7.361572987183170547, 37.05059781766744464, 9.846743663894590881 ) ) ;
#51999 = CARTESIAN_POINT ( 'NONE',  ( 17.08211943468705840, 30.13708216824730357, -12.26659068614894466 ) ) ;
#52000 = VERTEX_POINT ( 'NONE', #76750 ) ;
#52001 = CARTESIAN_POINT ( 'NONE',  ( 6.204703633549690345, 5.762082168247301794, -14.16423886937410259 ) ) ;
#52002 = AXIS2_PLACEMENT_3D ( 'NONE', #43723, #82214, #57732 ) ;
#52003 = CARTESIAN_POINT ( 'NONE',  ( 20.88017736071110519, 65.56368534415483396, 2.639326808657452039E-16 ) ) ;
#52004 = CARTESIAN_POINT ( 'NONE',  ( 17.96484262340118221, 59.93868534415484106, 7.964842623401181321 ) ) ;
#52005 = CARTESIAN_POINT ( 'NONE',  ( 20.36894250292379738, 54.92874883491396076, -10.36894250292379027 ) ) ;
#52006 = CARTESIAN_POINT ( 'NONE',  ( 3.591859063236763294, 3.290301336597087012, -11.09922568453595026 ) ) ;
#52007 = FACE_OUTER_BOUND ( 'NONE', #1164, .T. ) ;
#52008 = CARTESIAN_POINT ( 'NONE',  ( 17.96484262340118221, 61.18868534415482685, -7.964842623401177768 ) ) ;
#52009 = CARTESIAN_POINT ( 'NONE',  ( -6.767445849361066301, 0.5000000000000004441, -13.38662304974505801 ) ) ;
#52010 = DIRECTION ( 'NONE',  ( -0.5664062369248369366, 0.000000000000000000, 0.8241261886220129229 ) ) ;
#52011 = CARTESIAN_POINT ( 'NONE',  ( 20.88017736071110164, 10.35535201082150714, 2.915334737309930979 ) ) ;
#52012 = CARTESIAN_POINT ( 'NONE',  ( 20.88017736071110519, 15.56368534415483751, 2.639326808657452039E-16 ) ) ;
#52013 = CARTESIAN_POINT ( 'NONE',  ( 18.52753015748618282, 48.92559781766745886, -4.923371831947291888 ) ) ;
#52014 = CARTESIAN_POINT ( 'NONE',  ( 22.81628187352647785, 56.62363466993042493, 6.195893100308588602E-16 ) ) ;
#52015 = CARTESIAN_POINT ( 'NONE',  ( -14.82269085861171298, 0.3640475087720979608, 2.299529454046859822 ) ) ;
#52016 = ORIENTED_EDGE ( 'NONE', *, *, #30041, .T. ) ;
#52017 = CARTESIAN_POINT ( 'NONE',  ( 10.00000000000000000, 16.81368534415483751, -10.88017736071110342 ) ) ;
#52018 = CARTESIAN_POINT ( 'NONE',  ( -2.816281873526471635, 3.915301336597087456, -3.434112377981056508 ) ) ;
#52019 = CARTESIAN_POINT ( 'NONE',  ( 12.25993886608599581, 0.5000000000000004441, 8.642563219313704082 ) ) ;
#52020 = CARTESIAN_POINT ( 'NONE',  ( 5.076628168052703671, 16.84226448433411960, 8.527530157486179263 ) ) ;
#52021 = CARTESIAN_POINT ( 'NONE',  ( 12.63842701281683922, 44.55059781766745175, -9.846743663894590881 ) ) ;
#52022 = CARTESIAN_POINT ( 'NONE',  ( -0.8801773607110991993, 32.85535201082151247, -2.915334737309923874 ) ) ;
#52023 = CARTESIAN_POINT ( 'NONE',  ( 3.591859063236761518, 14.95696800326375531, 11.09922568453594849 ) ) ;
#52025 = LINE ( 'NONE', #7021, #36817 ) ;
#52024 = CARTESIAN_POINT ( 'NONE',  ( 15.44008868035555793, 51.39701867748816966, -9.422509992056140149 ) ) ;
#52026 = CARTESIAN_POINT ( 'NONE',  ( 0.6178305044545818747, 53.49863466993041072, -9.382169495545419124 ) ) ;
#52027 = VERTEX_POINT ( 'NONE', #8267 ) ;
#52028 = CARTESIAN_POINT ( 'NONE',  ( 0.5774900079438590739, 67.64701867748817676, -5.440088680355550821 ) ) ;
#52029 = CARTESIAN_POINT ( 'NONE',  ( 21.09922568453595559, 37.04030133659708923, -6.408140936763230044 ) ) ;
#52030 = CARTESIAN_POINT ( 'NONE',  ( 14.92337183194729633, 7.675597817667451750, 8.527530157486181039 ) ) ;
#52031 = CARTESIAN_POINT ( 'NONE',  ( 19.42250999205614193, 35.14701867748816966, 5.440088680355555262 ) ) ;
#52032 = CARTESIAN_POINT ( 'NONE',  ( 14.92337183194729988, 64.34226448433412315, -8.527530157486177487 ) ) ;
#52033 = CARTESIAN_POINT ( 'NONE',  ( 0.1532563361054083140, 51.00893115100078745, 1.131784320476157264E-15 ) ) ;
#52034 = CARTESIAN_POINT ( 'NONE',  ( 7.361572987183170547, 12.05059781766744997, 9.846743663894590881 ) ) ;
#52035 = CARTESIAN_POINT ( 'NONE',  ( 19.84674366389459621, 8.508931151000785675, 7.409399052514197653E-17 ) ) ;
#52036 = LINE ( 'NONE', #58041, #50584 ) ;
#52037 = CARTESIAN_POINT ( 'NONE',  ( 10.00000000000000178, 43.05374883491397497, 14.16423886937410082 ) ) ;
#52038 = AXIS2_PLACEMENT_3D ( 'NONE', #28242, #42273, #88746 ) ;
#52039 = CARTESIAN_POINT ( 'NONE',  ( 20.32896413005680358, 24.74545670184113888, 5.963430220938287007 ) ) ;
#52040 = EDGE_CURVE ( 'NONE', #73542, #3919, #787, .T. ) ;
#52041 = CARTESIAN_POINT ( 'NONE',  ( -6.607869636366940469, -50.96183896326462559, -4.000000000000000000 ) ) ;
#52042 = ORIENTED_EDGE ( 'NONE', *, *, #78535, .F. ) ;
#52043 = ORIENTED_EDGE ( 'NONE', *, *, #44520, .T. ) ;
#52044 = CARTESIAN_POINT ( 'NONE',  ( 10.00000000000000000, 65.55374883491396076, -14.16423886937410082 ) ) ;
#52045 = CARTESIAN_POINT ( 'NONE',  ( -0.8801773607110991993, 2.855352010821504471, -2.915334737309923874 ) ) ;
#52046 = CARTESIAN_POINT ( 'NONE',  ( 7.361572987183170547, 27.05059781766745175, 9.846743663894590881 ) ) ;
#52047 = CARTESIAN_POINT ( 'NONE',  ( 16.40814093676324603, 27.45696800326375708, -11.09922568453594671 ) ) ;
#52048 = DIRECTION ( 'NONE',  ( -0.06975647374412534407, -0.9975640502598241977, 0.000000000000000000 ) ) ;
#52050 = CARTESIAN_POINT ( 'NONE',  ( 10.00000000000000000, 0.5537488349139675359, -14.16423886937410082 ) ) ;
#52049 = CARTESIAN_POINT ( 'NONE',  ( -10.09777502097891499, 14.95077488074853456, 10.75551206493373257 ) ) ;
#52051 = CARTESIAN_POINT ( 'NONE',  ( 12.91533473730993009, 11.60535201082150536, -10.88017736071109987 ) ) ;
#52052 = CARTESIAN_POINT ( 'NONE',  ( -2.266590686148945544, 62.22041550158063927, 7.082119434687048631 ) ) ;
#52053 = CARTESIAN_POINT ( 'NONE',  ( 12.63842701281683922, 29.55059781766745175, -9.846743663894590881 ) ) ;
#52054 = CARTESIAN_POINT ( 'NONE',  ( 8.629999999999995453, 41.24999999999999289, -6.500000000000000888 ) ) ;
#52055 = CARTESIAN_POINT ( 'NONE',  ( 2.791683348922240793, 16.63393115100078745, 7.208316651077764092 ) ) ;
#52056 = LINE ( 'NONE', #5078, #73728 ) ;
#52057 = CARTESIAN_POINT ( 'NONE',  ( -3.469446951953614189E-15, 9.758931151000794557, -9.846743663894594434 ) ) ;
#52058 = VERTEX_POINT ( 'NONE', #23778 ) ;
#52059 = ORIENTED_EDGE ( 'NONE', *, *, #97004, .F. ) ;
#52060 = CARTESIAN_POINT ( 'NONE',  ( 1.175037534397233241, 15.00000000000000711, -14.57833316477036689 ) ) ;
#52061 = ORIENTED_EDGE ( 'NONE', *, *, #34522, .T. ) ;
#52062 = CARTESIAN_POINT ( 'NONE',  ( 13.79529636645030344, 18.26208216824730002, 14.16423886937410614 ) ) ;
#52064 = CARTESIAN_POINT ( 'NONE',  ( 2.035157376598824452, 43.68868534415484106, 7.964842623401179544 ) ) ;
#52063 = CARTESIAN_POINT ( 'NONE',  ( 10.00000000000000178, 19.31368534415484106, 10.88017736071110342 ) ) ;
#52066 = CARTESIAN_POINT ( 'NONE',  ( 21.09922568453594849, 21.20696800326375353, 6.408140936763242479 ) ) ;
#52065 = CARTESIAN_POINT ( 'NONE',  ( 2.791683348922240793, 66.63393115100079456, 7.208316651077764092 ) ) ;
#52067 = CARTESIAN_POINT ( 'NONE',  ( 6.204703633549690345, 2.845415501580634388, 14.16423886937410082 ) ) ;
#52068 = AXIS2_PLACEMENT_3D ( 'NONE', #72436, #3964, #81423 ) ;
#52069 = CIRCLE ( 'NONE', #69621, 62.00000000000000000 ) ;
#52070 = ADVANCED_FACE ( 'NONE', ( #54243 ), #86662, .T. ) ;
#52072 = CARTESIAN_POINT ( 'NONE',  ( 22.81628187352648496, 26.83196800326374998, -3.434112377981050290 ) ) ;
#52071 = TOROIDAL_SURFACE ( 'NONE', #21744, 14.49999999999999822, 0.5000000000000000000 ) ;
#52073 = ORIENTED_EDGE ( 'NONE', *, *, #15680, .F. ) ;
#52074 = CARTESIAN_POINT ( 'NONE',  ( 12.63842701281683034, 32.46726448433412315, 9.846743663894596210 ) ) ;
#52075 = EDGE_CURVE ( 'NONE', #23697, #85150, #27903, .T. ) ;
#52076 = CARTESIAN_POINT ( 'NONE',  ( 19.42250999205614193, 10.14701867748816966, 5.440088680355555262 ) ) ;
#52077 = ORIENTED_EDGE ( 'NONE', *, *, #10978, .T. ) ;
#52078 = CARTESIAN_POINT ( 'NONE',  ( 24.16423886937409904, 64.09541550158064638, 3.795296366450317205 ) ) ;
#52079 = ORIENTED_EDGE ( 'NONE', *, *, #58486, .F. ) ;
#52080 = CARTESIAN_POINT ( 'NONE',  ( 17.96484262340118221, 44.93868534415483396, 7.964842623401181321 ) ) ;
#52081 = CARTESIAN_POINT ( 'NONE',  ( 19.42250999205614193, 65.14701867748817676, 5.440088680355555262 ) ) ;
#52082 = CARTESIAN_POINT ( 'NONE',  ( -0.8801773607111008646, 63.27201867748817676, 2.915334737309923430 ) ) ;
#52083 = CARTESIAN_POINT ( 'NONE',  ( 19.42250999205614193, 60.14701867748817676, 5.440088680355555262 ) ) ;
#52084 = CARTESIAN_POINT ( 'NONE',  ( -14.97687855664607248, 0.5000000000000004441, -0.8325315005902533816 ) ) ;
#52086 = ORIENTED_EDGE ( 'NONE', *, *, #38436, .T. ) ;
#52085 = CARTESIAN_POINT ( 'NONE',  ( 10.76914169791313292, -96.07995077553798069, 4.000000000000000000 ) ) ;
#52087 = CARTESIAN_POINT ( 'NONE',  ( 0.1532563361054083140, 31.00893115100078390, 1.131784320476157264E-15 ) ) ;
#52088 = ORIENTED_EDGE ( 'NONE', *, *, #30883, .F. ) ;
#52089 = CARTESIAN_POINT ( 'NONE',  ( 0.1532563361054100626, 60.80059781766744464, -2.638427012816831230 ) ) ;
#52090 = ORIENTED_EDGE ( 'NONE', *, *, #73027, .F. ) ;
#52091 = EDGE_CURVE ( 'NONE', #8762, #42622, #6191, .T. ) ;
#52092 = CARTESIAN_POINT ( 'NONE',  ( -11.54609836565341929, 12.78764854742128598, -0.3568064872451662262 ) ) ;
#52093 = CYLINDRICAL_SURFACE ( 'NONE', #53781, 15.00000000000000000 ) ;
#52094 = DIRECTION ( 'NONE',  ( 0.000000000000000000, 0.000000000000000000, 1.000000000000000000 ) ) ;
#52095 = CARTESIAN_POINT ( 'NONE',  ( 20.88017736071110519, 10.56368534415483929, 2.639326808657452039E-16 ) ) ;
#52096 = PLANE ( 'NONE',  #69070 ) ;
#52097 = ORIENTED_EDGE ( 'NONE', *, *, #22814, .F. ) ;
#52098 = CARTESIAN_POINT ( 'NONE',  ( 14.49999999999999822, 60.50000000000000000, -5.000000000000000000 ) ) ;
#52099 = CARTESIAN_POINT ( 'NONE',  ( 19.84674366389459621, 43.50893115100078745, 7.409399052514197653E-17 ) ) ;
#52100 = CARTESIAN_POINT ( 'NONE',  ( -13.34343830728409053, 14.63595249122790598, 6.852200678592508254 ) ) ;
#52101 = AXIS2_PLACEMENT_3D ( 'NONE', #77577, #25102, #16107 ) ;
#52102 = CARTESIAN_POINT ( 'NONE',  ( 13.43411237798106583, 17.66530133659708923, -12.81628187352647252 ) ) ;
#52104 = EDGE_CURVE ( 'NONE', #31975, #30617, #59193, .T. ) ;
#52103 = CARTESIAN_POINT ( 'NONE',  ( 7.361572987183170547, 17.05059781766745530, 9.846743663894590881 ) ) ;
#52105 = CARTESIAN_POINT ( 'NONE',  ( -11.48952521350030587, 4.186587853438871531E-16, 8.845383562533662314 ) ) ;
#52106 = CARTESIAN_POINT ( 'NONE',  ( -1.099225684535947600, -1.293031996736246469, -6.408140936763238038 ) ) ;
#52107 = CARTESIAN_POINT ( 'NONE',  ( 20.15039907845753930, 0.07447313448805115144, 6.262539305110068177 ) ) ;
#52108 = VERTEX_POINT ( 'NONE', #13685 ) ;
#52109 = ORIENTED_EDGE ( 'NONE', *, *, #4559, .F. ) ;
#52110 = CARTESIAN_POINT ( 'NONE',  ( 0.5774900079438607392, 8.480352010821505360, 5.440088680355550821 ) ) ;
#52111 = CARTESIAN_POINT ( 'NONE',  ( -4.164238869374099927, 22.01208216824730357, 3.795296366450308767 ) ) ;
#52112 = CARTESIAN_POINT ( 'NONE',  ( 1.472469842513823179, 26.42559781766745175, 4.923371831947296329 ) ) ;
#52113 = CARTESIAN_POINT ( 'NONE',  ( 2.035157376598824452, 53.68868534415484817, 7.964842623401179544 ) ) ;
#52115 = FACE_OUTER_BOUND ( 'NONE', #43909, .T. ) ;
#52114 = CARTESIAN_POINT ( 'NONE',  ( 22.81628187352648496, 36.83196800326376064, -3.434112377981050290 ) ) ;
#52116 = CARTESIAN_POINT ( 'NONE',  ( 0.5774900079438607392, 18.48035201082150536, 5.440088680355550821 ) ) ;
#52117 = DIRECTION ( 'NONE',  ( 0.8070303256584298035, -0.5905099943842175847, 0.000000000000000000 ) ) ;
#52118 = CARTESIAN_POINT ( 'NONE',  ( -0.9082943533638283551, 15.00000000000000000, 14.47152380945581918 ) ) ;
#52119 = CARTESIAN_POINT ( 'NONE',  ( 10.00000000000000178, 67.25893115100079456, 9.846743663894594434 ) ) ;
#52120 = CARTESIAN_POINT ( 'NONE',  ( 0.1532563361054083140, 21.00893115100078745, 1.131784320476157264E-15 ) ) ;
#52121 = CARTESIAN_POINT ( 'NONE',  ( 5.440088680355556150, -10.26964798917848931, 9.422509992056138373 ) ) ;
#52122 = CARTESIAN_POINT ( 'NONE',  ( 10.00000000000000000, 32.87363466993042493, -12.81628187352647608 ) ) ;
#52123 = CARTESIAN_POINT ( 'NONE',  ( 14.62232599144297396, 2.134523027080836854E-16, -0.3548652576988654550 ) ) ;
#52125 = PLANE ( 'NONE',  #49589 ) ;
#52124 = CARTESIAN_POINT ( 'NONE',  ( 7.084665262690076126, 37.02201867748817676, -10.88017736071110164 ) ) ;
#52126 = CARTESIAN_POINT ( 'NONE',  ( 6.757727703329182489, -58.31565150548815524, -3.750000000000000444 ) ) ;
#52127 = CARTESIAN_POINT ( 'NONE',  ( 7.084665262690076126, 57.02201867748817676, -10.88017736071110164 ) ) ;
#52128 = CARTESIAN_POINT ( 'NONE',  ( 10.00000000000000000, 36.81368534415484106, -10.88017736071110342 ) ) ;
#52129 = CARTESIAN_POINT ( 'NONE',  ( 10.00000000000000000, 41.81368534415484106, -10.88017736071110342 ) ) ;
#52130 = CARTESIAN_POINT ( 'NONE',  ( 1.472469842513823179, 66.42559781766745175, 4.923371831947296329 ) ) ;
#52131 = CARTESIAN_POINT ( 'NONE',  ( -0.8801773607110991993, 52.85535201082151247, -2.915334737309923874 ) ) ;
#52132 = AXIS2_PLACEMENT_3D ( 'NONE', #91058, #51594, #46066 ) ;
#52133 = UNCERTAINTY_MEASURE_WITH_UNIT (LENGTH_MEASURE( 1.000000000000000082E-05 ), #30053, 'distance_accuracy_value', 'NONE');
#52134 = CARTESIAN_POINT ( 'NONE',  ( 2.791683348922240793, 31.63393115100078745, 7.208316651077764092 ) ) ;
#52135 = CARTESIAN_POINT ( 'NONE',  ( 15.44008868035555793, 11.39701867748817143, -9.422509992056140149 ) ) ;
#52136 = CARTESIAN_POINT ( 'NONE',  ( 0.6178305044545818747, 13.49863466993041783, -9.382169495545419124 ) ) ;
#52137 = VERTEX_POINT ( 'NONE', #97706 ) ;
#52138 = CARTESIAN_POINT ( 'NONE',  ( 17.96484262340118221, 24.93868534415484461, 7.964842623401181321 ) ) ;
#52139 = DIRECTION ( 'NONE',  ( 0.000000000000000000, 1.000000000000000000, 0.000000000000000000 ) ) ;
#52140 = CARTESIAN_POINT ( 'NONE',  ( 19.42250999205614548, 25.98035201082150891, -5.440088680355545492 ) ) ;
#52141 = CARTESIAN_POINT ( 'NONE',  ( 4.559911319644449179, 67.23035201082150536, -9.422509992056141925 ) ) ;
#52142 = CARTESIAN_POINT ( 'NONE',  ( 6.204703633549690345, 42.84541550158063217, 14.16423886937410082 ) ) ;
#52143 = CARTESIAN_POINT ( 'NONE',  ( 7.361572987183170547, 17.05059781766745530, 9.846743663894590881 ) ) ;
#52144 = CARTESIAN_POINT ( 'NONE',  ( 7.084665262690076126, 47.02201867748818387, -10.88017736071110164 ) ) ;
#52145 = FACE_OUTER_BOUND ( 'NONE', #29485, .T. ) ;
#52146 = FILL_AREA_STYLE_COLOUR ( '', #23436 ) ;
#52147 = ADVANCED_FACE ( 'NONE', ( #83668 ), #98701, .F. ) ;
#52149 = EDGE_LOOP ( 'NONE', ( #47009, #29514, #77272, #62578 ) ) ;
#52148 = CIRCLE ( 'NONE', #24983, 2.999999999999999112 ) ;
#52150 = CARTESIAN_POINT ( 'NONE',  ( -14.29730467489527967, 15.00000000000000000, -2.416004766803415471 ) ) ;
#52151 = CARTESIAN_POINT ( 'NONE',  ( 18.52753015748618282, 43.92559781766745175, -4.923371831947291888 ) ) ;
#52152 = ORIENTED_EDGE ( 'NONE', *, *, #73420, .T. ) ;
#52153 = VERTEX_POINT ( 'NONE', #22682 ) ;
#52154 = CARTESIAN_POINT ( 'NONE',  ( -9.402796353261203777, 0.5000000000000004441, 11.68706210897750708 ) ) ;
#52155 = CARTESIAN_POINT ( 'NONE',  ( -2.266590686148945544, 22.22041550158063572, 7.082119434687048631 ) ) ;
#52157 = CIRCLE ( 'NONE', #44145, 0.2500000000000002220 ) ;
#52156 = CARTESIAN_POINT ( 'NONE',  ( 17.08211943468705130, 23.47041550158063572, 12.26659068614894998 ) ) ;
#52158 = CARTESIAN_POINT ( 'NONE',  ( 10.00000000000000178, 54.31368534415484106, 10.88017736071110342 ) ) ;
#52159 = CARTESIAN_POINT ( 'NONE',  ( 4.559911319644449179, 3.897018677488171434, 9.422509992056141925 ) ) ;
#52160 = CARTESIAN_POINT ( 'NONE',  ( 16.40814093676323893, 0.7903013365970867898, 11.09922568453595026 ) ) ;
#52161 = CARTESIAN_POINT ( 'NONE',  ( 19.84674366389459266, 43.71726448433410894, -2.638427012816827677 ) ) ;
#52162 = LINE ( 'NONE', #95696, #70647 ) ;
#52164 = CARTESIAN_POINT ( 'NONE',  ( -2.816281873526471635, 3.915301336597087456, -3.434112377981056508 ) ) ;
#52163 = CARTESIAN_POINT ( 'NONE',  ( 19.42250999205614193, 45.14701867748817676, 5.440088680355555262 ) ) ;
#52165 = CARTESIAN_POINT ( 'NONE',  ( 2.917880565312950480, 10.97041550158063572, -12.26659068614894821 ) ) ;
#52166 = CARTESIAN_POINT ( 'NONE',  ( -0.8801773607111008646, 8.272018677488171434, 2.915334737309923430 ) ) ;
#52167 = CARTESIAN_POINT ( 'NONE',  ( 2.035157376598824452, 13.68868534415483751, 7.964842623401179544 ) ) ;
#52168 = CARTESIAN_POINT ( 'NONE',  ( 15.44008868035555793, 46.39701867748817676, -9.422509992056140149 ) ) ;
#52169 = CARTESIAN_POINT ( 'NONE',  ( 6.565887622018943937, 45.16530133659708923, 12.81628187352647430 ) ) ;
#52170 = CARTESIAN_POINT ( 'NONE',  ( -3.469446951953614189E-15, -30.24106884899920900, -9.846743663894594434 ) ) ;
#52171 = ORIENTED_EDGE ( 'NONE', *, *, #95985, .T. ) ;
#52172 = CARTESIAN_POINT ( 'NONE',  ( -10.00000000000000000, 82.00000000000000000, -5.000000000000000000 ) ) ;
#52173 = ORIENTED_EDGE ( 'NONE', *, *, #94394, .F. ) ;
#52174 = VERTEX_POINT ( 'NONE', #29172 ) ;
#52175 = MECHANICAL_DESIGN_GEOMETRIC_PRESENTATION_REPRESENTATION (  '', ( #53747 ), #68097 ) ;
#52176 = DIRECTION ( 'NONE',  ( -0.3007057995042767273, 0.000000000000000000, 0.9537169507482258224 ) ) ;
#52178 = CARTESIAN_POINT ( 'NONE',  ( 20.88017736071110519, 10.56368534415483929, 2.639326808657452039E-16 ) ) ;
#52177 = CARTESIAN_POINT ( 'NONE',  ( 10.00000000000000000, 40.55374883491397497, -14.16423886937410082 ) ) ;
#52180 = CARTESIAN_POINT ( 'NONE',  ( 18.52753015748618282, 43.92559781766745175, -4.923371831947291888 ) ) ;
#52179 = CARTESIAN_POINT ( 'NONE',  ( 0.1532563361054082862, 26.21726448433411605, 2.638427012816831674 ) ) ;
#52181 = CARTESIAN_POINT ( 'NONE',  ( 4.559911319644449179, 63.89701867748817676, 9.422509992056141925 ) ) ;
#52182 = CARTESIAN_POINT ( 'NONE',  ( 10.00000000000000000, -0.2410688489992152128, -9.846743663894594434 ) ) ;
#52183 = EDGE_CURVE ( 'NONE', #38304, #37672, #56666, .T. ) ;
#52184 = CARTESIAN_POINT ( 'NONE',  ( -11.09922568453595382, 18.70696800326376774, -6.408140936763226492 ) ) ;
#52185 = ORIENTED_EDGE ( 'NONE', *, *, #72820, .F. ) ;
#52186 = CARTESIAN_POINT ( 'NONE',  ( 2.917880565312948704, 37.63708216824731068, 12.26659068614894643 ) ) ;
#52187 = ADVANCED_FACE ( 'NONE', ( #30150 ), #38178, .T. ) ;
#52188 = CARTESIAN_POINT ( 'NONE',  ( -1.099225684535947600, 28.70696800326375353, -6.408140936763238038 ) ) ;
#52189 = ORIENTED_EDGE ( 'NONE', *, *, #70129, .F. ) ;
#52190 = CARTESIAN_POINT ( 'NONE',  ( 13.43411237798105340, 60.58196800326376064, 12.81628187352647963 ) ) ;
#52191 = CARTESIAN_POINT ( 'NONE',  ( 19.42250999205614193, 25.14701867748817321, 5.440088680355555262 ) ) ;
#52192 = CARTESIAN_POINT ( 'NONE',  ( 19.84674366389459621, 38.50893115100078745, 7.409399052514197653E-17 ) ) ;
#52193 = CARTESIAN_POINT ( 'NONE',  ( 19.42250999205614548, 30.98035201082150536, -5.440088680355545492 ) ) ;
#52194 =( BOUNDED_CURVE ( )  B_SPLINE_CURVE ( 2, ( #62694, #93194, #33663, #9213, #63185, #64159, #79181, #1738, #24721 ),
 .UNSPECIFIED., .F., .T. ) 
 B_SPLINE_CURVE_WITH_KNOTS ( ( 3, 2, 2, 2, 3 ),
 ( 0.8667998787605536437, 0.8690476190476190688, 0.8750000000000000000, 0.8809523809523809312, 0.8832001212394463563 ),
 .UNSPECIFIED. ) 
 CURVE ( )  GEOMETRIC_REPRESENTATION_ITEM ( )  RATIONAL_B_SPLINE_CURVE ( ( 0.9839835555609424134, 0.9871328979762474809, 1.000000000000000000, 0.9659258262890683122, 1.000000000000000000, 0.9659258262890683122, 1.000000000000000000, 0.9871328979762474809, 0.9839835555609424134 ) ) 
 REPRESENTATION_ITEM ( '' )  );
#52195 = LINE ( 'NONE', #22698, #53098 ) ;
#52196 = CARTESIAN_POINT ( 'NONE',  ( 0.1532563361054083140, 46.00893115100079456, 1.131784320476157264E-15 ) ) ;
#52197 = CARTESIAN_POINT ( 'NONE',  ( 2.791683348922240793, 46.63393115100077324, 7.208316651077764092 ) ) ;
#52199 = EDGE_LOOP ( 'NONE', ( #12063, #75944, #92749, #16287 ) ) ;
#52198 = FACE_OUTER_BOUND ( 'NONE', #83970, .T. ) ;
#52200 = CARTESIAN_POINT ( 'NONE',  ( 34.56412365047464874, 11.49999999999999645, 10.00000000000000000 ) ) ;
#52201 = CARTESIAN_POINT ( 'NONE',  ( 2.148416515056641440, 32.23726573380442062, 6.499999999999995559 ) ) ;
#52202 = CARTESIAN_POINT ( 'NONE',  ( -15.00000000000000000, 83.99999999999998579, 8.000000000000000000 ) ) ;
#52203 = AXIS2_PLACEMENT_3D ( 'NONE', #35218, #50736, #73713 ) ;
#52204 = CARTESIAN_POINT ( 'NONE',  ( -3.499999999999998668, 1.019547802438465434, -3.750000000000000000 ) ) ;
#52205 = CARTESIAN_POINT ( 'NONE',  ( 14.92337183194729633, 22.67559781766745175, 8.527530157486181039 ) ) ;
#52206 = CARTESIAN_POINT ( 'NONE',  ( 22.81628187352648496, 31.83196800326375353, -3.434112377981050290 ) ) ;
#52207 = DIRECTION ( 'NONE',  ( 0.000000000000000000, 0.000000000000000000, 1.000000000000000000 ) ) ;
#52208 = ORIENTED_EDGE ( 'NONE', *, *, #65393, .F. ) ;
#52209 = CARTESIAN_POINT ( 'NONE',  ( 2.791683348922237240, 55.38393115100078745, -7.208316651077763204 ) ) ;
#52210 = CYLINDRICAL_SURFACE ( 'NONE', #5886, 3.000000000000000888 ) ;
#52211 = CARTESIAN_POINT ( 'NONE',  ( 10.00000000000000000, 44.75893115100078745, -9.846743663894594434 ) ) ;
#52212 = CARTESIAN_POINT ( 'NONE',  ( 10.00000000000000000, 40.55374883491397497, -14.16423886937410082 ) ) ;
#52213 = CARTESIAN_POINT ( 'NONE',  ( 19.84674366389459621, 48.50893115100078745, 7.409399052514197653E-17 ) ) ;
#52214 = CARTESIAN_POINT ( 'NONE',  ( -1.099225684535947600, 48.70696800326375353, -6.408140936763238038 ) ) ;
#52215 = DIRECTION ( 'NONE',  ( 0.9970872288863209532, 0.07626964003977952655, 0.000000000000000000 ) ) ;
#52216 = CARTESIAN_POINT ( 'NONE',  ( 0.1532563361054082862, 1.217264484334117824, 2.638427012816831674 ) ) ;
#52217 = VECTOR ( 'NONE', #3426, 1000.000000000000000 ) ;
#52218 = CARTESIAN_POINT ( 'NONE',  ( -0.1503990784575323369, 4.248846992468888750, -6.262539305110070842 ) ) ;
#52219 = CARTESIAN_POINT ( 'NONE',  ( 2.791683348922240793, 46.63393115100077324, 7.208316651077764092 ) ) ;
#52221 = EDGE_CURVE ( 'NONE', #3044, #96338, #59789, .T. ) ;
#52220 = CARTESIAN_POINT ( 'NONE',  ( 15.44008868035555793, 41.39701867748817676, -9.422509992056140149 ) ) ;
#52222 = CIRCLE ( 'NONE', #80979, 0.2500000000000002220 ) ;
#52223 = APPLICATION_PROTOCOL_DEFINITION ( 'draft international standard', 'automotive_design', 1998, #98582 ) ;
#52224 = CARTESIAN_POINT ( 'NONE',  ( 19.88701968852526747, 31.79427333184086635, 6.480634945678623637 ) ) ;
#52225 = CARTESIAN_POINT ( 'NONE',  ( -0.8801773607110991993, 47.85535201082150536, -2.915334737309923874 ) ) ;
#52226 = ORIENTED_EDGE ( 'NONE', *, *, #76361, .F. ) ;
#52227 = LINE ( 'NONE', #22236, #4267 ) ;
#52228 = CARTESIAN_POINT ( 'NONE',  ( 19.42250999205614193, 10.14701867748816966, 5.440088680355555262 ) ) ;
#52230 = CARTESIAN_POINT ( 'NONE',  ( 2.035157376598824452, 48.68868534415483396, 7.964842623401179544 ) ) ;
#52229 = CARTESIAN_POINT ( 'NONE',  ( 2.791683348922237240, 65.38393115100078035, -7.208316651077763204 ) ) ;
#52231 = FILL_AREA_STYLE_COLOUR ( '', #5719 ) ;
#52232 = CARTESIAN_POINT ( 'NONE',  ( 17.96484262340118221, 56.18868534415484817, -7.964842623401177768 ) ) ;
#52233 = CARTESIAN_POINT ( 'NONE',  ( 19.72487221294570858, 70.00000000000000000, 6.000000000000000000 ) ) ;
#52235 = PLANE ( 'NONE',  #1676 ) ;
#52234 = CARTESIAN_POINT ( 'NONE',  ( 2.035157376598824452, 33.68868534415484106, 7.964842623401179544 ) ) ;
#52236 = CARTESIAN_POINT ( 'NONE',  ( 12.63842701281683034, 12.46726448433411782, 9.846743663894596210 ) ) ;
#52237 = CARTESIAN_POINT ( 'NONE',  ( 12.63842701281683922, 24.55059781766745175, -9.846743663894590881 ) ) ;
#52238 = CARTESIAN_POINT ( 'NONE',  ( 64.56412365047461321, 11.99999999999999467, -7.000000000000000888 ) ) ;
#52239 = CARTESIAN_POINT ( 'NONE',  ( 12.26659068614894466, 14.72041550158064638, -7.082119434687053960 ) ) ;
#52240 = CARTESIAN_POINT ( 'NONE',  ( -1.099225684535947600, -0.4596986634029132657, 6.408140936763237150 ) ) ;
#52242 = CARTESIAN_POINT ( 'NONE',  ( 0.1089645850228810053, 18.16234555792571115, 6.479102184480781013 ) ) ;
#52241 = CARTESIAN_POINT ( 'NONE',  ( 17.96484262340118221, 6.188685344154837509, -7.964842623401177768 ) ) ;
#52243 = CARTESIAN_POINT ( 'NONE',  ( 2.917880565312948704, 17.63708216824730357, 12.26659068614894643 ) ) ;
#52244 = CARTESIAN_POINT ( 'NONE',  ( 24.16423886937410614, 44.51208216824730357, -3.795296366450302550 ) ) ;
#52245 = CARTESIAN_POINT ( 'NONE',  ( 15.44008868035555260, 4.730352010821504471, 9.422509992056143702 ) ) ;
#52246 = ORIENTED_EDGE ( 'NONE', *, *, #79124, .F. ) ;
#52247 = CARTESIAN_POINT ( 'NONE',  ( 17.20831665107776587, 19.13393115100078035, -7.208316651077762316 ) ) ;
#52248 = CARTESIAN_POINT ( 'NONE',  ( -0.8801773607110991993, 17.85535201082150536, -2.915334737309923874 ) ) ;
#52249 = CARTESIAN_POINT ( 'NONE',  ( 19.84674366389459266, 48.71726448433413026, -2.638427012816827677 ) ) ;
#52250 = CARTESIAN_POINT ( 'NONE',  ( 15.94536257719940409, -0.03417435944610275333, 1.273895096820067296 ) ) ;
#52251 = CARTESIAN_POINT ( 'NONE',  ( -11.62719953690071506, 0.5000000000000004441, 9.476720473301710967 ) ) ;
#52252 = AXIS2_PLACEMENT_3D ( 'NONE', #61906, #2430, #46905 ) ;
#52253 = CARTESIAN_POINT ( 'NONE',  ( 16.40814093676323893, 35.79030133659708923, 11.09922568453595026 ) ) ;
#52254 = CARTESIAN_POINT ( 'NONE',  ( 2.791683348922237240, 35.38393115100079456, -7.208316651077763204 ) ) ;
#52255 = VERTEX_POINT ( 'NONE', #39655 ) ;
#52256 = CARTESIAN_POINT ( 'NONE',  ( 18.52753015748617571, 13.09226448433411960, 4.923371831947298993 ) ) ;
#52257 = CARTESIAN_POINT ( 'NONE',  ( 11.43665875882196481, -81.61983315978024223, -3.750000000000000000 ) ) ;
#52258 = CARTESIAN_POINT ( 'NONE',  ( -5.817157072110894944, 14.49999999999999112, 13.82608706751089755 ) ) ;
#52259 = CARTESIAN_POINT ( 'NONE',  ( 17.96484262340118221, 14.93868534415483751, 7.964842623401181321 ) ) ;
#52260 = CARTESIAN_POINT ( 'NONE',  ( -0.3689425029237898834, 46.17874883491397497, -10.36894250292378850 ) ) ;
#52261 = CARTESIAN_POINT ( 'NONE',  ( 17.96484262340118221, 46.18868534415484106, -7.964842623401177768 ) ) ;
#52262 = CARTESIAN_POINT ( 'NONE',  ( 17.96484262340118221, 66.18868534415483396, -7.964842623401177768 ) ) ;
#52263 = PLANE ( 'NONE',  #65618 ) ;
#52264 = CARTESIAN_POINT ( 'NONE',  ( 12.63842701281683922, 19.55059781766745175, -9.846743663894590881 ) ) ;
#52265 = CARTESIAN_POINT ( 'NONE',  ( 12.91533473730992121, 9.522018677488171434, 10.88017736071110164 ) ) ;
#52266 = CARTESIAN_POINT ( 'NONE',  ( 0.1532563361054082862, 11.21726448433411605, 2.638427012816831674 ) ) ;
#52267 = SURFACE_STYLE_USAGE ( .BOTH. , #66270 ) ;
#52268 = CARTESIAN_POINT ( 'NONE',  ( 0.1532563361054100626, 35.80059781766745175, -2.638427012816831230 ) ) ;
#52269 = CARTESIAN_POINT ( 'NONE',  ( 7.084665262690076126, 32.02201867748816966, -10.88017736071110164 ) ) ;
#52270 = EDGE_CURVE ( 'NONE', #54861, #43424, #15064, .T. ) ;
#52271 = ORIENTED_EDGE ( 'NONE', *, *, #74093, .T. ) ;
#52272 = CARTESIAN_POINT ( 'NONE',  ( 10.00000000000000000, 52.87363466993041783, -12.81628187352647608 ) ) ;
#52273 = CARTESIAN_POINT ( 'NONE',  ( 11.25000000000000355, 5.421802177851542837, -2.602085213965210642E-15 ) ) ;
#52274 = CARTESIAN_POINT ( 'NONE',  ( 14.92337183194729988, 14.34226448433411782, -8.527530157486177487 ) ) ;
#52275 = CARTESIAN_POINT ( 'NONE',  ( 22.81628187352647785, 46.41530133659708213, 3.434112377981063169 ) ) ;
#52277 = CARTESIAN_POINT ( 'NONE',  ( 7.361572987183170547, 32.05059781766745175, 9.846743663894590881 ) ) ;
#52276 = CARTESIAN_POINT ( 'NONE',  ( 2.035157376598822676, 2.438685344154838397, -7.964842623401177768 ) ) ;
#52278 = CARTESIAN_POINT ( 'NONE',  ( 20.00000000000000355, 96.99990787933366221, 4.499999999999999112 ) ) ;
#52279 = EDGE_CURVE ( 'NONE', #32515, #50673, #34308, .T. ) ;
#52280 = CARTESIAN_POINT ( 'NONE',  ( 2.791683348922237240, 0.3839311510007847872, -7.208316651077763204 ) ) ;
#52281 = CARTESIAN_POINT ( 'NONE',  ( 6.204703633549690345, 32.84541550158063927, 14.16423886937410082 ) ) ;
#52282 = CARTESIAN_POINT ( 'NONE',  ( 13.79529636645031943, 50.34541550158064638, -14.16423886937409904 ) ) ;
#52283 = CARTESIAN_POINT ( 'NONE',  ( 5.076628168052703671, 51.84226448433412315, 8.527530157486179263 ) ) ;
#52284 = CARTESIAN_POINT ( 'NONE',  ( 20.88017736071110519, 40.56368534415484106, 2.639326808657452039E-16 ) ) ;
#52285 = CARTESIAN_POINT ( 'NONE',  ( 18.52753015748617571, 8.092264484334117824, 4.923371831947298993 ) ) ;
#52286 = CIRCLE ( 'NONE', #45875, 15.00000000000000000 ) ;
#52287 =( LENGTH_UNIT ( ) NAMED_UNIT ( * ) SI_UNIT ( .MILLI., .METRE. ) );
#52288 = ORIENTED_EDGE ( 'NONE', *, *, #26638, .F. ) ;
#52289 = CARTESIAN_POINT ( 'NONE',  ( 22.81628187352648496, 51.83196800326376064, -3.434112377981050290 ) ) ;
#52290 = EDGE_CURVE ( 'NONE', #40499, #38777, #51901, .T. ) ;
#52291 = VECTOR ( 'NONE', #68849, 1000.000000000000000 ) ;
#52292 = CARTESIAN_POINT ( 'NONE',  ( 0.5774900079438607392, 63.48035201082149825, 5.440088680355550821 ) ) ;
#52293 = ORIENTED_EDGE ( 'NONE', *, *, #88420, .T. ) ;
#52294 = CARTESIAN_POINT ( 'NONE',  ( 6.204703633549690345, 2.845415501580634388, 14.16423886937410082 ) ) ;
#52295 = CARTESIAN_POINT ( 'NONE',  ( 12.63842701281683922, 4.550597817667451750, -9.846743663894590881 ) ) ;
#52296 = CARTESIAN_POINT ( 'NONE',  ( 17.96484262340118221, 31.18868534415483751, -7.964842623401177768 ) ) ;
#52297 = CONICAL_SURFACE ( 'NONE', #98652, 1.249999999999987121, 1.029744258676652979 ) ;
#52298 = DIRECTION ( 'NONE',  ( 0.000000000000000000, 0.000000000000000000, 1.000000000000000000 ) ) ;
#52299 = ORIENTED_EDGE ( 'NONE', *, *, #43747, .T. ) ;
#52300 = AXIS2_PLACEMENT_3D ( 'NONE', #76271, #36797, #28786 ) ;
#52301 = CARTESIAN_POINT ( 'NONE',  ( 20.88017736071110519, 30.56368534415484106, 2.639326808657452039E-16 ) ) ;
#52302 = ADVANCED_FACE ( 'NONE', ( #85636 ), #31634, .T. ) ;
#52303 = ORIENTED_EDGE ( 'NONE', *, *, #32753, .F. ) ;
#52304 = CARTESIAN_POINT ( 'NONE',  ( 12.91533473730993009, 31.60535201082150891, -10.88017736071109987 ) ) ;
#52305 = CARTESIAN_POINT ( 'NONE',  ( 0.000000000000000000, 14.49999999999999822, 0.000000000000000000 ) ) ;
#52306 = ORIENTED_EDGE ( 'NONE', *, *, #44311, .F. ) ;
#52307 = ADVANCED_FACE ( 'NONE', ( #17154 ), #92632, .F. ) ;
#52308 = ORIENTED_EDGE ( 'NONE', *, *, #53329, .F. ) ;
#52309 = CARTESIAN_POINT ( 'NONE',  ( 7.084665262690076126, 64.10535201082150536, 10.88017736071109987 ) ) ;
#52310 = DIRECTION ( 'NONE',  ( 0.000000000000000000, 1.000000000000000000, 0.000000000000000000 ) ) ;
#52312 = DIRECTION ( 'NONE',  ( 1.000000000000000000, 0.000000000000000000, 0.000000000000000000 ) ) ;
#52311 = CARTESIAN_POINT ( 'NONE',  ( 20.88017736071110875, 15.77201867748817143, -2.915334737309920765 ) ) ;
#52313 = CARTESIAN_POINT ( 'NONE',  ( 18.52753015748618282, 8.925597817667451750, -4.923371831947291888 ) ) ;
#52314 = CARTESIAN_POINT ( 'NONE',  ( -0.8801773607111008646, 18.27201867748817321, 2.915334737309923430 ) ) ;
#52315 = B_SPLINE_CURVE_WITH_KNOTS ( 'NONE', 3,
 ( #47733, #69271, #77736, #17258, #46269, #71237 ),
 .UNSPECIFIED., .F., .F.,
 ( 4, 2, 4 ),
 ( 3.409110551326284999E-05, 0.0004400426677351060040, 0.0008459942299569491852 ),
 .UNSPECIFIED. ) ;
#52316 = ORIENTED_EDGE ( 'NONE', *, *, #90582, .F. ) ;
#52317 = CARTESIAN_POINT ( 'NONE',  ( -1.099225684535947600, 48.70696800326375353, -6.408140936763238038 ) ) ;
#52318 = CARTESIAN_POINT ( 'NONE',  ( 20.88017736071110164, 45.35535201082149115, 2.915334737309930979 ) ) ;
#52319 = CARTESIAN_POINT ( 'NONE',  ( -46.88190520701112973, 103.4393505901440875, -6.246661988884179451 ) ) ;
#52320 = CARTESIAN_POINT ( 'NONE',  ( 13.43411237798105340, 50.58196800326375353, 12.81628187352647963 ) ) ;
#52321 = CARTESIAN_POINT ( 'NONE',  ( -0.8801773607111008646, 48.27201867748816966, 2.915334737309923430 ) ) ;
#52322 = CARTESIAN_POINT ( 'NONE',  ( 19.38216949554541202, 5.998634669930420493, 9.382169495545424454 ) ) ;
#52323 = LINE ( 'NONE', #76792, #442 ) ;
#52324 = CARTESIAN_POINT ( 'NONE',  ( 7.361572987183170547, 17.05059781766745530, 9.846743663894590881 ) ) ;
#52325 = CARTESIAN_POINT ( 'NONE',  ( 4.441305562537879226, -2.692695313950745017, -3.749999999999999556 ) ) ;
#52326 = CARTESIAN_POINT ( 'NONE',  ( 10.00000000000000000, 7.873634669930421381, -12.81628187352647608 ) ) ;
#52328 = CARTESIAN_POINT ( 'NONE',  ( -41.94000000000001194, 93.50000000000000000, 9.500000000000000000 ) ) ;
#52327 = FACE_OUTER_BOUND ( 'NONE', #94827, .T. ) ;
#52329 = CARTESIAN_POINT ( 'NONE',  ( 20.88017736071110519, 40.56368534415484106, 2.639326808657452039E-16 ) ) ;
#52330 = CARTESIAN_POINT ( 'NONE',  ( 19.84674366389459621, 43.50893115100078745, 7.409399052514197653E-17 ) ) ;
#52331 = FILL_AREA_STYLE_COLOUR ( '', #20013 ) ;
#52332 = CARTESIAN_POINT ( 'NONE',  ( 18.52753015748618282, 18.92559781766745175, -4.923371831947291888 ) ) ;
#52333 = CARTESIAN_POINT ( 'NONE',  ( 7.361572987183169658, 4.967264484334119601, -9.846743663894592657 ) ) ;
#52334 = EDGE_CURVE ( 'NONE', #95619, #14052, #86132, .T. ) ;
#52336 = ORIENTED_EDGE ( 'NONE', *, *, #98148, .T. ) ;
#52335 = CARTESIAN_POINT ( 'NONE',  ( 0.6178305044545838731, 9.748634669930416052, 9.382169495545420901 ) ) ;
#52337 = SURFACE_STYLE_FILL_AREA ( #46321 ) ;
#52338 = CARTESIAN_POINT ( 'NONE',  ( 2.791683348922237240, 60.38393115100078745, -7.208316651077763204 ) ) ;
#52339 = CARTESIAN_POINT ( 'NONE',  ( 10.00000000000000178, 32.25893115100078745, 9.846743663894594434 ) ) ;
#52340 = CARTESIAN_POINT ( 'NONE',  ( 6.829574850505125028, -88.00372650098202598, -2.750000000000000888 ) ) ;
#52341 = CARTESIAN_POINT ( 'NONE',  ( 0.5774900079438590739, 2.647018677488171434, -5.440088680355550821 ) ) ;
#52342 = CARTESIAN_POINT ( 'NONE',  ( 17.20831665107776587, 49.13393115100078745, -7.208316651077762316 ) ) ;
#52343 = FACE_OUTER_BOUND ( 'NONE', #54599, .T. ) ;
#52344 = CARTESIAN_POINT ( 'NONE',  ( 17.08211943468705840, 65.13708216824730357, -12.26659068614894466 ) ) ;
#52345 = PLANE ( 'NONE',  #39198 ) ;
#52346 = CARTESIAN_POINT ( 'NONE',  ( 20.88017736071110875, 25.77201867748816966, -2.915334737309920765 ) ) ;
#52347 = CARTESIAN_POINT ( 'NONE',  ( 20.36894250292379382, 43.67874883491397497, 10.36894250292379205 ) ) ;
#52349 = CARTESIAN_POINT ( 'NONE',  ( -3.750000000000000000, 10.25000000000000000, 2.750000000000000000 ) ) ;
#52348 = CARTESIAN_POINT ( 'NONE',  ( -0.3689425029237881626, 57.42874883491397497, 10.36894250292379027 ) ) ;
#52350 = CARTESIAN_POINT ( 'NONE',  ( 5.076628168052703671, 1.842264484334118047, 8.527530157486179263 ) ) ;
#52351 = CARTESIAN_POINT ( 'NONE',  ( 1.472469842513823179, 30.59226448433411960, -4.923371831947296329 ) ) ;
#52352 = CARTESIAN_POINT ( 'NONE',  ( 19.38216949554541557, 7.248634669930421381, -9.382169495545420901 ) ) ;
#52353 = TOROIDAL_SURFACE ( 'NONE', #9255, 14.49999999999999822, 0.5000000000000000000 ) ;
#52354 = LINE ( 'NONE', #37371, #16155 ) ;
#52356 = LINE ( 'NONE', #13370, #95392 ) ;
#52355 = VECTOR ( 'NONE', #50609, 1000.000000000000000 ) ;
#52357 = PRESENTATION_LAYER_ASSIGNMENT (  '', '', ( #85918 ) ) ;
#52358 = CARTESIAN_POINT ( 'NONE',  ( -6.732636091893173358, -88.11213685669363826, 2.750000000000000000 ) ) ;
#52359 = CARTESIAN_POINT ( 'NONE',  ( -0.3689425029237881626, 7.428748834913967869, 10.36894250292379027 ) ) ;
#52360 = CARTESIAN_POINT ( 'NONE',  ( 18.52753015748617571, 23.09226448433411960, 4.923371831947298993 ) ) ;
#52361 = CARTESIAN_POINT ( 'NONE',  ( 24.16423886937410614, 39.30374883491396787, 8.672049930838204340E-16 ) ) ;
#52362 = CARTESIAN_POINT ( 'NONE',  ( 5.076628168052703671, 11.84226448433411960, 8.527530157486179263 ) ) ;
#52364 = CARTESIAN_POINT ( 'NONE',  ( -5.625000000000007994, 7.088468844518210688, -9.742785792574931492 ) ) ;
#52363 = CARTESIAN_POINT ( 'NONE',  ( -6.787853370348170934, -86.25412202734862888, -2.500000000000000888 ) ) ;
#52365 = CARTESIAN_POINT ( 'NONE',  ( 20.88017736071110164, 30.35535201082151247, 2.915334737309930979 ) ) ;
#52366 = CARTESIAN_POINT ( 'NONE',  ( 13.43411237798105340, 40.58196800326375353, 12.81628187352647963 ) ) ;
#52367 = CARTESIAN_POINT ( 'NONE',  ( 12.91533473730992121, 4.522018677488169658, 10.88017736071110164 ) ) ;
#52368 = CARTESIAN_POINT ( 'NONE',  ( -1.099225684535947600, 39.54030133659708923, 6.408140936763237150 ) ) ;
#52369 = CARTESIAN_POINT ( 'NONE',  ( -1.099225684535947600, 58.70696800326375353, -6.408140936763238038 ) ) ;
#52370 = ORIENTED_EDGE ( 'NONE', *, *, #74957, .T. ) ;
#52371 = DIRECTION ( 'NONE',  ( 0.000000000000000000, -1.000000000000000000, 0.000000000000000000 ) ) ;
#52372 = CARTESIAN_POINT ( 'NONE',  ( 20.36894250292379382, 43.67874883491397497, 10.36894250292379205 ) ) ;
#52373 = SURFACE_SIDE_STYLE ('',( #57893 ) ) ;
#52374 = CARTESIAN_POINT ( 'NONE',  ( 2.035157376598824452, 3.688685344154837953, 7.964842623401179544 ) ) ;
#52375 = CARTESIAN_POINT ( 'NONE',  ( 2.035157376598822676, 17.43868534415483751, -7.964842623401177768 ) ) ;
#52376 = LINE ( 'NONE', #82880, #68721 ) ;
#52377 = DIRECTION ( 'NONE',  ( 0.000000000000000000, 1.000000000000000000, 0.000000000000000000 ) ) ;
#52378 = CARTESIAN_POINT ( 'NONE',  ( 7.084665262690076126, 54.10535201082151247, 10.88017736071109987 ) ) ;
#52379 = CARTESIAN_POINT ( 'NONE',  ( 7.084665262690076126, 64.10535201082150536, 10.88017736071109987 ) ) ;
#52380 = CARTESIAN_POINT ( 'NONE',  ( 22.81628187352647785, 21.41530133659708923, 3.434112377981063169 ) ) ;
#52381 = DIRECTION ( 'NONE',  ( -0.5547001962252290364, -0.8320502943378437211, 0.000000000000000000 ) ) ;
#52382 = DIRECTION ( 'NONE',  ( 0.000000000000000000, 0.000000000000000000, -1.000000000000000000 ) ) ;
#52383 = CARTESIAN_POINT ( 'NONE',  ( 12.63842701281683922, 19.55059781766745175, -9.846743663894590881 ) ) ;
#52384 = ADVANCED_FACE ( 'NONE', ( #9640 ), #63605, .F. ) ;
#52385 = CARTESIAN_POINT ( 'NONE',  ( 17.96484262340118221, 54.93868534415484106, 7.964842623401181321 ) ) ;
#52386 = B_SPLINE_CURVE_WITH_KNOTS ( 'NONE', 3,
 ( #73873, #59359, #65874, #73375, #80400, #42894 ),
 .UNSPECIFIED., .F., .F.,
 ( 4, 2, 4 ),
 ( 0.0002800225282680458404, 0.0006862279780657128125, 0.001092433427863379785 ),
 .UNSPECIFIED. ) ;
#52387 = EDGE_CURVE ( 'NONE', #97699, #59012, #10362, .T. ) ;
#52388 = EDGE_CURVE ( 'NONE', #18642, #82286, #11927, .T. ) ;
#52389 = CARTESIAN_POINT ( 'NONE',  ( 13.43411237798106583, 17.66530133659708923, -12.81628187352647252 ) ) ;
#52391 = ADVANCED_FACE ( 'NONE', ( #48114 ), #1173, .T. ) ;
#52390 = CARTESIAN_POINT ( 'NONE',  ( 19.42250999205614548, 10.98035201082150358, -5.440088680355545492 ) ) ;
#52392 = EDGE_CURVE ( 'NONE', #14084, #76878, #18356, .T. ) ;
#52393 = CARTESIAN_POINT ( 'NONE',  ( 1.472469842513823179, 41.42559781766745886, 4.923371831947296329 ) ) ;
#52394 = CARTESIAN_POINT ( 'NONE',  ( -2.816281873526473856, 64.12363466993042493, 9.499525473075851096E-16 ) ) ;
#52395 = CARTESIAN_POINT ( 'NONE',  ( 19.84674366389459266, 18.71726448433411960, -2.638427012816827677 ) ) ;
#52396 =( NAMED_UNIT ( * ) SI_UNIT ( $, .STERADIAN. ) SOLID_ANGLE_UNIT ( ) );
#52397 = CARTESIAN_POINT ( 'NONE',  ( 19.42250999205614548, 30.98035201082150536, -5.440088680355545492 ) ) ;
#52398 = CARTESIAN_POINT ( 'NONE',  ( -0.8801773607110991993, 27.85535201082150181, -2.915334737309923874 ) ) ;
#52399 = CARTESIAN_POINT ( 'NONE',  ( -0.8801773607111008646, 3.272018677488171434, 2.915334737309923430 ) ) ;
#52400 = CARTESIAN_POINT ( 'NONE',  ( 14.92337183194729633, 37.67559781766745175, 8.527530157486181039 ) ) ;
#52401 = CARTESIAN_POINT ( 'NONE',  ( 20.88017736071110875, 35.77201867748816966, -2.915334737309920765 ) ) ;
#52402 = CARTESIAN_POINT ( 'NONE',  ( 17.96484262340118221, 14.93868534415484106, 7.964842623401181321 ) ) ;
#52403 = ORIENTED_EDGE ( 'NONE', *, *, #52708, .F. ) ;
#52404 = CARTESIAN_POINT ( 'NONE',  ( 20.88017736071110519, 30.56368534415484106, 2.639326808657452039E-16 ) ) ;
#52405 = EDGE_CURVE ( 'NONE', #32248, #13300, #35901, .T. ) ;
#52406 = CARTESIAN_POINT ( 'NONE',  ( 6.565887622018943937, 45.16530133659708923, 12.81628187352647430 ) ) ;
#52407 = CARTESIAN_POINT ( 'NONE',  ( -0.8801773607110991993, 47.85535201082150536, -2.915334737309923874 ) ) ;
#52409 = CARTESIAN_POINT ( 'NONE',  ( 19.42250999205614193, 35.14701867748816966, 5.440088680355555262 ) ) ;
#52408 = CARTESIAN_POINT ( 'NONE',  ( 0.000000000000000000, 0.5000000000000004441, 0.000000000000000000 ) ) ;
#52410 = AXIS2_PLACEMENT_3D ( 'NONE', #41494, #71963, #78973 ) ;
#52411 = ORIENTED_EDGE ( 'NONE', *, *, #87122, .T. ) ;
#52412 = CARTESIAN_POINT ( 'NONE',  ( 1.472469842513823179, 55.59226448433412315, -4.923371831947296329 ) ) ;
#52413 = CARTESIAN_POINT ( 'NONE',  ( 10.00000000000000178, 34.31368534415484106, 10.88017736071110342 ) ) ;
#52414 = SURFACE_STYLE_FILL_AREA ( #8878 ) ;
#52415 = DIRECTION ( 'NONE',  ( -1.000000000000000000, 0.000000000000000000, 0.000000000000000000 ) ) ;
#52416 = CARTESIAN_POINT ( 'NONE',  ( -8.399999999999998579, 98.49999999999998579, 8.000000000000000000 ) ) ;
#52417 = CARTESIAN_POINT ( 'NONE',  ( 10.00000000000000000, 45.55374883491397497, -14.16423886937410082 ) ) ;
#52418 = CARTESIAN_POINT ( 'NONE',  ( 7.084665262690076126, 59.10535201082150536, 10.88017736071109987 ) ) ;
#52419 = PRESENTATION_STYLE_ASSIGNMENT (( #21939 ) ) ;
#52420 = CARTESIAN_POINT ( 'NONE',  ( -1.499999999999998668, 23.03999999999999915, 0.000000000000000000 ) ) ;
#52421 = CARTESIAN_POINT ( 'NONE',  ( 10.00000000000000000, -2.126365330069579951, -12.81628187352647608 ) ) ;
#52422 = CARTESIAN_POINT ( 'NONE',  ( 10.00000000000000000, 34.75893115100078745, -9.846743663894594434 ) ) ;
#52423 = ORIENTED_EDGE ( 'NONE', *, *, #35000, .T. ) ;
#52424 = ADVANCED_FACE ( 'NONE', ( #49581 ), #74209, .T. ) ;
#52425 = CARTESIAN_POINT ( 'NONE',  ( 0.1532563361054083140, 31.00893115100078390, 1.131784320476157264E-15 ) ) ;
#52426 = CARTESIAN_POINT ( 'NONE',  ( -12.81628187352647963, -16.08469866340291077, -3.434112377981046293 ) ) ;
#52427 = AXIS2_PLACEMENT_3D ( 'NONE', #12077, #33584, #10613 ) ;
#52428 = CARTESIAN_POINT ( 'NONE',  ( -0.8801773607111009756, 28.06368534415484106, 1.068504757029289695E-15 ) ) ;
#52429 = CARTESIAN_POINT ( 'NONE',  ( 10.00000000000000178, 27.25893115100078390, 9.846743663894594434 ) ) ;
#52430 = CARTESIAN_POINT ( 'NONE',  ( -2.816281873526473856, 24.12363466993042138, 9.499525473075851096E-16 ) ) ;
#52432 = CARTESIAN_POINT ( 'NONE',  ( 4.559911319644449179, 63.89701867748817676, 9.422509992056141925 ) ) ;
#52431 = CARTESIAN_POINT ( 'NONE',  ( 0.5774900079438607392, 68.48035201082150536, 5.440088680355550821 ) ) ;
#52434 = CARTESIAN_POINT ( 'NONE',  ( 7.084665262690076126, 7.022018677488169658, -10.88017736071110164 ) ) ;
#52433 = CARTESIAN_POINT ( 'NONE',  ( 12.91533473730992121, 29.52201867748817321, 10.88017736071110164 ) ) ;
#52435 = CARTESIAN_POINT ( 'NONE',  ( 17.08211943468705130, 48.47041550158063927, 12.26659068614894998 ) ) ;
#52436 = CIRCLE ( 'NONE', #77983, 0.5000000000000004441 ) ;
#52437 = ADVANCED_FACE ( 'NONE', ( #19590 ), #80592, .T. ) ;
#52438 = DIRECTION ( 'NONE',  ( 6.938893903907222067E-15, -1.000000000000000000, 0.000000000000000000 ) ) ;
#52439 = VERTEX_POINT ( 'NONE', #73565 ) ;
#52440 = CARTESIAN_POINT ( 'NONE',  ( 13.43411237798106583, 12.66530133659708746, -12.81628187352647252 ) ) ;
#52441 = CARTESIAN_POINT ( 'NONE',  ( 20.88017736071110875, 10.77201867748817143, -2.915334737309920765 ) ) ;
#52442 = CARTESIAN_POINT ( 'NONE',  ( -0.8801773607110991993, 47.85535201082150536, -2.915334737309923874 ) ) ;
#52443 =( LENGTH_UNIT ( ) NAMED_UNIT ( * ) SI_UNIT ( .MILLI., .METRE. ) );
#52444 = ORIENTED_EDGE ( 'NONE', *, *, #58022, .F. ) ;
#52445 = CARTESIAN_POINT ( 'NONE',  ( 20.88017736071110164, 55.35535201082149825, 2.915334737309930979 ) ) ;
#52446 = CARTESIAN_POINT ( 'NONE',  ( 2.791683348922237240, 35.38393115100079456, -7.208316651077763204 ) ) ;
#52447 = CARTESIAN_POINT ( 'NONE',  ( 12.63842701281683034, 22.46726448433411605, 9.846743663894596210 ) ) ;
#52448 = CARTESIAN_POINT ( 'NONE',  ( 0.1532563361054100626, 15.80059781766745353, -2.638427012816831230 ) ) ;
#52449 = CARTESIAN_POINT ( 'NONE',  ( 0.7375392941517004974, 14.49999999999999112, 14.98185688723477682 ) ) ;
#52451 = DIRECTION ( 'NONE',  ( 0.000000000000000000, -0.000000000000000000, 1.000000000000000000 ) ) ;
#52450 = CARTESIAN_POINT ( 'NONE',  ( 0.1532563361054083140, 6.008931151000784787, 1.131784320476157264E-15 ) ) ;
#52452 = CARTESIAN_POINT ( 'NONE',  ( 20.15039907845753220, 44.72266099184918176, 6.262539305110078836 ) ) ;
#52454 = ORIENTED_EDGE ( 'NONE', *, *, #32851, .T. ) ;
#52453 = CARTESIAN_POINT ( 'NONE',  ( 10.00000000000000178, 27.25893115100078390, 9.846743663894594434 ) ) ;
#52455 = CARTESIAN_POINT ( 'NONE',  ( -13.34343830728394309, 15.00000000000000000, -6.852200678592783589 ) ) ;
#52456 = CARTESIAN_POINT ( 'NONE',  ( 19.38216949554541202, 10.99863466993042138, 9.382169495545424454 ) ) ;
#52457 = CARTESIAN_POINT ( 'NONE',  ( 20.88017736071110875, 55.77201867748816966, -2.915334737309920765 ) ) ;
#52458 = CARTESIAN_POINT ( 'NONE',  ( -4.164238869374099927, 32.01208216824730357, 3.795296366450308767 ) ) ;
#52459 = UNCERTAINTY_MEASURE_WITH_UNIT (LENGTH_MEASURE( 1.000000000000000082E-05 ), #25346, 'distance_accuracy_value', 'NONE');
#52460 = CARTESIAN_POINT ( 'NONE',  ( -8.350463100005470096, 86.22728700194058149, 4.047063141920189899 ) ) ;
#52461 = CARTESIAN_POINT ( 'NONE',  ( 20.36894250292379738, 24.92874883491396787, -10.36894250292379027 ) ) ;
#52462 = CARTESIAN_POINT ( 'NONE',  ( 6.204703633549690345, 47.84541550158064638, 14.16423886937410082 ) ) ;
#52463 = EDGE_CURVE ( 'NONE', #46092, #72566, #79607, .T. ) ;
#52464 = CARTESIAN_POINT ( 'NONE',  ( -4.164238869374099039, 6.803748834913967869, 8.674139862899312516E-16 ) ) ;
#52465 = CARTESIAN_POINT ( 'NONE',  ( 13.79529636645030344, 13.26208216824729824, 14.16423886937410614 ) ) ;
#52466 = CARTESIAN_POINT ( 'NONE',  ( 15.44008868035555793, 41.39701867748817676, -9.422509992056140149 ) ) ;
#52467 = DIRECTION ( 'NONE',  ( 0.000000000000000000, 0.000000000000000000, 1.000000000000000000 ) ) ;
#52468 = CARTESIAN_POINT ( 'NONE',  ( 5.076628168052704559, 25.17559781766745175, -8.527530157486179263 ) ) ;
#52470 = CARTESIAN_POINT ( 'NONE',  ( 17.20831665107776587, 34.13393115100078745, -7.208316651077762316 ) ) ;
#52469 = CARTESIAN_POINT ( 'NONE',  ( 13.99999999999999822, 11.50000000000000000, -5.000000000000000000 ) ) ;
#52471 = CARTESIAN_POINT ( 'NONE',  ( 21.09922568453595559, 57.04030133659708923, -6.408140936763230044 ) ) ;
#52472 = CARTESIAN_POINT ( 'NONE',  ( 10.00000000000000000, 64.75893115100078035, -9.846743663894594434 ) ) ;
#52473 = EDGE_CURVE ( 'NONE', #26894, #30756, #41134, .T. ) ;
#52474 = CARTESIAN_POINT ( 'NONE',  ( 7.361572987183169658, 24.96726448433412315, -9.846743663894592657 ) ) ;
#52475 = CARTESIAN_POINT ( 'NONE',  ( 3.591859063236763294, 43.29030133659708923, -11.09922568453595026 ) ) ;
#52476 = CARTESIAN_POINT ( 'NONE',  ( -10.36894250292379205, -23.82125116508602858, -10.36894250292378672 ) ) ;
#52477 = CARTESIAN_POINT ( 'NONE',  ( 7.084665262690076126, 37.02201867748817676, -10.88017736071110164 ) ) ;
#52478 = CARTESIAN_POINT ( 'NONE',  ( 12.63842701281683922, 49.55059781766744464, -9.846743663894590881 ) ) ;
#52479 = CARTESIAN_POINT ( 'NONE',  ( 20.36894250292379738, 24.92874883491396787, -10.36894250292379027 ) ) ;
#52480 = EDGE_LOOP ( 'NONE', ( #95602, #81314, #64499, #61627 ) ) ;
#52481 = CARTESIAN_POINT ( 'NONE',  ( 2.035157376598822676, 67.43868534415484817, -7.964842623401177768 ) ) ;
#52482 = CARTESIAN_POINT ( 'NONE',  ( -0.8801773607111008646, 68.27201867748817676, 2.915334737309923430 ) ) ;
#52483 = CARTESIAN_POINT ( 'NONE',  ( -4.164238869374099927, 62.01208216824728936, 3.795296366450308767 ) ) ;
#52484 = CARTESIAN_POINT ( 'NONE',  ( -2.816281873526471635, 3.915301336597087456, -3.434112377981056508 ) ) ;
#52485 = CARTESIAN_POINT ( 'NONE',  ( 19.72487221294571569, 42.80223176428830811, -6.499999999999990230 ) ) ;
#52486 = CARTESIAN_POINT ( 'NONE',  ( 15.44008868035555260, 59.73035201082151247, 9.422509992056143702 ) ) ;
#52487 = LINE ( 'NONE', #60482, #35860 ) ;
#52488 = AXIS2_PLACEMENT_3D ( 'NONE', #64929, #87938, #81426 ) ;
#52489 = CARTESIAN_POINT ( 'NONE',  ( 6.565887622018943937, 33.08196800326374643, -12.81628187352647608 ) ) ;
#52490 = CARTESIAN_POINT ( 'NONE',  ( 17.08211943468705840, 45.13708216824730357, -12.26659068614894466 ) ) ;
#52491 = CARTESIAN_POINT ( 'NONE',  ( -10.88017736071109987, 23.27201867748817676, 2.915334737309934532 ) ) ;
#52492 = CARTESIAN_POINT ( 'NONE',  ( 10.00000000000000178, 9.313685344154839285, 10.88017736071110342 ) ) ;
#52493 = CARTESIAN_POINT ( 'NONE',  ( 12.91533473730993009, 16.60535201082150891, -10.88017736071109987 ) ) ;
#52494 = CARTESIAN_POINT ( 'NONE',  ( 1.472469842513823179, 60.59226448433412315, -4.923371831947296329 ) ) ;
#52495 = CARTESIAN_POINT ( 'NONE',  ( -2.816281873526471635, 53.91530133659709634, -3.434112377981056508 ) ) ;
#52496 = ORIENTED_EDGE ( 'NONE', *, *, #97772, .F. ) ;
#52497 = CARTESIAN_POINT ( 'NONE',  ( 2.035157376598824452, 23.68868534415484461, 7.964842623401179544 ) ) ;
#52498 = CARTESIAN_POINT ( 'NONE',  ( -2.816281873526473856, 19.12363466993042138, 9.499525473075851096E-16 ) ) ;
#52499 = CARTESIAN_POINT ( 'NONE',  ( 13.21236992757670059, 15.00000000000000000, 5.338143956176803151 ) ) ;
#52500 = AXIS2_PLACEMENT_3D ( 'NONE', #45403, #46399, #92871 ) ;
#52501 = EDGE_CURVE ( 'NONE', #86688, #69641, #57094, .T. ) ;
#52502 = CARTESIAN_POINT ( 'NONE',  ( 7.361572987183170547, 42.05059781766745886, 9.846743663894590881 ) ) ;
#52503 = CARTESIAN_POINT ( 'NONE',  ( -0.8801773607110991993, 37.85535201082151247, -2.915334737309923874 ) ) ;
#52504 = EDGE_CURVE ( 'NONE', #56450, #23152, #18615, .T. ) ;
#52505 = CARTESIAN_POINT ( 'NONE',  ( 0.6178305044545818747, 18.49863466993041428, -9.382169495545419124 ) ) ;
#52507 = CARTESIAN_POINT ( 'NONE',  ( -8.900000000000002132, 75.76920769491746910, -3.000000000000000000 ) ) ;
#52506 = CARTESIAN_POINT ( 'NONE',  ( 20.88017736071110875, 45.77201867748816966, -2.915334737309920765 ) ) ;
#52508 = CARTESIAN_POINT ( 'NONE',  ( 0.000000000000000000, 14.49999999999999822, 0.000000000000000000 ) ) ;
#52509 = CARTESIAN_POINT ( 'NONE',  ( 3.591859063236763294, 53.29030133659708923, -11.09922568453595026 ) ) ;
#52510 = ORIENTED_EDGE ( 'NONE', *, *, #85065, .T. ) ;
#52511 = CARTESIAN_POINT ( 'NONE',  ( -0.1503990784575328643, 30.12777174578613781, 6.262539305110068177 ) ) ;
#52512 = CARTESIAN_POINT ( 'NONE',  ( 0.5774900079438607392, 53.48035201082151247, 5.440088680355550821 ) ) ;
#52514 = CARTESIAN_POINT ( 'NONE',  ( 2.917880565312950480, 5.970415501580634832, -12.26659068614894821 ) ) ;
#52513 = CARTESIAN_POINT ( 'NONE',  ( 16.40814093676324603, 27.45696800326375708, -11.09922568453594671 ) ) ;
#52515 = CARTESIAN_POINT ( 'NONE',  ( 0.1532563361054100626, 5.800597817667452638, -2.638427012816831230 ) ) ;
#52516 = CARTESIAN_POINT ( 'NONE',  ( 4.559911319644449179, 37.23035201082150536, -9.422509992056141925 ) ) ;
#52517 = CARTESIAN_POINT ( 'NONE',  ( 18.95386800104996183, 3.238109087357262883, -6.500000000000001776 ) ) ;
#52518 = CARTESIAN_POINT ( 'NONE',  ( 19.84674366389459266, 63.30059781766745886, 2.638427012816836559 ) ) ;
#52519 = CARTESIAN_POINT ( 'NONE',  ( 19.84674366389459266, 18.30059781766745175, 2.638427012816836559 ) ) ;
#52520 = CARTESIAN_POINT ( 'NONE',  ( 12.63842701281683034, 12.46726448433411782, 9.846743663894596210 ) ) ;
#52521 = CARTESIAN_POINT ( 'NONE',  ( 64.56412365047461321, 29.50000000000000000, 9.500000000000000000 ) ) ;
#52522 = CARTESIAN_POINT ( 'NONE',  ( 17.08211943468705130, 43.47041550158063927, 12.26659068614894998 ) ) ;
#52523 = DIRECTION ( 'NONE',  ( 0.000000000000000000, 0.000000000000000000, 1.000000000000000000 ) ) ;
#52524 = CARTESIAN_POINT ( 'NONE',  ( 11.01442511525662482, -96.10567886042495900, -3.749999999999999112 ) ) ;
#52525 = CARTESIAN_POINT ( 'NONE',  ( -7.121448108955550360, -73.25984652122872376, -4.000000000000001776 ) ) ;
#52526 = VERTEX_POINT ( 'NONE', #42115 ) ;
#52527 = CARTESIAN_POINT ( 'NONE',  ( -4.164238869374098151, 61.59541550158063217, -3.795296366450310543 ) ) ;
#52528 = CARTESIAN_POINT ( 'NONE',  ( 2.035157376598822676, 2.438685344154838397, -7.964842623401177768 ) ) ;
#52529 = CARTESIAN_POINT ( 'NONE',  ( 1.472469842513823179, 30.59226448433411960, -4.923371831947296329 ) ) ;
#52530 = CARTESIAN_POINT ( 'NONE',  ( 0.6178305044545818747, 43.49863466993042493, -9.382169495545419124 ) ) ;
#52531 = DIRECTION ( 'NONE',  ( 1.000000000000000000, 0.000000000000000000, 0.000000000000000000 ) ) ;
#52533 = CARTESIAN_POINT ( 'NONE',  ( 24.16423886937410614, 4.512082168247300906, -3.795296366450302550 ) ) ;
#52532 = CARTESIAN_POINT ( 'NONE',  ( -11.88860330017057443, 90.28199325634325589, -6.828299344296716811 ) ) ;
#52534 = CARTESIAN_POINT ( 'NONE',  ( -0.8801773607111008646, 13.27201867748817143, 2.915334737309923430 ) ) ;
#52535 = CARTESIAN_POINT ( 'NONE',  ( 20.36894250292379738, 59.92874883491397497, -10.36894250292379027 ) ) ;
#52536 = CARTESIAN_POINT ( 'NONE',  ( 14.92337183194729988, 39.34226448433412315, -8.527530157486177487 ) ) ;
#52537 = CARTESIAN_POINT ( 'NONE',  ( 19.72487221294571569, 40.71833443783938122, -6.499999999999989342 ) ) ;
#52538 = CARTESIAN_POINT ( 'NONE',  ( 18.52753015748618282, 18.92559781766745175, -4.923371831947291888 ) ) ;
#52539 = EDGE_CURVE ( 'NONE', #53414, #10378, #41629, .T. ) ;
#52540 = DIRECTION ( 'NONE',  ( -0.000000000000000000, -1.000000000000000000, -0.000000000000000000 ) ) ;
#52541 = CARTESIAN_POINT ( 'NONE',  ( 8.527530157486179263, 13.09226448433412848, 4.923371831947292776 ) ) ;
#52542 = ORIENTED_EDGE ( 'NONE', *, *, #69083, .F. ) ;
#52543 = ORIENTED_EDGE ( 'NONE', *, *, #3396, .T. ) ;
#52544 = APPLICATION_CONTEXT ( 'automotive_design' ) ;
#52545 = CARTESIAN_POINT ( 'NONE',  ( 8.879999999999995453, 41.24999999999999289, 4.000000000000000000 ) ) ;
#52546 = ORIENTED_EDGE ( 'NONE', *, *, #21255, .T. ) ;
#52547 = CARTESIAN_POINT ( 'NONE',  ( 19.84674366389459266, 43.71726448433410894, -2.638427012816827677 ) ) ;
#52549 = CARTESIAN_POINT ( 'NONE',  ( 2.035157376598824452, 38.68868534415483396, 7.964842623401179544 ) ) ;
#52548 = CARTESIAN_POINT ( 'NONE',  ( 7.084665262690076126, 27.02201867748817676, -10.88017736071110164 ) ) ;
#52551 = CARTESIAN_POINT ( 'NONE',  ( 22.81628187352648496, 26.83196800326374998, -3.434112377981050290 ) ) ;
#52550 = CARTESIAN_POINT ( 'NONE',  ( 5.076628168052704559, 60.17559781766745175, -8.527530157486179263 ) ) ;
#52552 = CARTESIAN_POINT ( 'NONE',  ( 24.16423886937409904, 9.095415501580633943, 3.795296366450317205 ) ) ;
#52553 = CARTESIAN_POINT ( 'NONE',  ( 7.084665262690076126, 64.10535201082150536, 10.88017736071109987 ) ) ;
#52554 = CARTESIAN_POINT ( 'NONE',  ( 6.565887622018943937, 30.16530133659708568, 12.81628187352647430 ) ) ;
#52555 = ORIENTED_EDGE ( 'NONE', *, *, #94873, .T. ) ;
#52556 = CARTESIAN_POINT ( 'NONE',  ( 2.791683348922240793, 46.63393115100077324, 7.208316651077764092 ) ) ;
#52557 = CARTESIAN_POINT ( 'NONE',  ( 10.00000000000000178, 9.313685344154839285, 10.88017736071110342 ) ) ;
#52558 = ORIENTED_EDGE ( 'NONE', *, *, #64785, .F. ) ;
#52559 = CARTESIAN_POINT ( 'NONE',  ( 7.084665262690076126, 17.02201867748817676, -10.88017736071110164 ) ) ;
#52560 = EDGE_LOOP ( 'NONE', ( #69399, #72102, #11297, #70410, #38289 ) ) ;
#52561 = CARTESIAN_POINT ( 'NONE',  ( 20.88017736071110164, 45.35535201082149115, 2.915334737309930979 ) ) ;
#52562 = CARTESIAN_POINT ( 'NONE',  ( 15.44008868035555260, 54.73035201082150536, 9.422509992056143702 ) ) ;
#52563 = CIRCLE ( 'NONE', #97265, 1.750000000000001554 ) ;
#52564 = CARTESIAN_POINT ( 'NONE',  ( 12.91533473730992121, 59.52201867748816966, 10.88017736071110164 ) ) ;
#52565 = SURFACE_STYLE_USAGE ( .BOTH. , #90068 ) ;
#52566 = CARTESIAN_POINT ( 'NONE',  ( -0.8801773607110991993, 52.85535201082151247, -2.915334737309923874 ) ) ;
#52567 = CARTESIAN_POINT ( 'NONE',  ( -46.94000000000000483, 100.8832200551196934, 8.297377427102095027 ) ) ;
#52568 = VECTOR ( 'NONE', #60040, 1000.000000000000000 ) ;
#52569 = CARTESIAN_POINT ( 'NONE',  ( 1.959929470562274068, 11.50257860105348762, 5.767676674365839418 ) ) ;
#52571 = ORIENTED_EDGE ( 'NONE', *, *, #48882, .F. ) ;
#52570 =( NAMED_UNIT ( * ) PLANE_ANGLE_UNIT ( ) SI_UNIT ( $, .RADIAN. ) );
#52572 = CARTESIAN_POINT ( 'NONE',  ( 19.84674366389459621, 28.50893115100078745, 7.409399052514197653E-17 ) ) ;
#52573 = VERTEX_POINT ( 'NONE', #27576 ) ;
#52574 = CARTESIAN_POINT ( 'NONE',  ( 0.1532563361054083140, 66.00893115100079456, 1.131784320476157264E-15 ) ) ;
#52575 = CARTESIAN_POINT ( 'NONE',  ( 3.969999999999999751, 9.750000000000000000, -4.000000000000000000 ) ) ;
#52576 = CARTESIAN_POINT ( 'NONE',  ( 10.00000000000000178, 3.053748834913967425, 14.16423886937410082 ) ) ;
#52577 = CARTESIAN_POINT ( 'NONE',  ( -0.3289641300567998083, 8.078790035174471029, 5.963430220938281678 ) ) ;
#52579 = CARTESIAN_POINT ( 'NONE',  ( 2.791683348922237240, 35.38393115100079456, -7.208316651077763204 ) ) ;
#52578 = CARTESIAN_POINT ( 'NONE',  ( -46.68456736488007408, 103.6675473310227034, -5.775421524742654356 ) ) ;
#52580 = CARTESIAN_POINT ( 'NONE',  ( 20.88017736071110164, 10.35535201082150714, 2.915334737309930979 ) ) ;
#52581 = DIRECTION ( 'NONE',  ( -0.000000000000000000, -0.000000000000000000, 1.000000000000000000 ) ) ;
#52582 = ORIENTED_EDGE ( 'NONE', *, *, #58254, .F. ) ;
#52583 = CARTESIAN_POINT ( 'NONE',  ( -11.92686044187655980, 4.896642702460838770, 3.195792623639539087 ) ) ;
#52584 = CARTESIAN_POINT ( 'NONE',  ( 14.92337183194729988, 44.34226448433412315, -8.527530157486177487 ) ) ;
#52585 = CARTESIAN_POINT ( 'NONE',  ( 6.715867195167446901, 15.00000000000000000, -12.85095824508324469 ) ) ;
#52586 = CARTESIAN_POINT ( 'NONE',  ( -2.816281873526473856, 24.12363466993042138, 9.499525473075851096E-16 ) ) ;
#52587 = CARTESIAN_POINT ( 'NONE',  ( 19.84674366389459266, 18.71726448433411960, -2.638427012816827677 ) ) ;
#52588 = ADVANCED_FACE ( 'NONE', ( #56128 ), #45186, .T. ) ;
#52589 = VECTOR ( 'NONE', #50916, 1000.000000000000000 ) ;
#52590 = DIRECTION ( 'NONE',  ( 0.000000000000000000, 0.000000000000000000, -1.000000000000000000 ) ) ;
#52591 = CARTESIAN_POINT ( 'NONE',  ( -2.816281873526471635, 3.915301336597087456, -3.434112377981056508 ) ) ;
#52592 = CARTESIAN_POINT ( 'NONE',  ( -13.55255535720598026, 0.000000000000000000, 4.403492169842870396 ) ) ;
#52593 = ORIENTED_EDGE ( 'NONE', *, *, #93798, .T. ) ;
#52594 = EDGE_LOOP ( 'NONE', ( #41017, #55960, #84585, #12805, #30016, #43554 ) ) ;
#52595 = CARTESIAN_POINT ( 'NONE',  ( 17.96484262340118221, 21.18868534415483396, -7.964842623401177768 ) ) ;
#52596 = CARTESIAN_POINT ( 'NONE',  ( 22.26659068614894466, 18.88708216824730002, 7.082119434687054849 ) ) ;
#52597 = CARTESIAN_POINT ( 'NONE',  ( 12.63842701281683922, 29.55059781766745175, -9.846743663894590881 ) ) ;
#52598 = CARTESIAN_POINT ( 'NONE',  ( -0.8801773607111008646, 58.27201867748816966, 2.915334737309923430 ) ) ;
#52600 = CARTESIAN_POINT ( 'NONE',  ( -4.247994584727555534, -13.56436116443237516, -2.750000000000000444 ) ) ;
#52599 = CARTESIAN_POINT ( 'NONE',  ( -2.816281873526473856, 34.33196800326376064, 3.434112377981055619 ) ) ;
#52601 = CARTESIAN_POINT ( 'NONE',  ( 0.5774900079438590739, 12.64701867748817143, -5.440088680355550821 ) ) ;
#52602 = CARTESIAN_POINT ( 'NONE',  ( 1.274849032794231007, 43.57228050351031357, 6.499999999999895195 ) ) ;
#52603 = DIRECTION ( 'NONE',  ( 0.000000000000000000, 0.000000000000000000, 1.000000000000000000 ) ) ;
#52604 = CIRCLE ( 'NONE', #35036, 10.00000000000000178 ) ;
#52605 = CARTESIAN_POINT ( 'NONE',  ( 3.591859063236761518, 9.956968003263753531, 11.09922568453594849 ) ) ;
#52606 = CARTESIAN_POINT ( 'NONE',  ( 22.81628187352647785, 11.62363466993042138, 6.195893100308588602E-16 ) ) ;
#52607 = CARTESIAN_POINT ( 'NONE',  ( 2.791683348922237240, 25.38393115100078390, -7.208316651077763204 ) ) ;
#52608 = CARTESIAN_POINT ( 'NONE',  ( 10.88017736071110519, -9.436314655845157162, -2.602085213965210642E-15 ) ) ;
#52609 = CARTESIAN_POINT ( 'NONE',  ( 6.565887622018943937, 35.16530133659708923, 12.81628187352647430 ) ) ;
#52610 = CARTESIAN_POINT ( 'NONE',  ( 18.17829156368507171, 24.16792564121897158, 6.500000000000021316 ) ) ;
#52612 = CARTESIAN_POINT ( 'NONE',  ( 14.69227023463708548, 14.95077488074853456, 1.335400878252637646 ) ) ;
#52611 = CARTESIAN_POINT ( 'NONE',  ( 17.96484262340118221, 34.93868534415482685, 7.964842623401181321 ) ) ;
#52613 = VECTOR ( 'NONE', #56321, 1000.000000000000227 ) ;
#52614 = CARTESIAN_POINT ( 'NONE',  ( 2.120353041430552921, 4.509079855230530718E-16, 14.34413130794947122 ) ) ;
#52615 = CARTESIAN_POINT ( 'NONE',  ( 18.17829156368507171, 29.16792564121896447, 6.500000000000019540 ) ) ;
#52616 = CARTESIAN_POINT ( 'NONE',  ( 17.96484262340118221, 39.93868534415484106, 7.964842623401181321 ) ) ;
#52617 = CARTESIAN_POINT ( 'NONE',  ( 4.559911319644449179, 38.89701867748817676, 9.422509992056141925 ) ) ;
#52618 = CARTESIAN_POINT ( 'NONE',  ( 5.076628168052704559, 60.17559781766745175, -8.527530157486179263 ) ) ;
#52619 = ADVANCED_FACE ( 'NONE', ( #78025 ), #84551, .T. ) ;
#52620 = DIRECTION ( 'NONE',  ( -1.257568779154408793E-17, -1.000000000000000000, 0.000000000000000000 ) ) ;
#52621 = EDGE_CURVE ( 'NONE', #52153, #9012, #11989, .T. ) ;
#52622 = CARTESIAN_POINT ( 'NONE',  ( 18.52753015748617571, 38.09226448433412315, 4.923371831947298993 ) ) ;
#52623 = CARTESIAN_POINT ( 'NONE',  ( 7.084665262690076126, 14.10535201082150358, 10.88017736071109987 ) ) ;
#52624 = CARTESIAN_POINT ( 'NONE',  ( 16.40814093676324603, 12.45696800326375353, -11.09922568453594671 ) ) ;
#52625 = VERTEX_POINT ( 'NONE', #1563 ) ;
#52626 = CARTESIAN_POINT ( 'NONE',  ( 17.96484262340118221, 21.18868534415483396, -7.964842623401177768 ) ) ;
#52627 = LINE ( 'NONE', #22143, #12629 ) ;
#52628 = CARTESIAN_POINT ( 'NONE',  ( 7.084665262690076126, 32.02201867748816966, -10.88017736071110164 ) ) ;
#52629 = CARTESIAN_POINT ( 'NONE',  ( 10.00000000000000000, 4.758931151000784787, -9.846743663894594434 ) ) ;
#52630 = CARTESIAN_POINT ( 'NONE',  ( 2.917880565312950480, 40.97041550158063217, -12.26659068614894821 ) ) ;
#52631 = CARTESIAN_POINT ( 'NONE',  ( 14.92337183194729988, 24.34226448433411960, -8.527530157486177487 ) ) ;
#52632 = CARTESIAN_POINT ( 'NONE',  ( 17.96484262340118221, 46.18868534415484106, -7.964842623401177768 ) ) ;
#52633 = CARTESIAN_POINT ( 'NONE',  ( -0.3093388210927642268, 15.00000000000000000, 14.99680997725065978 ) ) ;
#52634 = CARTESIAN_POINT ( 'NONE',  ( -0.3689425029237881626, 2.428748834913967869, 10.36894250292379027 ) ) ;
#52635 = ORIENTED_EDGE ( 'NONE', *, *, #87839, .F. ) ;
#52636 = B_SPLINE_CURVE_WITH_KNOTS ( 'NONE', 3,
 ( #14758, #92211, #749, #22252, #7746, #53227 ),
 .UNSPECIFIED., .F., .F.,
 ( 4, 2, 4 ),
 ( 0.0002800484630364006439, 0.0006862541666483321437, 0.001092459870260263644 ),
 .UNSPECIFIED. ) ;
#52637 = DIRECTION ( 'NONE',  ( 0.000000000000000000, 1.000000000000000000, -0.000000000000000000 ) ) ;
#52638 = CARTESIAN_POINT ( 'NONE',  ( 19.84674366389459621, 53.50893115100078745, 7.409399052514197653E-17 ) ) ;
#52639 = ORIENTED_EDGE ( 'NONE', *, *, #78155, .T. ) ;
#52640 = VERTEX_POINT ( 'NONE', #24054 ) ;
#52641 = CARTESIAN_POINT ( 'NONE',  ( 2.917880565312950480, 20.97041550158063217, -12.26659068614894821 ) ) ;
#52642 = CARTESIAN_POINT ( 'NONE',  ( 24.16423886937410614, 19.51208216824729647, -3.795296366450302550 ) ) ;
#52643 = CARTESIAN_POINT ( 'NONE',  ( 17.96484262340118221, 64.93868534415483396, 7.964842623401181321 ) ) ;
#52644 = CARTESIAN_POINT ( 'NONE',  ( 6.204703633549690345, 65.76208216824731778, -14.16423886937410259 ) ) ;
#52645 = CARTESIAN_POINT ( 'NONE',  ( 10.00000000000000000, 2.873634669930420049, -12.81628187352647608 ) ) ;
#52646 = CARTESIAN_POINT ( 'NONE',  ( 5.076628168052704559, 45.17559781766745175, -8.527530157486179263 ) ) ;
#52647 = CARTESIAN_POINT ( 'NONE',  ( -8.028887233583267502, -1.053223610202706162, 4.000000000000000000 ) ) ;
#52649 = CARTESIAN_POINT ( 'NONE',  ( -2.816281873526473856, 14.33196800326375531, 3.434112377981055619 ) ) ;
#52648 = CARTESIAN_POINT ( 'NONE',  ( 7.084665262690076126, 47.02201867748818387, -10.88017736071110164 ) ) ;
#52650 = CARTESIAN_POINT ( 'NONE',  ( -2.266590686148945544, 16.38708216824730357, -7.082119434687050408 ) ) ;
#52651 = CARTESIAN_POINT ( 'NONE',  ( -0.8801773607110991993, 17.85535201082150536, -2.915334737309923874 ) ) ;
#52652 = CARTESIAN_POINT ( 'NONE',  ( 19.42250999205614548, 20.98035201082150891, -5.440088680355545492 ) ) ;
#52653 = CARTESIAN_POINT ( 'NONE',  ( 0.000000000000000000, -97.00000000000000000, 3.750000000000000000 ) ) ;
#52654 = CARTESIAN_POINT ( 'NONE',  ( 15.44008868035555793, 61.39701867748817676, -9.422509992056140149 ) ) ;
#52655 = CARTESIAN_POINT ( 'NONE',  ( 0.6178305044545818747, 48.49863466993042493, -9.382169495545419124 ) ) ;
#52656 = CARTESIAN_POINT ( 'NONE',  ( -2.638427012816840111, -20.03273551566587685, -9.846743663894590881 ) ) ;
#52657 = ORIENTED_EDGE ( 'NONE', *, *, #73534, .T. ) ;
#52658 = CYLINDRICAL_SURFACE ( 'NONE', #90673, 15.00000000000000000 ) ;
#52659 = ORIENTED_EDGE ( 'NONE', *, *, #19318, .F. ) ;
#52660 = DIRECTION ( 'NONE',  ( 1.257568779154408793E-17, 1.000000000000000000, -0.000000000000000000 ) ) ;
#52661 = AXIS2_PLACEMENT_3D ( 'NONE', #52798, #76296, #45303 ) ;
#52662 = EDGE_LOOP ( 'NONE', ( #97188, #39544, #10882, #61200, #14237, #7187, #87594, #39421 ) ) ;
#52663 = CARTESIAN_POINT ( 'NONE',  ( 1.180296924652878499, 0.000000000000000000, 5.323975374878061828 ) ) ;
#52665 = CARTESIAN_POINT ( 'NONE',  ( 15.44008868035555260, 4.730352010821505360, 9.422509992056143702 ) ) ;
#52664 = CARTESIAN_POINT ( 'NONE',  ( 22.26659068614895176, 64.72041550158064638, -7.082119434687042414 ) ) ;
#52667 = CARTESIAN_POINT ( 'NONE',  ( 5.076628168052703671, 41.84226448433411605, 8.527530157486179263 ) ) ;
#52666 = CARTESIAN_POINT ( 'NONE',  ( 10.00000000000000000, 24.75893115100078745, -9.846743663894594434 ) ) ;
#52668 = CARTESIAN_POINT ( 'NONE',  ( 17.96484262340118221, 64.93868534415483396, 7.964842623401181321 ) ) ;
#52669 = ADVANCED_FACE ( 'NONE', ( #62025 ), #89858, .T. ) ;
#52670 = CARTESIAN_POINT ( 'NONE',  ( -15.94000000000001371, 93.50000000000000000, 9.500000000000000000 ) ) ;
#52671 = CARTESIAN_POINT ( 'NONE',  ( 2.791683348922240793, 1.633931151000784565, 7.208316651077764092 ) ) ;
#52672 = CARTESIAN_POINT ( 'NONE',  ( 3.434112377981060948, 15.58196800326375353, 12.81628187352647430 ) ) ;
#52673 = ORIENTED_EDGE ( 'NONE', *, *, #30930, .T. ) ;
#52674 = CARTESIAN_POINT ( 'NONE',  ( 22.26659068614895176, 39.72041550158063217, -7.082119434687042414 ) ) ;
#52675 = ORIENTED_EDGE ( 'NONE', *, *, #83021, .T. ) ;
#52676 = CARTESIAN_POINT ( 'NONE',  ( 17.08211943468705840, 40.13708216824731068, -12.26659068614894466 ) ) ;
#52677 = ORIENTED_EDGE ( 'NONE', *, *, #16297, .F. ) ;
#52678 = CARTESIAN_POINT ( 'NONE',  ( 21.09922568453594849, 56.20696800326375353, 6.408140936763242479 ) ) ;
#52679 = CARTESIAN_POINT ( 'NONE',  ( 10.00000000000000000, 26.81368534415484106, -10.88017736071110342 ) ) ;
#52680 = CARTESIAN_POINT ( 'NONE',  ( 17.20831665107776587, 39.13393115100079456, -7.208316651077762316 ) ) ;
#52681 = CARTESIAN_POINT ( 'NONE',  ( -0.8801773607111009756, 28.06368534415484106, 1.068504757029289695E-15 ) ) ;
#52682 = CARTESIAN_POINT ( 'NONE',  ( 8.880000000000020322, 80.07179676972448590, 6.500000000000000888 ) ) ;
#52683 = LINE ( 'NONE', #97725, #71934 ) ;
#52684 = CARTESIAN_POINT ( 'NONE',  ( 2.791683348922240793, 51.63393115100078745, 7.208316651077764092 ) ) ;
#52685 = CARTESIAN_POINT ( 'NONE',  ( 0.1532563361054083140, 51.00893115100078745, 1.131784320476157264E-15 ) ) ;
#52687 = EDGE_LOOP ( 'NONE', ( #27805, #70994, #31627, #48836 ) ) ;
#52686 = DIRECTION ( 'NONE',  ( 1.000000000000000000, 0.000000000000000000, 0.000000000000000000 ) ) ;
#52688 = CARTESIAN_POINT ( 'NONE',  ( -0.2838433074297238012, 13.12729635533385597, 9.500000000000000000 ) ) ;
#52689 = CARTESIAN_POINT ( 'NONE',  ( -12.00809552683971759, 14.49999999999999112, 8.989195838243478676 ) ) ;
#52690 = FACE_OUTER_BOUND ( 'NONE', #91569, .T. ) ;
#52691 = ORIENTED_EDGE ( 'NONE', *, *, #76676, .T. ) ;
#52692 = CARTESIAN_POINT ( 'NONE',  ( 5.054308323419867577, 70.51564955044841554, -12.00000000000000000 ) ) ;
#52693 = CARTESIAN_POINT ( 'NONE',  ( 14.92337183194729633, 37.67559781766745175, 8.527530157486181039 ) ) ;
#52694 = DIRECTION ( 'NONE',  ( 0.000000000000000000, 0.000000000000000000, -1.000000000000000000 ) ) ;
#52695 = CARTESIAN_POINT ( 'NONE',  ( -1.099225684535947600, 39.54030133659708923, 6.408140936763237150 ) ) ;
#52696 = CYLINDRICAL_SURFACE ( 'NONE', #64330, 1.000000000000007772 ) ;
#52697 = ORIENTED_EDGE ( 'NONE', *, *, #89650, .T. ) ;
#52698 = CARTESIAN_POINT ( 'NONE',  ( 0.1532563361054082862, 61.21726448433412315, 2.638427012816831674 ) ) ;
#52699 = CARTESIAN_POINT ( 'NONE',  ( -11.49658347684252924, 14.95037108522090463, -9.245857368724228920 ) ) ;
#52700 = CARTESIAN_POINT ( 'NONE',  ( 19.84674366389459266, 38.30059781766745175, 2.638427012816836559 ) ) ;
#52701 = CARTESIAN_POINT ( 'NONE',  ( 6.204703633549690345, 35.76208216824729647, -14.16423886937410259 ) ) ;
#52702 = CARTESIAN_POINT ( 'NONE',  ( 19.84674366389459266, 43.30059781766744464, 2.638427012816836559 ) ) ;
#52703 = CARTESIAN_POINT ( 'NONE',  ( 13.43411237798106583, 47.66530133659709634, -12.81628187352647252 ) ) ;
#52704 = FACE_OUTER_BOUND ( 'NONE', #45130, .T. ) ;
#52705 = CARTESIAN_POINT ( 'NONE',  ( 10.00000000000000000, 9.758931151000785675, -9.846743663894594434 ) ) ;
#52706 = CARTESIAN_POINT ( 'NONE',  ( 10.00000000000000178, 42.25893115100078745, 9.846743663894594434 ) ) ;
#52707 = CARTESIAN_POINT ( 'NONE',  ( 10.00000000000000000, 41.81368534415484106, -10.88017736071110342 ) ) ;
#52708 = EDGE_CURVE ( 'NONE', #38399, #79527, #19976, .T. ) ;
#52709 = CARTESIAN_POINT ( 'NONE',  ( 17.20831665107776587, 39.13393115100079456, -7.208316651077762316 ) ) ;
#52710 = DIRECTION ( 'NONE',  ( 0.000000000000000000, 1.000000000000000000, 0.000000000000000000 ) ) ;
#52711 = CARTESIAN_POINT ( 'NONE',  ( 4.559911319644449179, 43.89701867748816966, 9.422509992056141925 ) ) ;
#52712 = EDGE_LOOP ( 'NONE', ( #90002, #85628, #64688, #57165 ) ) ;
#52713 = DIRECTION ( 'NONE',  ( 0.000000000000000000, 1.000000000000000000, 0.000000000000000000 ) ) ;
#52714 = CARTESIAN_POINT ( 'NONE',  ( 4.559911319644449179, 22.23035201082150536, -9.422509992056141925 ) ) ;
#52716 = CARTESIAN_POINT ( 'NONE',  ( 10.00000000000000000, 46.81368534415484106, -10.88017736071110342 ) ) ;
#52715 = CARTESIAN_POINT ( 'NONE',  ( 1.472469842513823179, 65.59226448433412315, -4.923371831947296329 ) ) ;
#52717 = CYLINDRICAL_SURFACE ( 'NONE', #23296, 15.00000000000000000 ) ;
#52718 = DIRECTION ( 'NONE',  ( 0.000000000000000000, 1.000000000000000000, 0.000000000000000000 ) ) ;
#52719 = AXIS2_PLACEMENT_3D ( 'NONE', #91617, #61108, #77096 ) ;
#52721 = DIRECTION ( 'NONE',  ( -0.000000000000000000, -1.000000000000000000, -0.000000000000000000 ) ) ;
#52720 = CARTESIAN_POINT ( 'NONE',  ( 7.084665262690076126, 44.10535201082151247, 10.88017736071109987 ) ) ;
#52722 = CARTESIAN_POINT ( 'NONE',  ( 0.1532563361054082862, 16.21726448433411960, 2.638427012816831674 ) ) ;
#52723 = CARTESIAN_POINT ( 'NONE',  ( 14.92337183194729633, 27.67559781766745530, 8.527530157486181039 ) ) ;
#52724 = CARTESIAN_POINT ( 'NONE',  ( -3.795296366450322534, 20.76208216824731068, -14.16423886937409904 ) ) ;
#52725 = CARTESIAN_POINT ( 'NONE',  ( 19.84674366389459621, 63.50893115100078745, 7.409399052514197653E-17 ) ) ;
#52726 = AXIS2_PLACEMENT_3D ( 'NONE', #30661, #9154, #92645 ) ;
#52727 = CARTESIAN_POINT ( 'NONE',  ( 17.08211943468705840, 65.13708216824730357, -12.26659068614894466 ) ) ;
#52728 = FILL_AREA_STYLE_COLOUR ( '', #94779 ) ;
#52729 = CARTESIAN_POINT ( 'NONE',  ( -0.3689425029237881626, 22.42874883491397142, 10.36894250292379027 ) ) ;
#52730 = CARTESIAN_POINT ( 'NONE',  ( 13.79529636645031943, 45.34541550158062506, -14.16423886937409904 ) ) ;
#52731 = CYLINDRICAL_SURFACE ( 'NONE', #77641, 11.25000000000000178 ) ;
#52732 = VERTEX_POINT ( 'NONE', #73362 ) ;
#52733 = CARTESIAN_POINT ( 'NONE',  ( 1.472469842513823179, 21.42559781766745175, 4.923371831947296329 ) ) ;
#52734 = EDGE_CURVE ( 'NONE', #51220, #40543, #90105, .T. ) ;
#52735 = CARTESIAN_POINT ( 'NONE',  ( 17.96484262340118221, 29.93868534415484106, 7.964842623401181321 ) ) ;
#52736 = CARTESIAN_POINT ( 'NONE',  ( 19.84674366389459266, 43.30059781766744464, 2.638427012816836559 ) ) ;
#52737 = CARTESIAN_POINT ( 'NONE',  ( 10.00000000000000000, 10.55374883491396787, -14.16423886937410082 ) ) ;
#52738 = DIRECTION ( 'NONE',  ( -1.000000000000000000, 1.257568779154408793E-17, 0.000000000000000000 ) ) ;
#52739 = CARTESIAN_POINT ( 'NONE',  ( 10.00000000000000000, 4.758931151000784787, -9.846743663894594434 ) ) ;
#52740 = CARTESIAN_POINT ( 'NONE',  ( 22.81628187352648496, 36.83196800326376064, -3.434112377981050290 ) ) ;
#52741 = CARTESIAN_POINT ( 'NONE',  ( 17.20831665107776587, 47.88393115100078745, 7.208316651077764980 ) ) ;
#52743 = EDGE_LOOP ( 'NONE', ( #59681, #17475, #4237, #71840 ) ) ;
#52742 = EDGE_CURVE ( 'NONE', #9920, #40011, #79079, .T. ) ;
#52744 = CARTESIAN_POINT ( 'NONE',  ( 7.361572987183169658, 9.967264484334119601, -9.846743663894592657 ) ) ;
#52745 = CARTESIAN_POINT ( 'NONE',  ( 7.079515573063599021, -88.00917032380691296, 4.000000000000000000 ) ) ;
#52746 = CARTESIAN_POINT ( 'NONE',  ( 17.96484262340118221, 14.93868534415484106, 7.964842623401181321 ) ) ;
#52747 = CARTESIAN_POINT ( 'NONE',  ( 17.08211943468705130, 48.47041550158063927, 12.26659068614894998 ) ) ;
#52748 = CARTESIAN_POINT ( 'NONE',  ( 15.44008868035555260, 39.73035201082150536, 9.422509992056143702 ) ) ;
#52749 =( LENGTH_UNIT ( ) NAMED_UNIT ( * ) SI_UNIT ( .MILLI., .METRE. ) );
#52750 =( GEOMETRIC_REPRESENTATION_CONTEXT ( 3 ) GLOBAL_UNCERTAINTY_ASSIGNED_CONTEXT ( ( #65148 ) ) GLOBAL_UNIT_ASSIGNED_CONTEXT ( ( #87270, #1350, #34754 ) ) REPRESENTATION_CONTEXT ( 'NONE', 'WORKASPACE' ) );
#52751 = CARTESIAN_POINT ( 'NONE',  ( -12.22474924877152347, 0.2301506569030525307, 8.589397507024811418 ) ) ;
#52752 = CARTESIAN_POINT ( 'NONE',  ( 17.20831665107776587, 22.88393115100078745, 7.208316651077764980 ) ) ;
#52753 = CARTESIAN_POINT ( 'NONE',  ( 4.559911319644449179, 3.897018677488170990, 9.422509992056141925 ) ) ;
#52754 = CARTESIAN_POINT ( 'NONE',  ( 7.361572987183170547, 42.05059781766745886, 9.846743663894590881 ) ) ;
#52755 = CARTESIAN_POINT ( 'NONE',  ( -46.75578508127857447, 100.8424743063331022, 9.091779743865453511 ) ) ;
#52756 = CARTESIAN_POINT ( 'NONE',  ( 1.472469842513823179, 46.42559781766745175, 4.923371831947296329 ) ) ;
#52757 = CARTESIAN_POINT ( 'NONE',  ( 4.559911319644449179, 38.89701867748817676, 9.422509992056141925 ) ) ;
#52758 = ORIENTED_EDGE ( 'NONE', *, *, #72137, .T. ) ;
#52759 = AXIS2_PLACEMENT_3D ( 'NONE', #21733, #76201, #15222 ) ;
#52760 = CARTESIAN_POINT ( 'NONE',  ( 21.09922568453595559, 57.04030133659708923, -6.408140936763230044 ) ) ;
#52761 = DIRECTION ( 'NONE',  ( 0.7132504491541801217, 0.000000000000000000, 0.7009092642998523415 ) ) ;
#52762 = CARTESIAN_POINT ( 'NONE',  ( 7.361572987183169658, 4.967264484334119601, -9.846743663894592657 ) ) ;
#52763 = CARTESIAN_POINT ( 'NONE',  ( 16.40814093676323893, 60.79030133659709634, 11.09922568453595026 ) ) ;
#52765 = CARTESIAN_POINT ( 'NONE',  ( 18.52753015748618282, 38.92559781766745175, -4.923371831947291888 ) ) ;
#52764 = CARTESIAN_POINT ( 'NONE',  ( -0.8801773607111009756, 3.063685344154838397, 1.068504757029289695E-15 ) ) ;
#52766 = DIRECTION ( 'NONE',  ( -0.000000000000000000, -0.000000000000000000, -1.000000000000000000 ) ) ;
#52767 = FACE_OUTER_BOUND ( 'NONE', #44564, .T. ) ;
#52768 = CARTESIAN_POINT ( 'NONE',  ( 13.79529636645030344, 28.26208216824729647, 14.16423886937410614 ) ) ;
#52769 = CARTESIAN_POINT ( 'NONE',  ( -0.3689425029237898834, 51.17874883491397497, -10.36894250292378850 ) ) ;
#52770 = CARTESIAN_POINT ( 'NONE',  ( 7.361572987183170547, 52.05059781766745175, 9.846743663894590881 ) ) ;
#52771 = CARTESIAN_POINT ( 'NONE',  ( 2.603489959281591659, 10.43575266056827644, -6.500000000000006217 ) ) ;
#52772 = CARTESIAN_POINT ( 'NONE',  ( 15.44008868035555793, 56.39701867748817676, -9.422509992056140149 ) ) ;
#52773 = CARTESIAN_POINT ( 'NONE',  ( 1.472469842513823179, 5.592264484334118713, -4.923371831947296329 ) ) ;
#52774 = CARTESIAN_POINT ( 'NONE',  ( -3.750000001621175638, 0.08803144853710938300, 4.000000000000000000 ) ) ;
#52775 = EDGE_CURVE ( 'NONE', #15093, #5021, #4402, .T. ) ;
#52776 = EDGE_LOOP ( 'NONE', ( #50006, #32352, #83662, #55928 ) ) ;
#52777 = CARTESIAN_POINT ( 'NONE',  ( 22.81628187352647785, 56.41530133659708213, 3.434112377981063169 ) ) ;
#52778 = CARTESIAN_POINT ( 'NONE',  ( 2.035157376598824452, 63.68868534415484106, 7.964842623401179544 ) ) ;
#52779 = ORIENTED_EDGE ( 'NONE', *, *, #80844, .T. ) ;
#52780 = CARTESIAN_POINT ( 'NONE',  ( 24.16423886937410614, 4.303748834913967869, 8.672049930838204340E-16 ) ) ;
#52781 = CARTESIAN_POINT ( 'NONE',  ( 7.361572987183169658, 4.967264484334119601, -9.846743663894592657 ) ) ;
#52782 = CARTESIAN_POINT ( 'NONE',  ( 4.559911319644449179, 23.89701867748817321, 9.422509992056141925 ) ) ;
#52783 = EDGE_CURVE ( 'NONE', #59056, #29326, #96656, .T. ) ;
#52784 = ORIENTED_EDGE ( 'NONE', *, *, #63758, .F. ) ;
#52785 = AXIS2_PLACEMENT_3D ( 'NONE', #3214, #79196, #95680 ) ;
#52786 = CARTESIAN_POINT ( 'NONE',  ( 15.44008868035555260, 24.73035201082150891, 9.422509992056143702 ) ) ;
#52787 = ORIENTED_EDGE ( 'NONE', *, *, #91387, .T. ) ;
#52788 = CARTESIAN_POINT ( 'NONE',  ( 4.559911319644449179, 32.23035201082150536, -9.422509992056141925 ) ) ;
#52789 = CIRCLE ( 'NONE', #41617, 0.5000000000000004441 ) ;
#52790 = CARTESIAN_POINT ( 'NONE',  ( 7.771322705631417804, 3.835866486557528145E-16, 12.24159072199922704 ) ) ;
#52791 = EDGE_CURVE ( 'NONE', #57881, #16048, #34956, .T. ) ;
#52792 = AXIS2_PLACEMENT_3D ( 'NONE', #37527, #50539, #28528 ) ;
#52793 = VERTEX_POINT ( 'NONE', #57377 ) ;
#52794 = CARTESIAN_POINT ( 'NONE',  ( 0.6178305044545818747, 18.49863466993041428, -9.382169495545419124 ) ) ;
#52795 = CARTESIAN_POINT ( 'NONE',  ( 18.52753015748617571, 3.092264484334118269, 4.923371831947298993 ) ) ;
#52796 = DIRECTION ( 'NONE',  ( 5.506706202140776441E-14, 0.000000000000000000, 1.000000000000000000 ) ) ;
#52798 = CARTESIAN_POINT ( 'NONE',  ( -13.21236992757677164, -0.03417435944610275333, 5.338143956176621074 ) ) ;
#52797 = CARTESIAN_POINT ( 'NONE',  ( 15.44008868035555260, 14.73035201082150536, 9.422509992056143702 ) ) ;
#52799 = CARTESIAN_POINT ( 'NONE',  ( 2.791683348922237240, 0.3839311510007847872, -7.208316651077763204 ) ) ;
#52800 = AXIS2_PLACEMENT_3D ( 'NONE', #5212, #50702, #81196 ) ;
#52801 = CARTESIAN_POINT ( 'NONE',  ( 17.96484262340118221, 34.93868534415482685, 7.964842623401181321 ) ) ;
#52802 = ORIENTED_EDGE ( 'NONE', *, *, #67725, .F. ) ;
#52803 = DIRECTION ( 'NONE',  ( 0.000000000000000000, 0.000000000000000000, -1.000000000000000000 ) ) ;
#52804 = CARTESIAN_POINT ( 'NONE',  ( 10.00000000000000000, 46.81368534415484106, -10.88017736071110342 ) ) ;
#52805 = FACE_OUTER_BOUND ( 'NONE', #72487, .T. ) ;
#52806 = CARTESIAN_POINT ( 'NONE',  ( 16.40814093676324603, 57.45696800326375353, -11.09922568453594671 ) ) ;
#52807 = CARTESIAN_POINT ( 'NONE',  ( 7.084665262690076126, 49.10535201082149825, 10.88017736071109987 ) ) ;
#52808 = CARTESIAN_POINT ( 'NONE',  ( 10.00000000000000000, 2.873634669930420049, -12.81628187352647608 ) ) ;
#52809 = DIRECTION ( 'NONE',  ( -0.000000000000000000, -1.000000000000000000, -0.000000000000000000 ) ) ;
#52810 = CARTESIAN_POINT ( 'NONE',  ( 2.791683348922240793, 16.63393115100078745, 7.208316651077764092 ) ) ;
#52811 = CARTESIAN_POINT ( 'NONE',  ( 16.40814093676323893, 60.79030133659709634, 11.09922568453595026 ) ) ;
#52812 = CARTESIAN_POINT ( 'NONE',  ( -0.000000000000000000, 77.49441643560989235, 8.098090826131633335 ) ) ;
#52813 = CARTESIAN_POINT ( 'NONE',  ( 17.20831665107776587, 9.133931151000787452, -7.208316651077762316 ) ) ;
#52814 = CARTESIAN_POINT ( 'NONE',  ( 22.81628187352648496, 1.831968003263753753, -3.434112377981050290 ) ) ;
#52815 = CARTESIAN_POINT ( 'NONE',  ( 14.92337183194729988, 59.34226448433412315, -8.527530157486177487 ) ) ;
#52816 = CARTESIAN_POINT ( 'NONE',  ( 2.035157376598822676, 32.43868534415483396, -7.964842623401177768 ) ) ;
#52817 = CARTESIAN_POINT ( 'NONE',  ( 19.84674366389459621, 53.50893115100078745, 7.409399052514197653E-17 ) ) ;
#52818 = DIRECTION ( 'NONE',  ( 1.000000000000000000, 0.000000000000000000, 0.000000000000000000 ) ) ;
#52819 = CARTESIAN_POINT ( 'NONE',  ( 0.1532563361054082862, 16.21726448433411960, 2.638427012816831674 ) ) ;
#52820 = CARTESIAN_POINT ( 'NONE',  ( 10.00000000000000000, 4.758931151000784787, -9.846743663894594434 ) ) ;
#52821 = EDGE_CURVE ( 'NONE', #3216, #31971, #36359, .T. ) ;
#52823 = VERTEX_POINT ( 'NONE', #97373 ) ;
#52822 = CARTESIAN_POINT ( 'NONE',  ( 21.09922568453595559, 7.040301336597086568, -6.408140936763230044 ) ) ;
#52824 = B_SPLINE_CURVE_WITH_KNOTS ( 'NONE', 3,
 ( #19399, #71900, #33883, #39939, #3424, #86430, #2948, #48414, #25921, #78917, #10428, #11402, #79418, #64387, #79895, #94898, #41924, #3914, #64871, #9437, #95395, #90338, #73868, #42402 ),
 .UNSPECIFIED., .F., .F.,
 ( 4, 2, 2, 2, 2, 2, 2, 2, 2, 2, 2, 4 ),
 ( 6.505213034913026604E-19, 0.003101839872476766513, 0.006203679744953532159, 0.01240735948990705911, 0.02481471897981411823, 0.04962943795962823645, 0.06203679744953529557, 0.07444415693944235468, 0.08685151642934942073, 0.09305519617430298152, 0.09615703604677973415, 0.09925887591925647291 ),
 .UNSPECIFIED. ) ;
#52825 = CARTESIAN_POINT ( 'NONE',  ( 7.361572987183169658, 64.96726448433412315, -9.846743663894592657 ) ) ;
#52826 = CIRCLE ( 'NONE', #87942, 4.000000000000003553 ) ;
#52827 = CARTESIAN_POINT ( 'NONE',  ( 4.471066085427381154, -3.611416924293318953, -2.750000000000000000 ) ) ;
#52829 = EDGE_CURVE ( 'NONE', #91269, #44178, #23375, .T. ) ;
#52828 = CARTESIAN_POINT ( 'NONE',  ( 0.5774900079438607392, 3.480352010821504916, 5.440088680355550821 ) ) ;
#52830 = CARTESIAN_POINT ( 'NONE',  ( 5.076628168052704559, 45.17559781766745175, -8.527530157486179263 ) ) ;
#52831 = CARTESIAN_POINT ( 'NONE',  ( -10.98829462902744858, 46.98606209026556968, 2.900000000000000355 ) ) ;
#52832 = CARTESIAN_POINT ( 'NONE',  ( 10.00000000000000178, 4.313685344154837509, 10.88017736071110342 ) ) ;
#52833 = CARTESIAN_POINT ( 'NONE',  ( 27.50000000000000355, 35.99999999999997158, -7.000000000000000000 ) ) ;
#52834 = CARTESIAN_POINT ( 'NONE',  ( 0.5774900079438607392, 38.48035201082150536, 5.440088680355550821 ) ) ;
#52835 = CARTESIAN_POINT ( 'NONE',  ( 2.917880565312948704, 47.63708216824730357, 12.26659068614894643 ) ) ;
#52837 = CARTESIAN_POINT ( 'NONE',  ( -6.000000000000014211, 80.07179676972448590, 6.500000000000000888 ) ) ;
#52836 = CARTESIAN_POINT ( 'NONE',  ( 10.00000000000000178, 4.313685344154837509, 10.88017736071110342 ) ) ;
#52838 = CARTESIAN_POINT ( 'NONE',  ( 5.076628168052704559, 0.1755978176674514724, -8.527530157486179263 ) ) ;
#52839 = CARTESIAN_POINT ( 'NONE',  ( 0.1532563361054100626, 30.80059781766744820, -2.638427012816831230 ) ) ;
#52840 = CARTESIAN_POINT ( 'NONE',  ( 0.6178305044545818747, 13.49863466993041783, -9.382169495545419124 ) ) ;
#52841 = ORIENTED_EDGE ( 'NONE', *, *, #39625, .T. ) ;
#52842 =( NAMED_UNIT ( * ) PLANE_ANGLE_UNIT ( ) SI_UNIT ( $, .RADIAN. ) );
#52843 = CARTESIAN_POINT ( 'NONE',  ( 19.84674366389459266, 58.71726448433411605, -2.638427012816827677 ) ) ;
#52844 = DIRECTION ( 'NONE',  ( 1.000000000000000000, 0.000000000000000000, 0.000000000000000000 ) ) ;
#52845 = CARTESIAN_POINT ( 'NONE',  ( 2.791683348922237240, 65.38393115100078035, -7.208316651077763204 ) ) ;
#52846 = CARTESIAN_POINT ( 'NONE',  ( -4.164238869374099927, 12.01208216824730357, 3.795296366450308767 ) ) ;
#52847 = MECHANICAL_DESIGN_GEOMETRIC_PRESENTATION_REPRESENTATION (  '', ( #1786 ), #12875 ) ;
#52848 = CARTESIAN_POINT ( 'NONE',  ( 12.63842701281683034, 27.46726448433411250, 9.846743663894596210 ) ) ;
#52849 = DIRECTION ( 'NONE',  ( 0.000000000000000000, -1.000000000000000000, -0.000000000000000000 ) ) ;
#52850 = ORIENTED_EDGE ( 'NONE', *, *, #82319, .F. ) ;
#52851 = EDGE_CURVE ( 'NONE', #37014, #9012, #75880, .T. ) ;
#52852 = CARTESIAN_POINT ( 'NONE',  ( -2.266590686148945544, 37.22041550158063217, 7.082119434687048631 ) ) ;
#52853 = CARTESIAN_POINT ( 'NONE',  ( 10.00000000000000000, 14.75893115100078568, -9.846743663894594434 ) ) ;
#52854 = DIRECTION ( 'NONE',  ( 6.608470384673550777E-17, 1.000000000000000000, -0.000000000000000000 ) ) ;
#52855 = CARTESIAN_POINT ( 'NONE',  ( 20.88017736071110875, 35.77201867748816966, -2.915334737309920765 ) ) ;
#52856 = CARTESIAN_POINT ( 'NONE',  ( 16.40814093676324603, 57.45696800326375353, -11.09922568453594671 ) ) ;
#52857 = CARTESIAN_POINT ( 'NONE',  ( 4.559911319644449179, 2.230352010821504471, -9.422509992056141925 ) ) ;
#52858 = VECTOR ( 'NONE', #71333, 1000.000000000000000 ) ;
#52859 = CARTESIAN_POINT ( 'NONE',  ( -2.816281873526471635, 28.91530133659708213, -3.434112377981056508 ) ) ;
#52860 = SURFACE_STYLE_FILL_AREA ( #68867 ) ;
#52862 = ORIENTED_EDGE ( 'NONE', *, *, #93509, .F. ) ;
#52861 = EDGE_CURVE ( 'NONE', #51203, #10110, #97223, .T. ) ;
#52863 = CARTESIAN_POINT ( 'NONE',  ( 1.492507162822246602, 12.19955587570480837, -6.500000000000021316 ) ) ;
#52864 = CARTESIAN_POINT ( 'NONE',  ( 20.03932841506541962, 35.62161441960502373, -6.397827110478998769 ) ) ;
#52865 = CARTESIAN_POINT ( 'NONE',  ( -4.164238869374098151, 41.59541550158061796, -3.795296366450310543 ) ) ;
#52866 = CARTESIAN_POINT ( 'NONE',  ( -0.3689425029237898834, 16.17874883491396076, -10.36894250292378850 ) ) ;
#52867 = CARTESIAN_POINT ( 'NONE',  ( 12.91533473730993009, 6.605352010821504471, -10.88017736071109987 ) ) ;
#52868 = CARTESIAN_POINT ( 'NONE',  ( 2.035157376598824452, 33.68868534415484106, 7.964842623401179544 ) ) ;
#52869 = CARTESIAN_POINT ( 'NONE',  ( 9.065164099344453774, 15.00000000000000000, 11.95084933600773169 ) ) ;
#52870 = CYLINDRICAL_SURFACE ( 'NONE', #46438, 0.2500000000000002220 ) ;
#52871 = CARTESIAN_POINT ( 'NONE',  ( 10.00000000000000178, 49.31368534415484106, 10.88017736071110342 ) ) ;
#52872 = CARTESIAN_POINT ( 'NONE',  ( 4.559911319644449179, 63.89701867748817676, 9.422509992056141925 ) ) ;
#52873 = CARTESIAN_POINT ( 'NONE',  ( 16.40814093676324603, 22.45696800326375353, -11.09922568453594671 ) ) ;
#52874 = CARTESIAN_POINT ( 'NONE',  ( -2.863771337576625609, 0.04962896698837778592, 14.47259902956226618 ) ) ;
#52875 = CARTESIAN_POINT ( 'NONE',  ( -1.909764518474497796, 0.000000000000000000, 5.107897229450579779 ) ) ;
#52876 = CARTESIAN_POINT ( 'NONE',  ( 10.00000000000000178, 42.25893115100078745, 9.846743663894594434 ) ) ;
#52877 = CARTESIAN_POINT ( 'NONE',  ( -2.816281873526473856, 14.12363466993041961, 9.499525473075851096E-16 ) ) ;
#52878 = CARTESIAN_POINT ( 'NONE',  ( -0.8801773607110990882, 42.85535201082151247, -2.915334737309924318 ) ) ;
#52879 = CARTESIAN_POINT ( 'NONE',  ( 20.88017736071110164, 15.35535201082150358, 2.915334737309930979 ) ) ;
#52880 = CARTESIAN_POINT ( 'NONE',  ( 1.472469842513823179, 40.59226448433411605, -4.923371831947296329 ) ) ;
#52881 = CARTESIAN_POINT ( 'NONE',  ( -7.993487411953518418, 14.95037111676103869, 12.40005926694992766 ) ) ;
#52882 = CARTESIAN_POINT ( 'NONE',  ( 1.472469842513823179, 20.59226448433411960, -4.923371831947296329 ) ) ;
#52883 = CARTESIAN_POINT ( 'NONE',  ( 17.08211943468705840, 5.137082168247300906, -12.26659068614894466 ) ) ;
#52884 = CARTESIAN_POINT ( 'NONE',  ( 67.06412365047464164, 26.99999999999998224, 9.500000000000000000 ) ) ;
#52885 = CARTESIAN_POINT ( 'NONE',  ( 10.00000000000000178, 29.31368534415483751, 10.88017736071110342 ) ) ;
#52886 = FACE_OUTER_BOUND ( 'NONE', #8996, .T. ) ;
#52887 = CARTESIAN_POINT ( 'NONE',  ( 17.96484262340118221, 31.18868534415483751, -7.964842623401177768 ) ) ;
#52888 = CARTESIAN_POINT ( 'NONE',  ( 10.00000000000000000, 16.81368534415483751, -10.88017736071110342 ) ) ;
#52889 = VERTEX_POINT ( 'NONE', #95383 ) ;
#52890 = AXIS2_PLACEMENT_3D ( 'NONE', #30836, #97390, #66872 ) ;
#52891 = CARTESIAN_POINT ( 'NONE',  ( 20.88017736071110875, 30.77201867748816966, -2.915334737309920765 ) ) ;
#52892 = AXIS2_PLACEMENT_3D ( 'NONE', #38354, #68847, #15850 ) ;
#52893 = CARTESIAN_POINT ( 'NONE',  ( 21.09922568453595559, 52.04030133659708923, -6.408140936763230044 ) ) ;
#52894 = EDGE_CURVE ( 'NONE', #9521, #27464, #32336, .T. ) ;
#52895 = CARTESIAN_POINT ( 'NONE',  ( -0.8801773607111008646, 48.27201867748816966, 2.915334737309923430 ) ) ;
#52896 = CARTESIAN_POINT ( 'NONE',  ( 0.5774900079438590739, 47.64701867748817676, -5.440088680355550821 ) ) ;
#52897 = ORIENTED_EDGE ( 'NONE', *, *, #14142, .F. ) ;
#52898 = CARTESIAN_POINT ( 'NONE',  ( 4.559911319644449179, 32.23035201082150536, -9.422509992056141925 ) ) ;
#52899 = SURFACE_SIDE_STYLE ('',( #52414 ) ) ;
#52900 = MECHANICAL_DESIGN_GEOMETRIC_PRESENTATION_REPRESENTATION (  '', ( #46481 ), #62454 ) ;
#52901 = CARTESIAN_POINT ( 'NONE',  ( 17.08211943468705130, 48.47041550158063927, 12.26659068614894998 ) ) ;
#52902 = CARTESIAN_POINT ( 'NONE',  ( 7.084665262690076126, 54.10535201082151247, 10.88017736071109987 ) ) ;
#52903 = CARTESIAN_POINT ( 'NONE',  ( 1.274849032794292736, 52.55509018479936856, -6.499999999999977796 ) ) ;
#52904 = CARTESIAN_POINT ( 'NONE',  ( 7.361572987183170547, 57.05059781766744464, 9.846743663894590881 ) ) ;
#52905 = CARTESIAN_POINT ( 'NONE',  ( -8.900000000000000355, 75.76920769491746910, 2.900000000000000355 ) ) ;
#52906 = CARTESIAN_POINT ( 'NONE',  ( 2.791683348922240793, 36.63393115100078035, 7.208316651077764092 ) ) ;
#52907 = ORIENTED_EDGE ( 'NONE', *, *, #54085, .F. ) ;
#52908 = CARTESIAN_POINT ( 'NONE',  ( 14.92337183194729633, 32.67559781766745175, 8.527530157486181039 ) ) ;
#52909 = CARTESIAN_POINT ( 'NONE',  ( 3.469446951953614189E-15, -14.62636533006957151, 12.81628187352647608 ) ) ;
#52910 = CARTESIAN_POINT ( 'NONE',  ( 19.42250999205614193, 20.14701867748817321, 5.440088680355555262 ) ) ;
#52911 = CARTESIAN_POINT ( 'NONE',  ( 7.361572987183170547, 32.05059781766745175, 9.846743663894590881 ) ) ;
#52913 = CARTESIAN_POINT ( 'NONE',  ( 22.81628187352647785, 21.41530133659708923, 3.434112377981063169 ) ) ;
#52912 = VECTOR ( 'NONE', #29589, 999.9999999999998863 ) ;
#52915 = CARTESIAN_POINT ( 'NONE',  ( 10.00000000000000178, 59.31368534415484106, 10.88017736071110342 ) ) ;
#52914 = DIRECTION ( 'NONE',  ( 1.000000000000000000, 0.000000000000000000, 0.000000000000000000 ) ) ;
#52917 = CARTESIAN_POINT ( 'NONE',  ( -0.8801773607110991993, 2.855352010821504471, -2.915334737309923874 ) ) ;
#52916 = CARTESIAN_POINT ( 'NONE',  ( 12.91533473730993009, 36.60535201082151247, -10.88017736071109987 ) ) ;
#52918 = CARTESIAN_POINT ( 'NONE',  ( 20.36894250292379382, 48.67874883491396076, 10.36894250292379205 ) ) ;
#52919 = AXIS2_PLACEMENT_3D ( 'NONE', #16491, #86463, #85970 ) ;
#52920 = CARTESIAN_POINT ( 'NONE',  ( -9.820177974736244764, 0.2301504389881804946, -11.25994418464066271 ) ) ;
#52921 = ORIENTED_EDGE ( 'NONE', *, *, #76902, .F. ) ;
#52922 = CARTESIAN_POINT ( 'NONE',  ( 16.40814093676323893, 20.79030133659708923, 11.09922568453595026 ) ) ;
#52923 = CARTESIAN_POINT ( 'NONE',  ( -0.8801773607111009756, 8.063685344154837509, 1.068504757029289695E-15 ) ) ;
#52924 = CARTESIAN_POINT ( 'NONE',  ( 15.44008868035555793, 46.39701867748817676, -9.422509992056140149 ) ) ;
#52925 = PRESENTATION_LAYER_ASSIGNMENT (  '', '', ( #11389 ) ) ;
#52926 = CARTESIAN_POINT ( 'NONE',  ( 9.838578643762680542, 27.00180849546987716, 3.000000000000000000 ) ) ;
#52927 = ORIENTED_EDGE ( 'NONE', *, *, #77475, .F. ) ;
#52928 = CARTESIAN_POINT ( 'NONE',  ( 2.035157376598822676, 57.43868534415484106, -7.964842623401177768 ) ) ;
#52929 = AXIS2_PLACEMENT_3D ( 'NONE', #46611, #166, #22653 ) ;
#52930 = CARTESIAN_POINT ( 'NONE',  ( 12.63842701281683034, 32.46726448433412315, 9.846743663894596210 ) ) ;
#52931 = CARTESIAN_POINT ( 'NONE',  ( 2.791683348922240793, 21.63393115100078745, 7.208316651077764092 ) ) ;
#52932 = CARTESIAN_POINT ( 'NONE',  ( 12.63842701281683034, 17.46726448433411250, 9.846743663894596210 ) ) ;
#52933 = FACE_OUTER_BOUND ( 'NONE', #33702, .T. ) ;
#52935 = CARTESIAN_POINT ( 'NONE',  ( 3.591859063236761518, 34.95696800326375353, 11.09922568453594849 ) ) ;
#52934 = CARTESIAN_POINT ( 'NONE',  ( 0.2751277870542913062, 49.36607318730131055, -6.499999999999992006 ) ) ;
#52937 = DIRECTION ( 'NONE',  ( -0.000000000000000000, 1.000000000000000000, -0.000000000000000000 ) ) ;
#52936 = CARTESIAN_POINT ( 'NONE',  ( 10.00000000000000178, 17.25893115100078745, 9.846743663894594434 ) ) ;
#52938 = CARTESIAN_POINT ( 'NONE',  ( 4.645843784090633477, -0.8374430341443380721, -4.000000000000000888 ) ) ;
#52940 = ORIENTED_EDGE ( 'NONE', *, *, #5001, .F. ) ;
#52939 = CARTESIAN_POINT ( 'NONE',  ( 19.84674366389459266, 38.30059781766745175, 2.638427012816836559 ) ) ;
#52941 = FACE_OUTER_BOUND ( 'NONE', #31857, .T. ) ;
#52942 = CARTESIAN_POINT ( 'NONE',  ( 6.565887622018943937, 8.081968003263751754, -12.81628187352647608 ) ) ;
#52943 = EDGE_CURVE ( 'NONE', #98205, #13047, #92314, .T. ) ;
#52944 = CARTESIAN_POINT ( 'NONE',  ( 4.559911319644449179, 52.23035201082151247, -9.422509992056141925 ) ) ;
#52946 = ADVANCED_FACE ( 'NONE', ( #37362 ), #60825, .F. ) ;
#52945 = CARTESIAN_POINT ( 'NONE',  ( 24.16423886937409904, 34.09541550158064638, 3.795296366450317205 ) ) ;
#52947 = CARTESIAN_POINT ( 'NONE',  ( -10.31693093662312144, 89.21683745890891259, 5.695017665638099302 ) ) ;
#52948 = CARTESIAN_POINT ( 'NONE',  ( 13.79529636645030344, 28.26208216824729647, 14.16423886937410614 ) ) ;
#52949 = CARTESIAN_POINT ( 'NONE',  ( -2.266590686148945544, 52.22041550158064638, 7.082119434687048631 ) ) ;
#52950 = CARTESIAN_POINT ( 'NONE',  ( 22.26659068614895176, 9.720415501580633943, -7.082119434687042414 ) ) ;
#52952 = CARTESIAN_POINT ( 'NONE',  ( -7.232415441807424017, -88.12698951299773853, 3.750000000000000000 ) ) ;
#52951 = CARTESIAN_POINT ( 'NONE',  ( 17.08211943468705130, 28.47041550158063572, 12.26659068614894998 ) ) ;
#52953 = CARTESIAN_POINT ( 'NONE',  ( 4.559911319644449179, 47.23035201082150536, -9.422509992056141925 ) ) ;
#52954 = CARTESIAN_POINT ( 'NONE',  ( 6.452519493965914954, -47.68837976023561964, -2.750000000000000000 ) ) ;
#52955 = CARTESIAN_POINT ( 'NONE',  ( 19.84674366389459621, 28.50893115100078745, 7.409399052514197653E-17 ) ) ;
#52957 = CARTESIAN_POINT ( 'NONE',  ( 2.791683348922240793, 41.63393115100078745, 7.208316651077764092 ) ) ;
#52956 = DIRECTION ( 'NONE',  ( 0.000000000000000000, 1.000000000000000000, 0.000000000000000000 ) ) ;
#52958 = CARTESIAN_POINT ( 'NONE',  ( 15.44008868035555260, 29.73035201082150891, 9.422509992056143702 ) ) ;
#52959 = CARTESIAN_POINT ( 'NONE',  ( 3.591859063236763294, 63.29030133659708923, -11.09922568453595026 ) ) ;
#52960 = CARTESIAN_POINT ( 'NONE',  ( 2.550000000000003819, 99.99999999999998579, 8.000000000000000000 ) ) ;
#52961 = CARTESIAN_POINT ( 'NONE',  ( 19.59242374975066525, 82.55671096202544845, -5.127491817725379875 ) ) ;
#52962 = CARTESIAN_POINT ( 'NONE',  ( 12.63842701281683034, 27.46726448433411250, 9.846743663894596210 ) ) ;
#52963 = CARTESIAN_POINT ( 'NONE',  ( 3.591859063236761518, 49.95696800326375353, 11.09922568453594849 ) ) ;
#52964 = CARTESIAN_POINT ( 'NONE',  ( 14.16423886937410259, -15.69625116508602680, -2.602085213965210642E-15 ) ) ;
#52965 = CARTESIAN_POINT ( 'NONE',  ( 20.88017736071110164, 45.35535201082149115, 2.915334737309930979 ) ) ;
#52966 = CARTESIAN_POINT ( 'NONE',  ( 19.84674366389459621, 53.50893115100078745, 7.409399052514197653E-17 ) ) ;
#52967 = CARTESIAN_POINT ( 'NONE',  ( 13.79529636645031943, 35.34541550158063927, -14.16423886937409904 ) ) ;
#52968 = VERTEX_POINT ( 'NONE', #75336 ) ;
#52969 =( NAMED_UNIT ( * ) SI_UNIT ( $, .STERADIAN. ) SOLID_ANGLE_UNIT ( ) );
#52970 = CARTESIAN_POINT ( 'NONE',  ( 0.5774900079438607392, 58.48035201082151247, 5.440088680355550821 ) ) ;
#52971 = CARTESIAN_POINT ( 'NONE',  ( 10.76445796113278419, 14.99999999999804601, 9.901260316216218271 ) ) ;
#52972 = CARTESIAN_POINT ( 'NONE',  ( 10.00000000000000178, 58.05374883491397497, 14.16423886937410082 ) ) ;
#52973 = CARTESIAN_POINT ( 'NONE',  ( -1.099225684535947600, 8.706968003263753531, -6.408140936763238038 ) ) ;
#52974 = LINE ( 'NONE', #36510, #33683 ) ;
#52975 = CARTESIAN_POINT ( 'NONE',  ( 20.88017736071110875, 55.77201867748816966, -2.915334737309920765 ) ) ;
#52976 = EDGE_CURVE ( 'NONE', #62128, #75793, #62400, .T. ) ;
#52977 = CARTESIAN_POINT ( 'NONE',  ( 13.55255535720591986, -0.03417435944610275333, 4.403492169843056914 ) ) ;
#52978 = CARTESIAN_POINT ( 'NONE',  ( -46.61145641952149532, 101.4776089914260950, -8.252540973952291026 ) ) ;
#52979 = CARTESIAN_POINT ( 'NONE',  ( 6.204703633549690345, 42.84541550158063217, 14.16423886937410082 ) ) ;
#52980 = CARTESIAN_POINT ( 'NONE',  ( 2.915334737309928315, 29.52201867748817676, 10.88017736071109987 ) ) ;
#52981 = CARTESIAN_POINT ( 'NONE',  ( -0.8801773607111008646, 13.27201867748817143, 2.915334737309923430 ) ) ;
#52982 = CARTESIAN_POINT ( 'NONE',  ( 2.035157376598824452, 23.68868534415484461, 7.964842623401179544 ) ) ;
#52983 = CARTESIAN_POINT ( 'NONE',  ( 0.1532563361054083140, 61.00893115100078745, 1.131784320476157264E-15 ) ) ;
#52984 = CARTESIAN_POINT ( 'NONE',  ( 0.6178305044545838731, 54.74863466993042493, 9.382169495545420901 ) ) ;
#52985 = DIRECTION ( 'NONE',  ( -0.8038568606172123987, 0.000000000000000000, -0.5948227867513479206 ) ) ;
#52986 = ORIENTED_EDGE ( 'NONE', *, *, #83788, .T. ) ;
#52987 = CARTESIAN_POINT ( 'NONE',  ( 17.96484262340118221, 14.93868534415483751, 7.964842623401181321 ) ) ;
#52988 = CARTESIAN_POINT ( 'NONE',  ( 21.09922568453594849, 16.20696800326375353, 6.408140936763242479 ) ) ;
#52989 = CARTESIAN_POINT ( 'NONE',  ( 20.10493008474206889, 39.71697413083879269, 6.336235997365759154 ) ) ;
#52990 = VECTOR ( 'NONE', #6624, 1000.000000000000000 ) ;
#52991 = CARTESIAN_POINT ( 'NONE',  ( 14.92337183194729988, 54.34226448433412315, -8.527530157486177487 ) ) ;
#52992 = CARTESIAN_POINT ( 'NONE',  ( 20.88017736071110164, 30.35535201082151247, 2.915334737309930979 ) ) ;
#52993 = CARTESIAN_POINT ( 'NONE',  ( 13.43411237798106583, 22.66530133659708923, -12.81628187352647252 ) ) ;
#52995 = CARTESIAN_POINT ( 'NONE',  ( 19.10478245763051319, 15.10160829253885950, 5.990408912944332087 ) ) ;
#52994 = CARTESIAN_POINT ( 'NONE',  ( 17.96484262340118221, 49.93868534415484106, 7.964842623401181321 ) ) ;
#52996 = DIRECTION ( 'NONE',  ( 0.000000000000000000, 0.000000000000000000, 1.000000000000000000 ) ) ;
#52997 =( GEOMETRIC_REPRESENTATION_CONTEXT ( 3 ) GLOBAL_UNCERTAINTY_ASSIGNED_CONTEXT ( ( #89285 ) ) GLOBAL_UNIT_ASSIGNED_CONTEXT ( ( #10368, #79350, #1903 ) ) REPRESENTATION_CONTEXT ( 'NONE', 'WORKASPACE' ) );
#52998 = CARTESIAN_POINT ( 'NONE',  ( 3.591859063236761518, 54.95696800326376064, 11.09922568453594849 ) ) ;
#52999 = ORIENTED_EDGE ( 'NONE', *, *, #61604, .T. ) ;
#53000 = CARTESIAN_POINT ( 'NONE',  ( 0.5774900079438590739, 47.64701867748817676, -5.440088680355550821 ) ) ;
#53002 = CARTESIAN_POINT ( 'NONE',  ( -2.266590686148945544, 2.220415501580634388, 7.082119434687048631 ) ) ;
#53001 = CARTESIAN_POINT ( 'NONE',  ( 16.40814093676323893, 30.79030133659708923, 11.09922568453595026 ) ) ;
#53003 = CARTESIAN_POINT ( 'NONE',  ( -0.8801773607111009756, 48.06368534415484817, 1.068504757029289695E-15 ) ) ;
#53004 = CARTESIAN_POINT ( 'NONE',  ( 13.79529636645030344, 48.26208216824728936, 14.16423886937410614 ) ) ;
#53005 = CARTESIAN_POINT ( 'NONE',  ( 7.361572987183169658, 64.96726448433412315, -9.846743663894592657 ) ) ;
#53006 = CARTESIAN_POINT ( 'NONE',  ( 2.791683348922240793, 16.63393115100078745, 7.208316651077764092 ) ) ;
#53007 = CARTESIAN_POINT ( 'NONE',  ( 1.472469842513823179, 6.425597817667451750, 4.923371831947296329 ) ) ;
#53008 = CARTESIAN_POINT ( 'NONE',  ( 0.4400000000000020006, 1.019547802438468986, -2.500000000000000000 ) ) ;
#53009 = CARTESIAN_POINT ( 'NONE',  ( 20.36894250292379382, 43.67874883491397497, 10.36894250292379205 ) ) ;
#53010 = AXIS2_PLACEMENT_3D ( 'NONE', #44585, #28098, #67599 ) ;
#53011 = DIRECTION ( 'NONE',  ( -1.000000000000000000, -0.000000000000000000, 0.000000000000000000 ) ) ;
#53012 = CARTESIAN_POINT ( 'NONE',  ( 17.96484262340118221, 6.188685344154836621, -7.964842623401177768 ) ) ;
#53013 = CARTESIAN_POINT ( 'NONE',  ( -5.070949216135518967, -24.98410106518212714, -4.000000000003224088 ) ) ;
#53014 = VERTEX_POINT ( 'NONE', #54306 ) ;
#53015 = CARTESIAN_POINT ( 'NONE',  ( 0.5774900079438607392, 8.480352010821505360, 5.440088680355550821 ) ) ;
#53016 = CARTESIAN_POINT ( 'NONE',  ( 6.204703633549690345, 65.76208216824731778, -14.16423886937410259 ) ) ;
#53017 = CARTESIAN_POINT ( 'NONE',  ( 19.84674366389459621, 48.50893115100078745, 7.409399052514197653E-17 ) ) ;
#53018 = CARTESIAN_POINT ( 'NONE',  ( 13.43411237798105340, 40.58196800326375353, 12.81628187352647963 ) ) ;
#53019 = CARTESIAN_POINT ( 'NONE',  ( -9.024359497401759356, 75.07164295747612925, -2.900000000000000799 ) ) ;
#53021 = CARTESIAN_POINT ( 'NONE',  ( -2.266590686148945544, 7.220415501580634832, 7.082119434687048631 ) ) ;
#53020 = CARTESIAN_POINT ( 'NONE',  ( 3.843542995449403588, 14.76984992748860748, 14.43777707753016948 ) ) ;
#53022 = CARTESIAN_POINT ( 'NONE',  ( 20.88017736071110164, 10.35535201082150714, 2.915334737309930979 ) ) ;
#53023 = CARTESIAN_POINT ( 'NONE',  ( 17.96484262340118221, 9.938685344154839285, 7.964842623401181321 ) ) ;
#53024 = CARTESIAN_POINT ( 'NONE',  ( 0.1532563361054100626, 45.80059781766745886, -2.638427012816831230 ) ) ;
#53025 = DIRECTION ( 'NONE',  ( 1.000000000000000000, 0.000000000000000000, 0.000000000000000000 ) ) ;
#53026 = CARTESIAN_POINT ( 'NONE',  ( 0.1532563361054083140, 26.00893115100078745, 1.131784320476157264E-15 ) ) ;
#53027 = CARTESIAN_POINT ( 'NONE',  ( 9.011287250621712985, 14.76930270348881002, 11.91783356064793686 ) ) ;
#53028 = CARTESIAN_POINT ( 'NONE',  ( -3.469446951953614189E-15, 14.75893115100079100, -9.846743663894594434 ) ) ;
#53029 = ORIENTED_EDGE ( 'NONE', *, *, #69915, .T. ) ;
#53030 = ORIENTED_EDGE ( 'NONE', *, *, #61404, .T. ) ;
#53031 = DIRECTION ( 'NONE',  ( 1.000000000000000000, 0.000000000000000000, 0.000000000000000000 ) ) ;
#53032 = ORIENTED_EDGE ( 'NONE', *, *, #81374, .T. ) ;
#53033 = CARTESIAN_POINT ( 'NONE',  ( 5.076628168052704559, 60.17559781766745175, -8.527530157486179263 ) ) ;
#53035 = CARTESIAN_POINT ( 'NONE',  ( -0.8801773607111009756, 33.06368534415484106, 1.068504757029289695E-15 ) ) ;
#53034 = CARTESIAN_POINT ( 'NONE',  ( -0.8801773607111009756, 38.06368534415484106, 1.068504757029289695E-15 ) ) ;
#53037 = CARTESIAN_POINT ( 'NONE',  ( 22.81628187352647785, 26.41530133659708923, 3.434112377981063169 ) ) ;
#53036 = CARTESIAN_POINT ( 'NONE',  ( 2.791683348922237240, 65.38393115100078035, -7.208316651077763204 ) ) ;
#53038 = CARTESIAN_POINT ( 'NONE',  ( -0.3689425029237898834, 6.178748834913968757, -10.36894250292378850 ) ) ;
#53039 = EDGE_CURVE ( 'NONE', #36181, #39274, #41999, .T. ) ;
#53040 = AXIS2_PLACEMENT_3D ( 'NONE', #70255, #9742, #32721 ) ;
#53041 = CARTESIAN_POINT ( 'NONE',  ( 13.43411237798105340, 45.58196800326374643, 12.81628187352647963 ) ) ;
#53042 = ORIENTED_EDGE ( 'NONE', *, *, #94363, .T. ) ;
#53043 = CARTESIAN_POINT ( 'NONE',  ( 19.84674366389459621, 48.50893115100078745, 7.409399052514197653E-17 ) ) ;
#53044 = CARTESIAN_POINT ( 'NONE',  ( 12.91533473730993009, 6.605352010821504471, -10.88017736071109987 ) ) ;
#53045 = ORIENTED_EDGE ( 'NONE', *, *, #73534, .F. ) ;
#53046 = CARTESIAN_POINT ( 'NONE',  ( 19.42250999205614548, 15.98035201082150714, -5.440088680355545492 ) ) ;
#53047 = VERTEX_POINT ( 'NONE', #45844 ) ;
#53048 = CARTESIAN_POINT ( 'NONE',  ( 19.42250999205614548, 60.98035201082151247, -5.440088680355545492 ) ) ;
#53049 = CARTESIAN_POINT ( 'NONE',  ( 12.91533473730992121, 59.52201867748816966, 10.88017736071110164 ) ) ;
#53050 = CARTESIAN_POINT ( 'NONE',  ( 0.5774900079438607392, 63.48035201082149825, 5.440088680355550821 ) ) ;
#53051 =( BOUNDED_SURFACE ( )  B_SPLINE_SURFACE ( 1, 2, ( 
 ( #69250, #14781, #53741, #84259, #61719, #45252, #91242, #69736, #30236, #53246, #1261, #16242, #23761, #31717, #54710, #77713, #67770, #29745, #60254, #83258, #1749, #10704, #55717, #64655, #57169, #86704, #78207, #18701, #32700, #9719, #40218, #87667, #47712, #70727, #49185, #18210, #86212, #19180, #11185, #71696, #93205, #2735, #41219, #3210, #48689, #49660, #79687, #9225, #63684, #2242, #33672, #79192, #64169, #26195, #63196, #32204, #94689, #94187, #48196, #56687, #25717, #87179, #56209, #39735, #62705, #10220, #41705, #17723, #78709, #93701, #95168, #72175, #40709, #24728, #25236, #71214, #26675, #55206, #70230, #3704, #85721, #17234, #33191, #34164, #5173, #97178, #19673, #35658, #43158, #13149, #65651, #50162, #82136, #74132, #13645, #97667, #29133, #12659, #66654, #59637, #21156, #12165, #58651, #42671, #34661, #27161, #73149, #28645, #65157, #73644, #89150, #20661, #51657, #74640, #88654, #88159, #44130, #4690, #20162, #80671, #66143, #90128, #35152, #96676, #50665, #6151, #95675, #27657, #5668, #96174, #51157, #11682, #36150, #59136, #36656, #58145, #81154, #67142, #21658, #28155, #81641, #43648, #89644, #80171, #42192, #72655, #4191, #57661, #23644, #54104, #45123, #61599, #44639, #75133, #90622, #31106, #60622, #69613, #77104, #30116, #22646, #45628, #30611, #658, #76615, #91123, #8132, #39126, #69126, #31597, #61117, #53126, #68632, #92113, #14658, #83634, #15149, #76127, #84617, #91626, #37646, #16121, #8617, #38625, #14155, #84133, #29618, #7653, #38146, #162, #60124, #7142, #46605, #22146, #52630, #1135, #62091, #23142, #53615, #75630, #92600, #15645, #46127, #52142, #82638, #6638, #37156, #98669, #67652, #98162, #83133, #68143, #33560, #47602, #24619, #55085, #72065, #62583, #85605, #64056, #33078, #70603, #34049, #26087, #86588, #9106, #17608, #25603, #18097, #2623, #3590, #94568, #24124, #78591, #17120, #56095, #94083, #63574, #41097, #93088, #56582, #86097, #48078, #48574, #85106, #64545, #93584, #79073, #10103, #9599, #11076, #40600, #3105, #18581, #16617, #54593, #87072, #32589, #71097, #25120, #10586, #41597, #2129, #78096, #49073, #79576, #40102, #71594, #55603, #47093, #77591, #63084, #39620, #70109, #1634, #32085, #72544, #81530, #35034, #50548, #42555, #12054, #43532, #81042, #4077, #96060, #5558, #26561, #66537, #73038, #58533, #27543, #42081, #28537, #34540, #13036, #12550, #65034, #88545, #58037, #4574, #65537, #95561, #35542, #96563, #27050, #20046, #57057, #28038, #36034, #43052, #97064, #73531, #66034, #95052, #74027, #57548, #5058, #88047, #11562, #19559, #50056, #89041, #80560, #20552 ),
 ( #51037, #87559, #19068, #49547, #80059, #2610, #37770, #62573, #71085, #75746, #17106, #67768, #32575, #86085, #33065, #68266, #16605, #94069, #40588, #1124, #9587, #93077, #45250, #47083, #56082, #18084, #85096, #77579, #10089, #63560, #31586, #48064, #29742, #60252, #7268, #17595, #9095, #86576, #25590, #39609, #70098, #32071, #47589, #78579, #63071, #1623, #93572, #48560, #55590, #79060, #78083, #24607, #55074, #37279, #62081, #85592, #40090, #70590, #98288, #2116, #24111, #90745, #22273, #52746, #25106, #83255, #14778, #92588, #54581, #4561, #57537, #89029, #3092, #11550, #50535, #57046, #19059, #3581, #66023, #80546, #49537, #64044, #79567, #11065, #96549, #94557, #71581, #12537, #28025, #18569, #87060, #72531, #34527, #27532, #49063, #65022, #4065, #42542, #95042, #41585, #43037, #35024, #73518, #58521, #72052, #81030, #34038, #80045, #64534, #42070, #20539, #26550, #95550, #27038, #5046, #87548, #88034, #35529, #19547, #50043, #41084, #65525, #58024, #51024, #12043, #73028, #10574, #33548, #96048, #88532, #20034, #26075, #56568, #38, #60985, #29004, #90008, #52992, #83507, #74511, #90989, #74015, #5544, #21033, #60500, #21528, #30486, #7525, #59514, #52022, #75009, #60001, #29993, #7018, #82513, #37523, #68508, #98541, #91497, #90494, #14031, #98037, #22520, #44009, #44510, #6514, #37022, #15024, #22030, #67021, #45496, #38015, #36021, #52503, #67520, #29491, #14529, #83011, #75504, #44999, #23018, #66524, #68014, #75997, #81517, #13024, #6032, #43520, #97051, #28525, #59017, #51523, #82015, #89524, #13526, #36532, #97542, #9972, #61478, #30980, #16493, #77463, #70475, #91984, #8975, #46969, #85474, #38996, #23515, #55470, #47463, #85973, #70974, #2494, #84975, #39974, #32950, #93461, #84494, #31954, #15995, #8006, #533, #46483, #1995, #38504, #39491, #62456, #92958, #24987, #47949, #61972, #92471, #53986, #17483, #76979, #23997, #8492, #69982, #63451, #69490, #1506, #54470, #78459, #1007, #24492, #40477, #31469, #54956, #83998, #77965, #32461, #93957, #16985, #9471, #53486, #15521, #62956, #46003, #76493, #69000, #33916, #42923, #4931, #71938, #64423, #95935, #27417, #18454, #34913, #17964, #48451, #63926, #4448, #94930, #73403, #50413, #3461, #26431, #18948, #3945, #72918, #49922, #56931, #80433, #12416, #42435, #35411, #34417, #87432, #41955, #65410, #86942, #49425, #79928, #11436, #57909, #64908, #10946, #88421, #80923, #78949, #95433, #72419, #26927, #57425, #87918, #19434, #11931, #65903, #10460, #19921, #25482, #55966, #86467, #48938, #40970, #71467, #2980, #33429, #94441, #25953, #56456, #79446, #41470 ) ),
 .UNSPECIFIED., .F., .F., .T. ) 
 B_SPLINE_SURFACE_WITH_KNOTS ( ( 2, 2 ),
 ( 3, 2, 2, 2, 2, 2, 2, 2, 2, 2, 2, 2, 2, 2, 2, 2, 2, 2, 2, 2, 2, 2, 2, 2, 2, 2, 2, 2, 2, 2, 2, 2, 2, 2, 2, 2, 2, 2, 2, 2, 2, 2, 2, 2, 2, 2, 2, 2, 2, 2, 2, 2, 2, 2, 2, 2, 2, 2, 2, 2, 2, 2, 2, 2, 2, 2, 2, 2, 2, 2, 2, 2, 2, 2, 2, 2, 2, 2, 2, 2, 2, 2, 2, 2, 2, 2, 2, 2, 2, 2, 2, 2, 2, 2, 2, 2, 2, 2, 2, 2, 2, 2, 2, 2, 2, 2, 2, 2, 2, 2, 2, 2, 2, 2, 2, 2, 2, 2, 2, 2, 2, 2, 2, 2, 2, 2, 2, 2, 2, 2, 2, 2, 2, 2, 2, 2, 2, 2, 2, 2, 2, 2, 2, 2, 2, 2, 2, 2, 2, 2, 2, 2, 2, 2, 2, 2, 2, 2, 2, 2, 2, 2, 3 ),
 ( 0.000000000000000000, 1.000000000000000000 ),
 ( 0.000000000000000000, 0.005952380952380952051, 0.01190476190476190410, 0.01785714285714285615, 0.02380952380952380820, 0.02976190476190476025, 0.03571428571428571230, 0.04166666666666666435, 0.04761904761904761640, 0.05357142857142856845, 0.05952380952380952051, 0.06547619047619047949, 0.07142857142857142461, 0.07738095238095238360, 0.08333333333333332871, 0.08928571428571428770, 0.09523809523809523281, 0.1011904761904761918, 0.1071428571428571369, 0.1130952380952380959, 0.1190476190476190410, 0.1250000000000000000, 0.1309523809523809590, 0.1369047619047619180, 0.1428571428571428492, 0.1488095238095238082, 0.1547619047619047672, 0.1607142857142857262, 0.1666666666666666574, 0.1726190476190476164, 0.1785714285714285754, 0.1845238095238095344, 0.1904761904761904656, 0.1964285714285714246, 0.2023809523809523836, 0.2083333333333333426, 0.2142857142857142738, 0.2202380952380952328, 0.2261904761904761918, 0.2321428571428571508, 0.2380952380952380820, 0.2440476190476190410, 0.2500000000000000000, 0.2559523809523809312, 0.2619047619047619180, 0.2678571428571428492, 0.2738095238095238360, 0.2797619047619047672, 0.2857142857142856984, 0.2916666666666666852, 0.2976190476190476164, 0.3035714285714285476, 0.3095238095238095344, 0.3154761904761904656, 0.3214285714285714524, 0.3273809523809523836, 0.3333333333333333148, 0.3392857142857143016, 0.3452380952380952328, 0.3511904761904761640, 0.3571428571428571508, 0.3630952380952380820, 0.3690476190476190688, 0.3750000000000000000, 0.3809523809523809312, 0.3869047619047619180, 0.3928571428571428492, 0.3988095238095238360, 0.4047619047619047672, 0.4107142857142856984, 0.4166666666666666852, 0.4226190476190476164, 0.4285714285714285476, 0.4345238095238095344, 0.4404761904761904656, 0.4464285714285714524, 0.4523809523809523836, 0.4583333333333333148, 0.4642857142857143016, 0.4702380952380952328, 0.4761904761904761640, 0.4821428571428571508, 0.4880952380952380820, 0.4940476190476190688, 0.5000000000000000000, 0.5059523809523809312, 0.5119047619047618625, 0.5178571428571429047, 0.5238095238095238360, 0.5297619047619047672, 0.5357142857142856984, 0.5416666666666666297, 0.5476190476190476719, 0.5535714285714286031, 0.5595238095238095344, 0.5654761904761904656, 0.5714285714285713969, 0.5773809523809523281, 0.5833333333333333703, 0.5892857142857143016, 0.5952380952380952328, 0.6011904761904761640, 0.6071428571428570953, 0.6130952380952381375, 0.6190476190476190688, 0.6250000000000000000, 0.6309523809523809312, 0.6369047619047618625, 0.6428571428571429047, 0.6488095238095238360, 0.6547619047619047672, 0.6607142857142856984, 0.6666666666666666297, 0.6726190476190476719, 0.6785714285714286031, 0.6845238095238095344, 0.6904761904761904656, 0.6964285714285713969, 0.7023809523809523281, 0.7083333333333333703, 0.7142857142857143016, 0.7202380952380952328, 0.7261904761904761640, 0.7321428571428570953, 0.7380952380952381375, 0.7440476190476190688, 0.7500000000000000000, 0.7559523809523809312, 0.7619047619047618625, 0.7678571428571429047, 0.7738095238095238360, 0.7797619047619047672, 0.7857142857142856984, 0.7916666666666666297, 0.7976190476190476719, 0.8035714285714286031, 0.8095238095238095344, 0.8154761904761904656, 0.8214285714285713969, 0.8273809523809523281, 0.8333333333333333703, 0.8392857142857143016, 0.8452380952380952328, 0.8511904761904761640, 0.8571428571428570953, 0.8630952380952381375, 0.8690476190476190688, 0.8750000000000000000, 0.8809523809523809312, 0.8869047619047618625, 0.8928571428571429047, 0.8988095238095238360, 0.9047619047619047672, 0.9107142857142856984, 0.9166666666666666297, 0.9226190476190476719, 0.9285714285714286031, 0.9345238095238095344, 0.9404761904761904656, 0.9464285714285713969, 0.9523809523809523281, 0.9583333333333333703, 0.9642857142857143016 ),
 .UNSPECIFIED. ) 
 GEOMETRIC_REPRESENTATION_ITEM ( )  RATIONAL_B_SPLINE_SURFACE ( (
 ( 1.000000000000000000, 0.9659258262890683122, 1.000000000000000000, 0.9659258262890683122, 1.000000000000000000, 0.9659258262890683122, 1.000000000000000000, 0.9659258262890683122, 1.000000000000000000, 0.9659258262890683122, 1.000000000000000000, 0.9659258262890683122, 1.000000000000000000, 0.9659258262890683122, 1.000000000000000000, 0.9659258262890683122, 1.000000000000000000, 0.9659258262890683122, 1.000000000000000000, 0.9659258262890683122, 1.000000000000000000, 0.9659258262890683122, 1.000000000000000000, 0.9659258262890683122, 1.000000000000000000, 0.9659258262890683122, 1.000000000000000000, 0.9659258262890683122, 1.000000000000000000, 0.9659258262890683122, 1.000000000000000000, 0.9659258262890683122, 1.000000000000000000, 0.9659258262890683122, 1.000000000000000000, 0.9659258262890683122, 1.000000000000000000, 0.9659258262890683122, 1.000000000000000000, 0.9659258262890683122, 1.000000000000000000, 0.9659258262890683122, 1.000000000000000000, 0.9659258262890683122, 1.000000000000000000, 0.9659258262890683122, 1.000000000000000000, 0.9659258262890683122, 1.000000000000000000, 0.9659258262890683122, 1.000000000000000000, 0.9659258262890683122, 1.000000000000000000, 0.9659258262890683122, 1.000000000000000000, 0.9659258262890683122, 1.000000000000000000, 0.9659258262890683122, 1.000000000000000000, 0.9659258262890683122, 1.000000000000000000, 0.9659258262890683122, 1.000000000000000000, 0.9659258262890683122, 1.000000000000000000, 0.9659258262890683122, 1.000000000000000000, 0.9659258262890683122, 1.000000000000000000, 0.9659258262890683122, 1.000000000000000000, 0.9659258262890683122, 1.000000000000000000, 0.9659258262890683122, 1.000000000000000000, 0.9659258262890683122, 1.000000000000000000, 0.9659258262890683122, 1.000000000000000000, 0.9659258262890683122, 1.000000000000000000, 0.9659258262890683122, 1.000000000000000000, 0.9659258262890683122, 1.000000000000000000, 0.9659258262890683122, 1.000000000000000000, 0.9659258262890683122, 1.000000000000000000, 0.9659258262890683122, 1.000000000000000000, 0.9659258262890683122, 1.000000000000000000, 0.9659258262890683122, 1.000000000000000000, 0.9659258262890683122, 1.000000000000000000, 0.9659258262890683122, 1.000000000000000000, 0.9659258262890683122, 1.000000000000000000, 0.9659258262890683122, 1.000000000000000000, 0.9659258262890683122, 1.000000000000000000, 0.9659258262890683122, 1.000000000000000000, 0.9659258262890683122, 1.000000000000000000, 0.9659258262890683122, 1.000000000000000000, 0.9659258262890683122, 1.000000000000000000, 0.9659258262890683122, 1.000000000000000000, 0.9659258262890683122, 1.000000000000000000, 0.9659258262890683122, 1.000000000000000000, 0.9659258262890683122, 1.000000000000000000, 0.9659258262890683122, 1.000000000000000000, 0.9659258262890683122, 1.000000000000000000, 0.9659258262890683122, 1.000000000000000000, 0.9659258262890683122, 1.000000000000000000, 0.9659258262890683122, 1.000000000000000000, 0.9659258262890683122, 1.000000000000000000, 0.9659258262890683122, 1.000000000000000000, 0.9659258262890683122, 1.000000000000000000, 0.9659258262890683122, 1.000000000000000000, 0.9659258262890683122, 1.000000000000000000, 0.9659258262890683122, 1.000000000000000000, 0.9659258262890683122, 1.000000000000000000, 0.9659258262890683122, 1.000000000000000000, 0.9659258262890683122, 1.000000000000000000, 0.9659258262890683122, 1.000000000000000000, 0.9659258262890683122, 1.000000000000000000, 0.9659258262890683122, 1.000000000000000000, 0.9659258262890683122, 1.000000000000000000, 0.9659258262890683122, 1.000000000000000000, 0.9659258262890683122, 1.000000000000000000, 0.9659258262890683122, 1.000000000000000000, 0.9659258262890683122, 1.000000000000000000, 0.9659258262890683122, 1.000000000000000000, 0.9659258262890683122, 1.000000000000000000, 0.9659258262890683122, 1.000000000000000000, 0.9659258262890683122, 1.000000000000000000, 0.9659258262890683122, 1.000000000000000000, 0.9659258262890683122, 1.000000000000000000, 0.9659258262890683122, 1.000000000000000000, 0.9659258262890683122, 1.000000000000000000, 0.9659258262890683122, 1.000000000000000000, 0.9659258262890683122, 1.000000000000000000, 0.9659258262890683122, 1.000000000000000000, 0.9659258262890683122, 1.000000000000000000, 0.9659258262890683122, 1.000000000000000000, 0.9659258262890683122, 1.000000000000000000, 0.9659258262890683122, 1.000000000000000000, 0.9659258262890683122, 1.000000000000000000, 0.9659258262890683122, 1.000000000000000000, 0.9659258262890683122, 1.000000000000000000, 0.9659258262890683122, 1.000000000000000000, 0.9659258262890683122, 1.000000000000000000, 0.9659258262890683122, 1.000000000000000000, 0.9659258262890683122, 1.000000000000000000, 0.9659258262890683122, 1.000000000000000000, 0.9659258262890683122, 1.000000000000000000, 0.9659258262890683122, 1.000000000000000000, 0.9659258262890683122, 1.000000000000000000, 0.9659258262890683122, 1.000000000000000000, 0.9659258262890683122, 1.000000000000000000, 0.9659258262890683122, 1.000000000000000000, 0.9659258262890683122, 1.000000000000000000, 0.9659258262890683122, 1.000000000000000000, 0.9659258262890683122, 1.000000000000000000, 0.9659258262890683122, 1.000000000000000000, 0.9659258262890683122, 1.000000000000000000, 0.9659258262890683122, 1.000000000000000000, 0.9659258262890683122, 1.000000000000000000, 0.9659258262890683122, 1.000000000000000000, 0.9659258262890683122, 1.000000000000000000, 0.9659258262890683122, 1.000000000000000000, 0.9659258262890683122, 1.000000000000000000, 0.9659258262890683122, 1.000000000000000000, 0.9659258262890683122, 1.000000000000000000, 0.9659258262890683122, 1.000000000000000000, 0.9659258262890683122, 1.000000000000000000, 0.9659258262890683122, 1.000000000000000000, 0.9659258262890683122, 1.000000000000000000, 0.9659258262890683122, 1.000000000000000000, 0.9659258262890683122, 1.000000000000000000, 0.9659258262890683122, 1.000000000000000000, 0.9659258262890683122, 1.000000000000000000, 0.9659258262890683122, 1.000000000000000000, 0.9659258262890683122, 1.000000000000000000, 0.9659258262890683122, 1.000000000000000000, 0.9659258262890683122, 1.000000000000000000, 0.9659258262890683122, 1.000000000000000000, 0.9659258262890683122, 1.000000000000000000, 0.9659258262890683122, 1.000000000000000000, 0.9659258262890683122, 1.000000000000000000, 0.9659258262890683122, 1.000000000000000000, 0.9659258262890683122, 1.000000000000000000, 0.9659258262890683122, 1.000000000000000000, 0.9659258262890683122, 1.000000000000000000, 0.9659258262890683122, 1.000000000000000000, 0.9659258262890683122, 1.000000000000000000, 0.9659258262890683122, 1.000000000000000000, 0.9659258262890683122, 1.000000000000000000, 0.9659258262890683122, 1.000000000000000000, 0.9659258262890683122, 1.000000000000000000, 0.9659258262890683122, 1.000000000000000000, 0.9659258262890683122, 1.000000000000000000, 0.9659258262890683122, 1.000000000000000000, 0.9659258262890683122, 1.000000000000000000, 0.9659258262890683122, 1.000000000000000000, 0.9659258262890683122, 1.000000000000000000, 0.9659258262890683122, 1.000000000000000000, 0.9659258262890683122, 1.000000000000000000, 0.9659258262890683122, 1.000000000000000000, 0.9659258262890683122, 1.000000000000000000, 0.9659258262890683122, 1.000000000000000000, 0.9659258262890683122, 1.000000000000000000),
 ( 1.000000000000000000, 0.9659258262890683122, 1.000000000000000000, 0.9659258262890683122, 1.000000000000000000, 0.9659258262890683122, 1.000000000000000000, 0.9659258262890683122, 1.000000000000000000, 0.9659258262890683122, 1.000000000000000000, 0.9659258262890683122, 1.000000000000000000, 0.9659258262890683122, 1.000000000000000000, 0.9659258262890683122, 1.000000000000000000, 0.9659258262890683122, 1.000000000000000000, 0.9659258262890683122, 1.000000000000000000, 0.9659258262890683122, 1.000000000000000000, 0.9659258262890683122, 1.000000000000000000, 0.9659258262890683122, 1.000000000000000000, 0.9659258262890683122, 1.000000000000000000, 0.9659258262890683122, 1.000000000000000000, 0.9659258262890683122, 1.000000000000000000, 0.9659258262890683122, 1.000000000000000000, 0.9659258262890683122, 1.000000000000000000, 0.9659258262890683122, 1.000000000000000000, 0.9659258262890683122, 1.000000000000000000, 0.9659258262890683122, 1.000000000000000000, 0.9659258262890683122, 1.000000000000000000, 0.9659258262890683122, 1.000000000000000000, 0.9659258262890683122, 1.000000000000000000, 0.9659258262890683122, 1.000000000000000000, 0.9659258262890683122, 1.000000000000000000, 0.9659258262890683122, 1.000000000000000000, 0.9659258262890683122, 1.000000000000000000, 0.9659258262890683122, 1.000000000000000000, 0.9659258262890683122, 1.000000000000000000, 0.9659258262890683122, 1.000000000000000000, 0.9659258262890683122, 1.000000000000000000, 0.9659258262890683122, 1.000000000000000000, 0.9659258262890683122, 1.000000000000000000, 0.9659258262890683122, 1.000000000000000000, 0.9659258262890683122, 1.000000000000000000, 0.9659258262890683122, 1.000000000000000000, 0.9659258262890683122, 1.000000000000000000, 0.9659258262890683122, 1.000000000000000000, 0.9659258262890683122, 1.000000000000000000, 0.9659258262890683122, 1.000000000000000000, 0.9659258262890683122, 1.000000000000000000, 0.9659258262890683122, 1.000000000000000000, 0.9659258262890683122, 1.000000000000000000, 0.9659258262890683122, 1.000000000000000000, 0.9659258262890683122, 1.000000000000000000, 0.9659258262890683122, 1.000000000000000000, 0.9659258262890683122, 1.000000000000000000, 0.9659258262890683122, 1.000000000000000000, 0.9659258262890683122, 1.000000000000000000, 0.9659258262890683122, 1.000000000000000000, 0.9659258262890683122, 1.000000000000000000, 0.9659258262890683122, 1.000000000000000000, 0.9659258262890683122, 1.000000000000000000, 0.9659258262890683122, 1.000000000000000000, 0.9659258262890683122, 1.000000000000000000, 0.9659258262890683122, 1.000000000000000000, 0.9659258262890683122, 1.000000000000000000, 0.9659258262890683122, 1.000000000000000000, 0.9659258262890683122, 1.000000000000000000, 0.9659258262890683122, 1.000000000000000000, 0.9659258262890683122, 1.000000000000000000, 0.9659258262890683122, 1.000000000000000000, 0.9659258262890683122, 1.000000000000000000, 0.9659258262890683122, 1.000000000000000000, 0.9659258262890683122, 1.000000000000000000, 0.9659258262890683122, 1.000000000000000000, 0.9659258262890683122, 1.000000000000000000, 0.9659258262890683122, 1.000000000000000000, 0.9659258262890683122, 1.000000000000000000, 0.9659258262890683122, 1.000000000000000000, 0.9659258262890683122, 1.000000000000000000, 0.9659258262890683122, 1.000000000000000000, 0.9659258262890683122, 1.000000000000000000, 0.9659258262890683122, 1.000000000000000000, 0.9659258262890683122, 1.000000000000000000, 0.9659258262890683122, 1.000000000000000000, 0.9659258262890683122, 1.000000000000000000, 0.9659258262890683122, 1.000000000000000000, 0.9659258262890683122, 1.000000000000000000, 0.9659258262890683122, 1.000000000000000000, 0.9659258262890683122, 1.000000000000000000, 0.9659258262890683122, 1.000000000000000000, 0.9659258262890683122, 1.000000000000000000, 0.9659258262890683122, 1.000000000000000000, 0.9659258262890683122, 1.000000000000000000, 0.9659258262890683122, 1.000000000000000000, 0.9659258262890683122, 1.000000000000000000, 0.9659258262890683122, 1.000000000000000000, 0.9659258262890683122, 1.000000000000000000, 0.9659258262890683122, 1.000000000000000000, 0.9659258262890683122, 1.000000000000000000, 0.9659258262890683122, 1.000000000000000000, 0.9659258262890683122, 1.000000000000000000, 0.9659258262890683122, 1.000000000000000000, 0.9659258262890683122, 1.000000000000000000, 0.9659258262890683122, 1.000000000000000000, 0.9659258262890683122, 1.000000000000000000, 0.9659258262890683122, 1.000000000000000000, 0.9659258262890683122, 1.000000000000000000, 0.9659258262890683122, 1.000000000000000000, 0.9659258262890683122, 1.000000000000000000, 0.9659258262890683122, 1.000000000000000000, 0.9659258262890683122, 1.000000000000000000, 0.9659258262890683122, 1.000000000000000000, 0.9659258262890683122, 1.000000000000000000, 0.9659258262890683122, 1.000000000000000000, 0.9659258262890683122, 1.000000000000000000, 0.9659258262890683122, 1.000000000000000000, 0.9659258262890683122, 1.000000000000000000, 0.9659258262890683122, 1.000000000000000000, 0.9659258262890683122, 1.000000000000000000, 0.9659258262890683122, 1.000000000000000000, 0.9659258262890683122, 1.000000000000000000, 0.9659258262890683122, 1.000000000000000000, 0.9659258262890683122, 1.000000000000000000, 0.9659258262890683122, 1.000000000000000000, 0.9659258262890683122, 1.000000000000000000, 0.9659258262890683122, 1.000000000000000000, 0.9659258262890683122, 1.000000000000000000, 0.9659258262890683122, 1.000000000000000000, 0.9659258262890683122, 1.000000000000000000, 0.9659258262890683122, 1.000000000000000000, 0.9659258262890683122, 1.000000000000000000, 0.9659258262890683122, 1.000000000000000000, 0.9659258262890683122, 1.000000000000000000, 0.9659258262890683122, 1.000000000000000000, 0.9659258262890683122, 1.000000000000000000, 0.9659258262890683122, 1.000000000000000000, 0.9659258262890683122, 1.000000000000000000, 0.9659258262890683122, 1.000000000000000000, 0.9659258262890683122, 1.000000000000000000, 0.9659258262890683122, 1.000000000000000000, 0.9659258262890683122, 1.000000000000000000, 0.9659258262890683122, 1.000000000000000000, 0.9659258262890683122, 1.000000000000000000, 0.9659258262890683122, 1.000000000000000000, 0.9659258262890683122, 1.000000000000000000, 0.9659258262890683122, 1.000000000000000000, 0.9659258262890683122, 1.000000000000000000, 0.9659258262890683122, 1.000000000000000000, 0.9659258262890683122, 1.000000000000000000, 0.9659258262890683122, 1.000000000000000000, 0.9659258262890683122, 1.000000000000000000, 0.9659258262890683122, 1.000000000000000000, 0.9659258262890683122, 1.000000000000000000, 0.9659258262890683122, 1.000000000000000000, 0.9659258262890683122, 1.000000000000000000, 0.9659258262890683122, 1.000000000000000000, 0.9659258262890683122, 1.000000000000000000, 0.9659258262890683122, 1.000000000000000000, 0.9659258262890683122, 1.000000000000000000, 0.9659258262890683122, 1.000000000000000000, 0.9659258262890683122, 1.000000000000000000, 0.9659258262890683122, 1.000000000000000000, 0.9659258262890683122, 1.000000000000000000, 0.9659258262890683122, 1.000000000000000000, 0.9659258262890683122, 1.000000000000000000, 0.9659258262890683122, 1.000000000000000000, 0.9659258262890683122, 1.000000000000000000, 0.9659258262890683122, 1.000000000000000000, 0.9659258262890683122, 1.000000000000000000) ) ) 
 REPRESENTATION_ITEM ( '' )  SURFACE ( )  );
#53052 = DIRECTION ( 'NONE',  ( 0.000000000000000000, 1.000000000000000000, 0.000000000000000000 ) ) ;
#53053 = EDGE_CURVE ( 'NONE', #98886, #21745, #30820, .T. ) ;
#53054 = CARTESIAN_POINT ( 'NONE',  ( 10.00000000000000000, 56.81368534415484106, -10.88017736071110342 ) ) ;
#53055 = FACE_OUTER_BOUND ( 'NONE', #9254, .T. ) ;
#53058 = EDGE_LOOP ( 'NONE', ( #75558, #69067, #33569 ) ) ;
#53057 = AXIS2_PLACEMENT_3D ( 'NONE', #82696, #43209, #21214 ) ;
#53056 = CARTESIAN_POINT ( 'NONE',  ( 14.26139399675174957, 15.00000000000000000, 2.619664342934486356 ) ) ;
#53059 = EDGE_CURVE ( 'NONE', #44176, #75287, #45547, .T. ) ;
#53060 = CARTESIAN_POINT ( 'NONE',  ( 2.791683348922240793, 36.63393115100078035, 7.208316651077764092 ) ) ;
#53061 = ORIENTED_EDGE ( 'NONE', *, *, #51018, .T. ) ;
#53062 = DIRECTION ( 'NONE',  ( 0.9975640502598243087, -0.06975647374412452528, -0.000000000000000000 ) ) ;
#53064 = EDGE_CURVE ( 'NONE', #32841, #50286, #13630, .T. ) ;
#53063 = SURFACE_STYLE_FILL_AREA ( #23088 ) ;
#53065 = TOROIDAL_SURFACE ( 'NONE', #62621, 14.49999999999999822, 0.5000000000000000000 ) ;
#53066 = CIRCLE ( 'NONE', #14775, 0.5000000000000004441 ) ;
#53067 = CARTESIAN_POINT ( 'NONE',  ( 22.26659068614895176, 9.720415501580633943, -7.082119434687042414 ) ) ;
#53068 = DIRECTION ( 'NONE',  ( 0.000000000000000000, 0.000000000000000000, -1.000000000000000000 ) ) ;
#53070 = CARTESIAN_POINT ( 'NONE',  ( 15.44008868035555793, 61.39701867748817676, -9.422509992056140149 ) ) ;
#53069 = CARTESIAN_POINT ( 'NONE',  ( -46.83185791578573287, 103.4687159110575010, -5.836295484760862351 ) ) ;
#53071 = CARTESIAN_POINT ( 'NONE',  ( 2.035157376598824452, 8.688685344154839285, 7.964842623401179544 ) ) ;
#53072 = CARTESIAN_POINT ( 'NONE',  ( 0.9413316022086001267, 48.45508385108958294, 6.499999999999960032 ) ) ;
#53074 = EDGE_LOOP ( 'NONE', ( #50577, #61637, #9536, #43236 ) ) ;
#53073 = CARTESIAN_POINT ( 'NONE',  ( 22.81628187352647785, 41.41530133659708923, 3.434112377981063169 ) ) ;
#53076 = PRESENTATION_LAYER_ASSIGNMENT (  '', '', ( #24273 ) ) ;
#53075 = DIRECTION ( 'NONE',  ( 0.000000000000000000, 0.000000000000000000, -1.000000000000000000 ) ) ;
#53077 = CARTESIAN_POINT ( 'NONE',  ( 19.84674366389459621, 48.50893115100078745, 7.409399052514197653E-17 ) ) ;
#53078 = PRESENTATION_STYLE_ASSIGNMENT (( #91074 ) ) ;
#53079 = CARTESIAN_POINT ( 'NONE',  ( 19.38216949554541202, 15.99863466993042138, 9.382169495545424454 ) ) ;
#53080 = CARTESIAN_POINT ( 'NONE',  ( 10.00000000000000178, 22.25893115100078745, 9.846743663894594434 ) ) ;
#53081 = FILL_AREA_STYLE ('',( #46565 ) ) ;
#53082 = CARTESIAN_POINT ( 'NONE',  ( 1.472469842513823179, 20.59226448433411960, -4.923371831947296329 ) ) ;
#53083 = CARTESIAN_POINT ( 'NONE',  ( 0.1532563361054100626, 65.80059781766745175, -2.638427012816831230 ) ) ;
#53084 = VECTOR ( 'NONE', #79200, 1000.000000000000114 ) ;
#53085 = LINE ( 'NONE', #82599, #73903 ) ;
#53087 = ORIENTED_EDGE ( 'NONE', *, *, #43631, .T. ) ;
#53086 = ADVANCED_FACE ( 'NONE', ( #67351 ), #15225, .T. ) ;
#53088 = ORIENTED_EDGE ( 'NONE', *, *, #9284, .F. ) ;
#53089 = CARTESIAN_POINT ( 'NONE',  ( 2.035157376598822676, 22.43868534415483396, -7.964842623401177768 ) ) ;
#53090 = CARTESIAN_POINT ( 'NONE',  ( 20.36894250292379738, 14.92874883491396432, -10.36894250292379027 ) ) ;
#53091 = CARTESIAN_POINT ( 'NONE',  ( 10.00000000000000178, 27.25893115100078390, 9.846743663894594434 ) ) ;
#53092 = CARTESIAN_POINT ( 'NONE',  ( 19.84674366389459266, 3.300597817667451750, 2.638427012816836559 ) ) ;
#53094 = CARTESIAN_POINT ( 'NONE',  ( 19.72487221294570858, 1.866073187300754110, 6.500000000000000888 ) ) ;
#53093 = CARTESIAN_POINT ( 'NONE',  ( 3.591859063236763294, 43.29030133659708923, -11.09922568453595026 ) ) ;
#53095 = CARTESIAN_POINT ( 'NONE',  ( -0.8801773607110991993, 17.85535201082150536, -2.915334737309923874 ) ) ;
#53096 = EDGE_CURVE ( 'NONE', #91322, #44682, #75836, .T. ) ;
#53097 = CARTESIAN_POINT ( 'NONE',  ( 19.72487221294570858, 70.00000000000000000, 6.500000000000000888 ) ) ;
#53098 = VECTOR ( 'NONE', #30660, 1000.000000000000000 ) ;
#53099 = CARTESIAN_POINT ( 'NONE',  ( 22.81628187352647785, 11.41530133659708390, 3.434112377981063169 ) ) ;
#53100 = CARTESIAN_POINT ( 'NONE',  ( -1.099225684535947600, 8.706968003263753531, -6.408140936763238038 ) ) ;
#53101 = CARTESIAN_POINT ( 'NONE',  ( 12.63842701281683034, 22.46726448433411605, 9.846743663894596210 ) ) ;
#53102 = CARTESIAN_POINT ( 'NONE',  ( -5.204170427930421283E-15, -13.18631465584516071, -10.88017736071110342 ) ) ;
#53103 = CARTESIAN_POINT ( 'NONE',  ( -2.816281873526473856, 39.33196800326374643, 3.434112377981055619 ) ) ;
#53104 = SURFACE_STYLE_USAGE ( .BOTH. , #76102 ) ;
#53106 = CARTESIAN_POINT ( 'NONE',  ( -1.761054936948036165, 12.86682408883346440, -10.00000000000000000 ) ) ;
#53105 = CARTESIAN_POINT ( 'NONE',  ( -0.8801773607111008646, 43.27201867748817676, 2.915334737309923430 ) ) ;
#53107 = DIRECTION ( 'NONE',  ( 0.000000000000000000, 0.000000000000000000, -1.000000000000000000 ) ) ;
#53109 = ADVANCED_FACE ( 'NONE', ( #21867 ), #52345, .T. ) ;
#53108 = CARTESIAN_POINT ( 'NONE',  ( -0.8801773607111008646, 68.27201867748817676, 2.915334737309923430 ) ) ;
#53110 = CARTESIAN_POINT ( 'NONE',  ( 12.91533473730992121, 34.52201867748817676, 10.88017736071110164 ) ) ;
#53112 = CARTESIAN_POINT ( 'NONE',  ( 19.42250999205614193, 45.14701867748817676, 5.440088680355555262 ) ) ;
#53111 = VECTOR ( 'NONE', #19844, 1000.000000000000000 ) ;
#53113 = CARTESIAN_POINT ( 'NONE',  ( 19.80777595082616926, 60.68878173731740588, -6.499999999999965361 ) ) ;
#53114 = CARTESIAN_POINT ( 'NONE',  ( 20.15039907845753930, 70.00000000000000000, -6.262539305110068177 ) ) ;
#53115 = UNCERTAINTY_MEASURE_WITH_UNIT (LENGTH_MEASURE( 1.000000000000000082E-05 ), #82735, 'distance_accuracy_value', 'NONE');
#53116 = CARTESIAN_POINT ( 'NONE',  ( 0.1532563361054082862, 56.21726448433411605, 2.638427012816831674 ) ) ;
#53118 = LINE ( 'NONE', #72774, #92622 ) ;
#53117 = CARTESIAN_POINT ( 'NONE',  ( 12.91533473730992121, 4.522018677488169658, 10.88017736071110164 ) ) ;
#53119 = CARTESIAN_POINT ( 'NONE',  ( 19.38216949554541202, 10.99863466993042138, 9.382169495545424454 ) ) ;
#53120 = VERTEX_POINT ( 'NONE', #52833 ) ;
#53121 = CARTESIAN_POINT ( 'NONE',  ( 12.91533473730992121, 44.52201867748816966, 10.88017736071110164 ) ) ;
#53123 = CARTESIAN_POINT ( 'NONE',  ( 19.72487221294570858, 6.866073187300758107, 6.500000000000000888 ) ) ;
#53122 = CARTESIAN_POINT ( 'NONE',  ( 10.00000000000000000, -2.126365330069579951, -12.81628187352647608 ) ) ;
#53124 = CARTESIAN_POINT ( 'NONE',  ( 17.96484262340118221, 29.93868534415484106, 7.964842623401181321 ) ) ;
#53125 = CARTESIAN_POINT ( 'NONE',  ( 1.472469842513823179, 16.42559781766745175, 4.923371831947296329 ) ) ;
#53126 = CARTESIAN_POINT ( 'NONE',  ( -0.3689425029237898834, 36.17874883491396787, -10.36894250292378850 ) ) ;
#53127 = CARTESIAN_POINT ( 'NONE',  ( 18.52753015748618282, 28.92559781766745175, -4.923371831947291888 ) ) ;
#53128 = CARTESIAN_POINT ( 'NONE',  ( 19.42250999205614193, 45.14701867748817676, 5.440088680355555262 ) ) ;
#53129 = DIRECTION ( 'NONE',  ( -5.818595309480553908E-17, -1.000000000000000000, -0.000000000000000000 ) ) ;
#53130 = CARTESIAN_POINT ( 'NONE',  ( -4.164238869374099039, 1.803748834913967647, 8.674139862899312516E-16 ) ) ;
#53131 = CARTESIAN_POINT ( 'NONE',  ( -46.76825711229114546, 103.5742016582868672, 5.803477452201137865 ) ) ;
#53132 = CARTESIAN_POINT ( 'NONE',  ( 14.92337183194729988, 54.34226448433412315, -8.527530157486177487 ) ) ;
#53133 = ORIENTED_EDGE ( 'NONE', *, *, #64473, .T. ) ;
#53134 = EDGE_LOOP ( 'NONE', ( #50083, #48901, #98171, #80437, #72314 ) ) ;
#53135 = CARTESIAN_POINT ( 'NONE',  ( 24.16423886937410614, 34.51208216824731068, -3.795296366450302550 ) ) ;
#53136 = CARTESIAN_POINT ( 'NONE',  ( -2.266590686148945544, 27.22041550158063572, 7.082119434687048631 ) ) ;
#53137 = CARTESIAN_POINT ( 'NONE',  ( 7.361572987183169658, 9.967264484334119601, -9.846743663894592657 ) ) ;
#53138 = CARTESIAN_POINT ( 'NONE',  ( -0.3689425029237881626, 67.42874883491396076, 10.36894250292379027 ) ) ;
#53139 = CARTESIAN_POINT ( 'NONE',  ( 10.00000000000000000, 44.75893115100078745, -9.846743663894594434 ) ) ;
#53140 = CARTESIAN_POINT ( 'NONE',  ( -11.26387636256299274, -65.37812658113601572, 4.000000000000000000 ) ) ;
#53142 = CARTESIAN_POINT ( 'NONE',  ( -2.816281873526471635, 18.91530133659708213, -3.434112377981056508 ) ) ;
#53141 = CARTESIAN_POINT ( 'NONE',  ( 17.96484262340118221, 41.18868534415484106, -7.964842623401177768 ) ) ;
#53143 = CARTESIAN_POINT ( 'NONE',  ( 2.917880565312948704, 17.63708216824730357, 12.26659068614894643 ) ) ;
#53144 = CARTESIAN_POINT ( 'NONE',  ( -0.8801773607111009756, 8.063685344154837509, 1.068504757029289695E-15 ) ) ;
#53145 = AXIS2_PLACEMENT_3D ( 'NONE', #97242, #28710, #59698 ) ;
#53146 = CARTESIAN_POINT ( 'NONE',  ( 12.91533473730993009, 31.60535201082150891, -10.88017736071109987 ) ) ;
#53147 = CARTESIAN_POINT ( 'NONE',  ( -7.750000000000000000, 40.74999999999999289, 4.250000000000000000 ) ) ;
#53148 = CARTESIAN_POINT ( 'NONE',  ( 4.559911319644449179, 62.23035201082150536, -9.422509992056141925 ) ) ;
#53149 = AXIS2_PLACEMENT_3D ( 'NONE', #96400, #14376, #67363 ) ;
#53150 = CARTESIAN_POINT ( 'NONE',  ( 10.00000000000000178, 50.37363466993042493, 12.81628187352647608 ) ) ;
#53151 = CARTESIAN_POINT ( 'NONE',  ( -8.527530157486173934, -28.57440218233254470, 4.923371831947302546 ) ) ;
#53152 = ORIENTED_EDGE ( 'NONE', *, *, #65118, .F. ) ;
#53153 = CARTESIAN_POINT ( 'NONE',  ( 20.15039907845753220, 34.72266099184918176, 6.262539305110077059 ) ) ;
#53154 = AXIS2_PLACEMENT_3D ( 'NONE', #42780, #27267, #34770 ) ;
#53155 = VERTEX_POINT ( 'NONE', #82842 ) ;
#53156 = CYLINDRICAL_SURFACE ( 'NONE', #86056, 0.09999999999999982514 ) ;
#53157 = ORIENTED_EDGE ( 'NONE', *, *, #13791, .T. ) ;
#53158 = LINE ( 'NONE', #67685, #42496 ) ;
#53160 = CARTESIAN_POINT ( 'NONE',  ( 6.204703633549690345, 65.76208216824731778, -14.16423886937410259 ) ) ;
#53159 = CARTESIAN_POINT ( 'NONE',  ( -4.164238869374099039, 61.80374883491397497, 8.674139862899312516E-16 ) ) ;
#53162 = CARTESIAN_POINT ( 'NONE',  ( 5.076628168052704559, 55.17559781766745175, -8.527530157486179263 ) ) ;
#53161 = CARTESIAN_POINT ( 'NONE',  ( 7.361572987183170547, 17.05059781766745530, 9.846743663894590881 ) ) ;
#53163 = CARTESIAN_POINT ( 'NONE',  ( 20.24186590665276597, 49.73410085661204505, 6.114288769123062295 ) ) ;
#53164 = EDGE_CURVE ( 'NONE', #50602, #89674, #83342, .T. ) ;
#53165 = CARTESIAN_POINT ( 'NONE',  ( 18.72515096720591643, 66.07228050351029935, -6.499999999999699796 ) ) ;
#53166 = CARTESIAN_POINT ( 'NONE',  ( 19.84674366389459621, 8.508931151000785675, 7.409399052514197653E-17 ) ) ;
#53167 = CARTESIAN_POINT ( 'NONE',  ( -6.408140936763232709, 14.95696800326375886, 11.09922568453595026 ) ) ;
#53168 = VERTEX_POINT ( 'NONE', #68348 ) ;
#53169 = CARTESIAN_POINT ( 'NONE',  ( 20.36894250292379382, 28.67874883491396787, 10.36894250292379205 ) ) ;
#53170 = CARTESIAN_POINT ( 'NONE',  ( 2.917880565312950480, 45.97041550158063927, -12.26659068614894821 ) ) ;
#53171 = VERTEX_POINT ( 'NONE', #31307 ) ;
#53172 = AXIS2_PLACEMENT_3D ( 'NONE', #32360, #24890, #77865 ) ;
#53173 = CARTESIAN_POINT ( 'NONE',  ( 19.38216949554541202, 60.99863466993042493, 9.382169495545424454 ) ) ;
#53174 = CARTESIAN_POINT ( 'NONE',  ( 2.791683348922240793, 56.63393115100078035, 7.208316651077764092 ) ) ;
#53175 = CARTESIAN_POINT ( 'NONE',  ( -0.8801773607111008646, 23.27201867748817676, 2.915334737309923430 ) ) ;
#53176 = CARTESIAN_POINT ( 'NONE',  ( 10.00000000000000178, 65.37363466993042493, 12.81628187352647608 ) ) ;
#53177 = CARTESIAN_POINT ( 'NONE',  ( 0.000000000000000000, 15.00000000000000000, 0.000000000000000000 ) ) ;
#53178 = CARTESIAN_POINT ( 'NONE',  ( 14.92337183194729988, 59.34226448433412315, -8.527530157486177487 ) ) ;
#53179 = CARTESIAN_POINT ( 'NONE',  ( 19.84674366389459621, 48.50893115100078745, 7.409399052514197653E-17 ) ) ;
#53180 = VECTOR ( 'NONE', #4671, 1000.000000000000114 ) ;
#53182 = ORIENTED_EDGE ( 'NONE', *, *, #33793, .T. ) ;
#53181 = DIRECTION ( 'NONE',  ( 0.000000000000000000, -1.000000000000000000, 0.000000000000000000 ) ) ;
#53183 = CIRCLE ( 'NONE', #10084, 7.250000000000002665 ) ;
#53184 = EDGE_CURVE ( 'NONE', #45005, #85332, #9306, .T. ) ;
#53185 = CARTESIAN_POINT ( 'NONE',  ( 0.000000000000000000, -97.00000000000000000, 4.000000000000000000 ) ) ;
#53186 = CARTESIAN_POINT ( 'NONE',  ( 19.84674366389459266, 8.300597817667451750, 2.638427012816836559 ) ) ;
#53187 = CARTESIAN_POINT ( 'NONE',  ( 0.000000000000000000, 14.49999999999999822, 0.000000000000000000 ) ) ;
#53188 = ORIENTED_EDGE ( 'NONE', *, *, #89065, .T. ) ;
#53189 = CARTESIAN_POINT ( 'NONE',  ( 19.50000000000000355, 79.40087001978915282, 5.000000000000000000 ) ) ;
#53190 = CARTESIAN_POINT ( 'NONE',  ( 0.1532563361054083140, 26.00893115100078745, 1.131784320476157264E-15 ) ) ;
#53192 = ADVANCED_FACE ( 'NONE', ( #32786 ), #16861, .T. ) ;
#53191 = DIRECTION ( 'NONE',  ( -0.9099612708765398850, 0.000000000000000000, -0.4146932426562461860 ) ) ;
#53193 = CARTESIAN_POINT ( 'NONE',  ( 10.00000000000000000, 37.87363466993041783, -12.81628187352647608 ) ) ;
#53194 = DIRECTION ( 'NONE',  ( -0.3173046564050833740, 0.000000000000000000, -0.9483236552062023206 ) ) ;
#53195 = CARTESIAN_POINT ( 'NONE',  ( -5.991992585808429972, 15.00000000000000000, -13.20401548210301357 ) ) ;
#53196 = FACE_OUTER_BOUND ( 'NONE', #62735, .T. ) ;
#53197 = CARTESIAN_POINT ( 'NONE',  ( 34.56412365047463453, 13.99999999999999645, 10.00000000000000000 ) ) ;
#53198 = CARTESIAN_POINT ( 'NONE',  ( 0.1532563361054083140, 41.00893115100078745, 1.131784320476157264E-15 ) ) ;
#53199 = CARTESIAN_POINT ( 'NONE',  ( -0.3689425029237898834, 31.17874883491396787, -10.36894250292378850 ) ) ;
#53200 = CARTESIAN_POINT ( 'NONE',  ( 12.63842701281683922, 44.55059781766745175, -9.846743663894590881 ) ) ;
#53201 = CARTESIAN_POINT ( 'NONE',  ( 0.000000000000000000, 80.32179676972448590, -4.000000000000000000 ) ) ;
#53202 = CARTESIAN_POINT ( 'NONE',  ( 12.63842701281683034, 7.467264484334118713, 9.846743663894596210 ) ) ;
#53203 = CARTESIAN_POINT ( 'NONE',  ( 14.92337183194729633, 47.67559781766745175, 8.527530157486181039 ) ) ;
#53204 = CARTESIAN_POINT ( 'NONE',  ( -0.8801773607111009756, 53.06368534415484106, 1.068504757029289695E-15 ) ) ;
#53205 = CARTESIAN_POINT ( 'NONE',  ( 1.472469842513823179, 41.42559781766745886, 4.923371831947296329 ) ) ;
#53206 = LINE ( 'NONE', #82715, #87445 ) ;
#53207 = ORIENTED_EDGE ( 'NONE', *, *, #11057, .F. ) ;
#53208 = B_SPLINE_CURVE_WITH_KNOTS ( 'NONE', 3,
 ( #85194, #63651, #56178, #9192, #78176, #9687 ),
 .UNSPECIFIED., .F., .F.,
 ( 4, 2, 4 ),
 ( 0.0002800065468393059492, 0.0006862118402932819439, 0.001092417133747257884 ),
 .UNSPECIFIED. ) ;
#53209 = CARTESIAN_POINT ( 'NONE',  ( 19.42250999205614193, 45.14701867748817676, 5.440088680355555262 ) ) ;
#53210 = CIRCLE ( 'NONE', #64401, 13.74999999999999467 ) ;
#53211 = ORIENTED_EDGE ( 'NONE', *, *, #35332, .F. ) ;
#53212 = CARTESIAN_POINT ( 'NONE',  ( 2.148416515056625453, 52.23726573380441351, 6.499999999999959144 ) ) ;
#53213 = CARTESIAN_POINT ( 'NONE',  ( 17.96484262340118221, 34.93868534415482685, 7.964842623401181321 ) ) ;
#53215 = CARTESIAN_POINT ( 'NONE',  ( 20.88017736071110164, 50.35535201082151247, 2.915334737309930979 ) ) ;
#53214 = CARTESIAN_POINT ( 'NONE',  ( 0.1532563361054082862, 66.21726448433413736, 2.638427012816831674 ) ) ;
#53216 = CARTESIAN_POINT ( 'NONE',  ( 8.879999999999991900, 21.00000000000000000, -2.899999999999999911 ) ) ;
#53217 = AXIS2_PLACEMENT_3D ( 'NONE', #29599, #24598, #55063 ) ;
#53218 = DIRECTION ( 'NONE',  ( 0.000000000000000000, 0.000000000000000000, -1.000000000000000000 ) ) ;
#53220 = DIRECTION ( 'NONE',  ( 0.6225146366376183016, 0.000000000000000000, -0.7826081568524148047 ) ) ;
#53219 = CARTESIAN_POINT ( 'NONE',  ( 4.559911319644449179, 42.23035201082151247, -9.422509992056141925 ) ) ;
#53221 = CARTESIAN_POINT ( 'NONE',  ( 1.472469842513823179, 11.42559781766745175, 4.923371831947296329 ) ) ;
#53222 = CARTESIAN_POINT ( 'NONE',  ( 2.791683348922240793, 31.63393115100078745, 7.208316651077764092 ) ) ;
#53223 = CARTESIAN_POINT ( 'NONE',  ( -1.915564264621539392, 15.00000000000000000, 14.37291249357986445 ) ) ;
#53224 = CARTESIAN_POINT ( 'NONE',  ( -12.26659068614895354, 26.38708216824731068, -7.082119434687038861 ) ) ;
#53225 = CARTESIAN_POINT ( 'NONE',  ( -1.099225684535947600, -1.293031996736246469, -6.408140936763238038 ) ) ;
#53226 = CARTESIAN_POINT ( 'NONE',  ( -0.3689425029237898834, 66.17874883491396076, -10.36894250292378850 ) ) ;
#53227 = CARTESIAN_POINT ( 'NONE',  ( 3.420591144908583736, 14.49999999999999112, -14.60477854057961800 ) ) ;
#53228 = CARTESIAN_POINT ( 'NONE',  ( 20.36894250292379382, 18.67874883491397142, 10.36894250292379205 ) ) ;
#53229 = CARTESIAN_POINT ( 'NONE',  ( 17.08211943468705840, 50.13708216824730357, -12.26659068614894466 ) ) ;
#53230 = CARTESIAN_POINT ( 'NONE',  ( 14.92337183194729633, 12.67559781766745353, 8.527530157486181039 ) ) ;
#53231 = VERTEX_POINT ( 'NONE', #31798 ) ;
#53232 = CARTESIAN_POINT ( 'NONE',  ( 5.076628168052704559, 30.17559781766745175, -8.527530157486179263 ) ) ;
#53233 = CARTESIAN_POINT ( 'NONE',  ( 2.035157376598824452, 28.68868534415484106, 7.964842623401179544 ) ) ;
#53234 = CARTESIAN_POINT ( 'NONE',  ( 10.00000000000000000, 44.75893115100078745, -9.846743663894594434 ) ) ;
#53236 =( NAMED_UNIT ( * ) SI_UNIT ( $, .STERADIAN. ) SOLID_ANGLE_UNIT ( ) );
#53235 = CARTESIAN_POINT ( 'NONE',  ( -0.3689425029237881626, 12.42874883491396609, 10.36894250292379027 ) ) ;
#53237 = DIRECTION ( 'NONE',  ( 1.000000000000000000, 0.000000000000000000, 0.000000000000000000 ) ) ;
#53238 = CARTESIAN_POINT ( 'NONE',  ( 12.63842701281683034, 12.46726448433411782, 9.846743663894596210 ) ) ;
#53239 = CARTESIAN_POINT ( 'NONE',  ( 10.00000000000000000, 37.87363466993041783, -12.81628187352647608 ) ) ;
#53240 = CARTESIAN_POINT ( 'NONE',  ( 10.00000000000000000, 44.75893115100078745, -9.846743663894594434 ) ) ;
#53241 = EDGE_LOOP ( 'NONE', ( #50158, #75044, #49096, #48087 ) ) ;
#53242 = CARTESIAN_POINT ( 'NONE',  ( 2.791683348922240793, 26.63393115100078745, 7.208316651077764092 ) ) ;
#53243 = CARTESIAN_POINT ( 'NONE',  ( 10.89310702335901482, -97.65080521010446546, -3.750000000000675016 ) ) ;
#53244 = CARTESIAN_POINT ( 'NONE',  ( -3.750000000000000000, 9.750000000000000000, 4.000000000000000000 ) ) ;
#53245 = CARTESIAN_POINT ( 'NONE',  ( 10.00000000000000178, 58.05374883491397497, 14.16423886937410082 ) ) ;
#53246 = CARTESIAN_POINT ( 'NONE',  ( -0.3689425029237881626, 2.428748834913967869, 10.36894250292379027 ) ) ;
#53247 = CARTESIAN_POINT ( 'NONE',  ( 20.15039907845753220, 51.74884699246889852, 6.262539305110077059 ) ) ;
#53248 = CARTESIAN_POINT ( 'NONE',  ( 0.1532563361054100626, 40.80059781766745886, -2.638427012816831230 ) ) ;
#53249 = CARTESIAN_POINT ( 'NONE',  ( 0.5774900079438607392, 13.48035201082150358, 5.440088680355550821 ) ) ;
#53250 = CARTESIAN_POINT ( 'NONE',  ( 2.791683348922237240, 35.38393115100079456, -7.208316651077763204 ) ) ;
#53251 = CARTESIAN_POINT ( 'NONE',  ( -1.435044756688069745, 2.551371850025650410E-18, -0.09325026079012421754 ) ) ;
#53252 = CARTESIAN_POINT ( 'NONE',  ( 2.791683348922237240, 50.38393115100078035, -7.208316651077763204 ) ) ;
#53253 = MECHANICAL_DESIGN_GEOMETRIC_PRESENTATION_REPRESENTATION (  '', ( #40494 ), #30830 ) ;
#53254 = CARTESIAN_POINT ( 'NONE',  ( 2.035157376598822676, 52.43868534415483396, -7.964842623401177768 ) ) ;
#53255 = ORIENTED_EDGE ( 'NONE', *, *, #20020, .T. ) ;
#53256 = ORIENTED_EDGE ( 'NONE', *, *, #86497, .T. ) ;
#53257 = CARTESIAN_POINT ( 'NONE',  ( 19.38216949554541557, 57.24863466993042493, -9.382169495545420901 ) ) ;
#53258 = CARTESIAN_POINT ( 'NONE',  ( 12.14357320772536575, 54.02013147999952736, 0.000000000000000000 ) ) ;
#53259 = CARTESIAN_POINT ( 'NONE',  ( 19.84674366389459266, 13.30059781766745353, 2.638427012816836559 ) ) ;
#53260 = CARTESIAN_POINT ( 'NONE',  ( 16.40814093676324603, 62.45696800326376064, -11.09922568453594671 ) ) ;
#53262 = CARTESIAN_POINT ( 'NONE',  ( 7.361572987183169658, 49.96726448433410894, -9.846743663894592657 ) ) ;
#53261 = CARTESIAN_POINT ( 'NONE',  ( 0.5774900079438607392, 8.480352010821505360, 5.440088680355550821 ) ) ;
#53263 = PRESENTATION_STYLE_ASSIGNMENT (( #13292 ) ) ;
#53264 = CARTESIAN_POINT ( 'NONE',  ( 20.36894250292379382, 28.67874883491396787, 10.36894250292379205 ) ) ;
#53265 = CARTESIAN_POINT ( 'NONE',  ( -0.3689425029237881626, 62.42874883491396787, 10.36894250292379027 ) ) ;
#53266 = CARTESIAN_POINT ( 'NONE',  ( 5.076628168052704559, 60.17559781766745175, -8.527530157486179263 ) ) ;
#53267 = CARTESIAN_POINT ( 'NONE',  ( 17.96484262340118221, 49.93868534415484106, 7.964842623401181321 ) ) ;
#53268 = CARTESIAN_POINT ( 'NONE',  ( 19.84674366389459266, 8.717264484334116048, -2.638427012816827677 ) ) ;
#53269 =( NAMED_UNIT ( * ) PLANE_ANGLE_UNIT ( ) SI_UNIT ( $, .RADIAN. ) );
#53270 = ORIENTED_EDGE ( 'NONE', *, *, #18233, .T. ) ;
#53271 = CARTESIAN_POINT ( 'NONE',  ( 21.09922568453595559, 62.04030133659709634, -6.408140936763230044 ) ) ;
#53272 = VERTEX_POINT ( 'NONE', #78292 ) ;
#53273 = CARTESIAN_POINT ( 'NONE',  ( 5.076628168052703671, 16.84226448433411960, 8.527530157486179263 ) ) ;
#53274 = ORIENTED_EDGE ( 'NONE', *, *, #19256, .T. ) ;
#53275 = CARTESIAN_POINT ( 'NONE',  ( 10.00000000000000000, 15.55374883491396787, -14.16423886937410082 ) ) ;
#53276 = CARTESIAN_POINT ( 'NONE',  ( 7.361572987183170547, 17.05059781766745530, 9.846743663894590881 ) ) ;
#53277 = CARTESIAN_POINT ( 'NONE',  ( 17.96484262340118221, 34.93868534415482685, 7.964842623401181321 ) ) ;
#53278 = EDGE_CURVE ( 'NONE', #14929, #1780, #28123, .T. ) ;
#53279 = CARTESIAN_POINT ( 'NONE',  ( 3.836325488036181675, 14.63595249122789177, -14.50112432709423693 ) ) ;
#53280 = VERTEX_POINT ( 'NONE', #70318 ) ;
#53281 = CARTESIAN_POINT ( 'NONE',  ( 20.88017736071110875, 25.77201867748816966, -2.915334737309920765 ) ) ;
#53282 = AXIS2_PLACEMENT_3D ( 'NONE', #23771, #39258, #30742 ) ;
#53283 = ORIENTED_EDGE ( 'NONE', *, *, #79035, .F. ) ;
#53284 = CARTESIAN_POINT ( 'NONE',  ( -0.8801773607110991993, 37.85535201082151247, -2.915334737309923874 ) ) ;
#53285 = SURFACE_STYLE_FILL_AREA ( #75296 ) ;
#53286 = EDGE_LOOP ( 'NONE', ( #17024, #60, #63941, #42331 ) ) ;
#53287 = VECTOR ( 'NONE', #43410, 1000.000000000000000 ) ;
#53288 = ORIENTED_EDGE ( 'NONE', *, *, #37520, .F. ) ;
#53289 = CARTESIAN_POINT ( 'NONE',  ( 22.81628187352647785, 21.62363466993041783, 6.195893100308588602E-16 ) ) ;
#53290 = CARTESIAN_POINT ( 'NONE',  ( 10.00000000000000000, 14.75893115100078568, -9.846743663894594434 ) ) ;
#53291 = FACE_OUTER_BOUND ( 'NONE', #14290, .T. ) ;
#53292 = CARTESIAN_POINT ( 'NONE',  ( 1.377727649040772586E-15, 15.00000000000000000, 11.25000000000000178 ) ) ;
#53293 = CARTESIAN_POINT ( 'NONE',  ( 18.52753015748618282, 18.92559781766745175, -4.923371831947291888 ) ) ;
#53294 = CARTESIAN_POINT ( 'NONE',  ( 7.084665262690076126, 32.02201867748816966, -10.88017736071110164 ) ) ;
#53295 = ORIENTED_EDGE ( 'NONE', *, *, #5537, .T. ) ;
#53296 = ADVANCED_FACE ( 'NONE', ( #10303 ), #69824, .T. ) ;
#53297 = CARTESIAN_POINT ( 'NONE',  ( 10.00000000000000178, 65.37363466993042493, 12.81628187352647608 ) ) ;
#53298 = CARTESIAN_POINT ( 'NONE',  ( 12.91533473730993009, 46.60535201082150536, -10.88017736071109987 ) ) ;
#53299 = CARTESIAN_POINT ( 'NONE',  ( -1.236172813752466570, 0.04922511925147319417, 14.70095156538447867 ) ) ;
#53300 = CARTESIAN_POINT ( 'NONE',  ( 0.6178305044545818747, 53.49863466993041072, -9.382169495545419124 ) ) ;
#53301 = CARTESIAN_POINT ( 'NONE',  ( 0.5774900079438590739, 57.64701867748817676, -5.440088680355550821 ) ) ;
#53302 = CARTESIAN_POINT ( 'NONE',  ( 3.591859063236761518, -0.04303199673624671928, 11.09922568453594849 ) ) ;
#53303 = FILL_AREA_STYLE_COLOUR ( '', #27512 ) ;
#53304 = CARTESIAN_POINT ( 'NONE',  ( 12.63842701281683922, 24.55059781766745175, -9.846743663894590881 ) ) ;
#53305 = CARTESIAN_POINT ( 'NONE',  ( 10.00000000000000178, 55.37363466993042493, 12.81628187352647608 ) ) ;
#53306 = DIRECTION ( 'NONE',  ( -1.000000000000000000, -0.000000000000000000, 0.000000000000000000 ) ) ;
#53307 = CARTESIAN_POINT ( 'NONE',  ( 5.076628168052703671, 1.842264484334118047, 8.527530157486179263 ) ) ;
#53308 = CARTESIAN_POINT ( 'NONE',  ( 6.565887622018943937, 15.16530133659708568, 12.81628187352647430 ) ) ;
#53310 = CARTESIAN_POINT ( 'NONE',  ( -6.867502633528057565, -58.37509997445500431, -2.750000000000000000 ) ) ;
#53309 = CARTESIAN_POINT ( 'NONE',  ( -46.68456736488007408, 103.6675473310227034, 5.775421524742653467 ) ) ;
#53311 = CARTESIAN_POINT ( 'NONE',  ( 15.44008868035555260, 29.73035201082150891, 9.422509992056143702 ) ) ;
#53312 = CARTESIAN_POINT ( 'NONE',  ( -2.816281873526471635, -1.084698663402913210, -3.434112377981056508 ) ) ;
#53313 = PLANE ( 'NONE',  #98279 ) ;
#53314 = CARTESIAN_POINT ( 'NONE',  ( 10.00000000000000178, 17.25893115100078745, 9.846743663894594434 ) ) ;
#53315 = CARTESIAN_POINT ( 'NONE',  ( 19.84674366389459266, 3.300597817667451750, 2.638427012816836559 ) ) ;
#53317 = EDGE_LOOP ( 'NONE', ( #35570, #33176, #82284, #45539 ) ) ;
#53316 = CARTESIAN_POINT ( 'NONE',  ( 13.43411237798105340, 15.58196800326374998, 12.81628187352647963 ) ) ;
#53318 = CARTESIAN_POINT ( 'NONE',  ( 0.000000000000000000, 0.000000000000000000, 0.000000000000000000 ) ) ;
#53319 = CARTESIAN_POINT ( 'NONE',  ( 1.472469842513823179, 60.59226448433412315, -4.923371831947296329 ) ) ;
#53320 = CARTESIAN_POINT ( 'NONE',  ( 4.145754220388979228, -0.8370734722079299361, -2.500000000000000888 ) ) ;
#53321 = CARTESIAN_POINT ( 'NONE',  ( 10.00000000000000178, 68.05374883491397497, 14.16423886937410082 ) ) ;
#53322 = CARTESIAN_POINT ( 'NONE',  ( 7.361572987183170547, 42.05059781766745886, 9.846743663894590881 ) ) ;
#53323 = CARTESIAN_POINT ( 'NONE',  ( 19.72487221294571569, 65.71833443783937412, -6.499999999999983125 ) ) ;
#53324 = CARTESIAN_POINT ( 'NONE',  ( 20.88017736071110164, 5.355352010821503583, 2.915334737309930979 ) ) ;
#53325 = CARTESIAN_POINT ( 'NONE',  ( -19.00000000000000000, 75.76920769491739804, 3.000000000000000000 ) ) ;
#53326 = CARTESIAN_POINT ( 'NONE',  ( 0.5774900079438607392, 28.48035201082150891, 5.440088680355550821 ) ) ;
#53328 = CARTESIAN_POINT ( 'NONE',  ( 15.00000000000000000, 11.00000000000000000, 6.000000000000000000 ) ) ;
#53327 = CARTESIAN_POINT ( 'NONE',  ( 10.00000000000000178, 63.05374883491396076, 14.16423886937410082 ) ) ;
#53329 = EDGE_CURVE ( 'NONE', #87207, #67193, #71302, .T. ) ;
#53330 = CARTESIAN_POINT ( 'NONE',  ( 12.63842701281683034, 22.46726448433411605, 9.846743663894596210 ) ) ;
#53331 = CARTESIAN_POINT ( 'NONE',  ( 16.40814093676324603, 7.456968003263754419, -11.09922568453594671 ) ) ;
#53332 = CARTESIAN_POINT ( 'NONE',  ( 0.000000000000000000, 15.00000000000000000, 0.000000000000000000 ) ) ;
#53333 = CARTESIAN_POINT ( 'NONE',  ( -10.58981376305295008, -0.03417435944610275333, 9.535111140613638625 ) ) ;
#53334 = EDGE_CURVE ( 'NONE', #14534, #34081, #18292, .T. ) ;
#53335 = FACE_OUTER_BOUND ( 'NONE', #83586, .T. ) ;
#53336 = CARTESIAN_POINT ( 'NONE',  ( -11.51381718487193417, -65.37259455513435569, -3.999999999996394884 ) ) ;
#53337 = CARTESIAN_POINT ( 'NONE',  ( 13.79529636645031943, 10.34541550158063394, -14.16423886937409904 ) ) ;
#53338 = CARTESIAN_POINT ( 'NONE',  ( 0.1532563361054082862, 31.21726448433412315, 2.638427012816831674 ) ) ;
#53339 = PRESENTATION_STYLE_ASSIGNMENT (( #7374 ) ) ;
#53340 = ORIENTED_EDGE ( 'NONE', *, *, #82133, .T. ) ;
#53341 = TOROIDAL_SURFACE ( 'NONE', #85321, 8.250000000000000000, 0.2500000000000000000 ) ;
#53342 = CARTESIAN_POINT ( 'NONE',  ( -0.3689425029237881626, 52.42874883491396076, 10.36894250292379027 ) ) ;
#53343 = CARTESIAN_POINT ( 'NONE',  ( 18.52753015748618282, 8.925597817667451750, -4.923371831947291888 ) ) ;
#53345 = LINE ( 'NONE', #67874, #32663 ) ;
#53344 = CARTESIAN_POINT ( 'NONE',  ( -39.70923076923077133, 109.3461538461538396, -9.500000000000000000 ) ) ;
#53346 = CARTESIAN_POINT ( 'NONE',  ( 19.42250999205614548, 35.98035201082151247, -5.440088680355545492 ) ) ;
#53347 = CARTESIAN_POINT ( 'NONE',  ( 3.591859063236761518, 54.95696800326376064, 11.09922568453594849 ) ) ;
#53348 = CARTESIAN_POINT ( 'NONE',  ( 7.084665262690076126, 4.105352010821503583, 10.88017736071109987 ) ) ;
#53349 = CARTESIAN_POINT ( 'NONE',  ( 6.565887622018943937, 38.08196800326376064, -12.81628187352647608 ) ) ;
#53350 = CARTESIAN_POINT ( 'NONE',  ( 12.63842701281683034, 62.46726448433410894, 9.846743663894596210 ) ) ;
#53351 = CARTESIAN_POINT ( 'NONE',  ( 5.076628168052704559, 0.1755978176674514724, -8.527530157486179263 ) ) ;
#53352 = ORIENTED_EDGE ( 'NONE', *, *, #95101, .T. ) ;
#53353 = VECTOR ( 'NONE', #17207, 1000.000000000000227 ) ;
#53354 = CARTESIAN_POINT ( 'NONE',  ( 0.000000000000000000, 0.5000000000000004441, 0.000000000000000000 ) ) ;
#53355 = CARTESIAN_POINT ( 'NONE',  ( 11.75209714983967935, 14.95077488074854166, 8.918201205062084469 ) ) ;
#53356 = CARTESIAN_POINT ( 'NONE',  ( 24.16423886937410614, 34.51208216824731068, -3.795296366450302550 ) ) ;
#53357 = CARTESIAN_POINT ( 'NONE',  ( 17.08211943468705840, 20.13708216824730357, -12.26659068614894466 ) ) ;
#53358 = CARTESIAN_POINT ( 'NONE',  ( -0.8801773607111008646, 3.272018677488171434, 2.915334737309923430 ) ) ;
#53359 = CARTESIAN_POINT ( 'NONE',  ( 20.88017736071110875, 30.77201867748816966, -2.915334737309920765 ) ) ;
#53360 = CARTESIAN_POINT ( 'NONE',  ( -45.94000000000001194, 107.5383484153110061, 12.00000000000000000 ) ) ;
#53361 =( NAMED_UNIT ( * ) SI_UNIT ( $, .STERADIAN. ) SOLID_ANGLE_UNIT ( ) );
#53362 = CARTESIAN_POINT ( 'NONE',  ( 20.88017736071110519, 65.56368534415483396, 2.639326808657452039E-16 ) ) ;
#53363 = CARTESIAN_POINT ( 'NONE',  ( 20.88017736071110164, 60.35535201082151957, 2.915334737309930979 ) ) ;
#53364 = CARTESIAN_POINT ( 'NONE',  ( 19.38216949554541202, 30.99863466993042138, 9.382169495545424454 ) ) ;
#53365 = CARTESIAN_POINT ( 'NONE',  ( 14.64885433385999569, 14.95077488074853456, -1.748475581354204333 ) ) ;
#53366 = LINE ( 'NONE', #13401, #69063 ) ;
#53367 = CARTESIAN_POINT ( 'NONE',  ( 0.1532563361054083140, 36.00893115100078745, 1.131784320476157264E-15 ) ) ;
#53368 = CARTESIAN_POINT ( 'NONE',  ( 2.035157376598822676, 17.43868534415483751, -7.964842623401177768 ) ) ;
#53369 = CARTESIAN_POINT ( 'NONE',  ( -1.099225684535947600, 24.54030133659708923, 6.408140936763237150 ) ) ;
#53370 = CARTESIAN_POINT ( 'NONE',  ( 5.076628168052703671, 11.84226448433411960, 8.527530157486179263 ) ) ;
#53371 = CARTESIAN_POINT ( 'NONE',  ( 0.5774900079438590739, 2.647018677488170990, -5.440088680355550821 ) ) ;
#53372 = CARTESIAN_POINT ( 'NONE',  ( 12.63842701281683034, 32.46726448433412315, 9.846743663894596210 ) ) ;
#53373 = CARTESIAN_POINT ( 'NONE',  ( 22.81628187352647785, 56.41530133659708213, 3.434112377981063169 ) ) ;
#53374 = CARTESIAN_POINT ( 'NONE',  ( 7.361572987183169658, 14.96726448433411960, -9.846743663894592657 ) ) ;
#53375 = CARTESIAN_POINT ( 'NONE',  ( 17.08211943468705130, 8.470415501580635720, 12.26659068614894998 ) ) ;
#53376 = CARTESIAN_POINT ( 'NONE',  ( 18.18329248733322956, 42.60290668512021028, 6.499999999999960920 ) ) ;
#53377 = CARTESIAN_POINT ( 'NONE',  ( 12.91533473730993009, 36.60535201082151247, -10.88017736071109987 ) ) ;
#53378 = CARTESIAN_POINT ( 'NONE',  ( 12.91533473730993009, 11.60535201082150536, -10.88017736071109987 ) ) ;
#53379 = CARTESIAN_POINT ( 'NONE',  ( 19.42250999205614548, 30.98035201082150536, -5.440088680355545492 ) ) ;
#53380 = CARTESIAN_POINT ( 'NONE',  ( 4.559911319644449179, 18.89701867748817321, 9.422509992056141925 ) ) ;
#53381 = EDGE_LOOP ( 'NONE', ( #35237, #21776, #75047, #98709, #94018, #97885 ) ) ;
#53382 = CARTESIAN_POINT ( 'NONE',  ( 15.44008868035555793, 36.39701867748816966, -9.422509992056140149 ) ) ;
#53383 = AXIS2_PLACEMENT_3D ( 'NONE', #17848, #17368, #62844 ) ;
#53384 = CARTESIAN_POINT ( 'NONE',  ( 16.40814093676324603, 47.45696800326375353, -11.09922568453594671 ) ) ;
#53385 = ADVANCED_FACE ( 'NONE', ( #56296 ), #10791, .F. ) ;
#53386 = CARTESIAN_POINT ( 'NONE',  ( 7.084665262690076126, 49.10535201082149825, 10.88017736071109987 ) ) ;
#53388 = CARTESIAN_POINT ( 'NONE',  ( -0.8801773607111008646, 53.27201867748816966, 2.915334737309923430 ) ) ;
#53387 = DIRECTION ( 'NONE',  ( -0.000000000000000000, -0.000000000000000000, -1.000000000000000000 ) ) ;
#53389 = VERTEX_POINT ( 'NONE', #20750 ) ;
#53390 = CARTESIAN_POINT ( 'NONE',  ( 4.559911319644449179, 47.23035201082150536, -9.422509992056141925 ) ) ;
#53391 = CARTESIAN_POINT ( 'NONE',  ( 4.657035931881701174, -8.268334176800257396, 3.999999999999194866 ) ) ;
#53392 = CARTESIAN_POINT ( 'NONE',  ( -0.1503990784575328643, 25.12777174578613426, 6.262539305110068177 ) ) ;
#53393 = CARTESIAN_POINT ( 'NONE',  ( 22.26659068614895176, 49.72041550158063927, -7.082119434687042414 ) ) ;
#53394 = CARTESIAN_POINT ( 'NONE',  ( 12.91533473730993009, 66.60535201082150536, -10.88017736071109987 ) ) ;
#53395 = B_SPLINE_CURVE_WITH_KNOTS ( 'NONE', 3,
 ( #13827, #44308, #335, #21330, #74810, #60789 ),
 .UNSPECIFIED., .F., .F.,
 ( 4, 2, 4 ),
 ( 0.000000000000000000, 0.0002605067024380874896, 0.0005210134048761749792 ),
 .UNSPECIFIED. ) ;
#53396 = CARTESIAN_POINT ( 'NONE',  ( 19.89103541497712513, 25.66234555792570760, -6.479102184480775684 ) ) ;
#53397 = CARTESIAN_POINT ( 'NONE',  ( -3.772056942336352137, -0.8420495280537267924, -4.000000000000000000 ) ) ;
#53398 = CARTESIAN_POINT ( 'NONE',  ( 10.00000000000000178, 62.25893115100078745, 9.846743663894594434 ) ) ;
#53399 = CARTESIAN_POINT ( 'NONE',  ( -13.86186289918438952, 5.522654816098036239E-16, -4.667665767315160252 ) ) ;
#53400 = CARTESIAN_POINT ( 'NONE',  ( 14.92337183194729633, 27.67559781766745530, 8.527530157486181039 ) ) ;
#53401 = ORIENTED_EDGE ( 'NONE', *, *, #28910, .F. ) ;
#53402 = CARTESIAN_POINT ( 'NONE',  ( 17.20831665107776587, 29.13393115100078390, -7.208316651077762316 ) ) ;
#53403 = CARTESIAN_POINT ( 'NONE',  ( -12.81628187352647608, -0.8763653300695728454, 3.903127820947815962E-15 ) ) ;
#53404 = CARTESIAN_POINT ( 'NONE',  ( 12.91533473730993009, 26.60535201082150536, -10.88017736071109987 ) ) ;
#53405 = CARTESIAN_POINT ( 'NONE',  ( 18.52753015748617571, 38.09226448433412315, 4.923371831947298993 ) ) ;
#53406 = CARTESIAN_POINT ( 'NONE',  ( 0.6178305044545838731, 19.74863466993042138, 9.382169495545420901 ) ) ;
#53408 = CARTESIAN_POINT ( 'NONE',  ( 20.88017736071110519, 55.56368534415484817, 2.639326808657452039E-16 ) ) ;
#53407 = CARTESIAN_POINT ( 'NONE',  ( 2.035157376598822676, 67.43868534415484817, -7.964842623401177768 ) ) ;
#53409 = CARTESIAN_POINT ( 'NONE',  ( 10.00000000000000000, 46.81368534415484106, -10.88017736071110342 ) ) ;
#53410 = CARTESIAN_POINT ( 'NONE',  ( 6.204703633549690345, 52.84541550158062506, 14.16423886937410082 ) ) ;
#53411 = EDGE_CURVE ( 'NONE', #7169, #69512, #88250, .T. ) ;
#53412 = CARTESIAN_POINT ( 'NONE',  ( 0.6178305044545818747, 28.49863466993041783, -9.382169495545419124 ) ) ;
#53413 = CYLINDRICAL_SURFACE ( 'NONE', #3600, 1.499999999999998890 ) ;
#53414 = VERTEX_POINT ( 'NONE', #19267 ) ;
#53415 = TOROIDAL_SURFACE ( 'NONE', #91762, 2.250000000000001332, 0.2500000000000000000 ) ;
#53416 = CARTESIAN_POINT ( 'NONE',  ( -1.099225684535947600, 8.706968003263753531, -6.408140936763238038 ) ) ;
#53417 = CARTESIAN_POINT ( 'NONE',  ( -0.8801773607111009756, 18.06368534415484106, 1.068504757029289695E-15 ) ) ;
#53418 = CARTESIAN_POINT ( 'NONE',  ( 20.88017736071110519, 65.56368534415483396, 2.639326808657452039E-16 ) ) ;
#53419 = ADVANCED_FACE ( 'NONE', ( #65740 ), #8914, .T. ) ;
#53420 = VERTEX_POINT ( 'NONE', #72744 ) ;
#53421 = CARTESIAN_POINT ( 'NONE',  ( 0.5774900079438590739, 57.64701867748817676, -5.440088680355550821 ) ) ;
#53422 = CARTESIAN_POINT ( 'NONE',  ( 19.84674366389459621, 53.50893115100078745, 7.409399052514197653E-17 ) ) ;
#53423 = CARTESIAN_POINT ( 'NONE',  ( 14.92337183194729988, 19.34226448433411960, -8.527530157486177487 ) ) ;
#53424 = CARTESIAN_POINT ( 'NONE',  ( 17.20831665107776587, 27.88393115100078390, 7.208316651077764980 ) ) ;
#53425 = DIRECTION ( 'NONE',  ( 1.000000000000000000, -0.000000000000000000, 0.000000000000000000 ) ) ;
#53427 = CARTESIAN_POINT ( 'NONE',  ( 19.38216949554541557, 42.24863466993041783, -9.382169495545420901 ) ) ;
#53426 = DIRECTION ( 'NONE',  ( 1.000000000000000000, 0.000000000000000000, 0.000000000000000000 ) ) ;
#53429 = CARTESIAN_POINT ( 'NONE',  ( 19.80777595082616216, 50.68878173731742010, -6.499999999999934275 ) ) ;
#53428 = CARTESIAN_POINT ( 'NONE',  ( 0.1532563361054082862, 11.21726448433411605, 2.638427012816831674 ) ) ;
#53430 = CARTESIAN_POINT ( 'NONE',  ( 5.930053198192434039, -28.64714083316721371, -3.999999999999999112 ) ) ;
#53432 = ORIENTED_EDGE ( 'NONE', *, *, #85870, .F. ) ;
#53431 = CARTESIAN_POINT ( 'NONE',  ( 19.84674366389459621, 38.50893115100078745, 7.409399052514197653E-17 ) ) ;
#53433 =( BOUNDED_SURFACE ( )  B_SPLINE_SURFACE ( 1, 2, ( 
 ( #12494, #42994, #35978, #66479, #97007, #28485, #11024, #58979, #41542, #89482, #3537, #33997, #64495, #14485, #36976, #29950, #98988, #21484, #37481, #21988, #67476, #29451, #90945, #97996, #53442, #30936, #74967, #59958, #89968, #75954, #52464, #51982, #22475, #30442, #44957, #75460, #61435, #7965, #14982, #82469, #7481, #45453, #36486, #6976, #52950, #13485, #38463, #59466, #43963, #51479, #15477, #81973, #28963, #83461, #60455, #68468, #13990, #44465, #6472, #67970, #83951, #68955, #90450, #82966, #98495, #60941, #487, #37978, #91452, #22977, #45960, #91941, #74467, #5991, #66978, #76449, #97499, #9931, #54915, #85429, #31911, #55923, #46924, #62413, #69443, #93418, #24448, #53945, #39449, #84935, #16446, #92428, #63886, #69940, #2940, #47908, #963, #25440, #92918, #86422, #70435, #23953, #70934, #77416, #78413, #47420, #77922, #61927, #32908, #9428, #54426, #2452, #17923, #31423, #8444, #1460, #40435, #63407, #93912, #24941, #55423, #48407, #38951, #8932, #76935, #16938, #39932, #46444, #78910, #17441, #1952, #32416, #10419, #40927, #71424, #33388, #62918, #23472, #85931, #84452, #15951, #88379, #34375, #35864, #80388, #34872, #12375, #56889, #3908, #26887, #49386, #65863, #20378, #64381, #10909, #57380, #86901, #25913, #49876, #64864, #27375, #11891, #94891, #19876, #73861, #42391, #87874, #26389, #19390, #5389, #56415, #87392, #18910, #79887, #71892, #27865, #95896, #3415, #72870, #43361, #42881, #94398, #72379, #95385, #96391, #4404, #50369, #18411, #11394, #41916, #65366, #48894, #79407, #80877, #41431, #58350, #57868, #88872, #73364, #4892, #35372, #50872, #81364, #12863, #33876, #5870, #75838, #52347, #97375, #45338, #60827, #43848, #51363, #44345, #22361, #7358, #90834, #37364, #67857, #37860, #81850, #21365, #20872, #74851, #13363, #89361, #52835, #60340, #66857, #51860, #83344, #85189, #68352, #91328, #97879, #98870, #28843, #74342, #30325, #14866, #6352, #9187, #82844, #6853, #24203, #59346, #36861, #29339, #82345, #54670, #16696, #36361, #89849, #59840, #58855, #96891, #21869, #67353, #98376, #14364, #13866, #47169, #77674, #44834, #90330, #75338, #29832, #66353, #28367, #9682, #70685, #63157, #17200, #72138, #41180, #47677, #25680, #87632, #87139, #19146, #17686, #48158, #11149, #48652, #33636, #32165, #40178, #2204, #32665, #80134, #39702, #56653, #49623, #63646, #40675, #33152, #94650, #26640, #95129, #70189, #1706, #71175, #55164, #26158, #2701, #94154, #78672, #3665, #93665, #10181, #85679, #10666, #56173, #62666, #55677, #25199, #86176, #86666, #93167, #18170, #24692, #78171, #79152, #71661, #41670 ),
 ( #3171, #64132, #18662, #49150, #79651, #34128, #64620, #57136, #12620, #5134, #66617, #97634, #67109, #59601, #11643, #43122, #27125, #97144, #73610, #35625, #20124, #44095, #35115, #50628, #57627, #81608, #66110, #42156, #27623, #73112, #4654, #80636, #52110, #58108, #90097, #36111, #88124, #13615, #81119, #74606, #58616, #12133, #59102, #65614, #28615, #96639, #28116, #50129, #21124, #89117, #42635, #89611, #6119, #19636, #95639, #88617, #51623, #82103, #36625, #13117, #43613, #29099, #96140, #20628, #65120, #51117, #74100, #34622, #21625, #5633, #72621, #4155, #8097, #1100, #23605, #8583, #15115, #16085, #83098, #6606, #54071, #76577, #22612, #24088, #68600, #23108, #625, #45091, #91085, #45591, #37613, #84586, #39089, #52595, #98123, #76089, #75099, #14120, #38111, #53089, #15609, #128, #14626, #38593, #62058, #30577, #7619, #75597, #61082, #92562, #44604, #7109, #68107, #98632, #60086, #37119, #61569, #83601, #91592, #53580, #84093, #31071, #46093, #46572, #30083, #67615, #77071, #92080, #69091, #69580, #31563, #60590, #82602, #29584, #90588, #22115, #25082, #41562, #2587, #41061, #10065, #40065, #40564, #9564, #71062, #93054, #25568, #47563, #48538, #33042, #48041, #79037, #17575, #78553, #62549, #63537, #56060, #86064, #94047, #86554, #18058, #71558, #95019, #33526, #85073, #10550, #3070, #64021, #55565, #94533, #70566, #26052, #56541, #24587, #87035, #18545, #2092, #32551, #49037, #63052, #79541, #34016, #78061, #93549, #55050, #11041, #72029, #85569, #3556, #64513, #54556, #16582, #47058, #77556, #9072, #17083, #39585, #70076, #1596, #32047, #28004, #87525, #81995, #34509, #19039, #26527, #89502, #57024, #4047, #96529, #35507, #43497, #65002, #88015, #19527, #81012, #28506, #13506, #12025, #96027, #50515, #43015, #43988, #49515, #66505, #74490, #66999, #35002, #12513, #97030, #50024, #21013, #73996, #51501, #6014, #80024, #59000, #95529, #20517, #42049, #36506, #57519, #11528, #20014, #58500, #72513, #27019, #80526, #42524, #73008, #4540, #65505, #27509, #89010, #66001, #5522, #58003, #88512, #73497, #5023, #51002, #81497, #13002, #36002, #22499, #15003, #53964, #97521, #38483, #84472, #38972, #6996, #52970, #68977, #90473, #61455, #15498, #23493, #91964, #28983, #511, #37000, #91471, #14008, #46461, #29471, #30957, #59489, #76469, #37501, #45473, #90965, #67993, #45980, #75976, #15971, #22007, #89989, #76955, #7984, #60476, #7504, #8465, #67496, #21505, #98518, #52003, #82492, #29971, #44489, #37995, #83973, #83482, #82989, #68487, #52481, #14, #98017, #30462, #14507, #22996, #60963, #53463, #74989, #6492 ) ),
 .UNSPECIFIED., .F., .F., .F. ) 
 B_SPLINE_SURFACE_WITH_KNOTS ( ( 2, 2 ),
 ( 3, 2, 2, 2, 2, 2, 2, 2, 2, 2, 2, 2, 2, 2, 2, 2, 2, 2, 2, 2, 2, 2, 2, 2, 2, 2, 2, 2, 2, 2, 2, 2, 2, 2, 2, 2, 2, 2, 2, 2, 2, 2, 2, 2, 2, 2, 2, 2, 2, 2, 2, 2, 2, 2, 2, 2, 2, 2, 2, 2, 2, 2, 2, 2, 2, 2, 2, 2, 2, 2, 2, 2, 2, 2, 2, 2, 2, 2, 2, 2, 2, 2, 2, 2, 2, 2, 2, 2, 2, 2, 2, 2, 2, 2, 2, 2, 2, 2, 2, 2, 2, 2, 2, 2, 2, 2, 2, 2, 2, 2, 2, 2, 2, 2, 2, 2, 2, 2, 2, 2, 2, 2, 2, 2, 2, 2, 2, 2, 2, 2, 2, 2, 2, 2, 2, 2, 2, 2, 2, 2, 2, 2, 2, 2, 2, 2, 2, 2, 2, 2, 2, 2, 2, 2, 2, 2, 2, 2, 2, 2, 2, 2, 3 ),
 ( 0.000000000000000000, 1.000000000000000000 ),
 ( 0.000000000000000000, 0.005952380952380952051, 0.01190476190476190410, 0.01785714285714285615, 0.02380952380952380820, 0.02976190476190476025, 0.03571428571428571230, 0.04166666666666666435, 0.04761904761904761640, 0.05357142857142856845, 0.05952380952380952051, 0.06547619047619047949, 0.07142857142857142461, 0.07738095238095238360, 0.08333333333333332871, 0.08928571428571428770, 0.09523809523809523281, 0.1011904761904761918, 0.1071428571428571369, 0.1130952380952380959, 0.1190476190476190410, 0.1250000000000000000, 0.1309523809523809590, 0.1369047619047619180, 0.1428571428571428492, 0.1488095238095238082, 0.1547619047619047672, 0.1607142857142857262, 0.1666666666666666574, 0.1726190476190476164, 0.1785714285714285754, 0.1845238095238095344, 0.1904761904761904656, 0.1964285714285714246, 0.2023809523809523836, 0.2083333333333333426, 0.2142857142857142738, 0.2202380952380952328, 0.2261904761904761918, 0.2321428571428571508, 0.2380952380952380820, 0.2440476190476190410, 0.2500000000000000000, 0.2559523809523809312, 0.2619047619047619180, 0.2678571428571428492, 0.2738095238095238360, 0.2797619047619047672, 0.2857142857142856984, 0.2916666666666666852, 0.2976190476190476164, 0.3035714285714285476, 0.3095238095238095344, 0.3154761904761904656, 0.3214285714285714524, 0.3273809523809523836, 0.3333333333333333148, 0.3392857142857143016, 0.3452380952380952328, 0.3511904761904761640, 0.3571428571428571508, 0.3630952380952380820, 0.3690476190476190688, 0.3750000000000000000, 0.3809523809523809312, 0.3869047619047619180, 0.3928571428571428492, 0.3988095238095238360, 0.4047619047619047672, 0.4107142857142856984, 0.4166666666666666852, 0.4226190476190476164, 0.4285714285714285476, 0.4345238095238095344, 0.4404761904761904656, 0.4464285714285714524, 0.4523809523809523836, 0.4583333333333333148, 0.4642857142857143016, 0.4702380952380952328, 0.4761904761904761640, 0.4821428571428571508, 0.4880952380952380820, 0.4940476190476190688, 0.5000000000000000000, 0.5059523809523809312, 0.5119047619047618625, 0.5178571428571429047, 0.5238095238095238360, 0.5297619047619047672, 0.5357142857142856984, 0.5416666666666666297, 0.5476190476190476719, 0.5535714285714286031, 0.5595238095238095344, 0.5654761904761904656, 0.5714285714285713969, 0.5773809523809523281, 0.5833333333333333703, 0.5892857142857143016, 0.5952380952380952328, 0.6011904761904761640, 0.6071428571428570953, 0.6130952380952381375, 0.6190476190476190688, 0.6250000000000000000, 0.6309523809523809312, 0.6369047619047618625, 0.6428571428571429047, 0.6488095238095238360, 0.6547619047619047672, 0.6607142857142856984, 0.6666666666666666297, 0.6726190476190476719, 0.6785714285714286031, 0.6845238095238095344, 0.6904761904761904656, 0.6964285714285713969, 0.7023809523809523281, 0.7083333333333333703, 0.7142857142857143016, 0.7202380952380952328, 0.7261904761904761640, 0.7321428571428570953, 0.7380952380952381375, 0.7440476190476190688, 0.7500000000000000000, 0.7559523809523809312, 0.7619047619047618625, 0.7678571428571429047, 0.7738095238095238360, 0.7797619047619047672, 0.7857142857142856984, 0.7916666666666666297, 0.7976190476190476719, 0.8035714285714286031, 0.8095238095238095344, 0.8154761904761904656, 0.8214285714285713969, 0.8273809523809523281, 0.8333333333333333703, 0.8392857142857143016, 0.8452380952380952328, 0.8511904761904761640, 0.8571428571428570953, 0.8630952380952381375, 0.8690476190476190688, 0.8750000000000000000, 0.8809523809523809312, 0.8869047619047618625, 0.8928571428571429047, 0.8988095238095238360, 0.9047619047619047672, 0.9107142857142856984, 0.9166666666666666297, 0.9226190476190476719, 0.9285714285714286031, 0.9345238095238095344, 0.9404761904761904656, 0.9464285714285713969, 0.9523809523809523281, 0.9583333333333333703, 0.9642857142857143016 ),
 .UNSPECIFIED. ) 
 GEOMETRIC_REPRESENTATION_ITEM ( )  RATIONAL_B_SPLINE_SURFACE ( (
 ( 1.000000000000000000, 0.9659258262890683122, 1.000000000000000000, 0.9659258262890683122, 1.000000000000000000, 0.9659258262890683122, 1.000000000000000000, 0.9659258262890683122, 1.000000000000000000, 0.9659258262890683122, 1.000000000000000000, 0.9659258262890683122, 1.000000000000000000, 0.9659258262890683122, 1.000000000000000000, 0.9659258262890683122, 1.000000000000000000, 0.9659258262890683122, 1.000000000000000000, 0.9659258262890683122, 1.000000000000000000, 0.9659258262890683122, 1.000000000000000000, 0.9659258262890683122, 1.000000000000000000, 0.9659258262890683122, 1.000000000000000000, 0.9659258262890683122, 1.000000000000000000, 0.9659258262890683122, 1.000000000000000000, 0.9659258262890683122, 1.000000000000000000, 0.9659258262890683122, 1.000000000000000000, 0.9659258262890683122, 1.000000000000000000, 0.9659258262890683122, 1.000000000000000000, 0.9659258262890683122, 1.000000000000000000, 0.9659258262890683122, 1.000000000000000000, 0.9659258262890683122, 1.000000000000000000, 0.9659258262890683122, 1.000000000000000000, 0.9659258262890683122, 1.000000000000000000, 0.9659258262890683122, 1.000000000000000000, 0.9659258262890683122, 1.000000000000000000, 0.9659258262890683122, 1.000000000000000000, 0.9659258262890683122, 1.000000000000000000, 0.9659258262890683122, 1.000000000000000000, 0.9659258262890683122, 1.000000000000000000, 0.9659258262890683122, 1.000000000000000000, 0.9659258262890683122, 1.000000000000000000, 0.9659258262890683122, 1.000000000000000000, 0.9659258262890683122, 1.000000000000000000, 0.9659258262890683122, 1.000000000000000000, 0.9659258262890683122, 1.000000000000000000, 0.9659258262890683122, 1.000000000000000000, 0.9659258262890683122, 1.000000000000000000, 0.9659258262890683122, 1.000000000000000000, 0.9659258262890683122, 1.000000000000000000, 0.9659258262890683122, 1.000000000000000000, 0.9659258262890683122, 1.000000000000000000, 0.9659258262890683122, 1.000000000000000000, 0.9659258262890683122, 1.000000000000000000, 0.9659258262890683122, 1.000000000000000000, 0.9659258262890683122, 1.000000000000000000, 0.9659258262890683122, 1.000000000000000000, 0.9659258262890683122, 1.000000000000000000, 0.9659258262890683122, 1.000000000000000000, 0.9659258262890683122, 1.000000000000000000, 0.9659258262890683122, 1.000000000000000000, 0.9659258262890683122, 1.000000000000000000, 0.9659258262890683122, 1.000000000000000000, 0.9659258262890683122, 1.000000000000000000, 0.9659258262890683122, 1.000000000000000000, 0.9659258262890683122, 1.000000000000000000, 0.9659258262890683122, 1.000000000000000000, 0.9659258262890683122, 1.000000000000000000, 0.9659258262890683122, 1.000000000000000000, 0.9659258262890683122, 1.000000000000000000, 0.9659258262890683122, 1.000000000000000000, 0.9659258262890683122, 1.000000000000000000, 0.9659258262890683122, 1.000000000000000000, 0.9659258262890683122, 1.000000000000000000, 0.9659258262890683122, 1.000000000000000000, 0.9659258262890683122, 1.000000000000000000, 0.9659258262890683122, 1.000000000000000000, 0.9659258262890683122, 1.000000000000000000, 0.9659258262890683122, 1.000000000000000000, 0.9659258262890683122, 1.000000000000000000, 0.9659258262890683122, 1.000000000000000000, 0.9659258262890683122, 1.000000000000000000, 0.9659258262890683122, 1.000000000000000000, 0.9659258262890683122, 1.000000000000000000, 0.9659258262890683122, 1.000000000000000000, 0.9659258262890683122, 1.000000000000000000, 0.9659258262890683122, 1.000000000000000000, 0.9659258262890683122, 1.000000000000000000, 0.9659258262890683122, 1.000000000000000000, 0.9659258262890683122, 1.000000000000000000, 0.9659258262890683122, 1.000000000000000000, 0.9659258262890683122, 1.000000000000000000, 0.9659258262890683122, 1.000000000000000000, 0.9659258262890683122, 1.000000000000000000, 0.9659258262890683122, 1.000000000000000000, 0.9659258262890683122, 1.000000000000000000, 0.9659258262890683122, 1.000000000000000000, 0.9659258262890683122, 1.000000000000000000, 0.9659258262890683122, 1.000000000000000000, 0.9659258262890683122, 1.000000000000000000, 0.9659258262890683122, 1.000000000000000000, 0.9659258262890683122, 1.000000000000000000, 0.9659258262890683122, 1.000000000000000000, 0.9659258262890683122, 1.000000000000000000, 0.9659258262890683122, 1.000000000000000000, 0.9659258262890683122, 1.000000000000000000, 0.9659258262890683122, 1.000000000000000000, 0.9659258262890683122, 1.000000000000000000, 0.9659258262890683122, 1.000000000000000000, 0.9659258262890683122, 1.000000000000000000, 0.9659258262890683122, 1.000000000000000000, 0.9659258262890683122, 1.000000000000000000, 0.9659258262890683122, 1.000000000000000000, 0.9659258262890683122, 1.000000000000000000, 0.9659258262890683122, 1.000000000000000000, 0.9659258262890683122, 1.000000000000000000, 0.9659258262890683122, 1.000000000000000000, 0.9659258262890683122, 1.000000000000000000, 0.9659258262890683122, 1.000000000000000000, 0.9659258262890683122, 1.000000000000000000, 0.9659258262890683122, 1.000000000000000000, 0.9659258262890683122, 1.000000000000000000, 0.9659258262890683122, 1.000000000000000000, 0.9659258262890683122, 1.000000000000000000, 0.9659258262890683122, 1.000000000000000000, 0.9659258262890683122, 1.000000000000000000, 0.9659258262890683122, 1.000000000000000000, 0.9659258262890683122, 1.000000000000000000, 0.9659258262890683122, 1.000000000000000000, 0.9659258262890683122, 1.000000000000000000, 0.9659258262890683122, 1.000000000000000000, 0.9659258262890683122, 1.000000000000000000, 0.9659258262890683122, 1.000000000000000000, 0.9659258262890683122, 1.000000000000000000, 0.9659258262890683122, 1.000000000000000000, 0.9659258262890683122, 1.000000000000000000, 0.9659258262890683122, 1.000000000000000000, 0.9659258262890683122, 1.000000000000000000, 0.9659258262890683122, 1.000000000000000000, 0.9659258262890683122, 1.000000000000000000, 0.9659258262890683122, 1.000000000000000000, 0.9659258262890683122, 1.000000000000000000, 0.9659258262890683122, 1.000000000000000000, 0.9659258262890683122, 1.000000000000000000, 0.9659258262890683122, 1.000000000000000000, 0.9659258262890683122, 1.000000000000000000, 0.9659258262890683122, 1.000000000000000000, 0.9659258262890683122, 1.000000000000000000, 0.9659258262890683122, 1.000000000000000000, 0.9659258262890683122, 1.000000000000000000, 0.9659258262890683122, 1.000000000000000000, 0.9659258262890683122, 1.000000000000000000, 0.9659258262890683122, 1.000000000000000000, 0.9659258262890683122, 1.000000000000000000, 0.9659258262890683122, 1.000000000000000000, 0.9659258262890683122, 1.000000000000000000, 0.9659258262890683122, 1.000000000000000000, 0.9659258262890683122, 1.000000000000000000, 0.9659258262890683122, 1.000000000000000000, 0.9659258262890683122, 1.000000000000000000, 0.9659258262890683122, 1.000000000000000000, 0.9659258262890683122, 1.000000000000000000, 0.9659258262890683122, 1.000000000000000000, 0.9659258262890683122, 1.000000000000000000, 0.9659258262890683122, 1.000000000000000000, 0.9659258262890683122, 1.000000000000000000, 0.9659258262890683122, 1.000000000000000000, 0.9659258262890683122, 1.000000000000000000, 0.9659258262890683122, 1.000000000000000000, 0.9659258262890683122, 1.000000000000000000, 0.9659258262890683122, 1.000000000000000000, 0.9659258262890683122, 1.000000000000000000),
 ( 1.000000000000000000, 0.9659258262890683122, 1.000000000000000000, 0.9659258262890683122, 1.000000000000000000, 0.9659258262890683122, 1.000000000000000000, 0.9659258262890683122, 1.000000000000000000, 0.9659258262890683122, 1.000000000000000000, 0.9659258262890683122, 1.000000000000000000, 0.9659258262890683122, 1.000000000000000000, 0.9659258262890683122, 1.000000000000000000, 0.9659258262890683122, 1.000000000000000000, 0.9659258262890683122, 1.000000000000000000, 0.9659258262890683122, 1.000000000000000000, 0.9659258262890683122, 1.000000000000000000, 0.9659258262890683122, 1.000000000000000000, 0.9659258262890683122, 1.000000000000000000, 0.9659258262890683122, 1.000000000000000000, 0.9659258262890683122, 1.000000000000000000, 0.9659258262890683122, 1.000000000000000000, 0.9659258262890683122, 1.000000000000000000, 0.9659258262890683122, 1.000000000000000000, 0.9659258262890683122, 1.000000000000000000, 0.9659258262890683122, 1.000000000000000000, 0.9659258262890683122, 1.000000000000000000, 0.9659258262890683122, 1.000000000000000000, 0.9659258262890683122, 1.000000000000000000, 0.9659258262890683122, 1.000000000000000000, 0.9659258262890683122, 1.000000000000000000, 0.9659258262890683122, 1.000000000000000000, 0.9659258262890683122, 1.000000000000000000, 0.9659258262890683122, 1.000000000000000000, 0.9659258262890683122, 1.000000000000000000, 0.9659258262890683122, 1.000000000000000000, 0.9659258262890683122, 1.000000000000000000, 0.9659258262890683122, 1.000000000000000000, 0.9659258262890683122, 1.000000000000000000, 0.9659258262890683122, 1.000000000000000000, 0.9659258262890683122, 1.000000000000000000, 0.9659258262890683122, 1.000000000000000000, 0.9659258262890683122, 1.000000000000000000, 0.9659258262890683122, 1.000000000000000000, 0.9659258262890683122, 1.000000000000000000, 0.9659258262890683122, 1.000000000000000000, 0.9659258262890683122, 1.000000000000000000, 0.9659258262890683122, 1.000000000000000000, 0.9659258262890683122, 1.000000000000000000, 0.9659258262890683122, 1.000000000000000000, 0.9659258262890683122, 1.000000000000000000, 0.9659258262890683122, 1.000000000000000000, 0.9659258262890683122, 1.000000000000000000, 0.9659258262890683122, 1.000000000000000000, 0.9659258262890683122, 1.000000000000000000, 0.9659258262890683122, 1.000000000000000000, 0.9659258262890683122, 1.000000000000000000, 0.9659258262890683122, 1.000000000000000000, 0.9659258262890683122, 1.000000000000000000, 0.9659258262890683122, 1.000000000000000000, 0.9659258262890683122, 1.000000000000000000, 0.9659258262890683122, 1.000000000000000000, 0.9659258262890683122, 1.000000000000000000, 0.9659258262890683122, 1.000000000000000000, 0.9659258262890683122, 1.000000000000000000, 0.9659258262890683122, 1.000000000000000000, 0.9659258262890683122, 1.000000000000000000, 0.9659258262890683122, 1.000000000000000000, 0.9659258262890683122, 1.000000000000000000, 0.9659258262890683122, 1.000000000000000000, 0.9659258262890683122, 1.000000000000000000, 0.9659258262890683122, 1.000000000000000000, 0.9659258262890683122, 1.000000000000000000, 0.9659258262890683122, 1.000000000000000000, 0.9659258262890683122, 1.000000000000000000, 0.9659258262890683122, 1.000000000000000000, 0.9659258262890683122, 1.000000000000000000, 0.9659258262890683122, 1.000000000000000000, 0.9659258262890683122, 1.000000000000000000, 0.9659258262890683122, 1.000000000000000000, 0.9659258262890683122, 1.000000000000000000, 0.9659258262890683122, 1.000000000000000000, 0.9659258262890683122, 1.000000000000000000, 0.9659258262890683122, 1.000000000000000000, 0.9659258262890683122, 1.000000000000000000, 0.9659258262890683122, 1.000000000000000000, 0.9659258262890683122, 1.000000000000000000, 0.9659258262890683122, 1.000000000000000000, 0.9659258262890683122, 1.000000000000000000, 0.9659258262890683122, 1.000000000000000000, 0.9659258262890683122, 1.000000000000000000, 0.9659258262890683122, 1.000000000000000000, 0.9659258262890683122, 1.000000000000000000, 0.9659258262890683122, 1.000000000000000000, 0.9659258262890683122, 1.000000000000000000, 0.9659258262890683122, 1.000000000000000000, 0.9659258262890683122, 1.000000000000000000, 0.9659258262890683122, 1.000000000000000000, 0.9659258262890683122, 1.000000000000000000, 0.9659258262890683122, 1.000000000000000000, 0.9659258262890683122, 1.000000000000000000, 0.9659258262890683122, 1.000000000000000000, 0.9659258262890683122, 1.000000000000000000, 0.9659258262890683122, 1.000000000000000000, 0.9659258262890683122, 1.000000000000000000, 0.9659258262890683122, 1.000000000000000000, 0.9659258262890683122, 1.000000000000000000, 0.9659258262890683122, 1.000000000000000000, 0.9659258262890683122, 1.000000000000000000, 0.9659258262890683122, 1.000000000000000000, 0.9659258262890683122, 1.000000000000000000, 0.9659258262890683122, 1.000000000000000000, 0.9659258262890683122, 1.000000000000000000, 0.9659258262890683122, 1.000000000000000000, 0.9659258262890683122, 1.000000000000000000, 0.9659258262890683122, 1.000000000000000000, 0.9659258262890683122, 1.000000000000000000, 0.9659258262890683122, 1.000000000000000000, 0.9659258262890683122, 1.000000000000000000, 0.9659258262890683122, 1.000000000000000000, 0.9659258262890683122, 1.000000000000000000, 0.9659258262890683122, 1.000000000000000000, 0.9659258262890683122, 1.000000000000000000, 0.9659258262890683122, 1.000000000000000000, 0.9659258262890683122, 1.000000000000000000, 0.9659258262890683122, 1.000000000000000000, 0.9659258262890683122, 1.000000000000000000, 0.9659258262890683122, 1.000000000000000000, 0.9659258262890683122, 1.000000000000000000, 0.9659258262890683122, 1.000000000000000000, 0.9659258262890683122, 1.000000000000000000, 0.9659258262890683122, 1.000000000000000000, 0.9659258262890683122, 1.000000000000000000, 0.9659258262890683122, 1.000000000000000000, 0.9659258262890683122, 1.000000000000000000, 0.9659258262890683122, 1.000000000000000000, 0.9659258262890683122, 1.000000000000000000, 0.9659258262890683122, 1.000000000000000000, 0.9659258262890683122, 1.000000000000000000, 0.9659258262890683122, 1.000000000000000000, 0.9659258262890683122, 1.000000000000000000, 0.9659258262890683122, 1.000000000000000000, 0.9659258262890683122, 1.000000000000000000, 0.9659258262890683122, 1.000000000000000000, 0.9659258262890683122, 1.000000000000000000, 0.9659258262890683122, 1.000000000000000000, 0.9659258262890683122, 1.000000000000000000, 0.9659258262890683122, 1.000000000000000000, 0.9659258262890683122, 1.000000000000000000, 0.9659258262890683122, 1.000000000000000000, 0.9659258262890683122, 1.000000000000000000, 0.9659258262890683122, 1.000000000000000000, 0.9659258262890683122, 1.000000000000000000, 0.9659258262890683122, 1.000000000000000000, 0.9659258262890683122, 1.000000000000000000, 0.9659258262890683122, 1.000000000000000000, 0.9659258262890683122, 1.000000000000000000, 0.9659258262890683122, 1.000000000000000000, 0.9659258262890683122, 1.000000000000000000, 0.9659258262890683122, 1.000000000000000000, 0.9659258262890683122, 1.000000000000000000, 0.9659258262890683122, 1.000000000000000000, 0.9659258262890683122, 1.000000000000000000, 0.9659258262890683122, 1.000000000000000000, 0.9659258262890683122, 1.000000000000000000, 0.9659258262890683122, 1.000000000000000000, 0.9659258262890683122, 1.000000000000000000) ) ) 
 REPRESENTATION_ITEM ( '' )  SURFACE ( )  );
#53434 = DIRECTION ( 'NONE',  ( 0.000000000000000000, 0.000000000000000000, -1.000000000000000000 ) ) ;
#53435 = CARTESIAN_POINT ( 'NONE',  ( 10.00000000000000178, 10.37363466993041961, 12.81628187352647608 ) ) ;
#53436 = VECTOR ( 'NONE', #27883, 1000.000000000000000 ) ;
#53437 = CARTESIAN_POINT ( 'NONE',  ( 2.035157376598824452, 48.68868534415483396, 7.964842623401179544 ) ) ;
#53438 = CARTESIAN_POINT ( 'NONE',  ( -4.164238869374099927, 37.01208216824731068, 3.795296366450308767 ) ) ;
#53439 = DIRECTION ( 'NONE',  ( 1.257568779154408793E-17, 1.000000000000000000, -0.000000000000000000 ) ) ;
#53440 = CARTESIAN_POINT ( 'NONE',  ( 20.36894250292379738, 29.92874883491396432, -10.36894250292379027 ) ) ;
#53441 = CARTESIAN_POINT ( 'NONE',  ( 17.08211943468705130, 58.47041550158063927, 12.26659068614894998 ) ) ;
#53442 = CARTESIAN_POINT ( 'NONE',  ( 10.00000000000000000, 5.553748834913967869, -14.16423886937410082 ) ) ;
#53444 = CARTESIAN_POINT ( 'NONE',  ( 19.84674366389459266, 33.30059781766745175, 2.638427012816836559 ) ) ;
#53443 = CARTESIAN_POINT ( 'NONE',  ( 17.08211943468705840, 20.13708216824730357, -12.26659068614894466 ) ) ;
#53445 = CARTESIAN_POINT ( 'NONE',  ( 20.88017736071110164, 45.35535201082149115, 2.915334737309930979 ) ) ;
#53446 = CARTESIAN_POINT ( 'NONE',  ( 4.380000000000000782, 1.019547802438464545, -3.750000000000000888 ) ) ;
#53448 = CARTESIAN_POINT ( 'NONE',  ( 18.52753015748618282, 48.92559781766745886, -4.923371831947291888 ) ) ;
#53447 = DIRECTION ( 'NONE',  ( 0.000000000000000000, 0.000000000000000000, 1.000000000000000000 ) ) ;
#53449 = CARTESIAN_POINT ( 'NONE',  ( 12.91533473730992121, 24.52201867748816966, 10.88017736071110164 ) ) ;
#53450 = CARTESIAN_POINT ( 'NONE',  ( 21.92686044187657046, 55.16212336850780673, 4.562052436263912550E-16 ) ) ;
#53451 = CARTESIAN_POINT ( 'NONE',  ( 14.92337183194729633, 57.67559781766745886, 8.527530157486181039 ) ) ;
#53452 = CARTESIAN_POINT ( 'NONE',  ( 0.000000000000000000, 0.000000000000000000, 0.000000000000000000 ) ) ;
#53453 = ADVANCED_FACE ( 'NONE', ( #41790 ), #35744, .F. ) ;
#53454 = CARTESIAN_POINT ( 'NONE',  ( 18.52753015748617571, 33.09226448433411605, 4.923371831947298993 ) ) ;
#53455 = CARTESIAN_POINT ( 'NONE',  ( 19.38216949554541202, 50.99863466993042493, 9.382169495545424454 ) ) ;
#53456 = CARTESIAN_POINT ( 'NONE',  ( -12.26659068614894110, -7.779584498419360727, 7.082119434687058401 ) ) ;
#53457 = CARTESIAN_POINT ( 'NONE',  ( 19.84674366389459621, 43.50893115100078745, 7.409399052514197653E-17 ) ) ;
#53458 = CARTESIAN_POINT ( 'NONE',  ( 0.1532563361054083140, 51.00893115100078745, 1.131784320476157264E-15 ) ) ;
#53459 = CARTESIAN_POINT ( 'NONE',  ( 20.36894250292379382, 43.67874883491397497, 10.36894250292379205 ) ) ;
#53460 = ORIENTED_EDGE ( 'NONE', *, *, #64756, .F. ) ;
#53461 = CARTESIAN_POINT ( 'NONE',  ( 17.08211943468705130, 13.47041550158063572, 12.26659068614894998 ) ) ;
#53462 = B_SPLINE_CURVE_WITH_KNOTS ( 'NONE', 3,
 ( #23122, #14133, #82117, #91605, #68612, #52610, #68121, #76592, #59615, #31086 ),
 .UNSPECIFIED., .F., .F.,
 ( 4, 3, 3, 4 ),
 ( 2.368389951639683899E-16, 0.0006253016069560743580, 0.001250604074564920856, 0.002501455912506532226 ),
 .UNSPECIFIED. ) ;
#53463 = CARTESIAN_POINT ( 'NONE',  ( 4.559911319644449179, 68.89701867748817676, 9.422509992056141925 ) ) ;
#53464 = CARTESIAN_POINT ( 'NONE',  ( 0.6289242262155387841, 20.99999999999999289, 0.000000000000000000 ) ) ;
#53465 = CARTESIAN_POINT ( 'NONE',  ( 10.00000000000000000, 60.55374883491397497, -14.16423886937410082 ) ) ;
#53466 = CARTESIAN_POINT ( 'NONE',  ( 13.43411237798105340, 10.58196800326375353, 12.81628187352647963 ) ) ;
#53467 = CARTESIAN_POINT ( 'NONE',  ( 18.17884179759845509, 43.66688879859522388, -6.500000000000054179 ) ) ;
#53468 = CARTESIAN_POINT ( 'NONE',  ( -0.8801773607110991993, 67.85535201082151957, -2.915334737309923874 ) ) ;
#53469 = CARTESIAN_POINT ( 'NONE',  ( 1.354709868695521013, 14.63595249122789177, 14.93870011653153540 ) ) ;
#53470 = CARTESIAN_POINT ( 'NONE',  ( -46.94000000000001194, 101.5930487410390270, -7.918115197747374268 ) ) ;
#53471 = CARTESIAN_POINT ( 'NONE',  ( 13.43411237798105340, 30.58196800326374998, 12.81628187352647963 ) ) ;
#53472 = CARTESIAN_POINT ( 'NONE',  ( -0.3689425029237881626, 57.42874883491397497, 10.36894250292379027 ) ) ;
#53473 = CARTESIAN_POINT ( 'NONE',  ( 10.88017736071109987, 25.77201867748818032, -2.915334737309928315 ) ) ;
#53474 = CARTESIAN_POINT ( 'NONE',  ( 4.559911319644449179, 17.23035201082150536, -9.422509992056141925 ) ) ;
#53475 = CARTESIAN_POINT ( 'NONE',  ( 19.42250999205614193, 20.14701867748817321, 5.440088680355555262 ) ) ;
#53476 = CARTESIAN_POINT ( 'NONE',  ( 19.84674366389459621, 58.50893115100078745, 7.409399052514197653E-17 ) ) ;
#53477 = CARTESIAN_POINT ( 'NONE',  ( 0.1532563361054082862, 56.21726448433411605, 2.638427012816831674 ) ) ;
#53478 = CARTESIAN_POINT ( 'NONE',  ( 13.43411237798105340, 50.58196800326375353, 12.81628187352647963 ) ) ;
#53479 = CARTESIAN_POINT ( 'NONE',  ( 1.472469842513823179, 1.425597817667451528, 4.923371831947296329 ) ) ;
#53480 = EDGE_LOOP ( 'NONE', ( #61315, #83283, #34817, #42714 ) ) ;
#53481 = CARTESIAN_POINT ( 'NONE',  ( 15.44008868035555793, 11.39701867748817143, -9.422509992056140149 ) ) ;
#53482 = CARTESIAN_POINT ( 'NONE',  ( 6.565887622018943937, 25.16530133659708213, 12.81628187352647430 ) ) ;
#53483 = CARTESIAN_POINT ( 'NONE',  ( 0.000000000000000000, -97.00000000000000000, 3.750000000000000000 ) ) ;
#53484 = MECHANICAL_DESIGN_GEOMETRIC_PRESENTATION_REPRESENTATION (  '', ( #23104 ), #82176 ) ;
#53485 = CARTESIAN_POINT ( 'NONE',  ( 18.52753015748617571, 43.09226448433412315, 4.923371831947298993 ) ) ;
#53486 = CARTESIAN_POINT ( 'NONE',  ( 17.96484262340118221, 54.93868534415484106, 7.964842623401181321 ) ) ;
#53487 = VECTOR ( 'NONE', #94872, 1000.000000000000000 ) ;
#53488 = CARTESIAN_POINT ( 'NONE',  ( 0.6178305044545818747, 23.49863466993041783, -9.382169495545419124 ) ) ;
#53490 = CARTESIAN_POINT ( 'NONE',  ( -14.99847009497950800, 14.49999999999999112, -0.2142307401082109986 ) ) ;
#53489 = CARTESIAN_POINT ( 'NONE',  ( 2.035157376598822676, 52.43868534415483396, -7.964842623401177768 ) ) ;
#53491 = EDGE_CURVE ( 'NONE', #67824, #78138, #95121, .T. ) ;
#53492 = CARTESIAN_POINT ( 'NONE',  ( 6.579634127946655475, -87.99828267815715321, -3.250000000000000888 ) ) ;
#53493 = CARTESIAN_POINT ( 'NONE',  ( 22.81628187352647785, 56.41530133659708213, 3.434112377981063169 ) ) ;
#53494 = ORIENTED_EDGE ( 'NONE', *, *, #48449, .F. ) ;
#53495 = CARTESIAN_POINT ( 'NONE',  ( 1.472469842513823179, 61.42559781766745175, 4.923371831947296329 ) ) ;
#53496 = DIRECTION ( 'NONE',  ( 0.000000000000000000, -1.000000000000000000, 0.000000000000000000 ) ) ;
#53497 = CARTESIAN_POINT ( 'NONE',  ( -0.8801773607111009756, 53.06368534415484106, 1.068504757029289695E-15 ) ) ;
#53498 = CARTESIAN_POINT ( 'NONE',  ( -1.099225684535947600, 44.54030133659708923, 6.408140936763237150 ) ) ;
#53499 = CARTESIAN_POINT ( 'NONE',  ( 2.791683348922237240, 10.38393115100078390, -7.208316651077763204 ) ) ;
#53500 = CARTESIAN_POINT ( 'NONE',  ( 12.91533473730992121, 54.52201867748816255, 10.88017736071110164 ) ) ;
#53501 = CARTESIAN_POINT ( 'NONE',  ( 7.361572987183170547, 67.05059781766746596, 9.846743663894590881 ) ) ;
#53502 = CARTESIAN_POINT ( 'NONE',  ( 0.1532563361054082862, 21.21726448433412315, 2.638427012816831674 ) ) ;
#53503 = CARTESIAN_POINT ( 'NONE',  ( 17.20831665107776587, 9.133931151000787452, -7.208316651077762316 ) ) ;
#53504 = CARTESIAN_POINT ( 'NONE',  ( 6.000000000000000000, 11.50000000000000000, -5.000000000000000000 ) ) ;
#53505 = CARTESIAN_POINT ( 'NONE',  ( -2.266590686148945544, 41.38708216824729647, -7.082119434687050408 ) ) ;
#53506 = LINE ( 'NONE', #37542, #23442 ) ;
#53507 = EDGE_CURVE ( 'NONE', #21503, #60570, #35242, .T. ) ;
#53508 = CARTESIAN_POINT ( 'NONE',  ( 12.91533473730992121, 9.522018677488171434, 10.88017736071110164 ) ) ;
#53509 = CARTESIAN_POINT ( 'NONE',  ( 8.629999999999995453, 40.99999999999999289, -4.250000000000000000 ) ) ;
#53510 = ORIENTED_EDGE ( 'NONE', *, *, #63145, .F. ) ;
#53511 = CARTESIAN_POINT ( 'NONE',  ( 0.5774900079438607392, 13.48035201082150358, 5.440088680355550821 ) ) ;
#53512 = CARTESIAN_POINT ( 'NONE',  ( 17.96484262340118221, 16.18868534415483396, -7.964842623401177768 ) ) ;
#53513 = CARTESIAN_POINT ( 'NONE',  ( 18.52753015748618282, 48.92559781766745886, -4.923371831947291888 ) ) ;
#53514 = VECTOR ( 'NONE', #45744, 1000.000000000000000 ) ;
#53515 = CARTESIAN_POINT ( 'NONE',  ( 0.6178305044545818747, 33.49863466993042493, -9.382169495545419124 ) ) ;
#53517 = CARTESIAN_POINT ( 'NONE',  ( -0.3689425029237898834, 6.178748834913968757, -10.36894250292378850 ) ) ;
#53516 = CARTESIAN_POINT ( 'NONE',  ( 0.000000000000000000, 2.500000000000005773, 0.000000000000000000 ) ) ;
#53518 = CARTESIAN_POINT ( 'NONE',  ( 17.96484262340118221, 31.18868534415483751, -7.964842623401177768 ) ) ;
#53519 = CARTESIAN_POINT ( 'NONE',  ( 7.084665262690076126, 4.105352010821503583, 10.88017736071109987 ) ) ;
#53520 = EDGE_CURVE ( 'NONE', #65756, #43512, #69596, .T. ) ;
#53521 = CARTESIAN_POINT ( 'NONE',  ( 1.472469842513823179, 46.42559781766745175, 4.923371831947296329 ) ) ;
#53522 = DIRECTION ( 'NONE',  ( -1.000000000000000000, -0.000000000000000000, -0.000000000000000000 ) ) ;
#53523 = CARTESIAN_POINT ( 'NONE',  ( 1.472469842513823179, 20.59226448433411960, -4.923371831947296329 ) ) ;
#53524 = CARTESIAN_POINT ( 'NONE',  ( -7.208316651077756099, 31.63393115100080166, 7.208316651077766757 ) ) ;
#53525 = EDGE_LOOP ( 'NONE', ( #58076, #93254, #45537, #65303, #6778 ) ) ;
#53526 = ORIENTED_EDGE ( 'NONE', *, *, #6400, .F. ) ;
#53527 = CARTESIAN_POINT ( 'NONE',  ( 2.791683348922237240, 60.38393115100078745, -7.208316651077763204 ) ) ;
#53529 = CARTESIAN_POINT ( 'NONE',  ( 20.88017736071110164, 35.35535201082150536, 2.915334737309930979 ) ) ;
#53528 = CARTESIAN_POINT ( 'NONE',  ( 4.559911319644449179, 33.89701867748817676, 9.422509992056141925 ) ) ;
#53531 = CARTESIAN_POINT ( 'NONE',  ( -1.099225684535947600, 28.70696800326375353, -6.408140936763238038 ) ) ;
#53530 = CARTESIAN_POINT ( 'NONE',  ( 10.00000000000000000, 64.75893115100078035, -9.846743663894594434 ) ) ;
#53532 = CARTESIAN_POINT ( 'NONE',  ( 24.16423886937409904, 14.09541550158063217, 3.795296366450317205 ) ) ;
#53533 = COLOUR_RGB ( '', 0.40784314, 0.44705882, 0.49803922) ;
#53534 = EDGE_CURVE ( 'NONE', #2183, #43301, #96731, .T. ) ;
#53535 = CIRCLE ( 'NONE', #2468, 15.00000000000000000 ) ;
#53536 = CARTESIAN_POINT ( 'NONE',  ( 10.00000000000000178, 40.37363466993042493, 12.81628187352647608 ) ) ;
#53537 = ORIENTED_EDGE ( 'NONE', *, *, #19126, .T. ) ;
#53538 = CARTESIAN_POINT ( 'NONE',  ( 14.92337183194729988, 49.34226448433411605, -8.527530157486177487 ) ) ;
#53539 = CARTESIAN_POINT ( 'NONE',  ( 2.035157376598824452, 13.68868534415483751, 7.964842623401179544 ) ) ;
#53540 = ORIENTED_EDGE ( 'NONE', *, *, #33169, .T. ) ;
#53541 = ADVANCED_FACE ( 'NONE', ( #21245 ), #82352, .T. ) ;
#53542 = CARTESIAN_POINT ( 'NONE',  ( 20.88017736071110519, 10.56368534415483929, 2.639326808657452039E-16 ) ) ;
#53543 = ORIENTED_EDGE ( 'NONE', *, *, #68204, .F. ) ;
#53544 = CARTESIAN_POINT ( 'NONE',  ( 15.44008868035555793, 61.39701867748817676, -9.422509992056140149 ) ) ;
#53545 = CARTESIAN_POINT ( 'NONE',  ( 17.96484262340118221, 54.93868534415484106, 7.964842623401181321 ) ) ;
#53546 = CARTESIAN_POINT ( 'NONE',  ( 17.96484262340118221, 61.18868534415482685, -7.964842623401177768 ) ) ;
#53547 = VECTOR ( 'NONE', #64492, 1000.000000000000000 ) ;
#53548 = CARTESIAN_POINT ( 'NONE',  ( 15.44008868035555793, 56.39701867748817676, -9.422509992056140149 ) ) ;
#53549 = CARTESIAN_POINT ( 'NONE',  ( 12.15129255554608534, -0.03417435944610275333, 10.40305174771247998 ) ) ;
#53550 = VECTOR ( 'NONE', #80665, 1000.000000000000114 ) ;
#53552 = ORIENTED_EDGE ( 'NONE', *, *, #36481, .T. ) ;
#53551 = CARTESIAN_POINT ( 'NONE',  ( 10.58840669699852199, -98.14374106289703548, 4.000000000000000000 ) ) ;
#53553 = CARTESIAN_POINT ( 'NONE',  ( 10.00000000000000000, 39.75893115100078745, -9.846743663894594434 ) ) ;
#53554 = ORIENTED_EDGE ( 'NONE', *, *, #32943, .F. ) ;
#53555 = CARTESIAN_POINT ( 'NONE',  ( 20.04068437667225666, 19.71974360917720759, 6.396802510829705746 ) ) ;
#53556 = CIRCLE ( 'NONE', #75909, 15.00000000000000000 ) ;
#53557 = CARTESIAN_POINT ( 'NONE',  ( 0.000000000000000000, 15.00000000000000000, 0.000000000000000000 ) ) ;
#53558 = CARTESIAN_POINT ( 'NONE',  ( 10.00000000000000178, 18.05374883491396787, 14.16423886937410082 ) ) ;
#53559 = ORIENTED_EDGE ( 'NONE', *, *, #16177, .T. ) ;
#53560 = CARTESIAN_POINT ( 'NONE',  ( -0.1023957841222410126, 35.13377557478296609, 6.340343622311920058 ) ) ;
#53562 = CARTESIAN_POINT ( 'NONE',  ( 7.084665262690076126, 64.10535201082150536, 10.88017736071109987 ) ) ;
#53561 = CARTESIAN_POINT ( 'NONE',  ( -8.399999999999998579, 98.49999999999998579, -8.525133428036873795 ) ) ;
#53563 = CARTESIAN_POINT ( 'NONE',  ( 0.5774900079438607392, 13.48035201082150358, 5.440088680355550821 ) ) ;
#53564 = CARTESIAN_POINT ( 'NONE',  ( 0.1129803114748856863, 59.29427333184092674, -6.480634945678684922 ) ) ;
#53566 = ORIENTED_EDGE ( 'NONE', *, *, #1785, .F. ) ;
#53565 = CARTESIAN_POINT ( 'NONE',  ( 16.40814093676323893, 40.79030133659708923, 11.09922568453595026 ) ) ;
#53567 = CYLINDRICAL_SURFACE ( 'NONE', #35257, 11.92686044187656513 ) ;
#53568 = CARTESIAN_POINT ( 'NONE',  ( 14.92337183194729988, 64.34226448433412315, -8.527530157486177487 ) ) ;
#53569 = CARTESIAN_POINT ( 'NONE',  ( 1.472469842513823179, 1.425597817667451528, 4.923371831947296329 ) ) ;
#53570 = CARTESIAN_POINT ( 'NONE',  ( 0.6178305044545818747, 33.49863466993042493, -9.382169495545419124 ) ) ;
#53571 = CARTESIAN_POINT ( 'NONE',  ( 14.92337183194729988, 24.34226448433411960, -8.527530157486177487 ) ) ;
#53572 = CARTESIAN_POINT ( 'NONE',  ( 7.674335239599288983, 14.76930270348881180, -12.81961907869216333 ) ) ;
#53573 = CARTESIAN_POINT ( 'NONE',  ( 6.565887622018943937, 15.16530133659708568, 12.81628187352647430 ) ) ;
#53574 =( NAMED_UNIT ( * ) SI_UNIT ( $, .STERADIAN. ) SOLID_ANGLE_UNIT ( ) );
#53575 = TOROIDAL_SURFACE ( 'NONE', #15287, 14.49999999999999822, 0.5000000000000000000 ) ;
#53576 = CARTESIAN_POINT ( 'NONE',  ( 17.20831665107776587, 12.88393115100078390, 7.208316651077764980 ) ) ;
#53578 = EDGE_LOOP ( 'NONE', ( #56698, #9610, #76390, #95833 ) ) ;
#53577 = B_SPLINE_CURVE_WITH_KNOTS ( 'NONE', 3,
 ( #46597, #53607, #39612, #1626, #23134, #39116 ),
 .UNSPECIFIED., .F., .F.,
 ( 4, 2, 4 ),
 ( 0.0002800111042666518849, 0.0006862164423004496472, 0.001092421780334247410 ),
 .UNSPECIFIED. ) ;
#53579 = ORIENTED_EDGE ( 'NONE', *, *, #47080, .T. ) ;
#53580 = CARTESIAN_POINT ( 'NONE',  ( 12.91533473730993009, 26.60535201082150536, -10.88017736071109987 ) ) ;
#53581 = CARTESIAN_POINT ( 'NONE',  ( 13.79529636645030344, 23.26208216824730002, 14.16423886937410614 ) ) ;
#53582 = CARTESIAN_POINT ( 'NONE',  ( 0.1532563361054083140, 36.00893115100078745, 1.131784320476157264E-15 ) ) ;
#53583 = CARTESIAN_POINT ( 'NONE',  ( 12.91533473730992121, 64.52201867748817676, 10.88017736071110164 ) ) ;
#53585 = CARTESIAN_POINT ( 'NONE',  ( -7.127794346849581686, -80.93619716733994096, -2.750000000000000444 ) ) ;
#53584 = CARTESIAN_POINT ( 'NONE',  ( 16.40814093676323893, 45.79030133659708923, 11.09922568453595026 ) ) ;
#53586 = CARTESIAN_POINT ( 'NONE',  ( 4.559911319644449179, 18.89701867748817321, 9.422509992056141925 ) ) ;
#53587 = DIRECTION ( 'NONE',  ( 0.000000000000000000, 1.000000000000000000, 0.000000000000000000 ) ) ;
#53588 = CARTESIAN_POINT ( 'NONE',  ( 6.565887622018943937, 8.081968003263751754, -12.81628187352647608 ) ) ;
#53589 = CARTESIAN_POINT ( 'NONE',  ( 16.40814093676324603, 12.45696800326375353, -11.09922568453594671 ) ) ;
#53590 = CARTESIAN_POINT ( 'NONE',  ( 0.1532563361054083140, 31.00893115100078390, 1.131784320476157264E-15 ) ) ;
#53591 = CARTESIAN_POINT ( 'NONE',  ( -2.915334737309917656, -5.894647989178490199, 10.88017736071110164 ) ) ;
#53592 = CARTESIAN_POINT ( 'NONE',  ( 6.565887622018943937, 33.08196800326374643, -12.81628187352647608 ) ) ;
#53593 = CARTESIAN_POINT ( 'NONE',  ( 14.49999999999999822, 60.50000000000000711, -6.500000000000000888 ) ) ;
#53595 = CARTESIAN_POINT ( 'NONE',  ( -4.000000000000000000, 10.25000000000000000, 2.750000000000000000 ) ) ;
#53594 = CARTESIAN_POINT ( 'NONE',  ( 0.5774900079438590739, 52.64701867748817676, -5.440088680355550821 ) ) ;
#53596 = VECTOR ( 'NONE', #91205, 1000.000000000000000 ) ;
#53597 = DIRECTION ( 'NONE',  ( 0.4771587602595978028, 0.000000000000000000, 0.8788171126619711560 ) ) ;
#53598 = DIRECTION ( 'NONE',  ( 0.000000000000000000, 0.000000000000000000, 1.000000000000000000 ) ) ;
#53599 = CARTESIAN_POINT ( 'NONE',  ( 10.00000000000000178, 39.31368534415484106, 10.88017736071110342 ) ) ;
#53600 = B_SPLINE_CURVE_WITH_KNOTS ( 'NONE', 3,
 ( #81092, #12593, #32754, #80608, #17289, #43093 ),
 .UNSPECIFIED., .F., .F.,
 ( 4, 2, 4 ),
 ( 0.0002800858945027110639, 0.0006862919646584216167, 0.001092498034814132169 ),
 .UNSPECIFIED. ) ;
#53601 = CARTESIAN_POINT ( 'NONE',  ( 20.88017736071110164, 45.35535201082149115, 2.915334737309930979 ) ) ;
#53602 = CARTESIAN_POINT ( 'NONE',  ( -12.25993886608593364, 15.00000000000000000, -8.642563219313787570 ) ) ;
#53603 = DIRECTION ( 'NONE',  ( -1.000000000000000000, -0.000000000000000000, -0.000000000000000000 ) ) ;
#53604 = CIRCLE ( 'NONE', #36048, 14.49999999999999822 ) ;
#53605 = CARTESIAN_POINT ( 'NONE',  ( 5.076628168052704559, 50.17559781766745886, -8.527530157486179263 ) ) ;
#53607 = CARTESIAN_POINT ( 'NONE',  ( 9.281709892946475193, -3.106493334055145310E-15, -11.30302492080705967 ) ) ;
#53606 = CARTESIAN_POINT ( 'NONE',  ( 15.44008868035555260, 4.730352010821504471, 9.422509992056143702 ) ) ;
#53608 = CARTESIAN_POINT ( 'NONE',  ( -1.099225684535947600, 8.706968003263753531, -6.408140936763238038 ) ) ;
#53609 = VERTEX_POINT ( 'NONE', #49751 ) ;
#53610 = CARTESIAN_POINT ( 'NONE',  ( 15.44008868035555793, 31.39701867748817676, -9.422509992056140149 ) ) ;
#53612 = FILL_AREA_STYLE ('',( #91623 ) ) ;
#53611 = CARTESIAN_POINT ( 'NONE',  ( 17.20831665107776587, 59.13393115100078745, -7.208316651077762316 ) ) ;
#53613 = CARTESIAN_POINT ( 'NONE',  ( 4.559911319644449179, 8.897018677488171434, 9.422509992056141925 ) ) ;
#53614 = CARTESIAN_POINT ( 'NONE',  ( 12.91533473730993009, 31.60535201082150891, -10.88017736071109987 ) ) ;
#53615 = CARTESIAN_POINT ( 'NONE',  ( -4.164238869374099039, 41.80374883491397497, 8.674139862899312516E-16 ) ) ;
#53616 = CARTESIAN_POINT ( 'NONE',  ( 0.1532563361054083140, 31.00893115100078390, 1.131784320476157264E-15 ) ) ;
#53617 = CARTESIAN_POINT ( 'NONE',  ( -0.8801773607110991993, 42.85535201082150536, -2.915334737309923874 ) ) ;
#53618 = CARTESIAN_POINT ( 'NONE',  ( 0.7375392941517004974, 14.49999999999999112, 14.98185688723477682 ) ) ;
#53619 = CARTESIAN_POINT ( 'NONE',  ( 6.204703633549690345, 5.762082168247301794, -14.16423886937410259 ) ) ;
#53620 = EDGE_CURVE ( 'NONE', #28166, #49358, #93507, .T. ) ;
#53621 = STYLED_ITEM ( 'NONE', ( #57621 ), #37372 ) ;
#53622 = CARTESIAN_POINT ( 'NONE',  ( 7.361572987183169658, 54.96726448433413026, -9.846743663894592657 ) ) ;
#53623 =( GEOMETRIC_REPRESENTATION_CONTEXT ( 3 ) GLOBAL_UNCERTAINTY_ASSIGNED_CONTEXT ( ( #70221 ) ) GLOBAL_UNIT_ASSIGNED_CONTEXT ( ( #39650, #63113, #55627 ) ) REPRESENTATION_CONTEXT ( 'NONE', 'WORKASPACE' ) );
#53625 = ORIENTED_EDGE ( 'NONE', *, *, #25776, .T. ) ;
#53624 = EDGE_CURVE ( 'NONE', #55108, #11363, #50757, .T. ) ;
#53626 = ORIENTED_EDGE ( 'NONE', *, *, #56040, .F. ) ;
#53627 = CIRCLE ( 'NONE', #10519, 100.0000000000000000 ) ;
#53628 = CARTESIAN_POINT ( 'NONE',  ( 20.36894250292379382, 33.67874883491396076, 10.36894250292379205 ) ) ;
#53629 = CARTESIAN_POINT ( 'NONE',  ( 6.204703633549690345, 17.84541550158063217, 14.16423886937410082 ) ) ;
#53630 = CARTESIAN_POINT ( 'NONE',  ( 0.1532563361054083140, 6.008931151000784787, 1.131784320476157264E-15 ) ) ;
#53631 = CARTESIAN_POINT ( 'NONE',  ( -1.099225684535947600, 9.540301336597087456, 6.408140936763237150 ) ) ;
#53632 = DIRECTION ( 'NONE',  ( 0.09584575252022037306, -0.000000000000000000, 0.9953961983671790748 ) ) ;
#53633 = CARTESIAN_POINT ( 'NONE',  ( -8.957287532613966263, -19.72663685366264019, 4.000000000000000000 ) ) ;
#53635 = CARTESIAN_POINT ( 'NONE',  ( -2.816281873526473856, 19.12363466993042138, 9.499525473075851096E-16 ) ) ;
#53634 = CARTESIAN_POINT ( 'NONE',  ( 7.084665262690076126, 54.10535201082151247, 10.88017736071109987 ) ) ;
#53636 = CARTESIAN_POINT ( 'NONE',  ( 24.16423886937409904, 34.09541550158064638, 3.795296366450317205 ) ) ;
#53637 = CARTESIAN_POINT ( 'NONE',  ( 4.559911319644449179, 18.89701867748817321, 9.422509992056141925 ) ) ;
#53638 =( GEOMETRIC_REPRESENTATION_CONTEXT ( 3 ) GLOBAL_UNCERTAINTY_ASSIGNED_CONTEXT ( ( #72491 ) ) GLOBAL_UNIT_ASSIGNED_CONTEXT ( ( #98428, #5442, #13921 ) ) REPRESENTATION_CONTEXT ( 'NONE', 'WORKASPACE' ) );
#53639 = ADVANCED_FACE ( 'NONE', ( #66232 ), #87753, .F. ) ;
#53640 = CARTESIAN_POINT ( 'NONE',  ( 20.88017736071110875, 35.77201867748816966, -2.915334737309920765 ) ) ;
#53641 = B_SPLINE_CURVE_WITH_KNOTS ( 'NONE', 3,
 ( #62709, #24732, #17727, #8732, #55210, #39250 ),
 .UNSPECIFIED., .F., .F.,
 ( 4, 2, 4 ),
 ( 0.0002800032591452409876, 0.0006862085204420063315, 0.001092413781738771567 ),
 .UNSPECIFIED. ) ;
#53642 = DIRECTION ( 'NONE',  ( -0.6494480483301799945, 0.000000000000000000, -0.7604059656000340395 ) ) ;
#53643 = CARTESIAN_POINT ( 'NONE',  ( 0.5774900079438607392, 63.48035201082149825, 5.440088680355550821 ) ) ;
#53644 = CARTESIAN_POINT ( 'NONE',  ( 22.81628187352647785, 51.62363466993042493, 6.195893100308588602E-16 ) ) ;
#53645 = CARTESIAN_POINT ( 'NONE',  ( -3.469446951953614189E-15, -20.24106884899921255, -9.846743663894594434 ) ) ;
#53646 = ORIENTED_EDGE ( 'NONE', *, *, #34055, .F. ) ;
#53647 = DIRECTION ( 'NONE',  ( 0.000000000000000000, -1.000000000000000000, 0.000000000000000000 ) ) ;
#53648 = ORIENTED_EDGE ( 'NONE', *, *, #70024, .T. ) ;
#53649 = CARTESIAN_POINT ( 'NONE',  ( -46.44000000000001194, 92.00000000000000000, 9.500000000000000000 ) ) ;
#53650 = ORIENTED_EDGE ( 'NONE', *, *, #83758, .F. ) ;
#53652 = CARTESIAN_POINT ( 'NONE',  ( 4.559911319644449179, 3.897018677488171434, 9.422509992056141925 ) ) ;
#53651 = CARTESIAN_POINT ( 'NONE',  ( 17.08211943468705130, 58.47041550158063927, 12.26659068614894998 ) ) ;
#53654 = CARTESIAN_POINT ( 'NONE',  ( 17.20831665107776587, 59.13393115100078745, -7.208316651077762316 ) ) ;
#53653 = CARTESIAN_POINT ( 'NONE',  ( 1.472469842513823179, 20.59226448433411960, -4.923371831947296329 ) ) ;
#53655 = CARTESIAN_POINT ( 'NONE',  ( 20.32896413005680714, 60.57879003517448524, -5.963430220938276349 ) ) ;
#53656 = CARTESIAN_POINT ( 'NONE',  ( 20.15039907845753220, 49.72266099184918176, 6.262539305110078836 ) ) ;
#53657 = CARTESIAN_POINT ( 'NONE',  ( 10.00000000000000000, 9.758931151000785675, -9.846743663894594434 ) ) ;
#53658 = CARTESIAN_POINT ( 'NONE',  ( 6.565887622018943937, 10.16530133659708746, 12.81628187352647430 ) ) ;
#53659 = CARTESIAN_POINT ( 'NONE',  ( -5.204170427930421283E-15, 17.87363466993041783, -12.81628187352647608 ) ) ;
#53660 = ORIENTED_EDGE ( 'NONE', *, *, #95142, .F. ) ;
#53661 = CARTESIAN_POINT ( 'NONE',  ( -2.266590686148945544, 32.22041550158063927, 7.082119434687048631 ) ) ;
#53662 = ADVANCED_FACE ( 'NONE', ( #12253 ), #79145, .T. ) ;
#53663 = CARTESIAN_POINT ( 'NONE',  ( 20.36894250292379738, 44.92874883491396787, -10.36894250292379027 ) ) ;
#53664 = ORIENTED_EDGE ( 'NONE', *, *, #4215, .F. ) ;
#53665 = CARTESIAN_POINT ( 'NONE',  ( 0.6178305044545818747, 63.49863466993043204, -9.382169495545419124 ) ) ;
#53666 = CARTESIAN_POINT ( 'NONE',  ( 1.472469842513823179, 46.42559781766745175, 4.923371831947296329 ) ) ;
#53667 = CARTESIAN_POINT ( 'NONE',  ( 20.88017736071110519, 20.56368534415484106, 2.639326808657452039E-16 ) ) ;
#53668 = CARTESIAN_POINT ( 'NONE',  ( -6.866275848337654253, -80.67678253189122017, 2.500000000000001332 ) ) ;
#53669 = CARTESIAN_POINT ( 'NONE',  ( 12.63842701281683034, 57.46726448433411605, 9.846743663894596210 ) ) ;
#53670 = CARTESIAN_POINT ( 'NONE',  ( 5.076628168052704559, 45.17559781766745175, -8.527530157486179263 ) ) ;
#53671 = EDGE_CURVE ( 'NONE', #3928, #29178, #89242, .T. ) ;
#53672 = CARTESIAN_POINT ( 'NONE',  ( 14.35000000000000142, 98.49999999999998579, -8.525133428036873795 ) ) ;
#53673 = LINE ( 'NONE', #217, #54080 ) ;
#53674 =( NAMED_UNIT ( * ) SI_UNIT ( $, .STERADIAN. ) SOLID_ANGLE_UNIT ( ) );
#53675 = CARTESIAN_POINT ( 'NONE',  ( -9.065164099344370285, 0.5000000000000004441, -11.95084933600779564 ) ) ;
#53676 = ORIENTED_EDGE ( 'NONE', *, *, #64231, .F. ) ;
#53677 = CARTESIAN_POINT ( 'NONE',  ( 8.630000000000000782, 1.019547802438459216, 4.000000000000000000 ) ) ;
#53678 = CARTESIAN_POINT ( 'NONE',  ( 7.361572987183170547, 27.05059781766745175, 9.846743663894590881 ) ) ;
#53679 = COLOUR_RGB ( '', 0.31764706, 0.68627451, 0.89019608) ;
#53680 = CARTESIAN_POINT ( 'NONE',  ( 19.38216949554541202, 40.99863466993042493, 9.382169495545424454 ) ) ;
#53681 = CARTESIAN_POINT ( 'NONE',  ( -9.065164099344613646, 15.00000000000000000, 11.95084933600761445 ) ) ;
#53682 = CYLINDRICAL_SURFACE ( 'NONE', #15568, 15.00000000000000000 ) ;
#53683 = ORIENTED_EDGE ( 'NONE', *, *, #16159, .F. ) ;
#53684 = CARTESIAN_POINT ( 'NONE',  ( 14.49999999999999822, 11.50000000000000000, 6.000000000000000000 ) ) ;
#53685 = CARTESIAN_POINT ( 'NONE',  ( 19.84674366389459266, 58.30059781766745886, 2.638427012816836559 ) ) ;
#53686 = CARTESIAN_POINT ( 'NONE',  ( 13.79529636645030344, 38.26208216824729647, 14.16423886937410614 ) ) ;
#53687 = CARTESIAN_POINT ( 'NONE',  ( 1.472469842513823179, 55.59226448433412315, -4.923371831947296329 ) ) ;
#53688 = CARTESIAN_POINT ( 'NONE',  ( 0.000000000000000000, 0.000000000000000000, 0.000000000000000000 ) ) ;
#53689 = CARTESIAN_POINT ( 'NONE',  ( 2.791683348922240793, 1.633931151000784565, 7.208316651077764092 ) ) ;
#53690 = CARTESIAN_POINT ( 'NONE',  ( -2.816281873526473856, 54.12363466993041783, 9.499525473075851096E-16 ) ) ;
#53691 = CARTESIAN_POINT ( 'NONE',  ( 2.917880565312950480, 0.9704155015806342766, -12.26659068614894821 ) ) ;
#53692 = CARTESIAN_POINT ( 'NONE',  ( 1.472469842513823179, 51.42559781766745886, 4.923371831947296329 ) ) ;
#53693 = CARTESIAN_POINT ( 'NONE',  ( 2.035157376598824452, 58.68868534415482685, 7.964842623401179544 ) ) ;
#53694 = CIRCLE ( 'NONE', #66397, 1.500000000000001332 ) ;
#53695 = CARTESIAN_POINT ( 'NONE',  ( -5.204170427930421283E-15, 6.412123368507812948, -11.92686044187656513 ) ) ;
#53696 = CARTESIAN_POINT ( 'NONE',  ( 7.084665262690076126, 59.10535201082150536, 10.88017736071109987 ) ) ;
#53697 = VECTOR ( 'NONE', #79259, 1000.000000000000000 ) ;
#53698 = ORIENTED_EDGE ( 'NONE', *, *, #8089, .T. ) ;
#53699 = CARTESIAN_POINT ( 'NONE',  ( -3.949999999999997069, 99.99999999999998579, -8.525133428036873795 ) ) ;
#53700 = CARTESIAN_POINT ( 'NONE',  ( 17.96484262340118221, 31.18868534415483751, -7.964842623401177768 ) ) ;
#53702 = CARTESIAN_POINT ( 'NONE',  ( 15.44008868035555793, 51.39701867748816966, -9.422509992056140149 ) ) ;
#53701 = CARTESIAN_POINT ( 'NONE',  ( -1.099225684535947600, 3.706968003263753531, -6.408140936763238038 ) ) ;
#53703 = CARTESIAN_POINT ( 'NONE',  ( -18.89999999999999147, 99.99999999999998579, 8.000000000000000000 ) ) ;
#53704 = CARTESIAN_POINT ( 'NONE',  ( -0.8801773607110991993, 67.85535201082151957, -2.915334737309923874 ) ) ;
#53705 = CARTESIAN_POINT ( 'NONE',  ( 13.74344568549453527, 14.76984872681200756, 5.860030649989749207 ) ) ;
#53707 = DIRECTION ( 'NONE',  ( -0.000000000000000000, -0.000000000000000000, -1.000000000000000000 ) ) ;
#53706 = CARTESIAN_POINT ( 'NONE',  ( 20.88017736071110519, 35.56368534415484106, 2.639326808657452039E-16 ) ) ;
#53708 = CARTESIAN_POINT ( 'NONE',  ( 17.20831665107776587, 9.133931151000787452, -7.208316651077762316 ) ) ;
#53709 = ADVANCED_FACE ( 'NONE', ( #27249 ), #34461, .T. ) ;
#53710 = CARTESIAN_POINT ( 'NONE',  ( 19.84674366389459266, 43.30059781766744464, 2.638427012816836559 ) ) ;
#53711 = CARTESIAN_POINT ( 'NONE',  ( -32.19000000000001194, 93.50000000000000000, -10.09898361729590199 ) ) ;
#53712 = CARTESIAN_POINT ( 'NONE',  ( 10.36894250292379027, 18.67874883491397142, 10.36894250292378672 ) ) ;
#53713 = CARTESIAN_POINT ( 'NONE',  ( 19.84674366389459266, 58.71726448433411605, -2.638427012816827677 ) ) ;
#53714 = CARTESIAN_POINT ( 'NONE',  ( -4.164238869374099039, 66.80374883491396076, 8.674139862899312516E-16 ) ) ;
#53715 = CARTESIAN_POINT ( 'NONE',  ( 19.72487221294571569, 27.80223176428830811, -6.499999999999990230 ) ) ;
#53716 = EDGE_CURVE ( 'NONE', #44632, #51712, #74221, .T. ) ;
#53717 = CARTESIAN_POINT ( 'NONE',  ( -0.3689425029237881626, 27.42874883491397142, 10.36894250292379027 ) ) ;
#53718 = VECTOR ( 'NONE', #93666, 1000.000000000000000 ) ;
#53720 = CARTESIAN_POINT ( 'NONE',  ( -0.3689425029237898834, 51.17874883491397497, -10.36894250292378850 ) ) ;
#53719 = SHAPE_REPRESENTATION ( '1.1 Cage', ( #27931 ), #96613 ) ;
#53721 = CARTESIAN_POINT ( 'NONE',  ( 0.1532563361054083140, 31.00893115100078390, 1.131784320476157264E-15 ) ) ;
#53722 = VECTOR ( 'NONE', #31411, 999.9999999999998863 ) ;
#53723 = CARTESIAN_POINT ( 'NONE',  ( 18.52753015748617571, 18.09226448433411960, 4.923371831947298993 ) ) ;
#53724 =( NAMED_UNIT ( * ) SI_UNIT ( $, .STERADIAN. ) SOLID_ANGLE_UNIT ( ) );
#53725 = EDGE_LOOP ( 'NONE', ( #73162, #33830, #74175, #82695, #98616, #91990 ) ) ;
#53726 = CARTESIAN_POINT ( 'NONE',  ( 7.361572987183169658, 29.96726448433411960, -9.846743663894592657 ) ) ;
#53727 = CARTESIAN_POINT ( 'NONE',  ( 15.44008868035555793, 21.39701867748817321, -9.422509992056140149 ) ) ;
#53728 = CARTESIAN_POINT ( 'NONE',  ( 1.472469842513823179, 60.59226448433412315, -4.923371831947296329 ) ) ;
#53730 = DIRECTION ( 'NONE',  ( 0.000000000000000000, 0.000000000000000000, 1.000000000000000000 ) ) ;
#53729 = CARTESIAN_POINT ( 'NONE',  ( -4.164238869374099927, 7.012082168247302683, 3.795296366450308767 ) ) ;
#53731 = CARTESIAN_POINT ( 'NONE',  ( 48.54513754358777788, 66.34502130956990129, -8.000000000000000000 ) ) ;
#53732 = CARTESIAN_POINT ( 'NONE',  ( 10.00000000000000000, 9.758931151000785675, -9.846743663894594434 ) ) ;
#53733 = CARTESIAN_POINT ( 'NONE',  ( 22.81628187352648496, 41.83196800326375353, -3.434112377981050290 ) ) ;
#53734 = CARTESIAN_POINT ( 'NONE',  ( 17.20831665107776587, 42.88393115100077324, 7.208316651077764980 ) ) ;
#53735 = EDGE_LOOP ( 'NONE', ( #21815, #94980, #96396, #6358 ) ) ;
#53736 = CARTESIAN_POINT ( 'NONE',  ( 7.361572987183169658, 24.96726448433412315, -9.846743663894592657 ) ) ;
#53737 = CARTESIAN_POINT ( 'NONE',  ( 10.34945593955694498, -32.01313548011169985, -3.750000000000000000 ) ) ;
#53738 = CARTESIAN_POINT ( 'NONE',  ( -46.67785289142584304, 101.1465011330960948, -8.702494886479120950 ) ) ;
#53739 = CARTESIAN_POINT ( 'NONE',  ( 22.26659068614895176, 59.72041550158063927, -7.082119434687042414 ) ) ;
#53740 = CARTESIAN_POINT ( 'NONE',  ( 20.88017736071110875, 50.77201867748817676, -2.915334737309920765 ) ) ;
#53741 = CARTESIAN_POINT ( 'NONE',  ( 2.917880565312950480, 0.9704155015806342766, -12.26659068614894821 ) ) ;
#53742 = CARTESIAN_POINT ( 'NONE',  ( 2.791683348922237240, 40.38393115100078035, -7.208316651077763204 ) ) ;
#53743 = CARTESIAN_POINT ( 'NONE',  ( 19.42250999205614548, 10.98035201082150358, -5.440088680355545492 ) ) ;
#53744 = CARTESIAN_POINT ( 'NONE',  ( 19.84674366389459621, 33.50893115100078745, 7.409399052514197653E-17 ) ) ;
#53745 = CARTESIAN_POINT ( 'NONE',  ( 5.810202895580367510, 0.04922511925147131373, 13.56051778013769393 ) ) ;
#53746 = CARTESIAN_POINT ( 'NONE',  ( 10.00000000000000000, 49.75893115100078745, -9.846743663894594434 ) ) ;
#53747 = STYLED_ITEM ( 'NONE', ( #84137 ), #55465 ) ;
#53748 = CARTESIAN_POINT ( 'NONE',  ( 2.035157376598822676, 47.43868534415484817, -7.964842623401177768 ) ) ;
#53749 = CARTESIAN_POINT ( 'NONE',  ( -5.073789285385954528, 0.000000000000000000, -1.998618750576442338 ) ) ;
#53751 = EDGE_LOOP ( 'NONE', ( #36218, #32077, #88112, #32108 ) ) ;
#53750 = EDGE_CURVE ( 'NONE', #57430, #26946, #67953, .T. ) ;
#53752 = ORIENTED_EDGE ( 'NONE', *, *, #23064, .F. ) ;
#53753 = CARTESIAN_POINT ( 'NONE',  ( -14.97687855664608847, 0.5000000000000004441, 0.8325315005899532883 ) ) ;
#53754 = CARTESIAN_POINT ( 'NONE',  ( 14.54804176595378706, 15.00000000000000000, 6.650705016170673112 ) ) ;
#53755 = CARTESIAN_POINT ( 'NONE',  ( 5.076628168052704559, 5.175597817667451750, -8.527530157486179263 ) ) ;
#53756 = CARTESIAN_POINT ( 'NONE',  ( 6.565887622018943937, 58.08196800326376064, -12.81628187352647608 ) ) ;
#53758 = CARTESIAN_POINT ( 'NONE',  ( 19.84674366389459266, 43.71726448433410894, -2.638427012816827677 ) ) ;
#53757 = CARTESIAN_POINT ( 'NONE',  ( 15.44008868035555793, 11.39701867748817143, -9.422509992056140149 ) ) ;
#53759 = DIRECTION ( 'NONE',  ( -0.000000000000000000, -0.000000000000000000, -1.000000000000000000 ) ) ;
#53760 = CARTESIAN_POINT ( 'NONE',  ( -0.3689425029237898834, 26.17874883491396432, -10.36894250292378850 ) ) ;
#53761 = EDGE_CURVE ( 'NONE', #77766, #41488, #91712, .T. ) ;
#53762 = AXIS2_PLACEMENT_3D ( 'NONE', #18446, #71456, #34907 ) ;
#53763 = CARTESIAN_POINT ( 'NONE',  ( 20.36894250292379382, 53.67874883491397497, 10.36894250292379205 ) ) ;
#53764 = CARTESIAN_POINT ( 'NONE',  ( 10.00000000000000178, 57.25893115100078745, 9.846743663894594434 ) ) ;
#53765 = CARTESIAN_POINT ( 'NONE',  ( 4.698669664746514485, 0.000000000000000000, -2.767727949825255163 ) ) ;
#53766 = CARTESIAN_POINT ( 'NONE',  ( 17.96484262340118221, 54.93868534415484106, 7.964842623401181321 ) ) ;
#53767 = CARTESIAN_POINT ( 'NONE',  ( 20.88017736071110875, 65.77201867748817676, -2.915334737309920765 ) ) ;
#53768 = SPHERICAL_SURFACE ( 'NONE', #68567, 0.2500000000000000000 ) ;
#53769 = VERTEX_POINT ( 'NONE', #6732 ) ;
#53770 = CARTESIAN_POINT ( 'NONE',  ( -2.816281873526473856, 54.33196800326376064, 3.434112377981055619 ) ) ;
#53771 = EDGE_LOOP ( 'NONE', ( #7817, #21704, #36183 ) ) ;
#53772 = CARTESIAN_POINT ( 'NONE',  ( 0.1532563361054082862, 11.21726448433411605, 2.638427012816831674 ) ) ;
#53773 = CIRCLE ( 'NONE', #7459, 14.49999999999999822 ) ;
#53774 = EDGE_LOOP ( 'NONE', ( #68020, #76783, #25287, #38301 ) ) ;
#53775 = CARTESIAN_POINT ( 'NONE',  ( 17.08211943468705840, 25.13708216824730357, -12.26659068614894466 ) ) ;
#53776 = CARTESIAN_POINT ( 'NONE',  ( 5.076628168052704559, 25.17559781766745175, -8.527530157486179263 ) ) ;
#53777 = CARTESIAN_POINT ( 'NONE',  ( 10.00000000000000000, 26.81368534415484106, -10.88017736071110342 ) ) ;
#53778 = CARTESIAN_POINT ( 'NONE',  ( -42.16485527613927076, 107.5383484153110061, -4.500000000000000888 ) ) ;
#53779 = VERTEX_POINT ( 'NONE', #53216 ) ;
#53780 = CARTESIAN_POINT ( 'NONE',  ( 17.96484262340118221, 31.18868534415483751, -7.964842623401177768 ) ) ;
#53781 = AXIS2_PLACEMENT_3D ( 'NONE', #82587, #98104, #94515 ) ;
#53782 =( BOUNDED_CURVE ( )  B_SPLINE_CURVE ( 2, ( #92982, #24018, #39512, #70004, #86958, #54487, #31487, #71484, #18472 ),
 .UNSPECIFIED., .F., .F. ) 
 B_SPLINE_CURVE_WITH_KNOTS ( ( 3, 2, 2, 2, 3 ),
 ( 0.2239427359034107945, 0.2261904761904761918, 0.2321428571428571508, 0.2380952380952380820, 0.2403429783823026467 ),
 .UNSPECIFIED. ) 
 CURVE ( )  GEOMETRIC_REPRESENTATION_ITEM ( )  RATIONAL_B_SPLINE_CURVE ( ( 0.9839835555609424134, 0.9871328979762477029, 1.000000000000000000, 0.9659258262890683122, 1.000000000000000000, 0.9659258262890683122, 1.000000000000000000, 0.9871328979762523659, 0.9839835555609446338 ) ) 
 REPRESENTATION_ITEM ( '' )  );
#53783 = VERTEX_POINT ( 'NONE', #90217 ) ;
#53784 = ORIENTED_EDGE ( 'NONE', *, *, #262, .F. ) ;
#53785 = EDGE_CURVE ( 'NONE', #17162, #93214, #248, .T. ) ;
#53786 =( LENGTH_UNIT ( ) NAMED_UNIT ( * ) SI_UNIT ( .MILLI., .METRE. ) );
#53787 = ORIENTED_EDGE ( 'NONE', *, *, #72367, .F. ) ;
#53788 = CARTESIAN_POINT ( 'NONE',  ( 22.81628187352647785, 16.62363466993042138, 6.195893100308588602E-16 ) ) ;
#53789 = CARTESIAN_POINT ( 'NONE',  ( 64.56412365047461321, 44.99999999999998579, 7.000000000000000000 ) ) ;
#53790 = CARTESIAN_POINT ( 'NONE',  ( 18.52753015748617571, 13.09226448433411960, 4.923371831947298993 ) ) ;
#53791 = CARTESIAN_POINT ( 'NONE',  ( 8.564643372776536978, 15.00000000000000000, 12.31449893000746343 ) ) ;
#53792 = CARTESIAN_POINT ( 'NONE',  ( 20.88017736071110164, 10.35535201082150536, 2.915334737309930979 ) ) ;
#53793 = CARTESIAN_POINT ( 'NONE',  ( 0.1532563361054083140, 16.00893115100078390, 1.131784320476157264E-15 ) ) ;
#53794 = CARTESIAN_POINT ( 'NONE',  ( 4.559911319644449179, 27.23035201082150536, -9.422509992056141925 ) ) ;
#53795 = AXIS2_PLACEMENT_3D ( 'NONE', #56355, #88320, #80325 ) ;
#53796 = AXIS2_PLACEMENT_3D ( 'NONE', #46451, #75471, #76944 ) ;
#53797 = AXIS2_PLACEMENT_3D ( 'NONE', #96681, #28159, #36154 ) ;
#53798 = ORIENTED_EDGE ( 'NONE', *, *, #97214, .T. ) ;
#53799 = ORIENTED_EDGE ( 'NONE', *, *, #52387, .T. ) ;
#53800 = CIRCLE ( 'NONE', #45812, 14.49999999999999822 ) ;
#53801 = CARTESIAN_POINT ( 'NONE',  ( -2.816281873526471635, 63.91530133659708923, -3.434112377981056508 ) ) ;
#53802 = CARTESIAN_POINT ( 'NONE',  ( 0.5774900079438607392, 58.48035201082151247, 5.440088680355550821 ) ) ;
#53803 = LINE ( 'NONE', #84314, #35623 ) ;
#53804 = CARTESIAN_POINT ( 'NONE',  ( 13.43411237798105340, 55.58196800326374643, 12.81628187352647963 ) ) ;
#53805 = CARTESIAN_POINT ( 'NONE',  ( 19.42250999205614193, 55.14701867748817676, 5.440088680355555262 ) ) ;
#53806 = CARTESIAN_POINT ( 'NONE',  ( 10.00000000000000000, -2.126365330069579951, -12.81628187352647608 ) ) ;
#53807 = DIRECTION ( 'NONE',  ( 0.9588197348681928300, 0.000000000000000000, 0.2840153447039234780 ) ) ;
#53808 = CARTESIAN_POINT ( 'NONE',  ( 5.076628168052703671, 31.84226448433412315, 8.527530157486179263 ) ) ;
#53809 = CARTESIAN_POINT ( 'NONE',  ( 0.6178305044545838731, 49.74863466993041072, 9.382169495545420901 ) ) ;
#53810 = CARTESIAN_POINT ( 'NONE',  ( 12.63842701281683922, 24.55059781766745175, -9.846743663894590881 ) ) ;
#53811 = CARTESIAN_POINT ( 'NONE',  ( -1.099225684535947600, 18.70696800326375353, -6.408140936763238038 ) ) ;
#53813 = CARTESIAN_POINT ( 'NONE',  ( -3.499999999999998668, 1.019547802438465434, -2.750000000000000444 ) ) ;
#53812 = LINE ( 'NONE', #84323, #38816 ) ;
#53814 = CARTESIAN_POINT ( 'NONE',  ( 15.44008868035555260, 39.73035201082150536, 9.422509992056143702 ) ) ;
#53815 = CARTESIAN_POINT ( 'NONE',  ( 0.1532563361054083140, 66.00893115100079456, 1.131784320476157264E-15 ) ) ;
#53816 = DIRECTION ( 'NONE',  ( 0.000000000000000000, 1.000000000000000000, 0.000000000000000000 ) ) ;
#53817 = CARTESIAN_POINT ( 'NONE',  ( 7.361572987183170547, 17.05059781766745530, 9.846743663894590881 ) ) ;
#53818 = CARTESIAN_POINT ( 'NONE',  ( 0.1532563361054083140, 11.00893115100078568, 1.131784320476157264E-15 ) ) ;
#53819 = CARTESIAN_POINT ( 'NONE',  ( 7.084665262690076126, 17.02201867748817676, -10.88017736071110164 ) ) ;
#53820 = CARTESIAN_POINT ( 'NONE',  ( 6.565887622018943937, 15.16530133659708568, 12.81628187352647430 ) ) ;
#53822 = CARTESIAN_POINT ( 'NONE',  ( 0.5774900079438590739, 2.647018677488170990, -5.440088680355550821 ) ) ;
#53821 = PRESENTATION_LAYER_ASSIGNMENT (  '', '', ( #49032 ) ) ;
#53823 = CARTESIAN_POINT ( 'NONE',  ( 10.00000000000000178, 57.25893115100078745, 9.846743663894594434 ) ) ;
#53824 = CARTESIAN_POINT ( 'NONE',  ( 6.757497259963602509, -58.30388498733370284, -2.500000000000000000 ) ) ;
#53825 = CARTESIAN_POINT ( 'NONE',  ( 17.96484262340118221, 11.18868534415484106, -7.964842623401177768 ) ) ;
#53826 = CARTESIAN_POINT ( 'NONE',  ( 12.63842701281683034, 47.46726448433412315, 9.846743663894596210 ) ) ;
#53827 = VECTOR ( 'NONE', #97071, 1000.000000000000000 ) ;
#53828 = DIRECTION ( 'NONE',  ( -0.06975647374410356982, -0.9975640502598257520, -0.000000000000000000 ) ) ;
#53829 = CARTESIAN_POINT ( 'NONE',  ( 2.035157376598824452, 18.68868534415484106, 7.964842623401179544 ) ) ;
#53830 = CARTESIAN_POINT ( 'NONE',  ( 20.05723567505239302, 69.83236346210667023, -6.413539670616450472 ) ) ;
#53831 = CARTESIAN_POINT ( 'NONE',  ( 15.44008868035555793, 36.39701867748816966, -9.422509992056140149 ) ) ;
#53833 = CARTESIAN_POINT ( 'NONE',  ( 0.000000000000000000, 0.5000000000000004441, 0.000000000000000000 ) ) ;
#53832 = CARTESIAN_POINT ( 'NONE',  ( 7.084665262690076126, 4.105352010821503583, 10.88017736071109987 ) ) ;
#53834 = CARTESIAN_POINT ( 'NONE',  ( -3.115783986955370732, 3.816680036666981737E-16, -14.16128137375401685 ) ) ;
#53835 = CARTESIAN_POINT ( 'NONE',  ( 19.84674366389459621, 23.50893115100078390, 7.409399052514197653E-17 ) ) ;
#53836 = CARTESIAN_POINT ( 'NONE',  ( 21.09922568453595559, 12.04030133659708746, -6.408140936763230044 ) ) ;
#53837 = CARTESIAN_POINT ( 'NONE',  ( -46.77384778588437086, 103.6211922023598362, 6.142868351312646524 ) ) ;
#53838 = PRESENTATION_STYLE_ASSIGNMENT (( #91336 ) ) ;
#53839 = EDGE_CURVE ( 'NONE', #43481, #21313, #22733, .T. ) ;
#53840 = CARTESIAN_POINT ( 'NONE',  ( 14.92337183194729633, 62.67559781766745886, 8.527530157486181039 ) ) ;
#53841 = CARTESIAN_POINT ( 'NONE',  ( -13.14228782657329653, 0.5000000000000004441, -7.230509711182418364 ) ) ;
#53842 = CARTESIAN_POINT ( 'NONE',  ( -10.07341714981312109, -32.14978703225555989, -3.750000000000000000 ) ) ;
#53843 = CARTESIAN_POINT ( 'NONE',  ( 24.16423886937410614, 14.51208216824730179, -3.795296366450302550 ) ) ;
#53844 = CIRCLE ( 'NONE', #36284, 14.49999999999999822 ) ;
#53845 = CARTESIAN_POINT ( 'NONE',  ( 17.20831665107776587, 37.88393115100078745, 7.208316651077764980 ) ) ;
#53846 =( NAMED_UNIT ( * ) SI_UNIT ( $, .STERADIAN. ) SOLID_ANGLE_UNIT ( ) );
#53847 = ORIENTED_EDGE ( 'NONE', *, *, #17613, .F. ) ;
#53848 = CARTESIAN_POINT ( 'NONE',  ( 13.79529636645031943, 60.34541550158063927, -14.16423886937409904 ) ) ;
#53849 = AXIS2_PLACEMENT_3D ( 'NONE', #26034, #79022, #33505 ) ;
#53850 = CARTESIAN_POINT ( 'NONE',  ( 19.84674366389459266, 3.717264484334118713, -2.638427012816827677 ) ) ;
#53852 = CARTESIAN_POINT ( 'NONE',  ( -11.61621867929619611, 15.00000000000000000, 10.99731149103378058 ) ) ;
#53851 = CARTESIAN_POINT ( 'NONE',  ( 0.2751277870542910842, 63.21833443783937412, 6.499999999999992006 ) ) ;
#53853 = CARTESIAN_POINT ( 'NONE',  ( 10.00000000000000178, 49.31368534415484106, 10.88017736071110342 ) ) ;
#53854 = CARTESIAN_POINT ( 'NONE',  ( 22.81628187352648496, 46.83196800326376064, -3.434112377981050290 ) ) ;
#53855 = CARTESIAN_POINT ( 'NONE',  ( -0.8801773607110991993, 22.85535201082150181, -2.915334737309923874 ) ) ;
#53856 = CARTESIAN_POINT ( 'NONE',  ( 16.40814093676323893, 45.79030133659708923, 11.09922568453595026 ) ) ;
#53857 = CARTESIAN_POINT ( 'NONE',  ( 3.591859063236763294, -1.709698663402913210, -11.09922568453595026 ) ) ;
#53858 = CARTESIAN_POINT ( 'NONE',  ( 0.2751277870542911952, 53.21833443783938122, 6.499999999999992006 ) ) ;
#53859 = EDGE_LOOP ( 'NONE', ( #49294, #54874, #78104, #85678 ) ) ;
#53860 = CARTESIAN_POINT ( 'NONE',  ( 2.126467202668119061, 1.181022659884616743, -6.500000000000000888 ) ) ;
#53861 = CARTESIAN_POINT ( 'NONE',  ( 6.204703633549690345, 37.84541550158063927, 14.16423886937410082 ) ) ;
#53862 = CARTESIAN_POINT ( 'NONE',  ( 10.00000000000000178, 13.05374883491396787, 14.16423886937410082 ) ) ;
#53863 = CARTESIAN_POINT ( 'NONE',  ( 20.88017736071110875, 25.77201867748816966, -2.915334737309920765 ) ) ;
#53864 =( GEOMETRIC_REPRESENTATION_CONTEXT ( 3 ) GLOBAL_UNCERTAINTY_ASSIGNED_CONTEXT ( ( #73142 ) ) GLOBAL_UNIT_ASSIGNED_CONTEXT ( ( #19975, #50967, #10511 ) ) REPRESENTATION_CONTEXT ( 'NONE', 'WORKASPACE' ) );
#53865 = CARTESIAN_POINT ( 'NONE',  ( 15.44008868035555793, 31.39701867748817676, -9.422509992056140149 ) ) ;
#53866 = CARTESIAN_POINT ( 'NONE',  ( 9.876730923139357188, 14.49999999999999112, -11.28938378619066363 ) ) ;
#53867 = CARTESIAN_POINT ( 'NONE',  ( 17.75000000000001776, 4.561680251642721935E-15, -6.250000000000000000 ) ) ;
#53868 = CARTESIAN_POINT ( 'NONE',  ( 19.42250999205614548, 65.98035201082151957, -5.440088680355545492 ) ) ;
#53869 = CARTESIAN_POINT ( 'NONE',  ( 17.96484262340118221, 59.93868534415484106, 7.964842623401181321 ) ) ;
#53870 = CARTESIAN_POINT ( 'NONE',  ( 10.00000000000000178, 25.37363466993041783, 12.81628187352647608 ) ) ;
#53871 = CARTESIAN_POINT ( 'NONE',  ( 18.17829156368508237, 19.16792564121896802, 6.499999999999999112 ) ) ;
#53872 = CARTESIAN_POINT ( 'NONE',  ( 6.000000000000000000, 11.50000000000000000, 6.000000000000000000 ) ) ;
#53873 = CARTESIAN_POINT ( 'NONE',  ( 10.00000000000000178, 7.258931151000785675, 9.846743663894594434 ) ) ;
#53874 = CARTESIAN_POINT ( 'NONE',  ( 19.84674366389459266, 33.30059781766744464, 2.638427012816836559 ) ) ;
#53875 = CIRCLE ( 'NONE', #72973, 3.999999999999999112 ) ;
#53876 = CARTESIAN_POINT ( 'NONE',  ( 15.44008868035555793, 11.39701867748817143, -9.422509992056140149 ) ) ;
#53877 = AXIS2_PLACEMENT_3D ( 'NONE', #27356, #20854, #76193 ) ;
#53878 = AXIS2_PLACEMENT_3D ( 'NONE', #61492, #76013, #68030 ) ;
#53879 = EDGE_CURVE ( 'NONE', #65586, #800, #38883, .T. ) ;
#53880 = CARTESIAN_POINT ( 'NONE',  ( -2.816281873526471635, 33.91530133659708213, -3.434112377981056508 ) ) ;
#53881 = CARTESIAN_POINT ( 'NONE',  ( 5.076628168052703671, 6.842264484334118713, 8.527530157486179263 ) ) ;
#53882 = CARTESIAN_POINT ( 'NONE',  ( 20.88017736071110164, 10.35535201082150714, 2.915334737309930979 ) ) ;
#53883 = CARTESIAN_POINT ( 'NONE',  ( 12.63842701281683922, 39.55059781766744464, -9.846743663894590881 ) ) ;
#53884 = CARTESIAN_POINT ( 'NONE',  ( 19.84674366389459621, 33.50893115100078745, 7.409399052514197653E-17 ) ) ;
#53885 = EDGE_CURVE ( 'NONE', #52058, #16281, #61686, .T. ) ;
#53886 = CARTESIAN_POINT ( 'NONE',  ( 10.00000000000000000, 20.55374883491396787, -14.16423886937410082 ) ) ;
#53887 = CARTESIAN_POINT ( 'NONE',  ( 0.5774900079438590739, 27.64701867748817676, -5.440088680355550821 ) ) ;
#53888 = CARTESIAN_POINT ( 'NONE',  ( 12.91533473730993009, 6.605352010821504471, -10.88017736071109987 ) ) ;
#53889 = CARTESIAN_POINT ( 'NONE',  ( 19.42250999205614548, 35.98035201082151247, -5.440088680355545492 ) ) ;
#53890 = CARTESIAN_POINT ( 'NONE',  ( 10.00000000000000178, 34.31368534415484106, 10.88017736071110342 ) ) ;
#53891 = ORIENTED_EDGE ( 'NONE', *, *, #42921, .F. ) ;
#53892 = CARTESIAN_POINT ( 'NONE',  ( 19.42250999205614548, 35.98035201082151247, -5.440088680355545492 ) ) ;
#53893 = CARTESIAN_POINT ( 'NONE',  ( 21.09922568453595559, 57.04030133659708923, -6.408140936763230044 ) ) ;
#53894 = CARTESIAN_POINT ( 'NONE',  ( 10.00000000000000178, 44.31368534415484106, 10.88017736071110342 ) ) ;
#53895 = CARTESIAN_POINT ( 'NONE',  ( 4.559911319644449179, 48.89701867748817676, 9.422509992056141925 ) ) ;
#53896 = ORIENTED_EDGE ( 'NONE', *, *, #94873, .F. ) ;
#53897 = CARTESIAN_POINT ( 'NONE',  ( 15.44008868035555260, 54.73035201082150536, 9.422509992056143702 ) ) ;
#53898 = CARTESIAN_POINT ( 'NONE',  ( 6.829574850505124139, -88.00372650098208283, 4.000000000000000000 ) ) ;
#53899 = CARTESIAN_POINT ( 'NONE',  ( -2.266590686148945544, 66.38708216824730357, -7.082119434687050408 ) ) ;
#53900 = CARTESIAN_POINT ( 'NONE',  ( 18.52753015748617571, 3.092264484334118269, 4.923371831947298993 ) ) ;
#53901 = CARTESIAN_POINT ( 'NONE',  ( 19.10478245763052030, 55.10160829253886305, 5.990408912944319653 ) ) ;
#53902 = AXIS2_PLACEMENT_3D ( 'NONE', #14401, #66392, #52381 ) ;
#53903 = CARTESIAN_POINT ( 'NONE',  ( -7.374944882893555764, -78.83129233208414632, -4.000000000000000888 ) ) ;
#53904 = CARTESIAN_POINT ( 'NONE',  ( 19.84674366389459266, 38.30059781766745175, 2.638427012816836559 ) ) ;
#53905 = EDGE_LOOP ( 'NONE', ( #28656, #60134, #20192, #798, #38668, #61233 ) ) ;
#53906 = CARTESIAN_POINT ( 'NONE',  ( 18.52753015748618282, 33.92559781766745886, -4.923371831947291888 ) ) ;
#53907 = CARTESIAN_POINT ( 'NONE',  ( 19.42250999205614193, 35.14701867748816966, 5.440088680355555262 ) ) ;
#53908 = CARTESIAN_POINT ( 'NONE',  ( 0.1532563361054083140, 36.00893115100078745, 1.131784320476157264E-15 ) ) ;
#53909 = CARTESIAN_POINT ( 'NONE',  ( 22.81628187352647785, 16.41530133659708923, 3.434112377981063169 ) ) ;
#53911 = CARTESIAN_POINT ( 'NONE',  ( 17.96484262340118221, 61.18868534415482685, -7.964842623401177768 ) ) ;
#53910 = DIRECTION ( 'NONE',  ( 0.8141155183563107967, 0.000000000000000000, 0.5807029557109515405 ) ) ;
#53913 =( NAMED_UNIT ( * ) PLANE_ANGLE_UNIT ( ) SI_UNIT ( $, .RADIAN. ) );
#53912 = CARTESIAN_POINT ( 'NONE',  ( 7.084665262690076126, 49.10535201082149825, 10.88017736071109987 ) ) ;
#53914 = CARTESIAN_POINT ( 'NONE',  ( -2.266590686148945544, 62.22041550158063927, 7.082119434687048631 ) ) ;
#53915 = ADVANCED_FACE ( 'NONE', ( #21750 ), #52717, .T. ) ;
#53916 = CARTESIAN_POINT ( 'NONE',  ( 19.38216949554541202, 15.99863466993042138, 9.382169495545424454 ) ) ;
#53917 = CARTESIAN_POINT ( 'NONE',  ( 5.500000000000000000, 11.00000000000000000, -5.000000000000000000 ) ) ;
#53918 = ORIENTED_EDGE ( 'NONE', *, *, #8830, .F. ) ;
#53919 = CARTESIAN_POINT ( 'NONE',  ( 21.09922568453594849, 11.20696800326375531, 6.408140936763242479 ) ) ;
#53920 = CARTESIAN_POINT ( 'NONE',  ( 20.88017736071110519, 15.56368534415483751, 2.639326808657452039E-16 ) ) ;
#53921 = CARTESIAN_POINT ( 'NONE',  ( 17.96484262340118221, 61.18868534415482685, -7.964842623401177768 ) ) ;
#53922 = ORIENTED_EDGE ( 'NONE', *, *, #3663, .T. ) ;
#53923 = CARTESIAN_POINT ( 'NONE',  ( 17.20831665107776587, 2.883931151000785231, 7.208316651077764980 ) ) ;
#53924 = CARTESIAN_POINT ( 'NONE',  ( 0.1532563361054082862, 51.21726448433412315, 2.638427012816831674 ) ) ;
#53925 = CARTESIAN_POINT ( 'NONE',  ( 19.84674366389459266, 38.30059781766745175, 2.638427012816836559 ) ) ;
#53926 = DIRECTION ( 'NONE',  ( 0.9366721892484018985, 0.000000000000000000, -0.3502073812594559410 ) ) ;
#53927 = VECTOR ( 'NONE', #20392, 1000.000000000000000 ) ;
#53928 = CARTESIAN_POINT ( 'NONE',  ( 1.472469842513823179, 21.42559781766745175, 4.923371831947296329 ) ) ;
#53929 = CARTESIAN_POINT ( 'NONE',  ( -9.065164099344613646, 0.5000000000000004441, 11.95084933600761445 ) ) ;
#53930 = CARTESIAN_POINT ( 'NONE',  ( -7.750000000000000000, 79.82179676972448590, 6.250000000000000000 ) ) ;
#53933 = LINE ( 'NONE', #76922, #92998 ) ;
#53932 = VECTOR ( 'NONE', #27018, 1000.000000000000000 ) ;
#53931 = CARTESIAN_POINT ( 'NONE',  ( 14.92337183194729988, 9.342264484334119601, -8.527530157486177487 ) ) ;
#53934 = CARTESIAN_POINT ( 'NONE',  ( 20.24186590665276597, 44.73410085661203794, 6.114288769123062295 ) ) ;
#53936 = VERTEX_POINT ( 'NONE', #29713 ) ;
#53935 = CARTESIAN_POINT ( 'NONE',  ( 17.20831665107776587, 47.88393115100078745, 7.208316651077764980 ) ) ;
#53937 = CIRCLE ( 'NONE', #39605, 0.2500000000000002220 ) ;
#53938 = CARTESIAN_POINT ( 'NONE',  ( 11.25000000000000000, 2.826366962315984832, -3.014428414850133908 ) ) ;
#53939 = CARTESIAN_POINT ( 'NONE',  ( 16.40814093676324603, 12.45696800326375353, -11.09922568453594671 ) ) ;
#53940 = CARTESIAN_POINT ( 'NONE',  ( 7.084665262690076126, 54.10535201082151247, 10.88017736071109987 ) ) ;
#53941 = CARTESIAN_POINT ( 'NONE',  ( 24.16423886937409904, 29.09541550158063572, 3.795296366450317205 ) ) ;
#53942 = CARTESIAN_POINT ( 'NONE',  ( 1.472469842513823179, 0.5922644843341181575, -4.923371831947296329 ) ) ;
#53943 = CARTESIAN_POINT ( 'NONE',  ( 24.16423886937409904, 49.09541550158063217, 3.795296366450317205 ) ) ;
#53944 = CARTESIAN_POINT ( 'NONE',  ( 2.917880565312950480, 55.97041550158063217, -12.26659068614894821 ) ) ;
#53945 = CARTESIAN_POINT ( 'NONE',  ( 20.36894250292379382, 18.67874883491397142, 10.36894250292379205 ) ) ;
#53947 = CARTESIAN_POINT ( 'NONE',  ( -0.2418659066527630297, 38.09014588040356131, 6.114288769123057854 ) ) ;
#53946 = CARTESIAN_POINT ( 'NONE',  ( 6.204703633549690345, 22.84541550158062861, 14.16423886937410082 ) ) ;
#53948 = CARTESIAN_POINT ( 'NONE',  ( -9.742785792574931492, 10.53470029564931920, 5.625000000000008882 ) ) ;
#53950 = CARTESIAN_POINT ( 'NONE',  ( 0.1532563361054082862, 36.21726448433410894, 2.638427012816831674 ) ) ;
#53949 = CARTESIAN_POINT ( 'NONE',  ( 5.000000000000002665, 44.99999999999999289, 0.000000000000000000 ) ) ;
#53951 = CARTESIAN_POINT ( 'NONE',  ( 17.96484262340118221, 26.18868534415483396, -7.964842623401177768 ) ) ;
#53952 = CARTESIAN_POINT ( 'NONE',  ( -7.684764310694971456, 14.49999999999999822, 12.88194075009929840 ) ) ;
#53953 = FACE_OUTER_BOUND ( 'NONE', #6537, .T. ) ;
#53954 = CARTESIAN_POINT ( 'NONE',  ( 19.64201483648641045, 84.95676665491684787, -5.303713241054131444 ) ) ;
#53955 = EDGE_CURVE ( 'NONE', #21351, #42200, #68850, .T. ) ;
#53956 = CARTESIAN_POINT ( 'NONE',  ( 7.361572987183169658, 44.96726448433412315, -9.846743663894592657 ) ) ;
#53957 = CARTESIAN_POINT ( 'NONE',  ( 3.591859063236761518, 54.95696800326376064, 11.09922568453594849 ) ) ;
#53958 = CARTESIAN_POINT ( 'NONE',  ( -5.204170427930421283E-15, -4.446251165086026802, -14.16423886937410082 ) ) ;
#53959 = CARTESIAN_POINT ( 'NONE',  ( 17.20831665107776587, 37.88393115100078745, 7.208316651077764980 ) ) ;
#53960 = CARTESIAN_POINT ( 'NONE',  ( 17.20831665107776587, 47.88393115100078745, 7.208316651077764980 ) ) ;
#53961 = CARTESIAN_POINT ( 'NONE',  ( 17.08211943468705130, 43.47041550158063927, 12.26659068614894998 ) ) ;
#53962 = EDGE_LOOP ( 'NONE', ( #86090, #71394, #10388, #24778 ) ) ;
#53963 = CARTESIAN_POINT ( 'NONE',  ( 10.00000000000000178, 13.05374883491396787, 14.16423886937410082 ) ) ;
#53964 = CARTESIAN_POINT ( 'NONE',  ( 4.559911319644449179, 57.23035201082150536, -9.422509992056141925 ) ) ;
#53965 = CARTESIAN_POINT ( 'NONE',  ( 17.96484262340118221, 9.938685344154839285, 7.964842623401181321 ) ) ;
#53966 = CARTESIAN_POINT ( 'NONE',  ( 3.591859063236761518, 4.956968003263753531, 11.09922568453594849 ) ) ;
#53967 = CARTESIAN_POINT ( 'NONE',  ( 20.32896413005680714, 2.604976035794174027, -5.963430220938276349 ) ) ;
#53968 = CARTESIAN_POINT ( 'NONE',  ( 12.91533473730993009, 66.60535201082150536, -10.88017736071109987 ) ) ;
#53969 = DIRECTION ( 'NONE',  ( 0.000000000000000000, 0.000000000000000000, 1.000000000000000000 ) ) ;
#53970 = CARTESIAN_POINT ( 'NONE',  ( 0.1955144967548973212, 14.32703681773340776, -6.500000000002781775 ) ) ;
#53971 = CARTESIAN_POINT ( 'NONE',  ( -4.164238869374099927, 62.01208216824728936, 3.795296366450308767 ) ) ;
#53972 = CARTESIAN_POINT ( 'NONE',  ( 0.3093388210927642268, 14.49999999999999822, -14.99680997725065978 ) ) ;
#53973 = CARTESIAN_POINT ( 'NONE',  ( 15.44008868035555793, 31.39701867748817676, -9.422509992056140149 ) ) ;
#53974 = CARTESIAN_POINT ( 'NONE',  ( 4.559911319644449179, 18.89701867748817321, 9.422509992056141925 ) ) ;
#53975 = CARTESIAN_POINT ( 'NONE',  ( 14.92337183194729633, 57.67559781766745886, 8.527530157486181039 ) ) ;
#53976 = CARTESIAN_POINT ( 'NONE',  ( 19.84674366389459621, 58.50893115100078745, 7.409399052514197653E-17 ) ) ;
#53977 = CARTESIAN_POINT ( 'NONE',  ( 3.591859063236761518, 54.95696800326376064, 11.09922568453594849 ) ) ;
#53978 =( NAMED_UNIT ( * ) SI_UNIT ( $, .STERADIAN. ) SOLID_ANGLE_UNIT ( ) );
#53979 = ORIENTED_EDGE ( 'NONE', *, *, #3531, .T. ) ;
#53980 = CARTESIAN_POINT ( 'NONE',  ( 19.42250999205614548, 15.98035201082150714, -5.440088680355545492 ) ) ;
#53981 = CARTESIAN_POINT ( 'NONE',  ( 13.43411237798106583, 12.66530133659708746, -12.81628187352647252 ) ) ;
#53982 = DIRECTION ( 'NONE',  ( 0.04361938736534638067, 0.000000000000000000, -0.9990482215818573541 ) ) ;
#53983 = CIRCLE ( 'NONE', #57178, 20.00000000000000000 ) ;
#53984 = ADVANCED_FACE ( 'NONE', ( #74728 ), #75718, .F. ) ;
#53985 = CARTESIAN_POINT ( 'NONE',  ( 0.1532563361054100626, 45.80059781766745886, -2.638427012816831230 ) ) ;
#53986 = CARTESIAN_POINT ( 'NONE',  ( 20.88017736071110164, 50.35535201082151247, 2.915334737309930979 ) ) ;
#53987 = CARTESIAN_POINT ( 'NONE',  ( 19.38216949554541202, 20.99863466993042138, 9.382169495545424454 ) ) ;
#53989 = FACE_OUTER_BOUND ( 'NONE', #33498, .T. ) ;
#53988 = CARTESIAN_POINT ( 'NONE',  ( -0.8801773607111008646, 63.27201867748817676, 2.915334737309923430 ) ) ;
#53990 = FACE_OUTER_BOUND ( 'NONE', #8921, .T. ) ;
#53991 = ORIENTED_EDGE ( 'NONE', *, *, #57701, .F. ) ;
#53992 = FILL_AREA_STYLE ('',( #61486 ) ) ;
#53993 = DIRECTION ( 'NONE',  ( 0.000000000000000000, -1.000000000000000000, 0.000000000000000000 ) ) ;
#53994 = EDGE_CURVE ( 'NONE', #11431, #18624, #11902, .T. ) ;
#53995 = CARTESIAN_POINT ( 'NONE',  ( -0.8801773607110991993, 47.85535201082150536, -2.915334737309923874 ) ) ;
#53997 = CARTESIAN_POINT ( 'NONE',  ( 17.08211943468705130, 13.47041550158063572, 12.26659068614894998 ) ) ;
#53996 = CARTESIAN_POINT ( 'NONE',  ( 19.38216949554541202, 40.99863466993042493, 9.382169495545424454 ) ) ;
#53998 = AXIS2_PLACEMENT_3D ( 'NONE', #96086, #79600, #34566 ) ;
#53999 = CARTESIAN_POINT ( 'NONE',  ( 17.20831665107776587, 62.88393115100078745, 7.208316651077764980 ) ) ;
#54000 = CARTESIAN_POINT ( 'NONE',  ( 0.1532563361054083140, 1.008931151000784787, 1.131784320476157264E-15 ) ) ;
#54001 = CARTESIAN_POINT ( 'NONE',  ( -19.64999999999999858, 98.99999999999998579, -7.750000000000000000 ) ) ;
#54002 = CARTESIAN_POINT ( 'NONE',  ( -4.164238869374099927, 42.01208216824728936, 3.795296366450308767 ) ) ;
#54003 = FACE_OUTER_BOUND ( 'NONE', #58799, .T. ) ;
#54004 = CARTESIAN_POINT ( 'NONE',  ( 7.084665262690076126, 4.105352010821503583, 10.88017736071109987 ) ) ;
#54005 = CARTESIAN_POINT ( 'NONE',  ( -4.511928667086301914, -13.83795187542450122, -4.000000000000000888 ) ) ;
#54006 = CIRCLE ( 'NONE', #28454, 0.09999999999999982514 ) ;
#54007 = ORIENTED_EDGE ( 'NONE', *, *, #1053, .T. ) ;
#54008 = EDGE_LOOP ( 'NONE', ( #41152, #18217, #52850, #38568 ) ) ;
#54009 = CARTESIAN_POINT ( 'NONE',  ( 0.5774900079438607392, 3.480352010821504916, 5.440088680355550821 ) ) ;
#54010 = CARTESIAN_POINT ( 'NONE',  ( -0.8801773607110991993, 7.855352010821506248, -2.915334737309923874 ) ) ;
#54011 = CARTESIAN_POINT ( 'NONE',  ( 12.63842701281683034, 42.46726448433412315, 9.846743663894596210 ) ) ;
#54012 = CARTESIAN_POINT ( 'NONE',  ( 19.38216949554541557, 37.24863466993041783, -9.382169495545420901 ) ) ;
#54013 = PRESENTATION_STYLE_ASSIGNMENT (( #31007 ) ) ;
#54015 = CARTESIAN_POINT ( 'NONE',  ( -4.164238869374099927, 7.012082168247302683, 3.795296366450308767 ) ) ;
#54014 = CARTESIAN_POINT ( 'NONE',  ( -8.223478179881800187, 85.80780507572961824, -3.936430718245989002 ) ) ;
#54016 = CARTESIAN_POINT ( 'NONE',  ( 2.035157376598824452, 28.68868534415484106, 7.964842623401179544 ) ) ;
#54017 = CARTESIAN_POINT ( 'NONE',  ( 0.5774900079438590739, 7.647018677488171434, -5.440088680355550821 ) ) ;
#54018 = CARTESIAN_POINT ( 'NONE',  ( 18.52753015748618282, 43.92559781766745175, -4.923371831947291888 ) ) ;
#54019 = CARTESIAN_POINT ( 'NONE',  ( 17.39651004071838614, 42.93575266056826933, 6.500000000000032863 ) ) ;
#54020 = CARTESIAN_POINT ( 'NONE',  ( 5.076628168052704559, 20.17559781766745175, -8.527530157486179263 ) ) ;
#54021 = PRESENTATION_STYLE_ASSIGNMENT (( #62006 ) ) ;
#54022 = CARTESIAN_POINT ( 'NONE',  ( -9.846743663894594434, 31.00893115100078390, 3.469446951953614189E-15 ) ) ;
#54023 = ORIENTED_EDGE ( 'NONE', *, *, #48685, .F. ) ;
#54024 = VERTEX_POINT ( 'NONE', #33157 ) ;
#54025 = CARTESIAN_POINT ( 'NONE',  ( 14.92337183194729633, 57.67559781766745886, 8.527530157486181039 ) ) ;
#54027 = CARTESIAN_POINT ( 'NONE',  ( 4.559911319644449179, 42.23035201082151247, -9.422509992056141925 ) ) ;
#54026 = CARTESIAN_POINT ( 'NONE',  ( 7.084665262690076126, 29.10535201082150181, 10.88017736071109987 ) ) ;
#54028 = CARTESIAN_POINT ( 'NONE',  ( -2.816281873526473856, 34.12363466993042493, 9.499525473075851096E-16 ) ) ;
#54029 = CARTESIAN_POINT ( 'NONE',  ( -0.3689425029237881626, 17.42874883491397142, 10.36894250292379027 ) ) ;
#54030 = EDGE_CURVE ( 'NONE', #34483, #105, #88707, .T. ) ;
#54031 =( BOUNDED_SURFACE ( )  B_SPLINE_SURFACE ( 1, 2, ( 
 ( #51013, #26540, #56554, #94545, #12524, #95540, #42533, #87048, #34029, #18559, #27030, #11054, #95031, #57529, #87538, #80536, #43026, #50033, #49528, #73017, #80035, #35014, #96037, #58012, #97531, #98529, #90481, #98025, #29982, #67505, #29479, #13516, #59988, #75493, #37009, #22018, #52492, #7005, #82999, #6022, #60487, #52011, #14517, #90976, #37510, #6501, #21514, #44986, #7514, #68003, #74499, #22509, #74999, #82500, #14018, #52981, #44498, #38005, #83984, #28990, #83495, #43997, #15014, #45483, #36518, #75985, #68498, #25, #30472, #15509, #60973, #91485, #67010, #23006, #53474, #89513, #45991, #5532, #66514, #36012, #59500, #97041, #28516, #59010, #21023, #82004, #51512, #89998, #93448, #15983, #38984, #69476, #31942, #78443, #77450, #61958, #25471, #46470, #92946, #32936, #9958, #46956, #40464, #24481, #76966, #24973, #31456, #1983, #1489, #62443, #8478, #85961, #54944, #85461, #16973, #7994, #9459, #61466, #54456, #32449, #17470, #47937, #55458, #47453, #62945, #91973, #92457, #30969, #84964, #23502, #522, #70963, #70461, #995, #23985, #2482, #93944, #63437, #55953, #8964, #86453, #16480, #53973, #17951, #76480, #39480, #38492, #77952, #39960, #68987, #69970, #84482, #79916, #3448, #19911, #73394, #18443, #63916, #11425, #40956, #78938, #3935, #87421, #80424, #34404, #48925, #42424, #27897, #64893, #49913, #88411, #96423, #11920, #10448, #79437, #10935, #71927, #26418, #80912, #12406, #95926, #95421, #58386, #27406, #88904, #33417, #18938, #4922, #33905, #72905, #71453, #41459, #64413, #94919, #48437, #2967, #65400, #94427, #72408, #49415, #41945, #4438, #35400, #65893, #25942, #56444, #26917, #86930, #34904, #57414, #87907, #56919, #42913, #19421, #57897, #50402, #90363, #21401, #50901, #36398, #81885, #13397, #89393, #60864, #66891, #98905, #44869, #66389, #52871, #20909, #43395, #60368, #14398, #59379, #20415, #6381, #59875, #37400, #43880, #28877, #51895, #74376, #90865, #45370, #51398, #35894, #82377, #12898, #81396, #74883, #89883, #52378, #36897, #5903, #75372, #30356, #67385, #21901, #22395, #68385, #82882, #73893, #97410, #13899, #44384, #97914, #83377, #14899, #67888, #29374, #5424, #98410, #96922, #28400, #6887, #75874, #29866, #7395, #58895, #37893, #23383, #61356, #32817, #91364, #9343, #40347, #16362, #92351, #84855, #47330, #78325, #47825, #70849, #22890, #23878, #7884, #77831, #54342, #46843, #884, #24852, #15878, #31344, #38376, #62331, #77338, #53362, #8364, #53868, #84378, #91865, #83869, #38872, #2362, #16854, #68877, #93331, #61845, #55334, #39364, #46362, #39846, #76850, #70352, #8850 ),
 ( #92838, #69859, #69363, #1380, #85842, #31835, #24367, #54829, #85342, #1870, #32327, #62831, #17356, #9845, #15393, #45879, #76369, #30859, #407, #64291, #63802, #3823, #79316, #41345, #34278, #10825, #65275, #42798, #86823, #71815, #2854, #87788, #94803, #94308, #64779, #11797, #26305, #56805, #73282, #19788, #26799, #33308, #19304, #57294, #48317, #87301, #95295, #25354, #50277, #71334, #55837, #63314, #27284, #93824, #40833, #49790, #72293, #80298, #25831, #56329, #18327, #18821, #95804, #49302, #48808, #12289, #3321, #79804, #80793, #86331, #4313, #11306, #4805, #33785, #42304, #34787, #41826, #57782, #72776, #88289, #17835, #78825, #10335, #73772, #29261, #50790, #83260, #66267, #6770, #96304, #14282, #74256, #82257, #28768, #5786, #52264, #13775, #67771, #28278, #27780, #37281, #44755, #97294, #44260, #22279, #5301, #75751, #43766, #58265, #35280, #36276, #52752, #74766, #21784, #89762, #20788, #21279, #89276, #51775, #35778, #6274, #58773, #59757, #36780, #59261, #90252, #67271, #97799, #43277, #82760, #75257, #66773, #98292, #29747, #60256, #90750, #96802, #14784, #81762, #45254, #65774, #88781, #20291, #51278, #81280, #12779, #13275, #76253, #92236, #76734, #62215, #69738, #91243, #772, #8730, #68271, #62707, #15277, #98791, #7273, #70232, #37774, #83754, #77225, #16244, #24246, #45758, #68756, #287, #61721, #9228, #8251, #91746, #55208, #7769, #23763, #93207, #30238, #47214, #54225, #47714, #23266, #39248, #77715, #30733, #1751, #54712, #92721, #46726, #60742, #38263, #61240, #1264, #22767, #85723, #53742, #39737, #53248, #85234, #46249, #84740, #31224, #38750, #16737, #31719, #32206, #84261, #15763, #24730, #17236, #69252, #56689, #65160, #48198, #19675, #86706, #70729, #78209, #48691, #95678, #26197, #64657, #33674, #63686, #64171, #33193, #94692, #17725, #49187, #71216, #72177, #87182, #71698, #3706, #41221, #3212, #86214, #18703, #79689, #10706, #11187, #41707, #34167, #95170, #78711, #26677, #25719, #57172, #87669, #19182, #79194, #94189, #49663, #80173, #11684, #10222, #42194, #72658, #56211, #18212, #4193, #34663, #27164, #57664, #2737, #88161, #40711, #9721, #40220, #2244, #32702, #63198, #93703, #25238, #55719, #8013, #13647, #20164, #13151, #58653, #84005, #73646, #89153, #96176, #21158, #51159, #80673, #66145, #12661, #43160, #50668, #91991, #96678, #30986, #74643, #27659, #53495, #20663, #15529, #97180, #81156, #45, #5175, #6153, #74135, #5670, #88656, #60993, #36152, #59138, #89646, #12168, #82138, #35154, #28157, #36658, #91504, #23024, #30494, #28648, #68515, #65653, #35660, #4692, #81643 ) ),
 .UNSPECIFIED., .F., .F., .F. ) 
 B_SPLINE_SURFACE_WITH_KNOTS ( ( 2, 2 ),
 ( 3, 2, 2, 2, 2, 2, 2, 2, 2, 2, 2, 2, 2, 2, 2, 2, 2, 2, 2, 2, 2, 2, 2, 2, 2, 2, 2, 2, 2, 2, 2, 2, 2, 2, 2, 2, 2, 2, 2, 2, 2, 2, 2, 2, 2, 2, 2, 2, 2, 2, 2, 2, 2, 2, 2, 2, 2, 2, 2, 2, 2, 2, 2, 2, 2, 2, 2, 2, 2, 2, 2, 2, 2, 2, 2, 2, 2, 2, 2, 2, 2, 2, 2, 2, 2, 2, 2, 2, 2, 2, 2, 2, 2, 2, 2, 2, 2, 2, 2, 2, 2, 2, 2, 2, 2, 2, 2, 2, 2, 2, 2, 2, 2, 2, 2, 2, 2, 2, 2, 2, 2, 2, 2, 2, 2, 2, 2, 2, 2, 2, 2, 2, 2, 2, 2, 2, 2, 2, 2, 2, 2, 2, 2, 2, 2, 2, 2, 2, 2, 2, 2, 2, 2, 2, 2, 2, 2, 2, 2, 2, 2, 2, 3 ),
 ( 0.000000000000000000, 1.000000000000000000 ),
 ( 0.000000000000000000, 0.005952380952380952051, 0.01190476190476190410, 0.01785714285714285615, 0.02380952380952380820, 0.02976190476190476025, 0.03571428571428571230, 0.04166666666666666435, 0.04761904761904761640, 0.05357142857142856845, 0.05952380952380952051, 0.06547619047619047949, 0.07142857142857142461, 0.07738095238095238360, 0.08333333333333332871, 0.08928571428571428770, 0.09523809523809523281, 0.1011904761904761918, 0.1071428571428571369, 0.1130952380952380959, 0.1190476190476190410, 0.1250000000000000000, 0.1309523809523809590, 0.1369047619047619180, 0.1428571428571428492, 0.1488095238095238082, 0.1547619047619047672, 0.1607142857142857262, 0.1666666666666666574, 0.1726190476190476164, 0.1785714285714285754, 0.1845238095238095344, 0.1904761904761904656, 0.1964285714285714246, 0.2023809523809523836, 0.2083333333333333426, 0.2142857142857142738, 0.2202380952380952328, 0.2261904761904761918, 0.2321428571428571508, 0.2380952380952380820, 0.2440476190476190410, 0.2500000000000000000, 0.2559523809523809312, 0.2619047619047619180, 0.2678571428571428492, 0.2738095238095238360, 0.2797619047619047672, 0.2857142857142856984, 0.2916666666666666852, 0.2976190476190476164, 0.3035714285714285476, 0.3095238095238095344, 0.3154761904761904656, 0.3214285714285714524, 0.3273809523809523836, 0.3333333333333333148, 0.3392857142857143016, 0.3452380952380952328, 0.3511904761904761640, 0.3571428571428571508, 0.3630952380952380820, 0.3690476190476190688, 0.3750000000000000000, 0.3809523809523809312, 0.3869047619047619180, 0.3928571428571428492, 0.3988095238095238360, 0.4047619047619047672, 0.4107142857142856984, 0.4166666666666666852, 0.4226190476190476164, 0.4285714285714285476, 0.4345238095238095344, 0.4404761904761904656, 0.4464285714285714524, 0.4523809523809523836, 0.4583333333333333148, 0.4642857142857143016, 0.4702380952380952328, 0.4761904761904761640, 0.4821428571428571508, 0.4880952380952380820, 0.4940476190476190688, 0.5000000000000000000, 0.5059523809523809312, 0.5119047619047618625, 0.5178571428571429047, 0.5238095238095238360, 0.5297619047619047672, 0.5357142857142856984, 0.5416666666666666297, 0.5476190476190476719, 0.5535714285714286031, 0.5595238095238095344, 0.5654761904761904656, 0.5714285714285713969, 0.5773809523809523281, 0.5833333333333333703, 0.5892857142857143016, 0.5952380952380952328, 0.6011904761904761640, 0.6071428571428570953, 0.6130952380952381375, 0.6190476190476190688, 0.6250000000000000000, 0.6309523809523809312, 0.6369047619047618625, 0.6428571428571429047, 0.6488095238095238360, 0.6547619047619047672, 0.6607142857142856984, 0.6666666666666666297, 0.6726190476190476719, 0.6785714285714286031, 0.6845238095238095344, 0.6904761904761904656, 0.6964285714285713969, 0.7023809523809523281, 0.7083333333333333703, 0.7142857142857143016, 0.7202380952380952328, 0.7261904761904761640, 0.7321428571428570953, 0.7380952380952381375, 0.7440476190476190688, 0.7500000000000000000, 0.7559523809523809312, 0.7619047619047618625, 0.7678571428571429047, 0.7738095238095238360, 0.7797619047619047672, 0.7857142857142856984, 0.7916666666666666297, 0.7976190476190476719, 0.8035714285714286031, 0.8095238095238095344, 0.8154761904761904656, 0.8214285714285713969, 0.8273809523809523281, 0.8333333333333333703, 0.8392857142857143016, 0.8452380952380952328, 0.8511904761904761640, 0.8571428571428570953, 0.8630952380952381375, 0.8690476190476190688, 0.8750000000000000000, 0.8809523809523809312, 0.8869047619047618625, 0.8928571428571429047, 0.8988095238095238360, 0.9047619047619047672, 0.9107142857142856984, 0.9166666666666666297, 0.9226190476190476719, 0.9285714285714286031, 0.9345238095238095344, 0.9404761904761904656, 0.9464285714285713969, 0.9523809523809523281, 0.9583333333333333703, 0.9642857142857143016 ),
 .UNSPECIFIED. ) 
 GEOMETRIC_REPRESENTATION_ITEM ( )  RATIONAL_B_SPLINE_SURFACE ( (
 ( 1.000000000000000000, 0.9659258262890683122, 1.000000000000000000, 0.9659258262890683122, 1.000000000000000000, 0.9659258262890683122, 1.000000000000000000, 0.9659258262890683122, 1.000000000000000000, 0.9659258262890683122, 1.000000000000000000, 0.9659258262890683122, 1.000000000000000000, 0.9659258262890683122, 1.000000000000000000, 0.9659258262890683122, 1.000000000000000000, 0.9659258262890683122, 1.000000000000000000, 0.9659258262890683122, 1.000000000000000000, 0.9659258262890683122, 1.000000000000000000, 0.9659258262890683122, 1.000000000000000000, 0.9659258262890683122, 1.000000000000000000, 0.9659258262890683122, 1.000000000000000000, 0.9659258262890683122, 1.000000000000000000, 0.9659258262890683122, 1.000000000000000000, 0.9659258262890683122, 1.000000000000000000, 0.9659258262890683122, 1.000000000000000000, 0.9659258262890683122, 1.000000000000000000, 0.9659258262890683122, 1.000000000000000000, 0.9659258262890683122, 1.000000000000000000, 0.9659258262890683122, 1.000000000000000000, 0.9659258262890683122, 1.000000000000000000, 0.9659258262890683122, 1.000000000000000000, 0.9659258262890683122, 1.000000000000000000, 0.9659258262890683122, 1.000000000000000000, 0.9659258262890683122, 1.000000000000000000, 0.9659258262890683122, 1.000000000000000000, 0.9659258262890683122, 1.000000000000000000, 0.9659258262890683122, 1.000000000000000000, 0.9659258262890683122, 1.000000000000000000, 0.9659258262890683122, 1.000000000000000000, 0.9659258262890683122, 1.000000000000000000, 0.9659258262890683122, 1.000000000000000000, 0.9659258262890683122, 1.000000000000000000, 0.9659258262890683122, 1.000000000000000000, 0.9659258262890683122, 1.000000000000000000, 0.9659258262890683122, 1.000000000000000000, 0.9659258262890683122, 1.000000000000000000, 0.9659258262890683122, 1.000000000000000000, 0.9659258262890683122, 1.000000000000000000, 0.9659258262890683122, 1.000000000000000000, 0.9659258262890683122, 1.000000000000000000, 0.9659258262890683122, 1.000000000000000000, 0.9659258262890683122, 1.000000000000000000, 0.9659258262890683122, 1.000000000000000000, 0.9659258262890683122, 1.000000000000000000, 0.9659258262890683122, 1.000000000000000000, 0.9659258262890683122, 1.000000000000000000, 0.9659258262890683122, 1.000000000000000000, 0.9659258262890683122, 1.000000000000000000, 0.9659258262890683122, 1.000000000000000000, 0.9659258262890683122, 1.000000000000000000, 0.9659258262890683122, 1.000000000000000000, 0.9659258262890683122, 1.000000000000000000, 0.9659258262890683122, 1.000000000000000000, 0.9659258262890683122, 1.000000000000000000, 0.9659258262890683122, 1.000000000000000000, 0.9659258262890683122, 1.000000000000000000, 0.9659258262890683122, 1.000000000000000000, 0.9659258262890683122, 1.000000000000000000, 0.9659258262890683122, 1.000000000000000000, 0.9659258262890683122, 1.000000000000000000, 0.9659258262890683122, 1.000000000000000000, 0.9659258262890683122, 1.000000000000000000, 0.9659258262890683122, 1.000000000000000000, 0.9659258262890683122, 1.000000000000000000, 0.9659258262890683122, 1.000000000000000000, 0.9659258262890683122, 1.000000000000000000, 0.9659258262890683122, 1.000000000000000000, 0.9659258262890683122, 1.000000000000000000, 0.9659258262890683122, 1.000000000000000000, 0.9659258262890683122, 1.000000000000000000, 0.9659258262890683122, 1.000000000000000000, 0.9659258262890683122, 1.000000000000000000, 0.9659258262890683122, 1.000000000000000000, 0.9659258262890683122, 1.000000000000000000, 0.9659258262890683122, 1.000000000000000000, 0.9659258262890683122, 1.000000000000000000, 0.9659258262890683122, 1.000000000000000000, 0.9659258262890683122, 1.000000000000000000, 0.9659258262890683122, 1.000000000000000000, 0.9659258262890683122, 1.000000000000000000, 0.9659258262890683122, 1.000000000000000000, 0.9659258262890683122, 1.000000000000000000, 0.9659258262890683122, 1.000000000000000000, 0.9659258262890683122, 1.000000000000000000, 0.9659258262890683122, 1.000000000000000000, 0.9659258262890683122, 1.000000000000000000, 0.9659258262890683122, 1.000000000000000000, 0.9659258262890683122, 1.000000000000000000, 0.9659258262890683122, 1.000000000000000000, 0.9659258262890683122, 1.000000000000000000, 0.9659258262890683122, 1.000000000000000000, 0.9659258262890683122, 1.000000000000000000, 0.9659258262890683122, 1.000000000000000000, 0.9659258262890683122, 1.000000000000000000, 0.9659258262890683122, 1.000000000000000000, 0.9659258262890683122, 1.000000000000000000, 0.9659258262890683122, 1.000000000000000000, 0.9659258262890683122, 1.000000000000000000, 0.9659258262890683122, 1.000000000000000000, 0.9659258262890683122, 1.000000000000000000, 0.9659258262890683122, 1.000000000000000000, 0.9659258262890683122, 1.000000000000000000, 0.9659258262890683122, 1.000000000000000000, 0.9659258262890683122, 1.000000000000000000, 0.9659258262890683122, 1.000000000000000000, 0.9659258262890683122, 1.000000000000000000, 0.9659258262890683122, 1.000000000000000000, 0.9659258262890683122, 1.000000000000000000, 0.9659258262890683122, 1.000000000000000000, 0.9659258262890683122, 1.000000000000000000, 0.9659258262890683122, 1.000000000000000000, 0.9659258262890683122, 1.000000000000000000, 0.9659258262890683122, 1.000000000000000000, 0.9659258262890683122, 1.000000000000000000, 0.9659258262890683122, 1.000000000000000000, 0.9659258262890683122, 1.000000000000000000, 0.9659258262890683122, 1.000000000000000000, 0.9659258262890683122, 1.000000000000000000, 0.9659258262890683122, 1.000000000000000000, 0.9659258262890683122, 1.000000000000000000, 0.9659258262890683122, 1.000000000000000000, 0.9659258262890683122, 1.000000000000000000, 0.9659258262890683122, 1.000000000000000000, 0.9659258262890683122, 1.000000000000000000, 0.9659258262890683122, 1.000000000000000000, 0.9659258262890683122, 1.000000000000000000, 0.9659258262890683122, 1.000000000000000000, 0.9659258262890683122, 1.000000000000000000, 0.9659258262890683122, 1.000000000000000000, 0.9659258262890683122, 1.000000000000000000, 0.9659258262890683122, 1.000000000000000000, 0.9659258262890683122, 1.000000000000000000, 0.9659258262890683122, 1.000000000000000000, 0.9659258262890683122, 1.000000000000000000, 0.9659258262890683122, 1.000000000000000000, 0.9659258262890683122, 1.000000000000000000, 0.9659258262890683122, 1.000000000000000000, 0.9659258262890683122, 1.000000000000000000, 0.9659258262890683122, 1.000000000000000000, 0.9659258262890683122, 1.000000000000000000, 0.9659258262890683122, 1.000000000000000000, 0.9659258262890683122, 1.000000000000000000, 0.9659258262890683122, 1.000000000000000000, 0.9659258262890683122, 1.000000000000000000, 0.9659258262890683122, 1.000000000000000000, 0.9659258262890683122, 1.000000000000000000, 0.9659258262890683122, 1.000000000000000000, 0.9659258262890683122, 1.000000000000000000, 0.9659258262890683122, 1.000000000000000000, 0.9659258262890683122, 1.000000000000000000, 0.9659258262890683122, 1.000000000000000000, 0.9659258262890683122, 1.000000000000000000, 0.9659258262890683122, 1.000000000000000000, 0.9659258262890683122, 1.000000000000000000, 0.9659258262890683122, 1.000000000000000000, 0.9659258262890683122, 1.000000000000000000, 0.9659258262890683122, 1.000000000000000000, 0.9659258262890683122, 1.000000000000000000, 0.9659258262890683122, 1.000000000000000000),
 ( 1.000000000000000000, 0.9659258262890683122, 1.000000000000000000, 0.9659258262890683122, 1.000000000000000000, 0.9659258262890683122, 1.000000000000000000, 0.9659258262890683122, 1.000000000000000000, 0.9659258262890683122, 1.000000000000000000, 0.9659258262890683122, 1.000000000000000000, 0.9659258262890683122, 1.000000000000000000, 0.9659258262890683122, 1.000000000000000000, 0.9659258262890683122, 1.000000000000000000, 0.9659258262890683122, 1.000000000000000000, 0.9659258262890683122, 1.000000000000000000, 0.9659258262890683122, 1.000000000000000000, 0.9659258262890683122, 1.000000000000000000, 0.9659258262890683122, 1.000000000000000000, 0.9659258262890683122, 1.000000000000000000, 0.9659258262890683122, 1.000000000000000000, 0.9659258262890683122, 1.000000000000000000, 0.9659258262890683122, 1.000000000000000000, 0.9659258262890683122, 1.000000000000000000, 0.9659258262890683122, 1.000000000000000000, 0.9659258262890683122, 1.000000000000000000, 0.9659258262890683122, 1.000000000000000000, 0.9659258262890683122, 1.000000000000000000, 0.9659258262890683122, 1.000000000000000000, 0.9659258262890683122, 1.000000000000000000, 0.9659258262890683122, 1.000000000000000000, 0.9659258262890683122, 1.000000000000000000, 0.9659258262890683122, 1.000000000000000000, 0.9659258262890683122, 1.000000000000000000, 0.9659258262890683122, 1.000000000000000000, 0.9659258262890683122, 1.000000000000000000, 0.9659258262890683122, 1.000000000000000000, 0.9659258262890683122, 1.000000000000000000, 0.9659258262890683122, 1.000000000000000000, 0.9659258262890683122, 1.000000000000000000, 0.9659258262890683122, 1.000000000000000000, 0.9659258262890683122, 1.000000000000000000, 0.9659258262890683122, 1.000000000000000000, 0.9659258262890683122, 1.000000000000000000, 0.9659258262890683122, 1.000000000000000000, 0.9659258262890683122, 1.000000000000000000, 0.9659258262890683122, 1.000000000000000000, 0.9659258262890683122, 1.000000000000000000, 0.9659258262890683122, 1.000000000000000000, 0.9659258262890683122, 1.000000000000000000, 0.9659258262890683122, 1.000000000000000000, 0.9659258262890683122, 1.000000000000000000, 0.9659258262890683122, 1.000000000000000000, 0.9659258262890683122, 1.000000000000000000, 0.9659258262890683122, 1.000000000000000000, 0.9659258262890683122, 1.000000000000000000, 0.9659258262890683122, 1.000000000000000000, 0.9659258262890683122, 1.000000000000000000, 0.9659258262890683122, 1.000000000000000000, 0.9659258262890683122, 1.000000000000000000, 0.9659258262890683122, 1.000000000000000000, 0.9659258262890683122, 1.000000000000000000, 0.9659258262890683122, 1.000000000000000000, 0.9659258262890683122, 1.000000000000000000, 0.9659258262890683122, 1.000000000000000000, 0.9659258262890683122, 1.000000000000000000, 0.9659258262890683122, 1.000000000000000000, 0.9659258262890683122, 1.000000000000000000, 0.9659258262890683122, 1.000000000000000000, 0.9659258262890683122, 1.000000000000000000, 0.9659258262890683122, 1.000000000000000000, 0.9659258262890683122, 1.000000000000000000, 0.9659258262890683122, 1.000000000000000000, 0.9659258262890683122, 1.000000000000000000, 0.9659258262890683122, 1.000000000000000000, 0.9659258262890683122, 1.000000000000000000, 0.9659258262890683122, 1.000000000000000000, 0.9659258262890683122, 1.000000000000000000, 0.9659258262890683122, 1.000000000000000000, 0.9659258262890683122, 1.000000000000000000, 0.9659258262890683122, 1.000000000000000000, 0.9659258262890683122, 1.000000000000000000, 0.9659258262890683122, 1.000000000000000000, 0.9659258262890683122, 1.000000000000000000, 0.9659258262890683122, 1.000000000000000000, 0.9659258262890683122, 1.000000000000000000, 0.9659258262890683122, 1.000000000000000000, 0.9659258262890683122, 1.000000000000000000, 0.9659258262890683122, 1.000000000000000000, 0.9659258262890683122, 1.000000000000000000, 0.9659258262890683122, 1.000000000000000000, 0.9659258262890683122, 1.000000000000000000, 0.9659258262890683122, 1.000000000000000000, 0.9659258262890683122, 1.000000000000000000, 0.9659258262890683122, 1.000000000000000000, 0.9659258262890683122, 1.000000000000000000, 0.9659258262890683122, 1.000000000000000000, 0.9659258262890683122, 1.000000000000000000, 0.9659258262890683122, 1.000000000000000000, 0.9659258262890683122, 1.000000000000000000, 0.9659258262890683122, 1.000000000000000000, 0.9659258262890683122, 1.000000000000000000, 0.9659258262890683122, 1.000000000000000000, 0.9659258262890683122, 1.000000000000000000, 0.9659258262890683122, 1.000000000000000000, 0.9659258262890683122, 1.000000000000000000, 0.9659258262890683122, 1.000000000000000000, 0.9659258262890683122, 1.000000000000000000, 0.9659258262890683122, 1.000000000000000000, 0.9659258262890683122, 1.000000000000000000, 0.9659258262890683122, 1.000000000000000000, 0.9659258262890683122, 1.000000000000000000, 0.9659258262890683122, 1.000000000000000000, 0.9659258262890683122, 1.000000000000000000, 0.9659258262890683122, 1.000000000000000000, 0.9659258262890683122, 1.000000000000000000, 0.9659258262890683122, 1.000000000000000000, 0.9659258262890683122, 1.000000000000000000, 0.9659258262890683122, 1.000000000000000000, 0.9659258262890683122, 1.000000000000000000, 0.9659258262890683122, 1.000000000000000000, 0.9659258262890683122, 1.000000000000000000, 0.9659258262890683122, 1.000000000000000000, 0.9659258262890683122, 1.000000000000000000, 0.9659258262890683122, 1.000000000000000000, 0.9659258262890683122, 1.000000000000000000, 0.9659258262890683122, 1.000000000000000000, 0.9659258262890683122, 1.000000000000000000, 0.9659258262890683122, 1.000000000000000000, 0.9659258262890683122, 1.000000000000000000, 0.9659258262890683122, 1.000000000000000000, 0.9659258262890683122, 1.000000000000000000, 0.9659258262890683122, 1.000000000000000000, 0.9659258262890683122, 1.000000000000000000, 0.9659258262890683122, 1.000000000000000000, 0.9659258262890683122, 1.000000000000000000, 0.9659258262890683122, 1.000000000000000000, 0.9659258262890683122, 1.000000000000000000, 0.9659258262890683122, 1.000000000000000000, 0.9659258262890683122, 1.000000000000000000, 0.9659258262890683122, 1.000000000000000000, 0.9659258262890683122, 1.000000000000000000, 0.9659258262890683122, 1.000000000000000000, 0.9659258262890683122, 1.000000000000000000, 0.9659258262890683122, 1.000000000000000000, 0.9659258262890683122, 1.000000000000000000, 0.9659258262890683122, 1.000000000000000000, 0.9659258262890683122, 1.000000000000000000, 0.9659258262890683122, 1.000000000000000000, 0.9659258262890683122, 1.000000000000000000, 0.9659258262890683122, 1.000000000000000000, 0.9659258262890683122, 1.000000000000000000, 0.9659258262890683122, 1.000000000000000000, 0.9659258262890683122, 1.000000000000000000, 0.9659258262890683122, 1.000000000000000000, 0.9659258262890683122, 1.000000000000000000, 0.9659258262890683122, 1.000000000000000000, 0.9659258262890683122, 1.000000000000000000, 0.9659258262890683122, 1.000000000000000000, 0.9659258262890683122, 1.000000000000000000, 0.9659258262890683122, 1.000000000000000000, 0.9659258262890683122, 1.000000000000000000, 0.9659258262890683122, 1.000000000000000000, 0.9659258262890683122, 1.000000000000000000, 0.9659258262890683122, 1.000000000000000000, 0.9659258262890683122, 1.000000000000000000, 0.9659258262890683122, 1.000000000000000000) ) ) 
 REPRESENTATION_ITEM ( '' )  SURFACE ( )  );
#54032 = CARTESIAN_POINT ( 'NONE',  ( -1.099225684535947600, 44.54030133659708923, 6.408140936763237150 ) ) ;
#54033 = ORIENTED_EDGE ( 'NONE', *, *, #70683, .F. ) ;
#54034 = CARTESIAN_POINT ( 'NONE',  ( 10.00000000000000178, 47.25893115100078745, 9.846743663894594434 ) ) ;
#54035 = CARTESIAN_POINT ( 'NONE',  ( 20.88017736071110875, 20.77201867748816611, -2.915334737309920765 ) ) ;
#54036 = ORIENTED_EDGE ( 'NONE', *, *, #19580, .T. ) ;
#54037 = CARTESIAN_POINT ( 'NONE',  ( 19.42250999205614548, 10.98035201082150536, -5.440088680355545492 ) ) ;
#54038 = EDGE_CURVE ( 'NONE', #15924, #82423, #53208, .T. ) ;
#54039 = VERTEX_POINT ( 'NONE', #86671 ) ;
#54040 = CARTESIAN_POINT ( 'NONE',  ( 20.88017736071110164, 55.35535201082149825, 2.915334737309930979 ) ) ;
#54041 = CARTESIAN_POINT ( 'NONE',  ( 0.5774900079438607392, 68.48035201082150536, 5.440088680355550821 ) ) ;
#54042 = CARTESIAN_POINT ( 'NONE',  ( 0.5774900079438607392, 68.48035201082150536, 5.440088680355550821 ) ) ;
#54043 = CARTESIAN_POINT ( 'NONE',  ( 0.1532563361054100626, 15.80059781766745353, -2.638427012816831230 ) ) ;
#54044 = CARTESIAN_POINT ( 'NONE',  ( 15.44008868035555793, 61.39701867748817676, -9.422509992056140149 ) ) ;
#54045 = CARTESIAN_POINT ( 'NONE',  ( -4.391700990647259495, 0.2306972965111845908, 14.28114200970186687 ) ) ;
#54046 = CARTESIAN_POINT ( 'NONE',  ( -46.94000000000001194, 102.4380508258080198, 6.413016458746108484 ) ) ;
#54048 = STYLED_ITEM ( 'NONE', ( #69891 ), #16638 ) ;
#54047 = CARTESIAN_POINT ( 'NONE',  ( 1.472469842513823179, 0.5922644843341181575, -4.923371831947296329 ) ) ;
#54049 = CARTESIAN_POINT ( 'NONE',  ( 2.791683348922237240, 40.38393115100078035, -7.208316651077763204 ) ) ;
#54050 = EDGE_LOOP ( 'NONE', ( #31591, #70075, #38651, #7519 ) ) ;
#54051 = CARTESIAN_POINT ( 'NONE',  ( 10.00000000000000000, 64.75893115100078035, -9.846743663894594434 ) ) ;
#54052 = PLANE ( 'NONE',  #88025 ) ;
#54053 = CARTESIAN_POINT ( 'NONE',  ( 13.79529636645031943, 20.34541550158063572, -14.16423886937409904 ) ) ;
#54054 = CARTESIAN_POINT ( 'NONE',  ( -2.393480905993287777, 14.49999999999999112, 14.80781041047755409 ) ) ;
#54055 = CARTESIAN_POINT ( 'NONE',  ( 20.25388882277768232, 70.00000000000000000, 6.092555545976966691 ) ) ;
#54056 = CARTESIAN_POINT ( 'NONE',  ( 20.88017736071110164, 20.35535201082150891, 2.915334737309930979 ) ) ;
#54057 = DIRECTION ( 'NONE',  ( 1.000000000000000000, 0.000000000000000000, 0.000000000000000000 ) ) ;
#54058 = ORIENTED_EDGE ( 'NONE', *, *, #1205, .F. ) ;
#54059 = CARTESIAN_POINT ( 'NONE',  ( 0.1532563361054100626, 5.800597817667452638, -2.638427012816831230 ) ) ;
#54060 = CARTESIAN_POINT ( 'NONE',  ( 2.791683348922237240, 5.383931151000785675, -7.208316651077763204 ) ) ;
#54061 = CARTESIAN_POINT ( 'NONE',  ( 0.6178305044545838731, 29.74863466993042138, 9.382169495545420901 ) ) ;
#54062 = CARTESIAN_POINT ( 'NONE',  ( 7.361572987183169658, 19.96726448433411960, -9.846743663894592657 ) ) ;
#54063 = EDGE_CURVE ( 'NONE', #61157, #57318, #17760, .T. ) ;
#54064 = CARTESIAN_POINT ( 'NONE',  ( 16.40814093676324603, 12.45696800326375353, -11.09922568453594671 ) ) ;
#54065 = VECTOR ( 'NONE', #98447, 1000.000000000000000 ) ;
#54066 = CARTESIAN_POINT ( 'NONE',  ( 3.640395162852214650, 89.00000000000000000, -12.00000000000000000 ) ) ;
#54067 = CARTESIAN_POINT ( 'NONE',  ( 10.00000000000000178, 2.258931151000784787, 9.846743663894594434 ) ) ;
#54068 = ORIENTED_EDGE ( 'NONE', *, *, #91988, .F. ) ;
#54069 = EDGE_CURVE ( 'NONE', #91634, #48230, #62671, .T. ) ;
#54070 = ORIENTED_EDGE ( 'NONE', *, *, #5113, .T. ) ;
#54071 = CARTESIAN_POINT ( 'NONE',  ( 0.5774900079438607392, 18.48035201082150536, 5.440088680355550821 ) ) ;
#54072 = CARTESIAN_POINT ( 'NONE',  ( 13.79529636645030344, 13.26208216824729824, 14.16423886937410614 ) ) ;
#54073 = CARTESIAN_POINT ( 'NONE',  ( 0.1532563361054082862, 36.21726448433410894, 2.638427012816831674 ) ) ;
#54074 = CARTESIAN_POINT ( 'NONE',  ( 0.5774900079438607392, 63.48035201082149825, 5.440088680355550821 ) ) ;
#54076 = CARTESIAN_POINT ( 'NONE',  ( -13.82671409943298357, 15.00000000000000000, 3.447387012295131115 ) ) ;
#54075 = CARTESIAN_POINT ( 'NONE',  ( 3.591859063236763294, 48.29030133659708923, -11.09922568453595026 ) ) ;
#54077 = CARTESIAN_POINT ( 'NONE',  ( 2.035157376598824452, 28.68868534415484106, 7.964842623401179544 ) ) ;
#54078 = CARTESIAN_POINT ( 'NONE',  ( -3.749999999999988010, -5.564482262735336175E-16, -4.000000000000000000 ) ) ;
#54079 = CARTESIAN_POINT ( 'NONE',  ( 0.6178305044545818747, 13.49863466993041783, -9.382169495545419124 ) ) ;
#54080 = VECTOR ( 'NONE', #16178, 1000.000000000000000 ) ;
#54081 = CARTESIAN_POINT ( 'NONE',  ( 10.00000000000000000, 7.873634669930421381, -12.81628187352647608 ) ) ;
#54082 = CARTESIAN_POINT ( 'NONE',  ( 17.20831665107776587, 37.88393115100078745, 7.208316651077764980 ) ) ;
#54083 = CARTESIAN_POINT ( 'NONE',  ( 10.88017736071110519, 0.5636853441548448362, -2.602085213965210642E-15 ) ) ;
#54084 = CARTESIAN_POINT ( 'NONE',  ( -1.099225684535947600, 54.54030133659708923, 6.408140936763237150 ) ) ;
#54085 = EDGE_CURVE ( 'NONE', #12575, #14459, #74630, .T. ) ;
#54087 = CARTESIAN_POINT ( 'NONE',  ( 0.2751277870542909731, 62.28217586085237656, -6.499999999999992006 ) ) ;
#54086 = CARTESIAN_POINT ( 'NONE',  ( 15.44008868035555260, 54.73035201082150536, 9.422509992056143702 ) ) ;
#54088 =( LENGTH_UNIT ( ) NAMED_UNIT ( * ) SI_UNIT ( .MILLI., .METRE. ) );
#54089 = CARTESIAN_POINT ( 'NONE',  ( 19.42250999205614193, 40.14701867748817676, 5.440088680355555262 ) ) ;
#54090 = CARTESIAN_POINT ( 'NONE',  ( 19.42250999205614548, 50.98035201082151247, -5.440088680355545492 ) ) ;
#54091 = CARTESIAN_POINT ( 'NONE',  ( 19.72487221294571569, 60.71833443783937412, -6.499999999999990230 ) ) ;
#54092 = CARTESIAN_POINT ( 'NONE',  ( 12.91533473730992121, 64.52201867748817676, 10.88017736071110164 ) ) ;
#54093 = CARTESIAN_POINT ( 'NONE',  ( 12.63842701281683034, 57.46726448433411605, 9.846743663894596210 ) ) ;
#54095 = DIRECTION ( 'NONE',  ( 0.9832549075639526182, 0.000000000000000000, 0.1822355254921578793 ) ) ;
#54094 = CARTESIAN_POINT ( 'NONE',  ( 12.91533473730993009, 6.605352010821504471, -10.88017736071109987 ) ) ;
#54096 = CARTESIAN_POINT ( 'NONE',  ( 16.40814093676323893, 5.790301336597087456, 11.09922568453595026 ) ) ;
#54097 = ORIENTED_EDGE ( 'NONE', *, *, #30413, .F. ) ;
#54098 = CARTESIAN_POINT ( 'NONE',  ( 4.559911319644449179, 37.23035201082150536, -9.422509992056141925 ) ) ;
#54099 = EDGE_CURVE ( 'NONE', #73183, #25080, #47167, .T. ) ;
#54101 = CARTESIAN_POINT ( 'NONE',  ( -12.67147417979180979, 0.04962887043496414657, 7.555862176155415888 ) ) ;
#54100 = CARTESIAN_POINT ( 'NONE',  ( 13.43411237798105340, 10.58196800326375353, 12.81628187352647963 ) ) ;
#54102 = CARTESIAN_POINT ( 'NONE',  ( -0.8801773607110991993, 7.855352010821504471, -2.915334737309923874 ) ) ;
#54103 = CARTESIAN_POINT ( 'NONE',  ( 2.035157376598822676, 22.43868534415483396, -7.964842623401177768 ) ) ;
#54104 = CARTESIAN_POINT ( 'NONE',  ( -4.164238869374098151, 31.59541550158063927, -3.795296366450310543 ) ) ;
#54105 = CARTESIAN_POINT ( 'NONE',  ( 19.84674366389459266, 23.71726448433412315, -2.638427012816827677 ) ) ;
#54106 = CARTESIAN_POINT ( 'NONE',  ( 2.035157376598824452, 63.68868534415484106, 7.964842623401179544 ) ) ;
#54107 = SPHERICAL_SURFACE ( 'NONE', #84143, 0.2500000000000000000 ) ;
#54108 = CARTESIAN_POINT ( 'NONE',  ( 22.26659068614894466, 3.887082168247300906, 7.082119434687054849 ) ) ;
#54109 = UNCERTAINTY_MEASURE_WITH_UNIT (LENGTH_MEASURE( 1.000000000000000082E-05 ), #28045, 'distance_accuracy_value', 'NONE');
#54110 = SURFACE_STYLE_FILL_AREA ( #7659 ) ;
#54111 = CARTESIAN_POINT ( 'NONE',  ( 19.84674366389459266, 63.30059781766745886, 2.638427012816836559 ) ) ;
#54112 = VERTEX_POINT ( 'NONE', #54675 ) ;
#54113 = ORIENTED_EDGE ( 'NONE', *, *, #70780, .T. ) ;
#54114 = CARTESIAN_POINT ( 'NONE',  ( -4.164238869374099927, 32.01208216824730357, 3.795296366450308767 ) ) ;
#54115 = CARTESIAN_POINT ( 'NONE',  ( -2.266590686148945544, 42.22041550158063217, 7.082119434687048631 ) ) ;
#54116 = CARTESIAN_POINT ( 'NONE',  ( 12.63842701281683034, 7.467264484334118713, 9.846743663894596210 ) ) ;
#54117 = CARTESIAN_POINT ( 'NONE',  ( 21.09922568453595559, 7.040301336597086568, -6.408140936763230044 ) ) ;
#54118 = CARTESIAN_POINT ( 'NONE',  ( 5.076628168052704559, 60.17559781766745175, -8.527530157486179263 ) ) ;
#54119 = CARTESIAN_POINT ( 'NONE',  ( -11.30179204364036849, -57.06033576790798634, 3.750000000000000000 ) ) ;
#54121 = CARTESIAN_POINT ( 'NONE',  ( 3.591859063236761518, 24.95696800326375353, 11.09922568453594849 ) ) ;
#54120 = CARTESIAN_POINT ( 'NONE',  ( 10.00000000000000000, 56.81368534415484106, -10.88017736071110342 ) ) ;
#54122 = CARTESIAN_POINT ( 'NONE',  ( 6.204703633549690345, 32.84541550158063927, 14.16423886937410082 ) ) ;
#54123 = CARTESIAN_POINT ( 'NONE',  ( 12.91533473730993009, 16.60535201082150891, -10.88017736071109987 ) ) ;
#54124 = CARTESIAN_POINT ( 'NONE',  ( 0.5774900079438607392, 33.48035201082150536, 5.440088680355550821 ) ) ;
#54125 = LINE ( 'NONE', #86118, #61917 ) ;
#54126 = CARTESIAN_POINT ( 'NONE',  ( 0.5774900079438590739, 57.64701867748817676, -5.440088680355550821 ) ) ;
#54127 = CARTESIAN_POINT ( 'NONE',  ( 4.923371831947295441, -5.657735515665875070, -8.527530157486179263 ) ) ;
#54128 = ORIENTED_EDGE ( 'NONE', *, *, #14370, .F. ) ;
#54129 = FACE_BOUND ( 'NONE', #3865, .T. ) ;
#54130 = EDGE_LOOP ( 'NONE', ( #5935, #24995, #39405, #21821, #94354, #89656 ) ) ;
#54131 = FACE_OUTER_BOUND ( 'NONE', #64595, .T. ) ;
#54132 = EDGE_LOOP ( 'NONE', ( #32455, #14311, #61266, #56966 ) ) ;
#54133 = CARTESIAN_POINT ( 'NONE',  ( 2.917880565312950480, 5.970415501580634832, -12.26659068614894821 ) ) ;
#54135 = CARTESIAN_POINT ( 'NONE',  ( 10.00000000000000000, 60.55374883491397497, -14.16423886937410082 ) ) ;
#54134 = CARTESIAN_POINT ( 'NONE',  ( 22.26659068614894466, 58.88708216824729647, 7.082119434687054849 ) ) ;
#54137 = CARTESIAN_POINT ( 'NONE',  ( 19.84674366389459621, 63.50893115100078745, 7.409399052514197653E-17 ) ) ;
#54136 = CARTESIAN_POINT ( 'NONE',  ( 19.84674366389459266, 38.71726448433412315, -2.638427012816827677 ) ) ;
#54138 = CARTESIAN_POINT ( 'NONE',  ( 21.92686044187657401, 60.37045670184114954, -3.195792623639525765 ) ) ;
#54139 = AXIS2_PLACEMENT_3D ( 'NONE', #80585, #12079, #36063 ) ;
#54140 = CARTESIAN_POINT ( 'NONE',  ( 0.000000000000000000, 15.00000000000000000, 0.000000000000000000 ) ) ;
#54141 = EDGE_CURVE ( 'NONE', #51203, #60398, #10671, .T. ) ;
#54142 = PRESENTATION_LAYER_ASSIGNMENT (  '', '', ( #31790 ) ) ;
#54143 = CARTESIAN_POINT ( 'NONE',  ( -1.099225684535947600, 8.706968003263753531, -6.408140936763238038 ) ) ;
#54144 = CARTESIAN_POINT ( 'NONE',  ( 11.09922568453595026, 26.20696800326376064, 6.408140936763232709 ) ) ;
#54145 = EDGE_LOOP ( 'NONE', ( #60776, #71626, #3301, #86039 ) ) ;
#54146 = CARTESIAN_POINT ( 'NONE',  ( 13.79529636645031943, 50.34541550158064638, -14.16423886937409904 ) ) ;
#54147 = CARTESIAN_POINT ( 'NONE',  ( 10.00000000000000178, 38.05374883491396787, 14.16423886937410082 ) ) ;
#54148 = VERTEX_POINT ( 'NONE', #71666 ) ;
#54149 = CARTESIAN_POINT ( 'NONE',  ( -1.099225684535947600, 53.70696800326376064, -6.408140936763238038 ) ) ;
#54150 = CARTESIAN_POINT ( 'NONE',  ( 7.084665262690076126, 27.02201867748817676, -10.88017736071110164 ) ) ;
#54151 = CARTESIAN_POINT ( 'NONE',  ( 0.1532563361054082862, 51.21726448433412315, 2.638427012816831674 ) ) ;
#54152 = CARTESIAN_POINT ( 'NONE',  ( 7.084665262690076126, 29.10535201082150181, 10.88017736071109987 ) ) ;
#54153 = CARTESIAN_POINT ( 'NONE',  ( 6.767445849361252819, 14.49999999999999112, -13.38662304974503492 ) ) ;
#54154 = CARTESIAN_POINT ( 'NONE',  ( 10.00000000000000178, 57.25893115100078745, 9.846743663894594434 ) ) ;
#54155 = DIRECTION ( 'NONE',  ( -1.000000000000000000, 0.000000000000000000, 0.000000000000000000 ) ) ;
#54156 = AXIS2_PLACEMENT_3D ( 'NONE', #53557, #39068, #68085 ) ;
#54157 = DIRECTION ( 'NONE',  ( -0.000000000000000000, -0.000000000000000000, 1.000000000000000000 ) ) ;
#54158 = CARTESIAN_POINT ( 'NONE',  ( -8.000000000000000000, 80.32179676972448590, -3.750000000000000000 ) ) ;
#54159 = CARTESIAN_POINT ( 'NONE',  ( 14.92337183194729633, 2.675597817667451750, 8.527530157486181039 ) ) ;
#54160 = DIRECTION ( 'NONE',  ( 1.000000000000000000, 0.000000000000000000, 0.000000000000000000 ) ) ;
#54161 = ORIENTED_EDGE ( 'NONE', *, *, #65807, .T. ) ;
#54162 =( NAMED_UNIT ( * ) SI_UNIT ( $, .STERADIAN. ) SOLID_ANGLE_UNIT ( ) );
#54163 = CARTESIAN_POINT ( 'NONE',  ( 2.791683348922240793, 26.63393115100078745, 7.208316651077764092 ) ) ;
#54164 = FACE_OUTER_BOUND ( 'NONE', #76034, .T. ) ;
#54165 = CARTESIAN_POINT ( 'NONE',  ( 3.591859063236763294, 43.29030133659708923, -11.09922568453595026 ) ) ;
#54166 = CARTESIAN_POINT ( 'NONE',  ( -5.795997163830251431, -0.03417435944610275333, 13.01802277140702024 ) ) ;
#54167 = ORIENTED_EDGE ( 'NONE', *, *, #4996, .F. ) ;
#54168 = AXIS2_PLACEMENT_3D ( 'NONE', #5391, #57382, #20874 ) ;
#54169 = CARTESIAN_POINT ( 'NONE',  ( 6.879999999999995453, 43.00000000000000000, 6.500000000000000888 ) ) ;
#54170 = DIRECTION ( 'NONE',  ( 0.000000000000000000, 0.000000000000000000, 1.000000000000000000 ) ) ;
#54171 = CARTESIAN_POINT ( 'NONE',  ( 10.00000000000000000, 59.75893115100078745, -9.846743663894594434 ) ) ;
#54172 = CARTESIAN_POINT ( 'NONE',  ( -4.164238869374099039, 36.80374883491396787, 8.674139862899312516E-16 ) ) ;
#54173 = CARTESIAN_POINT ( 'NONE',  ( 12.63842701281683034, 57.46726448433411605, 9.846743663894596210 ) ) ;
#54174 = SURFACE_STYLE_USAGE ( .BOTH. , #86166 ) ;
#54175 = CARTESIAN_POINT ( 'NONE',  ( 0.1532563361054100626, 25.80059781766744820, -2.638427012816831230 ) ) ;
#54176 = CARTESIAN_POINT ( 'NONE',  ( 13.43411237798106583, 57.66530133659708923, -12.81628187352647252 ) ) ;
#54177 = CARTESIAN_POINT ( 'NONE',  ( 6.565887622018943937, -1.918031996736246692, -12.81628187352647608 ) ) ;
#54178 = CARTESIAN_POINT ( 'NONE',  ( 4.559911319644449179, 57.23035201082150536, -9.422509992056141925 ) ) ;
#54179 = CARTESIAN_POINT ( 'NONE',  ( 0.1532563361054083140, 41.00893115100078745, 1.131784320476157264E-15 ) ) ;
#54180 = CARTESIAN_POINT ( 'NONE',  ( 12.50534872682727716, 15.00000000000000000, 7.339363270777608861 ) ) ;
#54181 = ADVANCED_FACE ( 'NONE', ( #3176 ), #33641, .F. ) ;
#54182 = CARTESIAN_POINT ( 'NONE',  ( 15.44008868035555260, 54.73035201082150536, 9.422509992056143702 ) ) ;
#54183 = EDGE_CURVE ( 'NONE', #61835, #75327, #77188, .T. ) ;
#54184 = EDGE_CURVE ( 'NONE', #11472, #44083, #42475, .T. ) ;
#54185 = EDGE_LOOP ( 'NONE', ( #70050, #76037, #55411, #74347 ) ) ;
#54186 = DIRECTION ( 'NONE',  ( 0.000000000000000000, 1.000000000000000000, 0.000000000000000000 ) ) ;
#54187 = CARTESIAN_POINT ( 'NONE',  ( -0.8801773607111009756, 28.06368534415484106, 1.068504757029289695E-15 ) ) ;
#54189 = CARTESIAN_POINT ( 'NONE',  ( 10.00000000000000000, 51.81368534415484106, -10.88017736071110342 ) ) ;
#54188 = CARTESIAN_POINT ( 'NONE',  ( 16.40814093676323893, 5.790301336597087456, 11.09922568453595026 ) ) ;
#54190 = CARTESIAN_POINT ( 'NONE',  ( 2.618367889266248100E-15, 44.99999999999999289, -7.000000000000000000 ) ) ;
#54191 = CARTESIAN_POINT ( 'NONE',  ( -7.674241358950961711, 0.2301500950314201710, 12.81905807005879439 ) ) ;
#54192 = CARTESIAN_POINT ( 'NONE',  ( 10.32896413005680181, 4.745456701841142433, 5.963430220938278126 ) ) ;
#54194 = CARTESIAN_POINT ( 'NONE',  ( -46.82017113615791004, 100.6079546444643427, 9.324761308090124601 ) ) ;
#54193 = CARTESIAN_POINT ( 'NONE',  ( 17.96484262340118221, 39.93868534415484106, 7.964842623401181321 ) ) ;
#54195 = CARTESIAN_POINT ( 'NONE',  ( 18.52753015748617571, 43.09226448433412315, 4.923371831947298993 ) ) ;
#54196 = CARTESIAN_POINT ( 'NONE',  ( 1.780824192092400615, 0.3640475087720986824, 14.89391369643515617 ) ) ;
#54197 = CARTESIAN_POINT ( 'NONE',  ( 14.16423886937410259, 24.30374883491398563, -2.602085213965210642E-15 ) ) ;
#54198 = CARTESIAN_POINT ( 'NONE',  ( 6.565887622018943937, 8.081968003263751754, -12.81628187352647608 ) ) ;
#54199 = CARTESIAN_POINT ( 'NONE',  ( 19.42250999205614193, 20.14701867748817321, 5.440088680355555262 ) ) ;
#54200 = CARTESIAN_POINT ( 'NONE',  ( 2.603489959281613420, 60.43575266056826933, -6.500000000000031086 ) ) ;
#54201 = CARTESIAN_POINT ( 'NONE',  ( 2.917880565312950480, 20.97041550158063217, -12.26659068614894821 ) ) ;
#54202 = CARTESIAN_POINT ( 'NONE',  ( 20.36894250292379738, 59.92874883491397497, -10.36894250292379027 ) ) ;
#54203 = CARTESIAN_POINT ( 'NONE',  ( 18.52753015748618282, 28.92559781766745175, -4.923371831947291888 ) ) ;
#54204 = CARTESIAN_POINT ( 'NONE',  ( 5.076628168052704559, 15.17559781766745175, -8.527530157486179263 ) ) ;
#54205 = ORIENTED_EDGE ( 'NONE', *, *, #45864, .F. ) ;
#54206 = CARTESIAN_POINT ( 'NONE',  ( 10.00000000000000000, 19.75893115100078390, -9.846743663894594434 ) ) ;
#54207 = CARTESIAN_POINT ( 'NONE',  ( 10.00000000000000000, 21.81368534415484106, -10.88017736071110342 ) ) ;
#54208 = CARTESIAN_POINT ( 'NONE',  ( 0.1532563361054082862, 56.21726448433411605, 2.638427012816831674 ) ) ;
#54210 = SURFACE_STYLE_FILL_AREA ( #23255 ) ;
#54209 = CARTESIAN_POINT ( 'NONE',  ( -0.3689425029237881626, 7.428748834913967869, 10.36894250292379027 ) ) ;
#54211 = CARTESIAN_POINT ( 'NONE',  ( -11.59580422753466422, 0.2301505044262088240, 9.421229451859115755 ) ) ;
#54212 = CARTESIAN_POINT ( 'NONE',  ( 2.791683348922240793, 16.63393115100078745, 7.208316651077764092 ) ) ;
#54213 = CARTESIAN_POINT ( 'NONE',  ( -1.099225684535947600, 34.54030133659708923, 6.408140936763237150 ) ) ;
#54214 = CARTESIAN_POINT ( 'NONE',  ( 14.92337183194729633, 37.67559781766745175, 8.527530157486181039 ) ) ;
#54215 = EDGE_LOOP ( 'NONE', ( #56683, #96586, #35585, #78119 ) ) ;
#54216 = CARTESIAN_POINT ( 'NONE',  ( 0.1532563361054083140, 16.00893115100078390, 1.131784320476157264E-15 ) ) ;
#54217 = EDGE_CURVE ( 'NONE', #54527, #59040, #92683, .T. ) ;
#54218 = CARTESIAN_POINT ( 'NONE',  ( 8.900267061460978013, -1.043551099215020317, -3.750000000000000000 ) ) ;
#54219 = CARTESIAN_POINT ( 'NONE',  ( 14.09394518620612224, 15.00000000000000000, -3.407449058785360752 ) ) ;
#54220 = CIRCLE ( 'NONE', #4771, 15.00000000000000000 ) ;
#54221 = CARTESIAN_POINT ( 'NONE',  ( 13.79529636645031943, 50.34541550158064638, -14.16423886937409904 ) ) ;
#54222 = CARTESIAN_POINT ( 'NONE',  ( -0.8801773607110991993, 57.85535201082149825, -2.915334737309923874 ) ) ;
#54223 = LINE ( 'NONE', #47212, #98503 ) ;
#54224 = CARTESIAN_POINT ( 'NONE',  ( 15.44008868035555793, 51.39701867748816966, -9.422509992056140149 ) ) ;
#54225 = CARTESIAN_POINT ( 'NONE',  ( 7.361572987183170547, 37.05059781766744464, 9.846743663894590881 ) ) ;
#54226 =( NAMED_UNIT ( * ) PLANE_ANGLE_UNIT ( ) SI_UNIT ( $, .RADIAN. ) );
#54227 = DIRECTION ( 'NONE',  ( -1.000000000000000000, 0.000000000000000000, 0.000000000000000000 ) ) ;
#54228 = CARTESIAN_POINT ( 'NONE',  ( 5.076628168052704559, 50.17559781766745886, -8.527530157486179263 ) ) ;
#54229 = B_SPLINE_CURVE_WITH_KNOTS ( 'NONE', 3,
 ( #84351, #92327, #68362, #8824, #23358, #53841 ),
 .UNSPECIFIED., .F., .F.,
 ( 4, 2, 4 ),
 ( 0.0002800020636817308482, 0.0006862073132860410825, 0.001092412562890351154 ),
 .UNSPECIFIED. ) ;
#54230 = TOROIDAL_SURFACE ( 'NONE', #30243, 9.538348415311009632, 7.000000000000000000 ) ;
#54231 = CARTESIAN_POINT ( 'NONE',  ( 15.44008868035555260, 49.73035201082150536, 9.422509992056143702 ) ) ;
#54232 = FILL_AREA_STYLE_COLOUR ( '', #13927 ) ;
#54233 = ADVANCED_FACE ( 'NONE', ( #73119 ), #96146, .T. ) ;
#54234 = ORIENTED_EDGE ( 'NONE', *, *, #53879, .F. ) ;
#54235 = ORIENTED_EDGE ( 'NONE', *, *, #94864, .T. ) ;
#54236 = DIRECTION ( 'NONE',  ( 0.000000000000000000, 1.000000000000000000, 0.000000000000000000 ) ) ;
#54237 = CARTESIAN_POINT ( 'NONE',  ( -8.000000000000001776, -7.313785530895824394, 3.750000000000000000 ) ) ;
#54238 = CARTESIAN_POINT ( 'NONE',  ( 1.472469842513823179, 41.42559781766745886, 4.923371831947296329 ) ) ;
#54239 = CARTESIAN_POINT ( 'NONE',  ( 19.84674366389459266, 28.71726448433411960, -2.638427012816827677 ) ) ;
#54240 = CARTESIAN_POINT ( 'NONE',  ( 13.43411237798106583, 52.66530133659708213, -12.81628187352647252 ) ) ;
#54242 = CARTESIAN_POINT ( 'NONE',  ( 0.1532563361054100626, 50.80059781766745175, -2.638427012816831230 ) ) ;
#54241 = CARTESIAN_POINT ( 'NONE',  ( 10.00000000000000000, 21.81368534415484106, -10.88017736071110342 ) ) ;
#54243 = FACE_OUTER_BOUND ( 'NONE', #67660, .T. ) ;
#54244 = CARTESIAN_POINT ( 'NONE',  ( 20.36894250292379738, 24.92874883491396787, -10.36894250292379027 ) ) ;
#54245 = CARTESIAN_POINT ( 'NONE',  ( 17.08211943468705130, 63.47041550158063927, 12.26659068614894998 ) ) ;
#54246 = CARTESIAN_POINT ( 'NONE',  ( 0.1532563361054082862, 51.21726448433412315, 2.638427012816831674 ) ) ;
#54247 = CARTESIAN_POINT ( 'NONE',  ( 18.00000000000000000, 78.50170875364594281, 3.769097879697934861 ) ) ;
#54248 = CARTESIAN_POINT ( 'NONE',  ( 2.035157376598822676, 47.43868534415484817, -7.964842623401177768 ) ) ;
#54249 = CARTESIAN_POINT ( 'NONE',  ( 12.63842701281683922, 19.55059781766745175, -9.846743663894590881 ) ) ;
#54250 = CARTESIAN_POINT ( 'NONE',  ( -6.607869636406700664, -50.96183896326240159, 3.750000000001612044 ) ) ;
#54251 = VERTEX_POINT ( 'NONE', #28122 ) ;
#54252 = B_SPLINE_CURVE_WITH_KNOTS ( 'NONE', 3,
 ( #41076, #85585, #2604, #72045, #47075, #26067, #3574, #26543, #93565, #40581, #86571, #33057, #25098, #48552, #71078, #9581, #79053, #48057, #78571, #17098, #39603, #47581, #71573, #2109, #78077, #18563, #3084, #32063 ),
 .UNSPECIFIED., .F., .F.,
 ( 4, 2, 2, 2, 2, 2, 2, 2, 2, 2, 2, 2, 2, 4 ),
 ( 0.000000000000000000, 0.003117168999339133169, 0.006234337998678266338, 0.01246867599735653268, 0.02493735199471306535, 0.03740602799206958068, 0.04987470398942610988, 0.06234337998678262521, 0.07481205598413914748, 0.08728073198149567669, 0.09351506998017390659, 0.09663223897951304930, 0.09819082347918259290, 0.09974940797885215038 ),
 .UNSPECIFIED. ) ;
#54253 = CARTESIAN_POINT ( 'NONE',  ( 3.969999999999999751, 0.000000000000000000, -2.500000000000000000 ) ) ;
#54254 = VERTEX_POINT ( 'NONE', #64625 ) ;
#54255 = CARTESIAN_POINT ( 'NONE',  ( 17.20831665107776587, 4.133931151000785675, -7.208316651077762316 ) ) ;
#54256 = EDGE_LOOP ( 'NONE', ( #53510, #60506, #22914, #65456 ) ) ;
#54257 = CARTESIAN_POINT ( 'NONE',  ( 20.36894250292379382, 23.67874883491397142, 10.36894250292379205 ) ) ;
#54258 = CARTESIAN_POINT ( 'NONE',  ( 18.52753015748618282, 13.92559781766745175, -4.923371831947291888 ) ) ;
#54259 = CARTESIAN_POINT ( 'NONE',  ( 4.559911319644449179, 42.23035201082151247, -9.422509992056141925 ) ) ;
#54260 = ORIENTED_EDGE ( 'NONE', *, *, #43268, .T. ) ;
#54261 = CARTESIAN_POINT ( 'NONE',  ( -0.8801773607111008646, 33.27201867748817676, 2.915334737309923430 ) ) ;
#54262 = CARTESIAN_POINT ( 'NONE',  ( 17.39651004071841456, 49.08210964143329136, -6.500000000000001776 ) ) ;
#54263 = EDGE_LOOP ( 'NONE', ( #53255, #13819, #46550, #75393, #52582, #52090 ) ) ;
#54264 = VERTEX_POINT ( 'NONE', #43619 ) ;
#54265 = CARTESIAN_POINT ( 'NONE',  ( -1.099225684535947600, 23.70696800326375708, -6.408140936763238038 ) ) ;
#54266 = CARTESIAN_POINT ( 'NONE',  ( 10.00000000000000178, 12.25893115100078568, 9.846743663894594434 ) ) ;
#54267 = CARTESIAN_POINT ( 'NONE',  ( -3.750000000000000000, 36.75000000000000000, 4.000000000000000000 ) ) ;
#54268 = CARTESIAN_POINT ( 'NONE',  ( -8.209432707284690878, 15.00000000000000000, -12.55409154915497183 ) ) ;
#54269 = CARTESIAN_POINT ( 'NONE',  ( 19.84674366389459266, 13.71726448433411782, -2.638427012816827677 ) ) ;
#54270 = CARTESIAN_POINT ( 'NONE',  ( 19.42250999205614548, 35.98035201082151247, -5.440088680355545492 ) ) ;
#54271 = EDGE_CURVE ( 'NONE', #11027, #28677, #7302, .T. ) ;
#54272 = VERTEX_POINT ( 'NONE', #12626 ) ;
#54273 = CARTESIAN_POINT ( 'NONE',  ( 21.09922568453595559, 62.04030133659709634, -6.408140936763230044 ) ) ;
#54274 = CARTESIAN_POINT ( 'NONE',  ( 2.035157376598822676, 52.43868534415483396, -7.964842623401177768 ) ) ;
#54275 = DIRECTION ( 'NONE',  ( -0.06975647374412535795, -0.9975640502598243087, 0.000000000000000000 ) ) ;
#54276 = CARTESIAN_POINT ( 'NONE',  ( 20.88017736071110164, 55.35535201082149825, 2.915334737309930979 ) ) ;
#54277 = CARTESIAN_POINT ( 'NONE',  ( 3.591859063236763294, 3.290301336597087012, -11.09922568453595026 ) ) ;
#54278 = VERTEX_POINT ( 'NONE', #66116 ) ;
#54279 = CARTESIAN_POINT ( 'NONE',  ( 8.235571585149870089, 11.99303362898264602, 8.235571585149868312 ) ) ;
#54280 = VERTEX_POINT ( 'NONE', #27629 ) ;
#54281 = AXIS2_PLACEMENT_3D ( 'NONE', #22393, #23875, #91362 ) ;
#54282 = CARTESIAN_POINT ( 'NONE',  ( 1.472469842513823179, 25.59226448433412315, -4.923371831947296329 ) ) ;
#54283 = CARTESIAN_POINT ( 'NONE',  ( -2.816281873526473856, 54.33196800326376064, 3.434112377981055619 ) ) ;
#54284 = FACE_OUTER_BOUND ( 'NONE', #20173, .T. ) ;
#54285 = CARTESIAN_POINT ( 'NONE',  ( 19.84674366389459621, 23.50893115100078390, 7.409399052514197653E-17 ) ) ;
#54286 = CARTESIAN_POINT ( 'NONE',  ( 21.09922568453595559, 22.04030133659708923, -6.408140936763230044 ) ) ;
#54288 = CARTESIAN_POINT ( 'NONE',  ( -3.585811749738964771, -2.700663748499701367, -2.750000000000000888 ) ) ;
#54287 = SURFACE_STYLE_FILL_AREA ( #21846 ) ;
#54289 = CARTESIAN_POINT ( 'NONE',  ( 15.44008868035555260, 54.73035201082150536, 9.422509992056143702 ) ) ;
#54290 = ADVANCED_FACE ( 'NONE', ( #42162 ), #42564, .T. ) ;
#54291 = CARTESIAN_POINT ( 'NONE',  ( 17.20831665107776587, 59.13393115100078745, -7.208316651077762316 ) ) ;
#54292 = FILL_AREA_STYLE_COLOUR ( '', #95018 ) ;
#54293 = CIRCLE ( 'NONE', #51089, 14.49999999999999822 ) ;
#54294 = CARTESIAN_POINT ( 'NONE',  ( 0.1532563361054083140, 31.00893115100078390, 1.131784320476157264E-15 ) ) ;
#54295 = CARTESIAN_POINT ( 'NONE',  ( 1.472469842513823179, 15.59226448433411960, -4.923371831947296329 ) ) ;
#54296 = CARTESIAN_POINT ( 'NONE',  ( 7.084665262690076126, 9.105352010821503583, 10.88017736071109987 ) ) ;
#54297 = CARTESIAN_POINT ( 'NONE',  ( 21.09922568453594849, 11.20696800326375531, 6.408140936763242479 ) ) ;
#54298 = FILL_AREA_STYLE_COLOUR ( '', #78974 ) ;
#54299 = CARTESIAN_POINT ( 'NONE',  ( 0.000000000000000000, 0.000000000000000000, -5.999999999999999112 ) ) ;
#54300 = EDGE_CURVE ( 'NONE', #6506, #91280, #29120, .T. ) ;
#54301 =( NAMED_UNIT ( * ) SI_UNIT ( $, .STERADIAN. ) SOLID_ANGLE_UNIT ( ) );
#54302 = CARTESIAN_POINT ( 'NONE',  ( 20.88017736071110875, 25.77201867748816966, -2.915334737309920765 ) ) ;
#54303 = EDGE_CURVE ( 'NONE', #3044, #17262, #30535, .T. ) ;
#54304 = CARTESIAN_POINT ( 'NONE',  ( -0.3289641300568005855, 50.10497603579418069, 5.963430220938281678 ) ) ;
#54305 = CARTESIAN_POINT ( 'NONE',  ( 10.00000000000000178, 14.31368534415483929, 10.88017736071110342 ) ) ;
#54307 = B_SPLINE_CURVE_WITH_KNOTS ( 'NONE', 3,
 ( #47165, #32662, #93164, #32160 ),
 .UNSPECIFIED., .F., .F.,
 ( 4, 4 ),
 ( 3.291406376790657244E-17, 0.001060528352562001547 ),
 .UNSPECIFIED. ) ;
#54306 = CARTESIAN_POINT ( 'NONE',  ( 0.2751277870542870319, 54.36607318730131055, -6.499999999999985789 ) ) ;
#54308 = CARTESIAN_POINT ( 'NONE',  ( 19.42250999205614548, 35.98035201082151247, -5.440088680355545492 ) ) ;
#54310 = LINE ( 'NONE', #52837, #94135 ) ;
#54309 = CARTESIAN_POINT ( 'NONE',  ( 17.96484262340118221, 6.188685344154837509, -7.964842623401177768 ) ) ;
#54311 = CARTESIAN_POINT ( 'NONE',  ( 19.84674366389459266, 3.717264484334118713, -2.638427012816827677 ) ) ;
#54312 = CARTESIAN_POINT ( 'NONE',  ( 10.00000000000000000, 19.75893115100078390, -9.846743663894594434 ) ) ;
#54313 = CARTESIAN_POINT ( 'NONE',  ( 18.00000000000000000, 78.80384757729335377, -3.750000000000000000 ) ) ;
#54314 = CARTESIAN_POINT ( 'NONE',  ( 1.983216688680936812, 0.000000000000000000, -14.11131997956737649 ) ) ;
#54315 = DIRECTION ( 'NONE',  ( 0.000000000000000000, 0.000000000000000000, 1.000000000000000000 ) ) ;
#54316 = CARTESIAN_POINT ( 'NONE',  ( -10.57486859796104994, -40.44919682093461688, -3.750000000000000000 ) ) ;
#54317 = CARTESIAN_POINT ( 'NONE',  ( 10.00000000000000178, 18.05374883491396787, 14.16423886937410082 ) ) ;
#54318 = CARTESIAN_POINT ( 'NONE',  ( 12.63842701281683922, 39.55059781766744464, -9.846743663894590881 ) ) ;
#54319 = CARTESIAN_POINT ( 'NONE',  ( 14.71525861348289865, 0.5000000000000004441, -2.908807992686582633 ) ) ;
#54320 = ORIENTED_EDGE ( 'NONE', *, *, #63452, .T. ) ;
#54321 = CARTESIAN_POINT ( 'NONE',  ( -2.266590686148945544, 47.22041550158063927, 7.082119434687048631 ) ) ;
#54322 = CARTESIAN_POINT ( 'NONE',  ( 1.472469842513823179, 16.42559781766745175, 4.923371831947296329 ) ) ;
#54324 = DIRECTION ( 'NONE',  ( 0.000000000000000000, -1.000000000000000000, 0.000000000000000000 ) ) ;
#54323 = DIRECTION ( 'NONE',  ( -0.000000000000000000, -0.000000000000000000, 1.000000000000000000 ) ) ;
#54325 = CARTESIAN_POINT ( 'NONE',  ( -0.8801773607111008646, 48.27201867748816966, 2.915334737309923430 ) ) ;
#54326 = CARTESIAN_POINT ( 'NONE',  ( 19.38216949554541557, 47.24863466993041783, -9.382169495545420901 ) ) ;
#54327 = CARTESIAN_POINT ( 'NONE',  ( 2.035157376598824452, 23.68868534415484461, 7.964842623401179544 ) ) ;
#54328 = CARTESIAN_POINT ( 'NONE',  ( 0.6178305044545838731, 49.74863466993041072, 9.382169495545420901 ) ) ;
#54329 = CARTESIAN_POINT ( 'NONE',  ( 0.1532563361054083140, 66.00893115100079456, 1.131784320476157264E-15 ) ) ;
#54330 = CARTESIAN_POINT ( 'NONE',  ( 5.076628168052703671, 6.842264484334118713, 8.527530157486179263 ) ) ;
#54331 = ORIENTED_EDGE ( 'NONE', *, *, #94597, .T. ) ;
#54332 = LINE ( 'NONE', #92830, #67639 ) ;
#54333 = EDGE_CURVE ( 'NONE', #26776, #10227, #55241, .T. ) ;
#54334 = DIRECTION ( 'NONE',  ( -0.6087614290087242086, 0.000000000000000000, 0.7933533402912323895 ) ) ;
#54335 = CARTESIAN_POINT ( 'NONE',  ( 13.79529636645031943, 55.34541550158062506, -14.16423886937409904 ) ) ;
#54336 = CARTESIAN_POINT ( 'NONE',  ( 22.26659068614894466, 18.88708216824730002, 7.082119434687054849 ) ) ;
#54337 = CARTESIAN_POINT ( 'NONE',  ( 2.035157376598824452, 13.68868534415483751, 7.964842623401179544 ) ) ;
#54339 = CARTESIAN_POINT ( 'NONE',  ( 18.72515096720568906, 15.05509018479935612, 6.500000000000002665 ) ) ;
#54338 = CARTESIAN_POINT ( 'NONE',  ( 7.084665262690076126, 42.02201867748816966, -10.88017736071110164 ) ) ;
#54340 = CARTESIAN_POINT ( 'NONE',  ( -14.49440716394870599, 15.00000000000000000, -0.4026921475168267484 ) ) ;
#54341 = DIRECTION ( 'NONE',  ( 0.000000000000000000, 0.000000000000000000, 1.000000000000000000 ) ) ;
#54342 = CARTESIAN_POINT ( 'NONE',  ( 2.035157376598824452, 63.68868534415484106, 7.964842623401179544 ) ) ;
#54343 = CARTESIAN_POINT ( 'NONE',  ( 2.035157376598822676, 67.43868534415484817, -7.964842623401177768 ) ) ;
#54344 = CARTESIAN_POINT ( 'NONE',  ( 5.076628168052704559, 25.17559781766745175, -8.527530157486179263 ) ) ;
#54345 = CARTESIAN_POINT ( 'NONE',  ( 18.50749283717777161, 19.69955587570480660, 6.499999999999979572 ) ) ;
#54346 = SURFACE_STYLE_USAGE ( .BOTH. , #47333 ) ;
#54347 = CARTESIAN_POINT ( 'NONE',  ( 12.63842701281683034, 12.46726448433411782, 9.846743663894596210 ) ) ;
#54348 = CARTESIAN_POINT ( 'NONE',  ( 17.20831665107776587, 37.88393115100078745, 7.208316651077764980 ) ) ;
#54349 = CARTESIAN_POINT ( 'NONE',  ( 20.88017736071110164, 20.35535201082150891, 2.915334737309930979 ) ) ;
#54350 = UNCERTAINTY_MEASURE_WITH_UNIT (LENGTH_MEASURE( 1.000000000000000082E-05 ), #21620, 'distance_accuracy_value', 'NONE');
#54351 = VECTOR ( 'NONE', #13153, 1000.000000000000000 ) ;
#54352 = CARTESIAN_POINT ( 'NONE',  ( 22.81628187352648496, 36.83196800326376064, -3.434112377981050290 ) ) ;
#54353 = CARTESIAN_POINT ( 'NONE',  ( 10.00000000000000178, 7.258931151000785675, 9.846743663894594434 ) ) ;
#54354 = DIRECTION ( 'NONE',  ( -0.000000000000000000, 0.000000000000000000, -1.000000000000000000 ) ) ;
#54355 = CARTESIAN_POINT ( 'NONE',  ( 0.1532563361054082862, 46.21726448433411605, 2.638427012816831674 ) ) ;
#54357 = CARTESIAN_POINT ( 'NONE',  ( 10.00000000000000178, 3.053748834913967425, 14.16423886937410082 ) ) ;
#54356 = CARTESIAN_POINT ( 'NONE',  ( 17.20831665107776587, 32.88393115100078745, 7.208316651077764980 ) ) ;
#54358 = CARTESIAN_POINT ( 'NONE',  ( -2.266590686148945544, 22.22041550158063572, 7.082119434687048631 ) ) ;
#54359 = VECTOR ( 'NONE', #45369, 1000.000000000000000 ) ;
#54360 = CARTESIAN_POINT ( 'NONE',  ( 15.44008868035555260, 29.73035201082150891, 9.422509992056143702 ) ) ;
#54361 = CARTESIAN_POINT ( 'NONE',  ( 12.91533473730992121, 14.52201867748817143, 10.88017736071110164 ) ) ;
#54362 = CIRCLE ( 'NONE', #84707, 15.00000000000000000 ) ;
#54363 = CARTESIAN_POINT ( 'NONE',  ( 20.88017736071110875, 45.77201867748816966, -2.915334737309920765 ) ) ;
#54364 = CARTESIAN_POINT ( 'NONE',  ( 20.88017736071110164, 30.35535201082151247, 2.915334737309930979 ) ) ;
#54365 = VERTEX_POINT ( 'NONE', #13634 ) ;
#54366 = CARTESIAN_POINT ( 'NONE',  ( 22.81628187352648496, 36.83196800326376064, -3.434112377981050290 ) ) ;
#54367 = TOROIDAL_SURFACE ( 'NONE', #14422, 14.49999999999999822, 0.5000000000000000000 ) ;
#54368 = CARTESIAN_POINT ( 'NONE',  ( -0.8801773607111008646, 38.27201867748816255, 2.915334737309923430 ) ) ;
#54369 = EDGE_LOOP ( 'NONE', ( #51703, #42719, #5610, #30278 ) ) ;
#54370 = CARTESIAN_POINT ( 'NONE',  ( -2.816281873526473856, 59.12363466993042493, 9.499525473075851096E-16 ) ) ;
#54371 = CARTESIAN_POINT ( 'NONE',  ( 15.44008868035555260, 54.73035201082150536, 9.422509992056143702 ) ) ;
#54372 = ORIENTED_EDGE ( 'NONE', *, *, #33783, .F. ) ;
#54373 = CARTESIAN_POINT ( 'NONE',  ( 0.5774900079438607392, 53.48035201082151247, 5.440088680355550821 ) ) ;
#54374 = CARTESIAN_POINT ( 'NONE',  ( 14.99999999999997691, 80.32179676972448590, -4.250000000000000000 ) ) ;
#54375 = CARTESIAN_POINT ( 'NONE',  ( -0.04068437667222171011, 37.21974360917720759, -6.396802510829769695 ) ) ;
#54376 = CARTESIAN_POINT ( 'NONE',  ( 2.917880565312948704, 57.63708216824731068, 12.26659068614894643 ) ) ;
#54377 = CARTESIAN_POINT ( 'NONE',  ( 2.035157376598824452, 63.68868534415484106, 7.964842623401179544 ) ) ;
#54378 = DIRECTION ( 'NONE',  ( -3.907985046680550391E-14, 0.000000000000000000, 1.000000000000000000 ) ) ;
#54379 = DIRECTION ( 'NONE',  ( 0.000000000000000000, 0.000000000000000000, -1.000000000000000000 ) ) ;
#54380 = CARTESIAN_POINT ( 'NONE',  ( 1.472469842513823179, 26.42559781766745175, 4.923371831947296329 ) ) ;
#54381 = ORIENTED_EDGE ( 'NONE', *, *, #76973, .F. ) ;
#54382 = CARTESIAN_POINT ( 'NONE',  ( 19.84674366389459266, 33.30059781766744464, 2.638427012816836559 ) ) ;
#54383 = VECTOR ( 'NONE', #68614, 1000.000000000000114 ) ;
#54384 = CARTESIAN_POINT ( 'NONE',  ( 15.44008868035555793, 41.39701867748817676, -9.422509992056140149 ) ) ;
#54385 = CARTESIAN_POINT ( 'NONE',  ( 5.076628168052703671, 36.84226448433412315, 8.527530157486179263 ) ) ;
#54386 = CARTESIAN_POINT ( 'NONE',  ( 0.6178305044545818747, 18.49863466993041428, -9.382169495545419124 ) ) ;
#54388 = CARTESIAN_POINT ( 'NONE',  ( 15.00000000000000178, 73.00000000000000000, 6.500000000000000888 ) ) ;
#54387 = DIRECTION ( 'NONE',  ( 0.000000000000000000, 1.000000000000000000, 0.000000000000000000 ) ) ;
#54389 = CARTESIAN_POINT ( 'NONE',  ( 2.035157376598822676, 52.43868534415483396, -7.964842623401177768 ) ) ;
#54390 = CARTESIAN_POINT ( 'NONE',  ( 20.36894250292379382, 63.67874883491396787, 10.36894250292379205 ) ) ;
#54391 = EDGE_CURVE ( 'NONE', #62008, #50558, #23355, .T. ) ;
#54392 = AXIS2_PLACEMENT_3D ( 'NONE', #72125, #73597, #3653 ) ;
#54393 = B_SPLINE_CURVE_WITH_KNOTS ( 'NONE', 3,
 ( #8834, #85325, #69842, #60848, #31817, #15861 ),
 .UNSPECIFIED., .F., .F.,
 ( 4, 2, 4 ),
 ( 3.409110551494648722E-05, 0.0004400426677367915589, 0.0008459942299586366374 ),
 .UNSPECIFIED. ) ;
#54394 = CARTESIAN_POINT ( 'NONE',  ( 22.81628187352647785, 26.41530133659708923, 3.434112377981063169 ) ) ;
#54395 = CARTESIAN_POINT ( 'NONE',  ( 0.1532563361054100626, 50.80059781766745886, -2.638427012816831230 ) ) ;
#54396 = ORIENTED_EDGE ( 'NONE', *, *, #74093, .F. ) ;
#54397 = CARTESIAN_POINT ( 'NONE',  ( 21.09922568453594849, 31.20696800326375353, 6.408140936763242479 ) ) ;
#54398 = CARTESIAN_POINT ( 'NONE',  ( 20.88017736071110519, 25.56368534415483751, 2.639326808657452039E-16 ) ) ;
#54399 = CARTESIAN_POINT ( 'NONE',  ( -0.8801773607110991993, 57.85535201082149825, -2.915334737309923874 ) ) ;
#54400 = EDGE_LOOP ( 'NONE', ( #5521, #82829, #15192, #43169 ) ) ;
#54401 = CARTESIAN_POINT ( 'NONE',  ( 3.384479038598206646, 0.2301507000107690937, 14.55223509985380304 ) ) ;
#54402 = CARTESIAN_POINT ( 'NONE',  ( 1.472469842513823179, 6.425597817667451750, 4.923371831947296329 ) ) ;
#54403 = CARTESIAN_POINT ( 'NONE',  ( 0.1532563361054083140, 56.00893115100078745, 1.131784320476157264E-15 ) ) ;
#54404 = CARTESIAN_POINT ( 'NONE',  ( 0.1532563361054082862, 41.21726448433411605, 2.638427012816831674 ) ) ;
#54405 = CARTESIAN_POINT ( 'NONE',  ( -13.61802159414294877, -2.748198397366576661E-15, -5.334603887713678105 ) ) ;
#54406 = CARTESIAN_POINT ( 'NONE',  ( 14.92337183194729633, 32.67559781766745175, 8.527530157486181039 ) ) ;
#54407 = DIRECTION ( 'NONE',  ( 0.000000000000000000, -1.000000000000000000, 0.000000000000000000 ) ) ;
#54408 = CARTESIAN_POINT ( 'NONE',  ( 12.60874940350947959, 15.00000000000000000, -7.160268045227033973 ) ) ;
#54410 = CARTESIAN_POINT ( 'NONE',  ( 20.03932841506543028, 50.62161441960502373, -6.397827110478998769 ) ) ;
#54409 = CARTESIAN_POINT ( 'NONE',  ( 5.076628168052703671, 16.84226448433411960, 8.527530157486179263 ) ) ;
#54411 = CARTESIAN_POINT ( 'NONE',  ( 7.184033521041851778, -73.16344059793529198, -4.000000000000002665 ) ) ;
#54413 = ORIENTED_EDGE ( 'NONE', *, *, #9646, .T. ) ;
#54412 = CARTESIAN_POINT ( 'NONE',  ( 12.63842701281683922, 49.55059781766744464, -9.846743663894590881 ) ) ;
#54414 = PRESENTATION_LAYER_ASSIGNMENT (  '', '', ( #27290 ) ) ;
#54415 = CARTESIAN_POINT ( 'NONE',  ( 20.32896413005680714, 17.60497603579417358, -5.963430220938276349 ) ) ;
#54416 = EDGE_CURVE ( 'NONE', #79731, #20729, #46115, .T. ) ;
#54417 = CARTESIAN_POINT ( 'NONE',  ( -2.816281873526473856, 9.123634669930421381, 9.499525473075851096E-16 ) ) ;
#54418 = CARTESIAN_POINT ( 'NONE',  ( -0.8801773607111009756, 58.06368534415484106, 1.068504757029289695E-15 ) ) ;
#54419 = CARTESIAN_POINT ( 'NONE',  ( -2.266590686148945544, 51.38708216824730357, -7.082119434687050408 ) ) ;
#54420 = EDGE_CURVE ( 'NONE', #74297, #30124, #39330, .T. ) ;
#54422 = PRESENTATION_STYLE_ASSIGNMENT (( #93413 ) ) ;
#54421 = CIRCLE ( 'NONE', #44857, 0.5000000000000004441 ) ;
#54423 = CARTESIAN_POINT ( 'NONE',  ( 66.76470751278411342, 44.99999999999998579, -9.500000000000000000 ) ) ;
#54424 = CARTESIAN_POINT ( 'NONE',  ( -0.3689425029237898834, 41.17874883491397497, -10.36894250292378850 ) ) ;
#54425 = CARTESIAN_POINT ( 'NONE',  ( 6.204703633549690345, 57.84541550158063927, 14.16423886937410082 ) ) ;
#54426 = CARTESIAN_POINT ( 'NONE',  ( 17.08211943468705130, 23.47041550158063572, 12.26659068614894998 ) ) ;
#54428 = CARTESIAN_POINT ( 'NONE',  ( 70.08911253270098030, 0.3894472361808988259, -9.500000000000000000 ) ) ;
#54427 = CARTESIAN_POINT ( 'NONE',  ( 24.16423886937410614, 24.51208216824730002, -3.795296366450302550 ) ) ;
#54429 = CARTESIAN_POINT ( 'NONE',  ( 5.510795456469524289, -25.29786701974074603, -3.750000000000000888 ) ) ;
#54431 = CARTESIAN_POINT ( 'NONE',  ( 10.00000000000000178, 42.25893115100078745, 9.846743663894594434 ) ) ;
#54430 = CARTESIAN_POINT ( 'NONE',  ( 4.471066085428756942, -3.611416924335026479, 2.750000000000000000 ) ) ;
#54432 = CARTESIAN_POINT ( 'NONE',  ( 7.084665262690076126, 19.10535201082150181, 10.88017736071109987 ) ) ;
#54433 = CARTESIAN_POINT ( 'NONE',  ( 0.2751277870542910842, 67.28217586085239077, -6.499999999999992006 ) ) ;
#54434 = CARTESIAN_POINT ( 'NONE',  ( 14.92337183194729633, 62.67559781766745886, 8.527530157486181039 ) ) ;
#54435 = LINE ( 'NONE', #75963, #65658 ) ;
#54436 = CARTESIAN_POINT ( 'NONE',  ( 17.20831665107776587, 44.13393115100078745, -7.208316651077762316 ) ) ;
#54437 = CARTESIAN_POINT ( 'NONE',  ( -2.816281873526473856, 49.33196800326374643, 3.434112377981055619 ) ) ;
#54438 = CARTESIAN_POINT ( 'NONE',  ( 10.36894250292378850, -10.07125116508603213, -10.36894250292379027 ) ) ;
#54439 = CARTESIAN_POINT ( 'NONE',  ( 1.472469842513823179, 41.42559781766745886, 4.923371831947296329 ) ) ;
#54440 = CARTESIAN_POINT ( 'NONE',  ( 14.92337183194729988, 59.34226448433412315, -8.527530157486177487 ) ) ;
#54441 = CARTESIAN_POINT ( 'NONE',  ( 17.08211943468705130, 33.47041550158063927, 12.26659068614894998 ) ) ;
#54442 = CARTESIAN_POINT ( 'NONE',  ( -0.3689425029237881626, 12.42874883491396609, 10.36894250292379027 ) ) ;
#54443 = EDGE_CURVE ( 'NONE', #49035, #16296, #55071, .T. ) ;
#54444 = CARTESIAN_POINT ( 'NONE',  ( -6.336100170400736253, 0.2301512019179792756, -13.53056138701896316 ) ) ;
#54446 = DIRECTION ( 'NONE',  ( 0.000000000000000000, 1.000000000000000000, 0.000000000000000000 ) ) ;
#54445 = CARTESIAN_POINT ( 'NONE',  ( 1.499999999999999556, 21.83999999999999986, 1.836970198721029194E-16 ) ) ;
#54447 = CARTESIAN_POINT ( 'NONE',  ( 10.00000000000000000, 1.813685344154838175, -10.88017736071110342 ) ) ;
#54448 = CARTESIAN_POINT ( 'NONE',  ( 0.6178305044545838731, 9.748634669930416052, 9.382169495545420901 ) ) ;
#54449 = SURFACE_SIDE_STYLE ('',( #62436 ) ) ;
#54450 = CARTESIAN_POINT ( 'NONE',  ( 2.791683348922240793, 1.633931151000784565, 7.208316651077764092 ) ) ;
#54451 = DIRECTION ( 'NONE',  ( 0.000000000000000000, 1.000000000000000000, 0.000000000000000000 ) ) ;
#54452 = CARTESIAN_POINT ( 'NONE',  ( 32.26500600480481040, -1.876920803484231371E-15, 0.000000000000000000 ) ) ;
#54453 = CARTESIAN_POINT ( 'NONE',  ( 14.47650479471819551, 0.5000000000000004441, 3.928206833722108549 ) ) ;
#54454 = CARTESIAN_POINT ( 'NONE',  ( 2.917880565312948704, 67.63708216824730357, 12.26659068614894643 ) ) ;
#54455 = LINE ( 'NONE', #92456, #83124 ) ;
#54456 = CARTESIAN_POINT ( 'NONE',  ( 15.44008868035555793, 26.39701867748817321, -9.422509992056140149 ) ) ;
#54457 = CARTESIAN_POINT ( 'NONE',  ( 12.91533473730992121, 29.52201867748817321, 10.88017736071110164 ) ) ;
#54458 = CARTESIAN_POINT ( 'NONE',  ( 2.791683348922240793, 61.63393115100079456, 7.208316651077764092 ) ) ;
#54459 = CARTESIAN_POINT ( 'NONE',  ( 2.791683348922237240, 50.38393115100078035, -7.208316651077763204 ) ) ;
#54460 = CARTESIAN_POINT ( 'NONE',  ( -45.94000000000001194, 103.9981609152045507, -5.961202730336931488 ) ) ;
#54461 = CARTESIAN_POINT ( 'NONE',  ( -0.1503990784575242878, 64.24884699246891273, -6.262539305110083276 ) ) ;
#54462 = ORIENTED_EDGE ( 'NONE', *, *, #33632, .T. ) ;
#54463 = AXIS2_PLACEMENT_3D ( 'NONE', #9823, #40325, #71313 ) ;
#54464 = TOROIDAL_SURFACE ( 'NONE', #11358, 14.49999999999999822, 0.5000000000000000000 ) ;
#54465 = CARTESIAN_POINT ( 'NONE',  ( 7.084665262690076126, 34.10535201082151247, 10.88017736071109987 ) ) ;
#54466 = CARTESIAN_POINT ( 'NONE',  ( -2.816281873526473856, 24.33196800326375353, 3.434112377981055619 ) ) ;
#54467 = CARTESIAN_POINT ( 'NONE',  ( 64.56412365047461321, 44.99999999999998579, -7.000000000000000000 ) ) ;
#54468 = CIRCLE ( 'NONE', #36929, 0.2500000000000002220 ) ;
#54469 = CARTESIAN_POINT ( 'NONE',  ( 5.076628168052703671, 56.84226448433412315, 8.527530157486179263 ) ) ;
#54470 = CARTESIAN_POINT ( 'NONE',  ( 4.559911319644449179, 52.23035201082151247, -9.422509992056141925 ) ) ;
#54471 = CARTESIAN_POINT ( 'NONE',  ( 13.43411237798106583, 17.66530133659708923, -12.81628187352647252 ) ) ;
#54473 = LINE ( 'NONE', #69004, #38461 ) ;
#54472 = CARTESIAN_POINT ( 'NONE',  ( 7.084665262690076126, 57.02201867748817676, -10.88017736071110164 ) ) ;
#54474 = CARTESIAN_POINT ( 'NONE',  ( 1.983216688680843109, 0.000000000000000000, 14.11131997956739070 ) ) ;
#54475 = ORIENTED_EDGE ( 'NONE', *, *, #6805, .T. ) ;
#54476 = CARTESIAN_POINT ( 'NONE',  ( 0.5774900079438590739, 52.64701867748817676, -5.440088680355550821 ) ) ;
#54478 = CARTESIAN_POINT ( 'NONE',  ( 20.36894250292379738, 9.928748834913966093, -10.36894250292379027 ) ) ;
#54477 = CARTESIAN_POINT ( 'NONE',  ( -2.816281873526473856, 49.12363466993042493, 9.499525473075851096E-16 ) ) ;
#54479 = CARTESIAN_POINT ( 'NONE',  ( 5.076628168052704559, 15.17559781766745175, -8.527530157486179263 ) ) ;
#54480 = CARTESIAN_POINT ( 'NONE',  ( 19.84674366389459266, 63.71726448433412315, -2.638427012816827677 ) ) ;
#54481 = CARTESIAN_POINT ( 'NONE',  ( 2.791683348922240793, 16.63393115100078745, 7.208316651077764092 ) ) ;
#54482 = CARTESIAN_POINT ( 'NONE',  ( 19.72487221294571569, 39.78217586085237656, 6.499999999999986677 ) ) ;
#54483 = CARTESIAN_POINT ( 'NONE',  ( 22.26659068614894466, 58.88708216824729647, 7.082119434687054849 ) ) ;
#54484 = EDGE_LOOP ( 'NONE', ( #84004, #65683, #68531, #70872 ) ) ;
#54485 = CARTESIAN_POINT ( 'NONE',  ( 0.000000000000000000, 99.99999999999998579, 8.000000000000000000 ) ) ;
#54486 = CARTESIAN_POINT ( 'NONE',  ( -0.8801773607110991993, 7.855352010821504471, -2.915334737309923874 ) ) ;
#54487 = CARTESIAN_POINT ( 'NONE',  ( 0.1532563361054082862, 16.21726448433411960, 2.638427012816831674 ) ) ;
#54488 = AXIS2_PLACEMENT_3D ( 'NONE', #531, #59509, #91982 ) ;
#54489 = VERTEX_POINT ( 'NONE', #93076 ) ;
#54490 = CARTESIAN_POINT ( 'NONE',  ( 19.42250999205614548, 5.980352010821504471, -5.440088680355545492 ) ) ;
#54491 = CARTESIAN_POINT ( 'NONE',  ( 19.42250999205614193, 10.14701867748816966, 5.440088680355555262 ) ) ;
#54492 = CARTESIAN_POINT ( 'NONE',  ( 2.791683348922240793, 41.63393115100078745, 7.208316651077764092 ) ) ;
#54493 = CARTESIAN_POINT ( 'NONE',  ( -1.099225684535947600, 43.70696800326375353, -6.408140936763238038 ) ) ;
#54494 = CARTESIAN_POINT ( 'NONE',  ( -5.625000000000007994, 12.08846884451820891, -9.742785792574931492 ) ) ;
#54496 = CARTESIAN_POINT ( 'NONE',  ( 20.36894250292379382, 23.67874883491397142, 10.36894250292379205 ) ) ;
#54495 = DIRECTION ( 'NONE',  ( 0.000000000000000000, 0.000000000000000000, 1.000000000000000000 ) ) ;
#54497 = CARTESIAN_POINT ( 'NONE',  ( 15.44008868035555260, 29.73035201082150891, 9.422509992056143702 ) ) ;
#54498 = CARTESIAN_POINT ( 'NONE',  ( 17.96484262340118221, 4.938685344154837509, 7.964842623401181321 ) ) ;
#54499 = CARTESIAN_POINT ( 'NONE',  ( 10.00000000000000178, 47.25893115100078745, 9.846743663894594434 ) ) ;
#54500 = DIRECTION ( 'NONE',  ( -0.000000000000000000, -1.000000000000000000, -0.000000000000000000 ) ) ;
#54501 = CARTESIAN_POINT ( 'NONE',  ( 5.076628168052703671, 31.84226448433412315, 8.527530157486179263 ) ) ;
#54502 =( GEOMETRIC_REPRESENTATION_CONTEXT ( 3 ) GLOBAL_UNCERTAINTY_ASSIGNED_CONTEXT ( ( #90372 ) ) GLOBAL_UNIT_ASSIGNED_CONTEXT ( ( #73522, #49067, #49541 ) ) REPRESENTATION_CONTEXT ( 'NONE', 'WORKASPACE' ) );
#54503 = B_SPLINE_CURVE_WITH_KNOTS ( 'NONE', 3,
 ( #98985, #44462, #74964, #6468, #20990, #36973 ),
 .UNSPECIFIED., .F., .F.,
 ( 4, 2, 4 ),
 ( 0.0002800313526655974386, 0.0006862368888107541701, 0.001092442424955911064 ),
 .UNSPECIFIED. ) ;
#54504 = LINE ( 'NONE', #70020, #56194 ) ;
#54505 = CARTESIAN_POINT ( 'NONE',  ( -8.527530157486173934, 31.42559781766746241, 4.923371831947302546 ) ) ;
#54506 = ORIENTED_EDGE ( 'NONE', *, *, #624, .F. ) ;
#54507 = CARTESIAN_POINT ( 'NONE',  ( 2.035157376598824452, 3.688685344154837953, 7.964842623401179544 ) ) ;
#54508 = CARTESIAN_POINT ( 'NONE',  ( 19.42250999205614193, 65.14701867748817676, 5.440088680355555262 ) ) ;
#54509 = CARTESIAN_POINT ( 'NONE',  ( 7.361572987183170547, 62.05059781766745886, 9.846743663894590881 ) ) ;
#54510 = CARTESIAN_POINT ( 'NONE',  ( 2.035157376598822676, 32.43868534415483396, -7.964842623401177768 ) ) ;
#54512 = CARTESIAN_POINT ( 'NONE',  ( -1.099225684535947600, 34.54030133659708923, 6.408140936763237150 ) ) ;
#54511 = CARTESIAN_POINT ( 'NONE',  ( 2.035157376598822676, 7.438685344154837509, -7.964842623401177768 ) ) ;
#54513 = CARTESIAN_POINT ( 'NONE',  ( -4.164238869374099039, 11.80374883491396965, 8.674139862899312516E-16 ) ) ;
#54514 = ADVANCED_FACE ( 'NONE', ( #9585 ), #77092, .T. ) ;
#54515 = CARTESIAN_POINT ( 'NONE',  ( 6.565887622018943937, 48.08196800326375353, -12.81628187352647608 ) ) ;
#54516 = ORIENTED_EDGE ( 'NONE', *, *, #8919, .T. ) ;
#54517 = CARTESIAN_POINT ( 'NONE',  ( 12.63842701281683922, 49.55059781766744464, -9.846743663894590881 ) ) ;
#54518 = CARTESIAN_POINT ( 'NONE',  ( 7.084665262690076126, 27.02201867748817676, -10.88017736071110164 ) ) ;
#54519 = ORIENTED_EDGE ( 'NONE', *, *, #67082, .T. ) ;
#54520 = CARTESIAN_POINT ( 'NONE',  ( 20.88017736071110164, 15.35535201082150358, 2.915334737309930979 ) ) ;
#54521 = EDGE_LOOP ( 'NONE', ( #905, #7911, #50594, #29968 ) ) ;
#54522 = CARTESIAN_POINT ( 'NONE',  ( 12.91533473730993009, 61.60535201082150536, -10.88017736071109987 ) ) ;
#54523 = SURFACE_STYLE_FILL_AREA ( #9034 ) ;
#54524 = CARTESIAN_POINT ( 'NONE',  ( 18.52753015748618282, 8.925597817667451750, -4.923371831947291888 ) ) ;
#54525 = CARTESIAN_POINT ( 'NONE',  ( 0.5774900079438590739, 62.64701867748817676, -5.440088680355550821 ) ) ;
#54527 = VERTEX_POINT ( 'NONE', #33545 ) ;
#54526 = CARTESIAN_POINT ( 'NONE',  ( 2.791683348922237240, 0.3839311510007847872, -7.208316651077763204 ) ) ;
#54528 =( BOUNDED_CURVE ( )  B_SPLINE_CURVE ( 2, ( #11305, #63313, #57293, #80297, #27283, #63800, #10824, #88288, #34786 ),
 .UNSPECIFIED., .F., .F. ) 
 B_SPLINE_CURVE_WITH_KNOTS ( ( 3, 2, 2, 2, 3 ),
 ( 0.6882284501891250406, 0.6904761904761904656, 0.6964285714285713969, 0.7023809523809523281, 0.7046286926680177531 ),
 .UNSPECIFIED. ) 
 CURVE ( )  GEOMETRIC_REPRESENTATION_ITEM ( )  RATIONAL_B_SPLINE_CURVE ( ( 0.9839835555609424134, 0.9871328979762474809, 1.000000000000000000, 0.9659258262890683122, 1.000000000000000000, 0.9659258262890683122, 1.000000000000000000, 0.9871328979762477029, 0.9839835555609425244 ) ) 
 REPRESENTATION_ITEM ( '' )  );
#54529 =( GEOMETRIC_REPRESENTATION_CONTEXT ( 3 ) GLOBAL_UNCERTAINTY_ASSIGNED_CONTEXT ( ( #96504 ) ) GLOBAL_UNIT_ASSIGNED_CONTEXT ( ( #80794, #35779, #27285 ) ) REPRESENTATION_CONTEXT ( 'NONE', 'WORKASPACE' ) );
#54530 = EDGE_CURVE ( 'NONE', #32093, #44664, #10572, .T. ) ;
#54531 = CARTESIAN_POINT ( 'NONE',  ( 18.52753015748617571, 38.09226448433412315, 4.923371831947298993 ) ) ;
#54532 = ORIENTED_EDGE ( 'NONE', *, *, #8840, .F. ) ;
#54533 = ORIENTED_EDGE ( 'NONE', *, *, #32843, .F. ) ;
#54534 = CARTESIAN_POINT ( 'NONE',  ( 19.72487221294570858, 0.5000000000000000000, -6.500000000000000888 ) ) ;
#54535 = CARTESIAN_POINT ( 'NONE',  ( 3.836325488036075981, 14.49999999999999112, 14.50112432709431687 ) ) ;
#54536 = CARTESIAN_POINT ( 'NONE',  ( 0.6178305044545818747, 58.49863466993042493, -9.382169495545419124 ) ) ;
#54537 = CARTESIAN_POINT ( 'NONE',  ( 22.26659068614894466, 8.887082168247300018, 7.082119434687054849 ) ) ;
#54538 = CARTESIAN_POINT ( 'NONE',  ( -0.3689425029237898834, 16.17874883491396076, -10.36894250292378850 ) ) ;
#54539 = CARTESIAN_POINT ( 'NONE',  ( 18.18329248733321535, 57.60290668512018897, 6.500000000000005329 ) ) ;
#54540 = CARTESIAN_POINT ( 'NONE',  ( 18.72515096720570327, 11.07228050351031712, -6.499999999999992006 ) ) ;
#54541 = CARTESIAN_POINT ( 'NONE',  ( 0.5774900079438607392, 23.48035201082150536, 5.440088680355550821 ) ) ;
#54542 = CARTESIAN_POINT ( 'NONE',  ( 6.000000000000000000, 61.50000000000000711, -6.500000000000000888 ) ) ;
#54543 = VERTEX_POINT ( 'NONE', #64041 ) ;
#54544 = CARTESIAN_POINT ( 'NONE',  ( 19.84674366389459621, 8.508931151000785675, 7.409399052514197653E-17 ) ) ;
#54545 = CARTESIAN_POINT ( 'NONE',  ( 0.1532563361054083140, 6.008931151000784787, 1.131784320476157264E-15 ) ) ;
#54546 = CARTESIAN_POINT ( 'NONE',  ( -1.099225684535947600, 29.54030133659708923, 6.408140936763237150 ) ) ;
#54547 = CARTESIAN_POINT ( 'NONE',  ( 10.00000000000000000, 29.75893115100078745, -9.846743663894594434 ) ) ;
#54548 = FACE_OUTER_BOUND ( 'NONE', #15708, .T. ) ;
#54549 = CARTESIAN_POINT ( 'NONE',  ( 22.81628187352648496, 21.83196800326374643, -3.434112377981050290 ) ) ;
#54550 = FACE_OUTER_BOUND ( 'NONE', #75585, .T. ) ;
#54551 = AXIS2_PLACEMENT_3D ( 'NONE', #94062, #1614, #63065 ) ;
#54552 = AXIS2_PLACEMENT_3D ( 'NONE', #1816, #62780, #32768 ) ;
#54553 = CARTESIAN_POINT ( 'NONE',  ( 17.20831665107776587, 2.883931151000785231, 7.208316651077764980 ) ) ;
#54554 = ORIENTED_EDGE ( 'NONE', *, *, #71268, .F. ) ;
#54555 = ORIENTED_EDGE ( 'NONE', *, *, #92397, .F. ) ;
#54556 = CARTESIAN_POINT ( 'NONE',  ( 15.44008868035555793, 41.39701867748817676, -9.422509992056140149 ) ) ;
#54557 = CARTESIAN_POINT ( 'NONE',  ( 22.26659068614894466, 38.88708216824731068, 7.082119434687054849 ) ) ;
#54558 = CARTESIAN_POINT ( 'NONE',  ( 0.1532563361054082862, 41.21726448433411605, 2.638427012816831674 ) ) ;
#54559 = CARTESIAN_POINT ( 'NONE',  ( 1.472469842513823179, 1.425597817667451528, 4.923371831947296329 ) ) ;
#54560 = CIRCLE ( 'NONE', #49778, 0.5000000000000000000 ) ;
#54562 = CARTESIAN_POINT ( 'NONE',  ( -6.841090228438033272, -58.65898919720570603, -3.750000000000000000 ) ) ;
#54561 = CARTESIAN_POINT ( 'NONE',  ( 13.43411237798106583, 52.66530133659708213, -12.81628187352647252 ) ) ;
#54563 = CARTESIAN_POINT ( 'NONE',  ( 7.084665262690076126, 27.02201867748817676, -10.88017736071110164 ) ) ;
#54564 = DIRECTION ( 'NONE',  ( 0.000000000000000000, 0.000000000000000000, -1.000000000000000000 ) ) ;
#54565 = EDGE_CURVE ( 'NONE', #70171, #74723, #2608, .T. ) ;
#54566 = CARTESIAN_POINT ( 'NONE',  ( 3.591859063236763294, 8.290301336597087456, -11.09922568453595026 ) ) ;
#54567 = CARTESIAN_POINT ( 'NONE',  ( 1.472469842513823179, 35.59226448433412315, -4.923371831947296329 ) ) ;
#54568 = CARTESIAN_POINT ( 'NONE',  ( -10.88017736071109987, -1.727981322511823015, 2.915334737309934532 ) ) ;
#54569 = CARTESIAN_POINT ( 'NONE',  ( 22.81628187352648496, 51.83196800326376064, -3.434112377981050290 ) ) ;
#54570 = PRESENTATION_STYLE_ASSIGNMENT (( #39103 ) ) ;
#54571 = TOROIDAL_SURFACE ( 'NONE', #51367, 1.000000000000000000, 0.5000000000000000000 ) ;
#54573 = CARTESIAN_POINT ( 'NONE',  ( 19.72487221294570858, 46.86607318730077054, 6.500000000000000888 ) ) ;
#54572 = CARTESIAN_POINT ( 'NONE',  ( 17.96484262340118221, 49.93868534415484106, 7.964842623401181321 ) ) ;
#54574 = ADVANCED_FACE ( 'NONE', ( #47587 ), #39608, .T. ) ;
#54575 = CARTESIAN_POINT ( 'NONE',  ( 67.06412365047464164, 14.00000000000001243, 10.00000000000000000 ) ) ;
#54576 = PRESENTATION_STYLE_ASSIGNMENT (( #62074 ) ) ;
#54577 = CARTESIAN_POINT ( 'NONE',  ( 0.5774900079438607392, 53.48035201082151247, 5.440088680355550821 ) ) ;
#54578 = CARTESIAN_POINT ( 'NONE',  ( 12.91533473730992121, 59.52201867748816966, 10.88017736071110164 ) ) ;
#54579 = FACE_OUTER_BOUND ( 'NONE', #41902, .T. ) ;
#54580 = CARTESIAN_POINT ( 'NONE',  ( 10.00000000000000178, 64.31368534415483396, 10.88017736071110342 ) ) ;
#54581 = CARTESIAN_POINT ( 'NONE',  ( 19.42250999205614548, 15.98035201082150714, -5.440088680355545492 ) ) ;
#54582 = CARTESIAN_POINT ( 'NONE',  ( 7.361572987183170547, 47.05059781766745175, 9.846743663894590881 ) ) ;
#54584 = PLANE ( 'NONE',  #52719 ) ;
#54583 = CARTESIAN_POINT ( 'NONE',  ( 4.559911319644449179, 17.23035201082150536, -9.422509992056141925 ) ) ;
#54585 = CARTESIAN_POINT ( 'NONE',  ( 13.43411237798105340, 25.58196800326374998, 12.81628187352647963 ) ) ;
#54586 = ORIENTED_EDGE ( 'NONE', *, *, #94487, .T. ) ;
#54587 = CARTESIAN_POINT ( 'NONE',  ( 10.00000000000000178, 39.31368534415484106, 10.88017736071110342 ) ) ;
#54588 = ADVANCED_FACE ( 'NONE', ( #54579 ), #78081, .T. ) ;
#54590 = CARTESIAN_POINT ( 'NONE',  ( 2.603489959281613420, 50.43575266056826933, -6.500000000000031086 ) ) ;
#54589 = CARTESIAN_POINT ( 'NONE',  ( 22.81628187352647785, 11.62363466993042138, 6.195893100308588602E-16 ) ) ;
#54591 = CARTESIAN_POINT ( 'NONE',  ( -0.8801773607111009756, 13.06368534415483929, 1.068504757029289695E-15 ) ) ;
#54592 = CARTESIAN_POINT ( 'NONE',  ( 0.5774900079438607392, 43.48035201082151247, 5.440088680355550821 ) ) ;
#54593 = CARTESIAN_POINT ( 'NONE',  ( 20.36894250292379382, 53.67874883491397497, 10.36894250292379205 ) ) ;
#54594 = CARTESIAN_POINT ( 'NONE',  ( 10.00000000000000178, 27.25893115100078390, 9.846743663894594434 ) ) ;
#54595 = CARTESIAN_POINT ( 'NONE',  ( 20.88017736071110164, 65.35535201082150536, 2.915334737309930979 ) ) ;
#54596 = FACE_OUTER_BOUND ( 'NONE', #65561, .T. ) ;
#54597 = CARTESIAN_POINT ( 'NONE',  ( 17.08211943468705840, 10.13708216824730179, -12.26659068614894466 ) ) ;
#54598 = ORIENTED_EDGE ( 'NONE', *, *, #68322, .T. ) ;
#54599 = EDGE_LOOP ( 'NONE', ( #96498, #58451, #35270, #679 ) ) ;
#54600 = CIRCLE ( 'NONE', #72160, 0.2500000000000002220 ) ;
#54601 = CARTESIAN_POINT ( 'NONE',  ( 17.08211943468705130, 38.47041550158063217, 12.26659068614894998 ) ) ;
#54602 = CARTESIAN_POINT ( 'NONE',  ( 22.26659068614894466, 33.88708216824730357, 7.082119434687054849 ) ) ;
#54603 = CARTESIAN_POINT ( 'NONE',  ( 7.361572987183169658, -0.03273551566588185635, -9.846743663894592657 ) ) ;
#54604 = CARTESIAN_POINT ( 'NONE',  ( 1.472469842513823179, 61.42559781766745175, 4.923371831947296329 ) ) ;
#54605 = CARTESIAN_POINT ( 'NONE',  ( -10.79671963678341484, -44.59934526487723616, 3.750000000000000000 ) ) ;
#54607 = CARTESIAN_POINT ( 'NONE',  ( 21.09922568453594849, 21.20696800326375353, 6.408140936763242479 ) ) ;
#54606 = CARTESIAN_POINT ( 'NONE',  ( 10.00000000000000178, 54.31368534415484106, 10.88017736071110342 ) ) ;
#54608 = CARTESIAN_POINT ( 'NONE',  ( -4.164238869374099039, 36.80374883491396787, 8.674139862899312516E-16 ) ) ;
#54609 = CARTESIAN_POINT ( 'NONE',  ( 19.42250999205614548, 20.98035201082150891, -5.440088680355545492 ) ) ;
#54610 = CARTESIAN_POINT ( 'NONE',  ( 19.42250999205614548, 25.98035201082150891, -5.440088680355545492 ) ) ;
#54611 = CARTESIAN_POINT ( 'NONE',  ( 20.32896413005680358, 4.745456701841137992, 5.963430220938287007 ) ) ;
#54612 = CARTESIAN_POINT ( 'NONE',  ( 17.96484262340118221, 51.18868534415483396, -7.964842623401177768 ) ) ;
#54613 = CARTESIAN_POINT ( 'NONE',  ( -3.469446951953614189E-15, -5.241068848999205443, -9.846743663894594434 ) ) ;
#54614 = ORIENTED_EDGE ( 'NONE', *, *, #64037, .T. ) ;
#54615 = ORIENTED_EDGE ( 'NONE', *, *, #14741, .T. ) ;
#54616 = CARTESIAN_POINT ( 'NONE',  ( 13.99999999999999822, 60.50000000000000000, 6.000000000000000000 ) ) ;
#54617 = VERTEX_POINT ( 'NONE', #33062 ) ;
#54618 = CARTESIAN_POINT ( 'NONE',  ( 22.26659068614895176, 9.720415501580633943, -7.082119434687042414 ) ) ;
#54620 = CARTESIAN_POINT ( 'NONE',  ( -0.3689425029237898834, 66.17874883491396076, -10.36894250292378850 ) ) ;
#54619 = CARTESIAN_POINT ( 'NONE',  ( -4.164238869374099927, 62.01208216824728936, 3.795296366450308767 ) ) ;
#54622 = CARTESIAN_POINT ( 'NONE',  ( 10.00000000000000178, 62.25893115100078745, 9.846743663894594434 ) ) ;
#54621 = CARTESIAN_POINT ( 'NONE',  ( 0.1532563361054083140, 41.00893115100078745, 1.131784320476157264E-15 ) ) ;
#54623 = CARTESIAN_POINT ( 'NONE',  ( -13.21382278599129023, 15.00000000000000711, -6.271621331965704371 ) ) ;
#54624 = CARTESIAN_POINT ( 'NONE',  ( 14.49999999999999822, 11.50000000000000000, 6.500000000000000888 ) ) ;
#54625 = EDGE_CURVE ( 'NONE', #32525, #2388, #16603, .T. ) ;
#54626 = AXIS2_PLACEMENT_3D ( 'NONE', #75410, #91897, #22431 ) ;
#54627 = EDGE_CURVE ( 'NONE', #32382, #18106, #85094, .T. ) ;
#54628 = CARTESIAN_POINT ( 'NONE',  ( -2.816281873526471635, -1.084698663402913210, -3.434112377981056508 ) ) ;
#54629 = VERTEX_POINT ( 'NONE', #2114 ) ;
#54630 = VECTOR ( 'NONE', #27226, 1000.000000000000114 ) ;
#54631 = TOROIDAL_SURFACE ( 'NONE', #11533, 14.49999999999999822, 0.5000000000000000000 ) ;
#54632 = CARTESIAN_POINT ( 'NONE',  ( 22.26659068614894466, 48.88708216824730357, 7.082119434687054849 ) ) ;
#54633 = ORIENTED_EDGE ( 'NONE', *, *, #7823, .F. ) ;
#54634 = CARTESIAN_POINT ( 'NONE',  ( 20.36894250292379382, 43.67874883491397497, 10.36894250292379205 ) ) ;
#54635 = ORIENTED_EDGE ( 'NONE', *, *, #12002, .F. ) ;
#54636 = CARTESIAN_POINT ( 'NONE',  ( 17.96484262340118221, 21.18868534415483396, -7.964842623401177768 ) ) ;
#54637 = CARTESIAN_POINT ( 'NONE',  ( 19.42250999205614193, 40.14701867748817676, 5.440088680355555262 ) ) ;
#54638 = CARTESIAN_POINT ( 'NONE',  ( 12.63842701281683922, 54.55059781766745175, -9.846743663894590881 ) ) ;
#54639 = CARTESIAN_POINT ( 'NONE',  ( 17.96484262340118221, 34.93868534415482685, 7.964842623401181321 ) ) ;
#54640 = COLOUR_RGB ( '', 0.09019608, 0.27058824, 0.51372549) ;
#54641 = EDGE_CURVE ( 'NONE', #54903, #87966, #39111, .T. ) ;
#54642 = CARTESIAN_POINT ( 'NONE',  ( -0.8801773607110991993, 67.85535201082151957, -2.915334737309923874 ) ) ;
#54643 = CARTESIAN_POINT ( 'NONE',  ( 10.00000000000000178, 24.31368534415484106, 10.88017736071110342 ) ) ;
#54644 = STYLED_ITEM ( 'NONE', ( #4774 ), #73259 ) ;
#54645 = FACE_OUTER_BOUND ( 'NONE', #98583, .T. ) ;
#54646 = EDGE_CURVE ( 'NONE', #38899, #96234, #12124, .T. ) ;
#54647 = CARTESIAN_POINT ( 'NONE',  ( -6.732636091893173358, -88.11213685669365248, 2.750000000000000000 ) ) ;
#54648 = ORIENTED_EDGE ( 'NONE', *, *, #91343, .T. ) ;
#54649 = CARTESIAN_POINT ( 'NONE',  ( 9.112672642476784546, -7.236390792806629335, 4.000000000000000000 ) ) ;
#54650 = CARTESIAN_POINT ( 'NONE',  ( 12.63842701281683922, 29.55059781766745175, -9.846743663894590881 ) ) ;
#54651 = CARTESIAN_POINT ( 'NONE',  ( -46.48609177761492361, 103.4075268915744630, 6.315643502655008845 ) ) ;
#54652 = CARTESIAN_POINT ( 'NONE',  ( 0.6178305044545818747, 48.49863466993042493, -9.382169495545419124 ) ) ;
#54653 = EDGE_CURVE ( 'NONE', #66421, #85266, #80799, .T. ) ;
#54654 = FACE_OUTER_BOUND ( 'NONE', #126, .T. ) ;
#54655 = DIRECTION ( 'NONE',  ( 0.000000000000000000, 0.000000000000000000, -1.000000000000000000 ) ) ;
#54656 = ORIENTED_EDGE ( 'NONE', *, *, #96782, .T. ) ;
#54657 = DIRECTION ( 'NONE',  ( -0.000000000000000000, -1.000000000000000000, -0.000000000000000000 ) ) ;
#54658 = CARTESIAN_POINT ( 'NONE',  ( 1.274849032794292736, 52.55509018479936856, -6.499999999999977796 ) ) ;
#54659 = CARTESIAN_POINT ( 'NONE',  ( 1.472469842513823179, 51.42559781766745886, 4.923371831947296329 ) ) ;
#54660 = CARTESIAN_POINT ( 'NONE',  ( 10.00000000000000178, 43.05374883491397497, 14.16423886937410082 ) ) ;
#54661 = CARTESIAN_POINT ( 'NONE',  ( 14.92337183194729633, 57.67559781766745886, 8.527530157486181039 ) ) ;
#54662 = CARTESIAN_POINT ( 'NONE',  ( 19.84674366389459266, 23.71726448433412315, -2.638427012816827677 ) ) ;
#54663 = CARTESIAN_POINT ( 'NONE',  ( 13.43411237798106583, 47.66530133659709634, -12.81628187352647252 ) ) ;
#54664 = CARTESIAN_POINT ( 'NONE',  ( 1.472469842513823179, 56.42559781766745886, 4.923371831947296329 ) ) ;
#54665 = CARTESIAN_POINT ( 'NONE',  ( 0.5774900079438607392, 53.48035201082151247, 5.440088680355550821 ) ) ;
#54666 = CARTESIAN_POINT ( 'NONE',  ( 19.84674366389459266, 48.30059781766745175, 2.638427012816836559 ) ) ;
#54667 = CARTESIAN_POINT ( 'NONE',  ( 12.79413655343692469, 14.76984915707685886, 7.715718893782970156 ) ) ;
#54668 = CARTESIAN_POINT ( 'NONE',  ( 10.00000000000000000, 56.81368534415484106, -10.88017736071110342 ) ) ;
#54669 = ORIENTED_EDGE ( 'NONE', *, *, #79343, .F. ) ;
#54670 = CARTESIAN_POINT ( 'NONE',  ( -0.3689425029237881626, 52.42874883491396076, 10.36894250292379027 ) ) ;
#54671 = FILL_AREA_STYLE_COLOUR ( '', #41667 ) ;
#54672 = CARTESIAN_POINT ( 'NONE',  ( 20.88017736071110164, 25.35535201082150891, 2.915334737309930979 ) ) ;
#54674 = CARTESIAN_POINT ( 'NONE',  ( 19.42250999205614193, 55.14701867748817676, 5.440088680355555262 ) ) ;
#54673 = CARTESIAN_POINT ( 'NONE',  ( 13.43411237798106583, 12.66530133659708746, -12.81628187352647252 ) ) ;
#54675 = CARTESIAN_POINT ( 'NONE',  ( -6.982525766850298687, -88.11956318484570261, -2.750000000000000444 ) ) ;
#54676 = CARTESIAN_POINT ( 'NONE',  ( 19.72487221294570858, 0.000000000000000000, -6.500000000000000888 ) ) ;
#54677 = CARTESIAN_POINT ( 'NONE',  ( 13.07751017357376888, 15.00000000000000000, 6.263284095430594611 ) ) ;
#54679 = LINE ( 'NONE', #77683, #16909 ) ;
#54678 = CARTESIAN_POINT ( 'NONE',  ( -0.8801773607111009756, 48.06368534415484817, 1.068504757029289695E-15 ) ) ;
#54680 = CARTESIAN_POINT ( 'NONE',  ( 1.472469842513823179, 40.59226448433411605, -4.923371831947296329 ) ) ;
#54681 = DIRECTION ( 'NONE',  ( -0.8320502943378436100, 0.5547001962252291474, -0.000000000000000000 ) ) ;
#54682 = CARTESIAN_POINT ( 'NONE',  ( -7.082119434687044190, 27.63708216824731068, 12.26659068614894998 ) ) ;
#54683 = CARTESIAN_POINT ( 'NONE',  ( 3.591859063236761518, 4.956968003263753531, 11.09922568453594849 ) ) ;
#54685 = CARTESIAN_POINT ( 'NONE',  ( 0.2751277870542967463, 69.50000000000000000, -6.500000000000000888 ) ) ;
#54684 = CARTESIAN_POINT ( 'NONE',  ( 20.88017736071110519, 15.56368534415483751, 2.639326808657452039E-16 ) ) ;
#54686 = CARTESIAN_POINT ( 'NONE',  ( 24.16423886937410614, 34.30374883491396787, 8.672049930838204340E-16 ) ) ;
#54687 = EDGE_CURVE ( 'NONE', #49707, #39559, #9092, .T. ) ;
#54688 = CARTESIAN_POINT ( 'NONE',  ( -4.164238869374099039, 66.80374883491396076, 8.674139862899312516E-16 ) ) ;
#54689 = AXIS2_PLACEMENT_3D ( 'NONE', #79920, #95930, #35897 ) ;
#54690 = CARTESIAN_POINT ( 'NONE',  ( 2.791683348922237240, 30.38393115100078390, -7.208316651077763204 ) ) ;
#54691 = CARTESIAN_POINT ( 'NONE',  ( 19.84674366389459266, 18.30059781766745175, 2.638427012816836559 ) ) ;
#54692 = CARTESIAN_POINT ( 'NONE',  ( 20.88017736071110519, 10.56368534415483751, 2.639326808657452039E-16 ) ) ;
#54693 = ORIENTED_EDGE ( 'NONE', *, *, #84787, .F. ) ;
#54694 = CARTESIAN_POINT ( 'NONE',  ( 17.20831665107776587, 42.88393115100077324, 7.208316651077764980 ) ) ;
#54695 = CARTESIAN_POINT ( 'NONE',  ( 4.559911319644449179, 28.89701867748817321, 9.422509992056141925 ) ) ;
#54696 = CARTESIAN_POINT ( 'NONE',  ( 5.076628168052703671, 56.84226448433412315, 8.527530157486179263 ) ) ;
#54698 = DIRECTION ( 'NONE',  ( -0.000000000000000000, 0.000000000000000000, 1.000000000000000000 ) ) ;
#54697 = CARTESIAN_POINT ( 'NONE',  ( -2.266590686148945544, 7.220415501580634832, 7.082119434687048631 ) ) ;
#54700 = DIRECTION ( 'NONE',  ( -1.000000000000000000, -1.636349903325072848E-16, 0.000000000000000000 ) ) ;
#54699 = B_SPLINE_CURVE_WITH_KNOTS ( 'NONE', 3,
 ( #84523, #39024, #16020, #46509 ),
 .UNSPECIFIED., .F., .F.,
 ( 4, 4 ),
 ( 3.252606517456513302E-19, 0.001036303429213085783 ),
 .UNSPECIFIED. ) ;
#54701 = AXIS2_PLACEMENT_3D ( 'NONE', #90454, #42997, #35491 ) ;
#54702 = CARTESIAN_POINT ( 'NONE',  ( 12.63842701281683034, 7.467264484334118713, 9.846743663894596210 ) ) ;
#54703 = CARTESIAN_POINT ( 'NONE',  ( 3.591859063236761518, 54.95696800326376064, 11.09922568453594849 ) ) ;
#54704 = CARTESIAN_POINT ( 'NONE',  ( 7.361572987183169658, 54.96726448433413026, -9.846743663894592657 ) ) ;
#54705 = ORIENTED_EDGE ( 'NONE', *, *, #79645, .T. ) ;
#54706 = CARTESIAN_POINT ( 'NONE',  ( 5.076628168052704559, 20.17559781766745175, -8.527530157486179263 ) ) ;
#54707 = LINE ( 'NONE', #93698, #78098 ) ;
#54708 = CARTESIAN_POINT ( 'NONE',  ( -4.164238869374099927, 67.01208216824728936, 3.795296366450308767 ) ) ;
#54709 = CARTESIAN_POINT ( 'NONE',  ( 20.88017736071110875, 55.77201867748816966, -2.915334737309920765 ) ) ;
#54710 = CARTESIAN_POINT ( 'NONE',  ( 17.08211943468705130, 3.470415501580634388, 12.26659068614894998 ) ) ;
#54711 = CARTESIAN_POINT ( 'NONE',  ( 4.559911319644449179, 62.23035201082150536, -9.422509992056141925 ) ) ;
#54712 = CARTESIAN_POINT ( 'NONE',  ( 19.84674366389459621, 38.50893115100078745, 7.409399052514197653E-17 ) ) ;
#54713 = CARTESIAN_POINT ( 'NONE',  ( 7.084665262690076126, 19.10535201082150181, 10.88017736071109987 ) ) ;
#54714 = AXIS2_PLACEMENT_3D ( 'NONE', #32801, #93312, #33292 ) ;
#54715 = CARTESIAN_POINT ( 'NONE',  ( 18.06765999051783922, 38.99127512925448968, 6.500000000000047073 ) ) ;
#54716 = CARTESIAN_POINT ( 'NONE',  ( 2.791683348922240793, 56.63393115100078035, 7.208316651077764092 ) ) ;
#54717 = AXIS2_PLACEMENT_3D ( 'NONE', #55608, #63091, #27057 ) ;
#54718 = VERTEX_POINT ( 'NONE', #10086 ) ;
#54719 = ORIENTED_EDGE ( 'NONE', *, *, #86910, .T. ) ;
#54720 = DIRECTION ( 'NONE',  ( -1.000000000000000000, -0.000000000000000000, -0.000000000000000000 ) ) ;
#54721 = CARTESIAN_POINT ( 'NONE',  ( -11.88139889192316900, -91.33459011216928047, -3.750000000000000000 ) ) ;
#54722 = CARTESIAN_POINT ( 'NONE',  ( 17.20831665107776587, 44.13393115100078745, -7.208316651077762316 ) ) ;
#54723 = CARTESIAN_POINT ( 'NONE',  ( 1.472469842513823179, 20.59226448433411960, -4.923371831947296329 ) ) ;
#54724 = CARTESIAN_POINT ( 'NONE',  ( 19.38216949554541557, 62.24863466993041072, -9.382169495545420901 ) ) ;
#54726 = CARTESIAN_POINT ( 'NONE',  ( 17.20831665107776587, 52.88393115100078035, 7.208316651077764980 ) ) ;
#54725 = CARTESIAN_POINT ( 'NONE',  ( 17.96484262340118221, 19.93868534415484106, 7.964842623401181321 ) ) ;
#54727 = DIRECTION ( 'NONE',  ( 0.000000000000000000, 1.000000000000000000, 0.000000000000000000 ) ) ;
#54728 = CARTESIAN_POINT ( 'NONE',  ( -4.164238869374099039, 41.80374883491397497, 8.674139862899312516E-16 ) ) ;
#54729 = CARTESIAN_POINT ( 'NONE',  ( 22.26659068614895176, 64.72041550158064638, -7.082119434687042414 ) ) ;
#54730 = CARTESIAN_POINT ( 'NONE',  ( 2.791683348922237240, 65.38393115100078035, -7.208316651077763204 ) ) ;
#54731 = EDGE_CURVE ( 'NONE', #42828, #26776, #20190, .T. ) ;
#54732 = DIRECTION ( 'NONE',  ( 0.5901017155109078427, 0.8073289077885689169, 0.000000000000000000 ) ) ;
#54733 = CARTESIAN_POINT ( 'NONE',  ( 7.084665262690076126, 49.10535201082149825, 10.88017736071109987 ) ) ;
#54734 = CARTESIAN_POINT ( 'NONE',  ( 5.076628168052703671, 16.84226448433411960, 8.527530157486179263 ) ) ;
#54735 = VECTOR ( 'NONE', #96495, 1000.000000000000114 ) ;
#54736 = CARTESIAN_POINT ( 'NONE',  ( -7.037696229836970296, -86.26312365674226612, 4.000000000000000000 ) ) ;
#54737 = ORIENTED_EDGE ( 'NONE', *, *, #30255, .T. ) ;
#54738 = VERTEX_POINT ( 'NONE', #31584 ) ;
#54739 = CARTESIAN_POINT ( 'NONE',  ( 5.076628168052704559, 15.17559781766745175, -8.527530157486179263 ) ) ;
#54740 = ORIENTED_EDGE ( 'NONE', *, *, #2891, .T. ) ;
#54741 = CARTESIAN_POINT ( 'NONE',  ( 20.36894250292379382, 18.67874883491397142, 10.36894250292379205 ) ) ;
#54742 = CARTESIAN_POINT ( 'NONE',  ( 18.52753015748617571, 23.09226448433411960, 4.923371831947298993 ) ) ;
#54743 = CARTESIAN_POINT ( 'NONE',  ( 7.084665262690076126, 49.10535201082149825, 10.88017736071109987 ) ) ;
#54744 = SURFACE_STYLE_USAGE ( .BOTH. , #69772 ) ;
#54745 = EDGE_CURVE ( 'NONE', #40893, #3546, #90415, .T. ) ;
#54746 = ORIENTED_EDGE ( 'NONE', *, *, #69115, .F. ) ;
#54747 = CARTESIAN_POINT ( 'NONE',  ( 15.44008868035555260, 44.73035201082151247, 9.422509992056143702 ) ) ;
#54748 = VECTOR ( 'NONE', #35716, 999.9999999999998863 ) ;
#54749 = EDGE_CURVE ( 'NONE', #7251, #71473, #56080, .T. ) ;
#54750 = EDGE_CURVE ( 'NONE', #93052, #15452, #1024, .T. ) ;
#54751 = ORIENTED_EDGE ( 'NONE', *, *, #69799, .T. ) ;
#54752 = CARTESIAN_POINT ( 'NONE',  ( -2.266590686148945544, 7.220415501580634832, 7.082119434687048631 ) ) ;
#54753 = VERTEX_POINT ( 'NONE', #42068 ) ;
#54754 = CARTESIAN_POINT ( 'NONE',  ( 22.81628187352647785, 11.62363466993042138, 6.195893100308588602E-16 ) ) ;
#54755 = FILL_AREA_STYLE_COLOUR ( '', #78076 ) ;
#54756 = CARTESIAN_POINT ( 'NONE',  ( 7.361572987183169658, 9.967264484334119601, -9.846743663894592657 ) ) ;
#54757 = PLANE ( 'NONE',  #19467 ) ;
#54758 = CARTESIAN_POINT ( 'NONE',  ( 0.6178305044545818747, 43.49863466993042493, -9.382169495545419124 ) ) ;
#54759 = DIRECTION ( 'NONE',  ( -0.000000000000000000, 0.000000000000000000, 1.000000000000000000 ) ) ;
#54760 = CARTESIAN_POINT ( 'NONE',  ( 0.1532563361054083140, 21.00893115100078745, 1.131784320476157264E-15 ) ) ;
#54761 = CARTESIAN_POINT ( 'NONE',  ( -0.8801773607111009756, 33.06368534415484106, 1.068504757029289695E-15 ) ) ;
#54762 = ORIENTED_EDGE ( 'NONE', *, *, #9284, .T. ) ;
#54763 = DIRECTION ( 'NONE',  ( 0.000000000000000000, 0.000000000000000000, 1.000000000000000000 ) ) ;
#54764 = CARTESIAN_POINT ( 'NONE',  ( 12.91533473730992121, 59.52201867748816966, 10.88017736071110164 ) ) ;
#54765 = LINE ( 'NONE', #2300, #19634 ) ;
#54766 = DIRECTION ( 'NONE',  ( 0.000000000000000000, 1.000000000000000000, 0.000000000000000000 ) ) ;
#54767 = CARTESIAN_POINT ( 'NONE',  ( 4.559911319644449179, 67.23035201082150536, -9.422509992056141925 ) ) ;
#54768 = AXIS2_PLACEMENT_3D ( 'NONE', #49128, #64599, #32646 ) ;
#54769 = COLOUR_RGB ( '', 0.09019608, 0.27058824, 0.51372549) ;
#54770 = CARTESIAN_POINT ( 'NONE',  ( 3.591859063236763294, 8.290301336597087456, -11.09922568453595026 ) ) ;
#54771 = ADVANCED_FACE ( 'NONE', ( #5044 ), #87212, .T. ) ;
#54773 = CARTESIAN_POINT ( 'NONE',  ( -3.750000000000000000, 36.75000000000000000, 2.750000000000000000 ) ) ;
#54772 = PRESENTATION_LAYER_ASSIGNMENT (  '', '', ( #94684 ) ) ;
#54774 = CARTESIAN_POINT ( 'NONE',  ( 7.361572987183169658, 29.96726448433411960, -9.846743663894592657 ) ) ;
#54775 = CARTESIAN_POINT ( 'NONE',  ( -2.816281873526471635, 58.91530133659707502, -3.434112377981056508 ) ) ;
#54776 = CARTESIAN_POINT ( 'NONE',  ( 6.204703633549690345, 12.84541550158063572, 14.16423886937410082 ) ) ;
#54777 = CARTESIAN_POINT ( 'NONE',  ( 12.63842701281683034, 22.46726448433411605, 9.846743663894596210 ) ) ;
#54778 =( GEOMETRIC_REPRESENTATION_CONTEXT ( 3 ) GLOBAL_UNCERTAINTY_ASSIGNED_CONTEXT ( ( #12275 ) ) GLOBAL_UNIT_ASSIGNED_CONTEXT ( ( #83322, #71763, #40783 ) ) REPRESENTATION_CONTEXT ( 'NONE', 'WORKASPACE' ) );
#54779 = CARTESIAN_POINT ( 'NONE',  ( -1.099225684535947600, 13.70696800326375353, -6.408140936763238038 ) ) ;
#54780 = FACE_OUTER_BOUND ( 'NONE', #64165, .T. ) ;
#54781 = CARTESIAN_POINT ( 'NONE',  ( 0.5774900079438607392, 43.48035201082151247, 5.440088680355550821 ) ) ;
#54782 = CARTESIAN_POINT ( 'NONE',  ( 5.076628168052703671, 56.84226448433412315, 8.527530157486179263 ) ) ;
#54783 = CARTESIAN_POINT ( 'NONE',  ( 20.15039907845753220, 51.74884699246889852, 6.262539305110077059 ) ) ;
#54784 = CARTESIAN_POINT ( 'NONE',  ( 17.20831665107776587, 34.13393115100078745, -7.208316651077762316 ) ) ;
#54785 = CARTESIAN_POINT ( 'NONE',  ( 0.1532563361054100626, 25.80059781766744820, -2.638427012816831230 ) ) ;
#54786 = CARTESIAN_POINT ( 'NONE',  ( 19.42250999205614548, 15.98035201082150714, -5.440088680355545492 ) ) ;
#54787 = CARTESIAN_POINT ( 'NONE',  ( 22.81628187352647785, 21.62363466993041783, 6.195893100308588602E-16 ) ) ;
#54788 = CARTESIAN_POINT ( 'NONE',  ( 12.63842701281683034, 27.46726448433411250, 9.846743663894596210 ) ) ;
#54789 = CARTESIAN_POINT ( 'NONE',  ( -4.000000000000000000, 78.07179676972445748, 4.250000000000000000 ) ) ;
#54790 = CARTESIAN_POINT ( 'NONE',  ( 10.00000000000000000, 16.81368534415483751, -10.88017736071110342 ) ) ;
#54791 = CARTESIAN_POINT ( 'NONE',  ( -0.3289641300568005855, 49.27164270246084499, -5.963430220938281678 ) ) ;
#54793 = CARTESIAN_POINT ( 'NONE',  ( 19.42250999205614548, 15.98035201082150714, -5.440088680355545492 ) ) ;
#54792 = CARTESIAN_POINT ( 'NONE',  ( 0.1532563361054100626, 45.80059781766745886, -2.638427012816831230 ) ) ;
#54794 = CARTESIAN_POINT ( 'NONE',  ( 2.035157376598824452, 38.68868534415483396, 7.964842623401179544 ) ) ;
#54796 = FILL_AREA_STYLE ('',( #24336 ) ) ;
#54795 = CARTESIAN_POINT ( 'NONE',  ( 15.44008868035555793, 6.397018677488171434, -9.422509992056140149 ) ) ;
#54797 = CARTESIAN_POINT ( 'NONE',  ( 12.63842701281683922, 19.55059781766745175, -9.846743663894590881 ) ) ;
#54798 =( BOUNDED_SURFACE ( )  B_SPLINE_SURFACE ( 1, 2, ( 
 ( #68286, #89779, #60759, #52280, #36293, #44769, #91259, #22785, #89294, #20804, #81778, #43780, #74272, #21296, #51788, #82275, #19142, #58610, #88120, #97139, #5628, #57622, #50122, #73107, #58104, #28110, #5130, #12128, #96136, #89607, #27121, #59098, #88610, #19631, #27617, #96634, #42151, #80632, #42629, #4648, #89112, #20120, #65113, #49618, #79647, #35110, #36106, #65609, #50623, #12616, #81114, #73605, #43117, #21117, #72132, #35620, #20624, #66104, #51113, #72616, #66611, #81601, #13112, #34123, #80129, #11636, #28609, #64615, #43608, #11145, #74095, #87628, #57131, #41664, #3659, #95125, #4151, #26633, #34616, #95634, #37113, #82597, #84086, #76082, #46085, #92073, #51616, #7103, #30571, #13611, #91586, #44091, #91079, #38586, #74601, #29094, #44597, #6600, #67610, #22604, #53082, #7610, #90584, #22109, #25562, #86546, #18053, #96020, #18538, #49029, #98009, #45971, #36498, #21999, #28976, #68479, #98508, #66990, #29962, #43977, #14499, #52474, #29463, #59969, #97513, #22489, #83473, #6003, #82979, #28498, #14995, #76461, #60468, #52962, #58992, #90957, #74480, #90463, #74980, #75474, #59479, #51994, #5, #89980, #82483, #7492, #45465, #6484, #6989, #36991, #7976, #75965, #30454, #66494, #60953, #21005, #91462, #67487, #22988, #97021, #53454, #51492, #13498, #61937, #38962, #69455, #93429, #62423, #1960, #499, #47431, #84945, #48416, #40443, #32426, #23483, #31923, #39940, #62927, #16947, #78918, #9940, #38475, #55434, #31435, #70944, #9439, #77931, #85940, #76946, #2462, #1469, #24458, #24951, #30948, #68968, #8941, #70443, #54924, #23962, #25449, #85440, #17451, #32918, #61447, #86432, #92439, #973, #47918, #78423, #63419, #55932, #16456, #54436, #93923, #91953, #46936, #53956, #39459, #84463, #15961, #8456, #46453, #77429, #69950, #41441, #71901, #73372, #95396, #49886, #95904, #65376, #4416, #57392, #3425, #26897, #27875, #63895, #88881, #41925, #19887, #49395, #27385, #87882, #57876, #19400, #50881, #25923, #72387, #42891, #56897, #18918, #33884, #58362, #11900, #79896, #56425, #64389, #94899, #86911, #18421, #88388, #87402, #35380, #89370, #58867, #44355, #67361, #98385, #20882, #29349, #74859, #14374, #66866, #28851, #83351, #37373, #7368, #98879, #60836, #13874, #29840, #22863, #52843, #12871, #59850, #37867, #73869, #59356, #21373, #68360, #35872, #90339, #82854, #44842, #66362, #96898, #51869, #82353, #69833, #84349, #92325, #53840, #84828, #93797, #23357, #1354, #23848, #93304, #7855, #859, #77802, #91841, #31807, #83843, #70328, #1842, #78300, #31318, #16335, #9818, #85815, #54803, #16826, #32300 ),
 ( #38355, #62804, #68848, #24828, #17328, #40319, #381, #70823, #61329, #66626, #50137, #25806, #19645, #13125, #50638, #20637, #86307, #66119, #73121, #36635, #59110, #51126, #40810, #20134, #28127, #43622, #5143, #6129, #97155, #67118, #5642, #80646, #51633, #96648, #58627, #44104, #33281, #74615, #55812, #58117, #17810, #94284, #63774, #12140, #42645, #4663, #35125, #65624, #27632, #53588, #84102, #59610, #15618, #75109, #91093, #75605, #60598, #6615, #52605, #31081, #67624, #37129, #633, #46102, #68116, #53099, #60096, #39097, #83609, #76587, #97643, #15124, #82612, #136, #98642, #54079, #46581, #76097, #98133, #8105, #14635, #29594, #30091, #23615, #45599, #84596, #14128, #44613, #9573, #79551, #18555, #94054, #47066, #25090, #2595, #56068, #48048, #49047, #41069, #11050, #1108, #55058, #92572, #40573, #78562, #77564, #39594, #32055, #32560, #17583, #2101, #34025, #51509, #12032, #20022, #35011, #27027, #28513, #65512, #20525, #36009, #64522, #89510, #57526, #72521, #51010, #13009, #96034, #59007, #50522, #81019, #74004, #97038, #42058, #12521, #43023, #95028, #26537, #80032, #43506, #87535, #73506, #4055, #5030, #5529, #35517, #66008, #28011, #96536, #21020, #19048, #49525, #98526, #30966, #36515, #23499, #29979, #53471, #60484, #37007, #15506, #15011, #14016, #13513, #98023, #91482, #97528, #59986, #22015, #52489, #76477, #22, #83981, #45988, #61463, #67007, #89996, #21512, #33839, #95858, #40403, #57835, #79371, #87841, #64348, #40891, #80353, #79857, #48372, #49355, #55890, #26358, #94856, #10876, #41400, #78876, #34338, #95352, #17889, #56858, #70898, #26851, #27342, #11360, #64833, #2417, #41879, #86387, #71866, #56383, #3377, #10386, #33357, #11851, #71392, #2906, #19360, #57348, #86872, #87359, #63852, #88344, #18873, #72342, #19842, #3875, #32874, #49844, #25884, #34837, #78380, #42361, #94365, #72834, #18382, #48861, #4372, #65332, #9900, #63372, #93877, #25404, #28332, #60309, #52317, #13833, #35335, #43816, #51825, #44314, #28816, #29800, #82810, #90802, #67321, #43330, #14330, #21335, #59315, #97844, #88837, #44803, #13332, #74311, #74815, #12342, #50332, #20840, #89814, #5838, #35834, #37335, #36328, #29309, #75308, #42848, #98342, #5355, #81333, #59805, #90299, #66823, #67825, #58822, #66321, #6819, #80845, #50841, #97345, #51332, #73332, #82312, #81814, #6320, #4859, #12830, #36829, #65828, #96360, #27833, #58319, #20345, #91294, #22329, #91798, #47265, #76785, #61289, #54273, #8302, #16298, #69298, #1803, #14833, #23319, #62264, #68809, #53801, #15330, #77767, #92288, #84312, #75804, #22817, #53297 ) ),
 .UNSPECIFIED., .F., .F., .T. ) 
 B_SPLINE_SURFACE_WITH_KNOTS ( ( 2, 2 ),
 ( 3, 2, 2, 2, 2, 2, 2, 2, 2, 2, 2, 2, 2, 2, 2, 2, 2, 2, 2, 2, 2, 2, 2, 2, 2, 2, 2, 2, 2, 2, 2, 2, 2, 2, 2, 2, 2, 2, 2, 2, 2, 2, 2, 2, 2, 2, 2, 2, 2, 2, 2, 2, 2, 2, 2, 2, 2, 2, 2, 2, 2, 2, 2, 2, 2, 2, 2, 2, 2, 2, 2, 2, 2, 2, 2, 2, 2, 2, 2, 2, 2, 2, 2, 2, 2, 2, 2, 2, 2, 2, 2, 2, 2, 2, 2, 2, 2, 2, 2, 2, 2, 2, 2, 2, 2, 2, 2, 2, 2, 2, 2, 2, 2, 2, 2, 2, 2, 2, 2, 2, 2, 2, 2, 2, 2, 2, 2, 2, 2, 2, 2, 2, 2, 2, 2, 2, 2, 2, 2, 2, 2, 2, 2, 2, 2, 2, 2, 2, 2, 2, 2, 2, 2, 2, 2, 2, 2, 2, 2, 2, 2, 2, 3 ),
 ( 0.000000000000000000, 1.000000000000000000 ),
 ( 0.000000000000000000, 0.005952380952380952051, 0.01190476190476190410, 0.01785714285714285615, 0.02380952380952380820, 0.02976190476190476025, 0.03571428571428571230, 0.04166666666666666435, 0.04761904761904761640, 0.05357142857142856845, 0.05952380952380952051, 0.06547619047619047949, 0.07142857142857142461, 0.07738095238095238360, 0.08333333333333332871, 0.08928571428571428770, 0.09523809523809523281, 0.1011904761904761918, 0.1071428571428571369, 0.1130952380952380959, 0.1190476190476190410, 0.1250000000000000000, 0.1309523809523809590, 0.1369047619047619180, 0.1428571428571428492, 0.1488095238095238082, 0.1547619047619047672, 0.1607142857142857262, 0.1666666666666666574, 0.1726190476190476164, 0.1785714285714285754, 0.1845238095238095344, 0.1904761904761904656, 0.1964285714285714246, 0.2023809523809523836, 0.2083333333333333426, 0.2142857142857142738, 0.2202380952380952328, 0.2261904761904761918, 0.2321428571428571508, 0.2380952380952380820, 0.2440476190476190410, 0.2500000000000000000, 0.2559523809523809312, 0.2619047619047619180, 0.2678571428571428492, 0.2738095238095238360, 0.2797619047619047672, 0.2857142857142856984, 0.2916666666666666852, 0.2976190476190476164, 0.3035714285714285476, 0.3095238095238095344, 0.3154761904761904656, 0.3214285714285714524, 0.3273809523809523836, 0.3333333333333333148, 0.3392857142857143016, 0.3452380952380952328, 0.3511904761904761640, 0.3571428571428571508, 0.3630952380952380820, 0.3690476190476190688, 0.3750000000000000000, 0.3809523809523809312, 0.3869047619047619180, 0.3928571428571428492, 0.3988095238095238360, 0.4047619047619047672, 0.4107142857142856984, 0.4166666666666666852, 0.4226190476190476164, 0.4285714285714285476, 0.4345238095238095344, 0.4404761904761904656, 0.4464285714285714524, 0.4523809523809523836, 0.4583333333333333148, 0.4642857142857143016, 0.4702380952380952328, 0.4761904761904761640, 0.4821428571428571508, 0.4880952380952380820, 0.4940476190476190688, 0.5000000000000000000, 0.5059523809523809312, 0.5119047619047618625, 0.5178571428571429047, 0.5238095238095238360, 0.5297619047619047672, 0.5357142857142856984, 0.5416666666666666297, 0.5476190476190476719, 0.5535714285714286031, 0.5595238095238095344, 0.5654761904761904656, 0.5714285714285713969, 0.5773809523809523281, 0.5833333333333333703, 0.5892857142857143016, 0.5952380952380952328, 0.6011904761904761640, 0.6071428571428570953, 0.6130952380952381375, 0.6190476190476190688, 0.6250000000000000000, 0.6309523809523809312, 0.6369047619047618625, 0.6428571428571429047, 0.6488095238095238360, 0.6547619047619047672, 0.6607142857142856984, 0.6666666666666666297, 0.6726190476190476719, 0.6785714285714286031, 0.6845238095238095344, 0.6904761904761904656, 0.6964285714285713969, 0.7023809523809523281, 0.7083333333333333703, 0.7142857142857143016, 0.7202380952380952328, 0.7261904761904761640, 0.7321428571428570953, 0.7380952380952381375, 0.7440476190476190688, 0.7500000000000000000, 0.7559523809523809312, 0.7619047619047618625, 0.7678571428571429047, 0.7738095238095238360, 0.7797619047619047672, 0.7857142857142856984, 0.7916666666666666297, 0.7976190476190476719, 0.8035714285714286031, 0.8095238095238095344, 0.8154761904761904656, 0.8214285714285713969, 0.8273809523809523281, 0.8333333333333333703, 0.8392857142857143016, 0.8452380952380952328, 0.8511904761904761640, 0.8571428571428570953, 0.8630952380952381375, 0.8690476190476190688, 0.8750000000000000000, 0.8809523809523809312, 0.8869047619047618625, 0.8928571428571429047, 0.8988095238095238360, 0.9047619047619047672, 0.9107142857142856984, 0.9166666666666666297, 0.9226190476190476719, 0.9285714285714286031, 0.9345238095238095344, 0.9404761904761904656, 0.9464285714285713969, 0.9523809523809523281, 0.9583333333333333703, 0.9642857142857143016 ),
 .UNSPECIFIED. ) 
 GEOMETRIC_REPRESENTATION_ITEM ( )  RATIONAL_B_SPLINE_SURFACE ( (
 ( 1.000000000000000000, 0.9659258262890683122, 1.000000000000000000, 0.9659258262890683122, 1.000000000000000000, 0.9659258262890683122, 1.000000000000000000, 0.9659258262890683122, 1.000000000000000000, 0.9659258262890683122, 1.000000000000000000, 0.9659258262890683122, 1.000000000000000000, 0.9659258262890683122, 1.000000000000000000, 0.9659258262890683122, 1.000000000000000000, 0.9659258262890683122, 1.000000000000000000, 0.9659258262890683122, 1.000000000000000000, 0.9659258262890683122, 1.000000000000000000, 0.9659258262890683122, 1.000000000000000000, 0.9659258262890683122, 1.000000000000000000, 0.9659258262890683122, 1.000000000000000000, 0.9659258262890683122, 1.000000000000000000, 0.9659258262890683122, 1.000000000000000000, 0.9659258262890683122, 1.000000000000000000, 0.9659258262890683122, 1.000000000000000000, 0.9659258262890683122, 1.000000000000000000, 0.9659258262890683122, 1.000000000000000000, 0.9659258262890683122, 1.000000000000000000, 0.9659258262890683122, 1.000000000000000000, 0.9659258262890683122, 1.000000000000000000, 0.9659258262890683122, 1.000000000000000000, 0.9659258262890683122, 1.000000000000000000, 0.9659258262890683122, 1.000000000000000000, 0.9659258262890683122, 1.000000000000000000, 0.9659258262890683122, 1.000000000000000000, 0.9659258262890683122, 1.000000000000000000, 0.9659258262890683122, 1.000000000000000000, 0.9659258262890683122, 1.000000000000000000, 0.9659258262890683122, 1.000000000000000000, 0.9659258262890683122, 1.000000000000000000, 0.9659258262890683122, 1.000000000000000000, 0.9659258262890683122, 1.000000000000000000, 0.9659258262890683122, 1.000000000000000000, 0.9659258262890683122, 1.000000000000000000, 0.9659258262890683122, 1.000000000000000000, 0.9659258262890683122, 1.000000000000000000, 0.9659258262890683122, 1.000000000000000000, 0.9659258262890683122, 1.000000000000000000, 0.9659258262890683122, 1.000000000000000000, 0.9659258262890683122, 1.000000000000000000, 0.9659258262890683122, 1.000000000000000000, 0.9659258262890683122, 1.000000000000000000, 0.9659258262890683122, 1.000000000000000000, 0.9659258262890683122, 1.000000000000000000, 0.9659258262890683122, 1.000000000000000000, 0.9659258262890683122, 1.000000000000000000, 0.9659258262890683122, 1.000000000000000000, 0.9659258262890683122, 1.000000000000000000, 0.9659258262890683122, 1.000000000000000000, 0.9659258262890683122, 1.000000000000000000, 0.9659258262890683122, 1.000000000000000000, 0.9659258262890683122, 1.000000000000000000, 0.9659258262890683122, 1.000000000000000000, 0.9659258262890683122, 1.000000000000000000, 0.9659258262890683122, 1.000000000000000000, 0.9659258262890683122, 1.000000000000000000, 0.9659258262890683122, 1.000000000000000000, 0.9659258262890683122, 1.000000000000000000, 0.9659258262890683122, 1.000000000000000000, 0.9659258262890683122, 1.000000000000000000, 0.9659258262890683122, 1.000000000000000000, 0.9659258262890683122, 1.000000000000000000, 0.9659258262890683122, 1.000000000000000000, 0.9659258262890683122, 1.000000000000000000, 0.9659258262890683122, 1.000000000000000000, 0.9659258262890683122, 1.000000000000000000, 0.9659258262890683122, 1.000000000000000000, 0.9659258262890683122, 1.000000000000000000, 0.9659258262890683122, 1.000000000000000000, 0.9659258262890683122, 1.000000000000000000, 0.9659258262890683122, 1.000000000000000000, 0.9659258262890683122, 1.000000000000000000, 0.9659258262890683122, 1.000000000000000000, 0.9659258262890683122, 1.000000000000000000, 0.9659258262890683122, 1.000000000000000000, 0.9659258262890683122, 1.000000000000000000, 0.9659258262890683122, 1.000000000000000000, 0.9659258262890683122, 1.000000000000000000, 0.9659258262890683122, 1.000000000000000000, 0.9659258262890683122, 1.000000000000000000, 0.9659258262890683122, 1.000000000000000000, 0.9659258262890683122, 1.000000000000000000, 0.9659258262890683122, 1.000000000000000000, 0.9659258262890683122, 1.000000000000000000, 0.9659258262890683122, 1.000000000000000000, 0.9659258262890683122, 1.000000000000000000, 0.9659258262890683122, 1.000000000000000000, 0.9659258262890683122, 1.000000000000000000, 0.9659258262890683122, 1.000000000000000000, 0.9659258262890683122, 1.000000000000000000, 0.9659258262890683122, 1.000000000000000000, 0.9659258262890683122, 1.000000000000000000, 0.9659258262890683122, 1.000000000000000000, 0.9659258262890683122, 1.000000000000000000, 0.9659258262890683122, 1.000000000000000000, 0.9659258262890683122, 1.000000000000000000, 0.9659258262890683122, 1.000000000000000000, 0.9659258262890683122, 1.000000000000000000, 0.9659258262890683122, 1.000000000000000000, 0.9659258262890683122, 1.000000000000000000, 0.9659258262890683122, 1.000000000000000000, 0.9659258262890683122, 1.000000000000000000, 0.9659258262890683122, 1.000000000000000000, 0.9659258262890683122, 1.000000000000000000, 0.9659258262890683122, 1.000000000000000000, 0.9659258262890683122, 1.000000000000000000, 0.9659258262890683122, 1.000000000000000000, 0.9659258262890683122, 1.000000000000000000, 0.9659258262890683122, 1.000000000000000000, 0.9659258262890683122, 1.000000000000000000, 0.9659258262890683122, 1.000000000000000000, 0.9659258262890683122, 1.000000000000000000, 0.9659258262890683122, 1.000000000000000000, 0.9659258262890683122, 1.000000000000000000, 0.9659258262890683122, 1.000000000000000000, 0.9659258262890683122, 1.000000000000000000, 0.9659258262890683122, 1.000000000000000000, 0.9659258262890683122, 1.000000000000000000, 0.9659258262890683122, 1.000000000000000000, 0.9659258262890683122, 1.000000000000000000, 0.9659258262890683122, 1.000000000000000000, 0.9659258262890683122, 1.000000000000000000, 0.9659258262890683122, 1.000000000000000000, 0.9659258262890683122, 1.000000000000000000, 0.9659258262890683122, 1.000000000000000000, 0.9659258262890683122, 1.000000000000000000, 0.9659258262890683122, 1.000000000000000000, 0.9659258262890683122, 1.000000000000000000, 0.9659258262890683122, 1.000000000000000000, 0.9659258262890683122, 1.000000000000000000, 0.9659258262890683122, 1.000000000000000000, 0.9659258262890683122, 1.000000000000000000, 0.9659258262890683122, 1.000000000000000000, 0.9659258262890683122, 1.000000000000000000, 0.9659258262890683122, 1.000000000000000000, 0.9659258262890683122, 1.000000000000000000, 0.9659258262890683122, 1.000000000000000000, 0.9659258262890683122, 1.000000000000000000, 0.9659258262890683122, 1.000000000000000000, 0.9659258262890683122, 1.000000000000000000, 0.9659258262890683122, 1.000000000000000000, 0.9659258262890683122, 1.000000000000000000, 0.9659258262890683122, 1.000000000000000000, 0.9659258262890683122, 1.000000000000000000, 0.9659258262890683122, 1.000000000000000000, 0.9659258262890683122, 1.000000000000000000, 0.9659258262890683122, 1.000000000000000000, 0.9659258262890683122, 1.000000000000000000, 0.9659258262890683122, 1.000000000000000000, 0.9659258262890683122, 1.000000000000000000, 0.9659258262890683122, 1.000000000000000000, 0.9659258262890683122, 1.000000000000000000, 0.9659258262890683122, 1.000000000000000000, 0.9659258262890683122, 1.000000000000000000, 0.9659258262890683122, 1.000000000000000000, 0.9659258262890683122, 1.000000000000000000, 0.9659258262890683122, 1.000000000000000000, 0.9659258262890683122, 1.000000000000000000, 0.9659258262890683122, 1.000000000000000000),
 ( 1.000000000000000000, 0.9659258262890683122, 1.000000000000000000, 0.9659258262890683122, 1.000000000000000000, 0.9659258262890683122, 1.000000000000000000, 0.9659258262890683122, 1.000000000000000000, 0.9659258262890683122, 1.000000000000000000, 0.9659258262890683122, 1.000000000000000000, 0.9659258262890683122, 1.000000000000000000, 0.9659258262890683122, 1.000000000000000000, 0.9659258262890683122, 1.000000000000000000, 0.9659258262890683122, 1.000000000000000000, 0.9659258262890683122, 1.000000000000000000, 0.9659258262890683122, 1.000000000000000000, 0.9659258262890683122, 1.000000000000000000, 0.9659258262890683122, 1.000000000000000000, 0.9659258262890683122, 1.000000000000000000, 0.9659258262890683122, 1.000000000000000000, 0.9659258262890683122, 1.000000000000000000, 0.9659258262890683122, 1.000000000000000000, 0.9659258262890683122, 1.000000000000000000, 0.9659258262890683122, 1.000000000000000000, 0.9659258262890683122, 1.000000000000000000, 0.9659258262890683122, 1.000000000000000000, 0.9659258262890683122, 1.000000000000000000, 0.9659258262890683122, 1.000000000000000000, 0.9659258262890683122, 1.000000000000000000, 0.9659258262890683122, 1.000000000000000000, 0.9659258262890683122, 1.000000000000000000, 0.9659258262890683122, 1.000000000000000000, 0.9659258262890683122, 1.000000000000000000, 0.9659258262890683122, 1.000000000000000000, 0.9659258262890683122, 1.000000000000000000, 0.9659258262890683122, 1.000000000000000000, 0.9659258262890683122, 1.000000000000000000, 0.9659258262890683122, 1.000000000000000000, 0.9659258262890683122, 1.000000000000000000, 0.9659258262890683122, 1.000000000000000000, 0.9659258262890683122, 1.000000000000000000, 0.9659258262890683122, 1.000000000000000000, 0.9659258262890683122, 1.000000000000000000, 0.9659258262890683122, 1.000000000000000000, 0.9659258262890683122, 1.000000000000000000, 0.9659258262890683122, 1.000000000000000000, 0.9659258262890683122, 1.000000000000000000, 0.9659258262890683122, 1.000000000000000000, 0.9659258262890683122, 1.000000000000000000, 0.9659258262890683122, 1.000000000000000000, 0.9659258262890683122, 1.000000000000000000, 0.9659258262890683122, 1.000000000000000000, 0.9659258262890683122, 1.000000000000000000, 0.9659258262890683122, 1.000000000000000000, 0.9659258262890683122, 1.000000000000000000, 0.9659258262890683122, 1.000000000000000000, 0.9659258262890683122, 1.000000000000000000, 0.9659258262890683122, 1.000000000000000000, 0.9659258262890683122, 1.000000000000000000, 0.9659258262890683122, 1.000000000000000000, 0.9659258262890683122, 1.000000000000000000, 0.9659258262890683122, 1.000000000000000000, 0.9659258262890683122, 1.000000000000000000, 0.9659258262890683122, 1.000000000000000000, 0.9659258262890683122, 1.000000000000000000, 0.9659258262890683122, 1.000000000000000000, 0.9659258262890683122, 1.000000000000000000, 0.9659258262890683122, 1.000000000000000000, 0.9659258262890683122, 1.000000000000000000, 0.9659258262890683122, 1.000000000000000000, 0.9659258262890683122, 1.000000000000000000, 0.9659258262890683122, 1.000000000000000000, 0.9659258262890683122, 1.000000000000000000, 0.9659258262890683122, 1.000000000000000000, 0.9659258262890683122, 1.000000000000000000, 0.9659258262890683122, 1.000000000000000000, 0.9659258262890683122, 1.000000000000000000, 0.9659258262890683122, 1.000000000000000000, 0.9659258262890683122, 1.000000000000000000, 0.9659258262890683122, 1.000000000000000000, 0.9659258262890683122, 1.000000000000000000, 0.9659258262890683122, 1.000000000000000000, 0.9659258262890683122, 1.000000000000000000, 0.9659258262890683122, 1.000000000000000000, 0.9659258262890683122, 1.000000000000000000, 0.9659258262890683122, 1.000000000000000000, 0.9659258262890683122, 1.000000000000000000, 0.9659258262890683122, 1.000000000000000000, 0.9659258262890683122, 1.000000000000000000, 0.9659258262890683122, 1.000000000000000000, 0.9659258262890683122, 1.000000000000000000, 0.9659258262890683122, 1.000000000000000000, 0.9659258262890683122, 1.000000000000000000, 0.9659258262890683122, 1.000000000000000000, 0.9659258262890683122, 1.000000000000000000, 0.9659258262890683122, 1.000000000000000000, 0.9659258262890683122, 1.000000000000000000, 0.9659258262890683122, 1.000000000000000000, 0.9659258262890683122, 1.000000000000000000, 0.9659258262890683122, 1.000000000000000000, 0.9659258262890683122, 1.000000000000000000, 0.9659258262890683122, 1.000000000000000000, 0.9659258262890683122, 1.000000000000000000, 0.9659258262890683122, 1.000000000000000000, 0.9659258262890683122, 1.000000000000000000, 0.9659258262890683122, 1.000000000000000000, 0.9659258262890683122, 1.000000000000000000, 0.9659258262890683122, 1.000000000000000000, 0.9659258262890683122, 1.000000000000000000, 0.9659258262890683122, 1.000000000000000000, 0.9659258262890683122, 1.000000000000000000, 0.9659258262890683122, 1.000000000000000000, 0.9659258262890683122, 1.000000000000000000, 0.9659258262890683122, 1.000000000000000000, 0.9659258262890683122, 1.000000000000000000, 0.9659258262890683122, 1.000000000000000000, 0.9659258262890683122, 1.000000000000000000, 0.9659258262890683122, 1.000000000000000000, 0.9659258262890683122, 1.000000000000000000, 0.9659258262890683122, 1.000000000000000000, 0.9659258262890683122, 1.000000000000000000, 0.9659258262890683122, 1.000000000000000000, 0.9659258262890683122, 1.000000000000000000, 0.9659258262890683122, 1.000000000000000000, 0.9659258262890683122, 1.000000000000000000, 0.9659258262890683122, 1.000000000000000000, 0.9659258262890683122, 1.000000000000000000, 0.9659258262890683122, 1.000000000000000000, 0.9659258262890683122, 1.000000000000000000, 0.9659258262890683122, 1.000000000000000000, 0.9659258262890683122, 1.000000000000000000, 0.9659258262890683122, 1.000000000000000000, 0.9659258262890683122, 1.000000000000000000, 0.9659258262890683122, 1.000000000000000000, 0.9659258262890683122, 1.000000000000000000, 0.9659258262890683122, 1.000000000000000000, 0.9659258262890683122, 1.000000000000000000, 0.9659258262890683122, 1.000000000000000000, 0.9659258262890683122, 1.000000000000000000, 0.9659258262890683122, 1.000000000000000000, 0.9659258262890683122, 1.000000000000000000, 0.9659258262890683122, 1.000000000000000000, 0.9659258262890683122, 1.000000000000000000, 0.9659258262890683122, 1.000000000000000000, 0.9659258262890683122, 1.000000000000000000, 0.9659258262890683122, 1.000000000000000000, 0.9659258262890683122, 1.000000000000000000, 0.9659258262890683122, 1.000000000000000000, 0.9659258262890683122, 1.000000000000000000, 0.9659258262890683122, 1.000000000000000000, 0.9659258262890683122, 1.000000000000000000, 0.9659258262890683122, 1.000000000000000000, 0.9659258262890683122, 1.000000000000000000, 0.9659258262890683122, 1.000000000000000000, 0.9659258262890683122, 1.000000000000000000, 0.9659258262890683122, 1.000000000000000000, 0.9659258262890683122, 1.000000000000000000, 0.9659258262890683122, 1.000000000000000000, 0.9659258262890683122, 1.000000000000000000, 0.9659258262890683122, 1.000000000000000000, 0.9659258262890683122, 1.000000000000000000, 0.9659258262890683122, 1.000000000000000000, 0.9659258262890683122, 1.000000000000000000, 0.9659258262890683122, 1.000000000000000000, 0.9659258262890683122, 1.000000000000000000, 0.9659258262890683122, 1.000000000000000000) ) ) 
 REPRESENTATION_ITEM ( '' )  SURFACE ( )  );
#54799 = CARTESIAN_POINT ( 'NONE',  ( 17.20831665107776587, 44.13393115100078745, -7.208316651077762316 ) ) ;
#54800 = CARTESIAN_POINT ( 'NONE',  ( -46.59701958359876528, 103.7651961684614719, 6.068442458532165240 ) ) ;
#54801 = DIRECTION ( 'NONE',  ( -0.000000000000000000, -1.000000000000000000, -0.000000000000000000 ) ) ;
#54802 = AXIS2_PLACEMENT_3D ( 'NONE', #92942, #83980, #31452 ) ;
#54803 = CARTESIAN_POINT ( 'NONE',  ( 5.076628168052703671, 66.84226448433412315, 8.527530157486179263 ) ) ;
#54804 = CARTESIAN_POINT ( 'NONE',  ( 9.876730923139255935, 0.3639310091266618197, 11.28938378619071337 ) ) ;
#54805 = PRESENTATION_STYLE_ASSIGNMENT (( #31320 ) ) ;
#54806 = CARTESIAN_POINT ( 'NONE',  ( 2.917880565312950480, 20.97041550158063217, -12.26659068614894821 ) ) ;
#54807 = CIRCLE ( 'NONE', #67613, 3.750000000000001776 ) ;
#54808 = CARTESIAN_POINT ( 'NONE',  ( 18.52753015748618282, 38.92559781766745175, -4.923371831947291888 ) ) ;
#54809 = DIRECTION ( 'NONE',  ( 0.000000000000000000, 0.000000000000000000, 1.000000000000000000 ) ) ;
#54810 = B_SPLINE_CURVE_WITH_KNOTS ( 'NONE', 3,
 ( #19062, #11068, #49540, #64537, #35027, #48067 ),
 .UNSPECIFIED., .F., .F.,
 ( 4, 2, 4 ),
 ( 3.409110551496214716E-05, 0.0004400426677368003410, 0.0008459942299586385890 ),
 .UNSPECIFIED. ) ;
#54811 = CARTESIAN_POINT ( 'NONE',  ( -4.164238869374099039, 56.80374883491397497, 8.674139862899312516E-16 ) ) ;
#54812 = CARTESIAN_POINT ( 'NONE',  ( 12.63842701281683922, 19.55059781766745175, -9.846743663894590881 ) ) ;
#54814 = DIRECTION ( 'NONE',  ( 0.8433914458128921599, 0.000000000000000000, -0.5372996083468137840 ) ) ;
#54813 = CYLINDRICAL_SURFACE ( 'NONE', #17982, 1.500000000000001332 ) ;
#54815 = CARTESIAN_POINT ( 'NONE',  ( 2.035157376598822676, 52.43868534415483396, -7.964842623401177768 ) ) ;
#54816 = CARTESIAN_POINT ( 'NONE',  ( -2.816281873526473856, 49.33196800326374643, 3.434112377981055619 ) ) ;
#54817 = CARTESIAN_POINT ( 'NONE',  ( 12.91533473730992121, 14.52201867748817143, 10.88017736071110164 ) ) ;
#54818 = CARTESIAN_POINT ( 'NONE',  ( -2.816281873526473856, 54.12363466993041783, 9.499525473075851096E-16 ) ) ;
#54819 = CARTESIAN_POINT ( 'NONE',  ( 10.00000000000000000, 64.75893115100078035, -9.846743663894594434 ) ) ;
#54820 = CARTESIAN_POINT ( 'NONE',  ( 17.20831665107776587, 19.13393115100078035, -7.208316651077762316 ) ) ;
#54821 = ORIENTED_EDGE ( 'NONE', *, *, #45617, .F. ) ;
#54822 = FACE_OUTER_BOUND ( 'NONE', #81188, .T. ) ;
#54823 = CARTESIAN_POINT ( 'NONE',  ( 0.9408516040111585266, 17.46693863883975695, -6.499999999999988454 ) ) ;
#54824 = CARTESIAN_POINT ( 'NONE',  ( 13.79529636645030344, 48.26208216824728936, 14.16423886937410614 ) ) ;
#54825 = CARTESIAN_POINT ( 'NONE',  ( 17.08211943468705840, 15.13708216824730179, -12.26659068614894466 ) ) ;
#54826 = CARTESIAN_POINT ( 'NONE',  ( 10.00000000000000000, 16.81368534415483751, -10.88017736071110342 ) ) ;
#54827 = CARTESIAN_POINT ( 'NONE',  ( 19.42250999205614193, 35.14701867748816966, 5.440088680355555262 ) ) ;
#54828 = CARTESIAN_POINT ( 'NONE',  ( 14.29484424893241901, 0.2301500622783320127, 4.345072767107231115 ) ) ;
#54829 = CARTESIAN_POINT ( 'NONE',  ( 0.1532563361054082862, 1.217264484334117824, 2.638427012816831674 ) ) ;
#54830 = DIRECTION ( 'NONE',  ( -6.938893903907222067E-15, 0.000000000000000000, 1.000000000000000000 ) ) ;
#54831 = CARTESIAN_POINT ( 'NONE',  ( 2.791683348922237240, 20.38393115100078745, -7.208316651077763204 ) ) ;
#54832 = CARTESIAN_POINT ( 'NONE',  ( 5.147851794460816421, 14.99999999999795364, -13.68970903997665545 ) ) ;
#54833 = CARTESIAN_POINT ( 'NONE',  ( 5.500000000000000000, 11.50000000000000000, 6.000000000000000000 ) ) ;
#54834 = CARTESIAN_POINT ( 'NONE',  ( 5.076628168052704559, 15.17559781766745175, -8.527530157486179263 ) ) ;
#54835 = CARTESIAN_POINT ( 'NONE',  ( 19.84674366389459266, 33.71726448433410894, -2.638427012816827677 ) ) ;
#54836 = EDGE_CURVE ( 'NONE', #6306, #11368, #47301, .T. ) ;
#54837 = CARTESIAN_POINT ( 'NONE',  ( 7.084665262690076126, 14.10535201082150358, 10.88017736071109987 ) ) ;
#54838 = CARTESIAN_POINT ( 'NONE',  ( 22.81628187352648496, 31.83196800326375353, -3.434112377981050290 ) ) ;
#54839 = VECTOR ( 'NONE', #7875, 1000.000000000000000 ) ;
#54841 = CARTESIAN_POINT ( 'NONE',  ( 19.84674366389459266, 13.30059781766745353, 2.638427012816836559 ) ) ;
#54840 = CARTESIAN_POINT ( 'NONE',  ( 20.36894250292379738, 39.92874883491396787, -10.36894250292379027 ) ) ;
#54842 = CARTESIAN_POINT ( 'NONE',  ( -4.250000000000000000, 78.07179676972445748, -6.250000000000000000 ) ) ;
#54843 = CARTESIAN_POINT ( 'NONE',  ( 14.92337183194729633, 47.67559781766745175, 8.527530157486181039 ) ) ;
#54844 = AXIS2_PLACEMENT_3D ( 'NONE', #89590, #27104, #27602 ) ;
#54846 = CARTESIAN_POINT ( 'NONE',  ( 6.204703633549690345, 0.7620821682473009062, -14.16423886937410259 ) ) ;
#54845 = CARTESIAN_POINT ( 'NONE',  ( 2.791683348922240793, 36.63393115100078035, 7.208316651077764092 ) ) ;
#54847 = CARTESIAN_POINT ( 'NONE',  ( 10.00000000000000000, 15.55374883491396787, -14.16423886937410082 ) ) ;
#54848 = CARTESIAN_POINT ( 'NONE',  ( -0.8801773607111009756, 53.06368534415484106, 1.068504757029289695E-15 ) ) ;
#54849 = CARTESIAN_POINT ( 'NONE',  ( 2.035157376598824452, 13.68868534415483751, 7.964842623401179544 ) ) ;
#54850 = AXIS2_PLACEMENT_3D ( 'NONE', #92968, #40484, #2004 ) ;
#54851 = CARTESIAN_POINT ( 'NONE',  ( 15.44008868035555260, 44.73035201082151247, 9.422509992056143702 ) ) ;
#54852 = CARTESIAN_POINT ( 'NONE',  ( 20.88017736071110164, 25.35535201082150891, 2.915334737309930979 ) ) ;
#54853 = VERTEX_POINT ( 'NONE', #88529 ) ;
#54854 = CARTESIAN_POINT ( 'NONE',  ( -2.816281873526473856, 34.33196800326376064, 3.434112377981055619 ) ) ;
#54855 = EDGE_CURVE ( 'NONE', #44141, #10785, #5792, .T. ) ;
#54856 = CARTESIAN_POINT ( 'NONE',  ( 2.035157376598824452, 43.68868534415484106, 7.964842623401179544 ) ) ;
#54857 = ORIENTED_EDGE ( 'NONE', *, *, #41541, .T. ) ;
#54858 = CARTESIAN_POINT ( 'NONE',  ( -1.099225684535947600, 58.70696800326375353, -6.408140936763238038 ) ) ;
#54859 = ADVANCED_FACE ( 'NONE', ( #49059 ), #1119, .T. ) ;
#54860 = CARTESIAN_POINT ( 'NONE',  ( 12.91533473730993009, 56.60535201082151247, -10.88017736071109987 ) ) ;
#54861 = VERTEX_POINT ( 'NONE', #96545 ) ;
#54863 = EDGE_CURVE ( 'NONE', #67942, #33221, #80042, .T. ) ;
#54862 = CARTESIAN_POINT ( 'NONE',  ( 12.91533473730993009, 51.60535201082149825, -10.88017736071109987 ) ) ;
#54864 = CARTESIAN_POINT ( 'NONE',  ( 4.559911319644449179, 7.230352010821504471, -9.422509992056141925 ) ) ;
#54865 = CARTESIAN_POINT ( 'NONE',  ( 5.419894505350487002, 15.00000000000000000, 13.98659156302462314 ) ) ;
#54866 = SURFACE_STYLE_FILL_AREA ( #30891 ) ;
#54867 = CARTESIAN_POINT ( 'NONE',  ( 13.79529636645030344, 58.26208216824728936, 14.16423886937410614 ) ) ;
#54868 = CARTESIAN_POINT ( 'NONE',  ( 4.559911319644449179, 68.89701867748817676, 9.422509992056141925 ) ) ;
#54869 = CARTESIAN_POINT ( 'NONE',  ( -4.164238869374099039, 11.80374883491396965, 8.674139862899312516E-16 ) ) ;
#54870 = ADVANCED_FACE ( 'NONE', ( #79563 ), #60078, .T. ) ;
#54871 = CARTESIAN_POINT ( 'NONE',  ( -7.330068351210572430, -69.53589943318687006, -4.000000000000000888 ) ) ;
#54872 = CARTESIAN_POINT ( 'NONE',  ( 20.88017736071110164, 15.35535201082150358, 2.915334737309930979 ) ) ;
#54873 = CARTESIAN_POINT ( 'NONE',  ( 14.92337183194729633, 52.67559781766745175, 8.527530157486181039 ) ) ;
#54874 = ORIENTED_EDGE ( 'NONE', *, *, #46641, .F. ) ;
#54875 = CARTESIAN_POINT ( 'NONE',  ( 10.00000000000000178, 42.25893115100078745, 9.846743663894594434 ) ) ;
#54876 = CARTESIAN_POINT ( 'NONE',  ( -0.8801773607111009756, 63.06368534415484106, 1.068504757029289695E-15 ) ) ;
#54877 = CARTESIAN_POINT ( 'NONE',  ( 15.44008868035555260, 44.73035201082151247, 9.422509992056143702 ) ) ;
#54878 = CARTESIAN_POINT ( 'NONE',  ( 5.076628168052704559, 40.17559781766745175, -8.527530157486179263 ) ) ;
#54880 = DIRECTION ( 'NONE',  ( 0.000000000000000000, 0.000000000000000000, 1.000000000000000000 ) ) ;
#54879 = FILL_AREA_STYLE_COLOUR ( '', #22826 ) ;
#54881 = CARTESIAN_POINT ( 'NONE',  ( 15.44008868035555260, 44.73035201082151247, 9.422509992056143702 ) ) ;
#54882 = CARTESIAN_POINT ( 'NONE',  ( 13.79529636645030344, 53.26208216824730357, 14.16423886937410614 ) ) ;
#54883 = CARTESIAN_POINT ( 'NONE',  ( 22.81628187352647785, 21.41530133659708923, 3.434112377981063169 ) ) ;
#54884 = VERTEX_POINT ( 'NONE', #18567 ) ;
#54885 = CARTESIAN_POINT ( 'NONE',  ( 3.591859063236761518, 24.95696800326375353, 11.09922568453594849 ) ) ;
#54886 = CARTESIAN_POINT ( 'NONE',  ( 0.5774900079438607392, 18.48035201082150536, 5.440088680355550821 ) ) ;
#54888 = ORIENTED_EDGE ( 'NONE', *, *, #81084, .T. ) ;
#54887 = EDGE_CURVE ( 'NONE', #52573, #86532, #94869, .T. ) ;
#54889 = CARTESIAN_POINT ( 'NONE',  ( 0.5774900079438590739, 67.64701867748817676, -5.440088680355550821 ) ) ;
#54890 = ADVANCED_BREP_SHAPE_REPRESENTATION ( '', ( #74133, #27931 ), #40723 ) ;
#54891 = CARTESIAN_POINT ( 'NONE',  ( 12.63842701281683922, 49.55059781766744464, -9.846743663894590881 ) ) ;
#54893 = CARTESIAN_POINT ( 'NONE',  ( 17.20831665107776587, 39.13393115100079456, -7.208316651077762316 ) ) ;
#54892 = CARTESIAN_POINT ( 'NONE',  ( 7.361572987183169658, 14.96726448433411960, -9.846743663894592657 ) ) ;
#54894 = CARTESIAN_POINT ( 'NONE',  ( -8.160053284515589311, -4.177241847651679052, 3.750000000000001332 ) ) ;
#54895 = DIRECTION ( 'NONE',  ( -0.8141155183563226760, 0.000000000000000000, 0.5807029557109348872 ) ) ;
#54896 = CARTESIAN_POINT ( 'NONE',  ( 17.20831665107776587, 24.13393115100078035, -7.208316651077762316 ) ) ;
#54897 = CARTESIAN_POINT ( 'NONE',  ( 20.24186590665277308, 56.76028685723173339, 6.114288769123047196 ) ) ;
#54898 = DIRECTION ( 'NONE',  ( -0.000000000000000000, 1.000000000000000000, -0.000000000000000000 ) ) ;
#54900 = CARTESIAN_POINT ( 'NONE',  ( 17.20831665107776587, 2.883931151000785231, 7.208316651077764980 ) ) ;
#54899 = CARTESIAN_POINT ( 'NONE',  ( 17.20831665107776587, 29.13393115100078390, -7.208316651077762316 ) ) ;
#54901 = PLANE ( 'NONE',  #82486 ) ;
#54903 = VERTEX_POINT ( 'NONE', #10397 ) ;
#54902 = CARTESIAN_POINT ( 'NONE',  ( 2.791683348922240793, 46.63393115100077324, 7.208316651077764092 ) ) ;
#54904 = DIRECTION ( 'NONE',  ( 0.8141155183563185682, 0.000000000000000000, -0.5807029557109406603 ) ) ;
#54905 = CARTESIAN_POINT ( 'NONE',  ( 21.09922568453595559, 27.04030133659708568, -6.408140936763230044 ) ) ;
#54906 = CIRCLE ( 'NONE', #82041, 0.2500000000000002220 ) ;
#54907 = EDGE_CURVE ( 'NONE', #57773, #98073, #70319, .T. ) ;
#54908 = CARTESIAN_POINT ( 'NONE',  ( 4.380000000000002558, 1.019547802438462547, -2.750000000000000000 ) ) ;
#54909 = CARTESIAN_POINT ( 'NONE',  ( 20.36894250292379738, 49.92874883491396787, -10.36894250292379027 ) ) ;
#54910 = CARTESIAN_POINT ( 'NONE',  ( 18.52753015748617571, 3.092264484334118269, 4.923371831947298993 ) ) ;
#54911 = CARTESIAN_POINT ( 'NONE',  ( -46.93999999999902428, 100.4992020706143023, 9.114648421618825935 ) ) ;
#54912 =( GEOMETRIC_REPRESENTATION_CONTEXT ( 3 ) GLOBAL_UNCERTAINTY_ASSIGNED_CONTEXT ( ( #26506 ) ) GLOBAL_UNIT_ASSIGNED_CONTEXT ( ( #91207, #23233, #14243 ) ) REPRESENTATION_CONTEXT ( 'NONE', 'WORKASPACE' ) );
#54913 = CARTESIAN_POINT ( 'NONE',  ( 24.16423886937410614, 49.30374883491396787, 8.672049930838204340E-16 ) ) ;
#54914 = CARTESIAN_POINT ( 'NONE',  ( 22.26659068614894466, 63.88708216824730357, 7.082119434687054849 ) ) ;
#54915 = CARTESIAN_POINT ( 'NONE',  ( -4.164238869374099039, 16.80374883491396787, 8.674139862899312516E-16 ) ) ;
#54916 = CARTESIAN_POINT ( 'NONE',  ( 2.917880565312948704, 32.63708216824730357, 12.26659068614894643 ) ) ;
#54917 = CARTESIAN_POINT ( 'NONE',  ( -5.999999999999994671, 79.82179676972448590, -6.500000000000000888 ) ) ;
#54919 = CARTESIAN_POINT ( 'NONE',  ( 19.84674366389459266, 38.30059781766745175, 2.638427012816836559 ) ) ;
#54918 = CARTESIAN_POINT ( 'NONE',  ( 4.572805491842157011, -6.390838093384605401, 2.500000000000000000 ) ) ;
#54920 = VERTEX_POINT ( 'NONE', #70909 ) ;
#54921 = CARTESIAN_POINT ( 'NONE',  ( 19.42250999205614193, 35.14701867748816966, 5.440088680355555262 ) ) ;
#54922 = DIRECTION ( 'NONE',  ( 0.000000000000000000, 1.000000000000000000, 0.000000000000000000 ) ) ;
#54923 = CARTESIAN_POINT ( 'NONE',  ( 11.75249112337023760, 14.95037104118845583, -8.918310463591724968 ) ) ;
#54924 = CARTESIAN_POINT ( 'NONE',  ( 0.1532563361054083140, 41.00893115100078745, 1.131784320476157264E-15 ) ) ;
#54925 = CARTESIAN_POINT ( 'NONE',  ( 3.591859063236761518, 59.95696800326375353, 11.09922568453594849 ) ) ;
#54926 = CARTESIAN_POINT ( 'NONE',  ( -10.36894250292378317, -2.571251165086037460, 10.36894250292379560 ) ) ;
#54927 = CARTESIAN_POINT ( 'NONE',  ( 19.84674366389459621, 38.50893115100078745, 7.409399052514197653E-17 ) ) ;
#54928 = CARTESIAN_POINT ( 'NONE',  ( 7.361572987183170547, 62.05059781766745886, 9.846743663894590881 ) ) ;
#54929 = ORIENTED_EDGE ( 'NONE', *, *, #31726, .T. ) ;
#54930 = CARTESIAN_POINT ( 'NONE',  ( 13.79529636645030344, 8.262082168247300018, 14.16423886937410614 ) ) ;
#54931 = CARTESIAN_POINT ( 'NONE',  ( -14.43100913236851568, 15.00000000000000000, 1.412789942453067216 ) ) ;
#54933 = PLANE ( 'NONE',  #28090 ) ;
#54932 = CARTESIAN_POINT ( 'NONE',  ( 1.847237859018745487, 0.04962896072147187504, -14.63711110085117717 ) ) ;
#54934 = CARTESIAN_POINT ( 'NONE',  ( 19.42250999205614548, 5.980352010821504471, -5.440088680355545492 ) ) ;
#54935 = CARTESIAN_POINT ( 'NONE',  ( 0.6178305044545818747, 8.498634669930421381, -9.382169495545419124 ) ) ;
#54936 = FILL_AREA_STYLE_COLOUR ( '', #16158 ) ;
#54937 = CARTESIAN_POINT ( 'NONE',  ( 2.035157376598822676, 62.43868534415483396, -7.964842623401177768 ) ) ;
#54938 = CARTESIAN_POINT ( 'NONE',  ( 20.32896413005680003, 41.77164270246083788, 5.963430220938287007 ) ) ;
#54939 = CARTESIAN_POINT ( 'NONE',  ( 2.603489959281581889, 30.43575266056827999, -6.499999999999995559 ) ) ;
#54940 = EDGE_CURVE ( 'NONE', #1302, #42327, #55304, .T. ) ;
#54941 = LINE ( 'NONE', #85456, #27920 ) ;
#54942 = CARTESIAN_POINT ( 'NONE',  ( 13.79529636645030344, 63.26208216824730357, 14.16423886937410614 ) ) ;
#54943 = DIRECTION ( 'NONE',  ( 0.000000000000000000, 1.000000000000000000, 0.000000000000000000 ) ) ;
#54944 = CARTESIAN_POINT ( 'NONE',  ( 19.42250999205614193, 25.14701867748817321, 5.440088680355555262 ) ) ;
#54945 = CARTESIAN_POINT ( 'NONE',  ( 0.5774900079438607392, 43.48035201082151247, 5.440088680355550821 ) ) ;
#54946 = CARTESIAN_POINT ( 'NONE',  ( 13.43411237798105340, 0.5819680032637533085, 12.81628187352647963 ) ) ;
#54947 = CARTESIAN_POINT ( 'NONE',  ( 7.361572987183170547, 57.05059781766744464, 9.846743663894590881 ) ) ;
#54948 = CARTESIAN_POINT ( 'NONE',  ( 6.565887622018943937, 63.08196800326376064, -12.81628187352647608 ) ) ;
#54949 = CARTESIAN_POINT ( 'NONE',  ( 14.92337183194729633, 2.675597817667451750, 8.527530157486181039 ) ) ;
#54950 = ORIENTED_EDGE ( 'NONE', *, *, #69949, .T. ) ;
#54951 = EDGE_CURVE ( 'NONE', #81651, #38851, #82435, .T. ) ;
#54952 = CARTESIAN_POINT ( 'NONE',  ( 17.96484262340118221, 34.93868534415482685, 7.964842623401181321 ) ) ;
#54953 = CARTESIAN_POINT ( 'NONE',  ( 6.565887622018943937, 35.16530133659708923, 12.81628187352647430 ) ) ;
#54954 = DIRECTION ( 'NONE',  ( 0.02617694830788287394, 0.000000000000000000, -0.9996573249755570378 ) ) ;
#54955 = CARTESIAN_POINT ( 'NONE',  ( 0.1532563361054082862, 56.21726448433411605, 2.638427012816831674 ) ) ;
#54956 = CARTESIAN_POINT ( 'NONE',  ( 0.5774900079438607392, 53.48035201082151247, 5.440088680355550821 ) ) ;
#54957 = CARTESIAN_POINT ( 'NONE',  ( 19.38216949554541557, 32.24863466993041783, -9.382169495545420901 ) ) ;
#54959 = CARTESIAN_POINT ( 'NONE',  ( 20.88017736071110164, 15.35535201082150181, 2.915334737309930979 ) ) ;
#54958 = CARTESIAN_POINT ( 'NONE',  ( 17.96484262340118221, 56.18868534415484817, -7.964842623401177768 ) ) ;
#54960 = CARTESIAN_POINT ( 'NONE',  ( 16.40814093676324603, 62.45696800326376064, -11.09922568453594671 ) ) ;
#54961 = EDGE_LOOP ( 'NONE', ( #21622, #5328, #5585, #60665 ) ) ;
#54962 = CARTESIAN_POINT ( 'NONE',  ( 9.879999999999990123, 20.99999999999999645, -3.000000000000000000 ) ) ;
#54963 = CARTESIAN_POINT ( 'NONE',  ( -3.499999999999998668, 1.019547802438465434, 2.750000000000000444 ) ) ;
#54964 = CARTESIAN_POINT ( 'NONE',  ( 7.084665262690076126, 2.022018677488170990, -10.88017736071110164 ) ) ;
#54966 = CARTESIAN_POINT ( 'NONE',  ( -0.3689425029237881626, 12.42874883491396609, 10.36894250292379027 ) ) ;
#54965 = CARTESIAN_POINT ( 'NONE',  ( 21.09922568453594849, 51.20696800326375353, 6.408140936763242479 ) ) ;
#54967 = CARTESIAN_POINT ( 'NONE',  ( 10.00000000000000178, 12.25893115100078568, 9.846743663894594434 ) ) ;
#54968 = CARTESIAN_POINT ( 'NONE',  ( 7.084665262690076126, 12.02201867748817143, -10.88017736071110164 ) ) ;
#54969 = CARTESIAN_POINT ( 'NONE',  ( 18.52753015748618282, 23.92559781766745530, -4.923371831947291888 ) ) ;
#54970 = CYLINDRICAL_SURFACE ( 'NONE', #71436, 4.000000000000001776 ) ;
#54971 = CARTESIAN_POINT ( 'NONE',  ( 6.204703633549690345, 52.84541550158062506, 14.16423886937410082 ) ) ;
#54972 = ORIENTED_EDGE ( 'NONE', *, *, #61523, .T. ) ;
#54973 = SURFACE_STYLE_USAGE ( .BOTH. , #62974 ) ;
#54974 = CARTESIAN_POINT ( 'NONE',  ( 10.00000000000000178, 4.313685344154837509, 10.88017736071110342 ) ) ;
#54975 = DIRECTION ( 'NONE',  ( -0.000000000000000000, -0.000000000000000000, 1.000000000000000000 ) ) ;
#54976 = EDGE_LOOP ( 'NONE', ( #528, #10690, #73050, #64619 ) ) ;
#54977 = ORIENTED_EDGE ( 'NONE', *, *, #29682, .F. ) ;
#54978 = CARTESIAN_POINT ( 'NONE',  ( 4.559911319644449179, 12.23035201082150714, -9.422509992056141925 ) ) ;
#54980 = EDGE_CURVE ( 'NONE', #96981, #76186, #5845, .T. ) ;
#54979 = CARTESIAN_POINT ( 'NONE',  ( 4.559911319644449179, 8.897018677488173211, 9.422509992056141925 ) ) ;
#54981 = CARTESIAN_POINT ( 'NONE',  ( 14.92337183194729988, 39.34226448433412315, -8.527530157486177487 ) ) ;
#54982 = CARTESIAN_POINT ( 'NONE',  ( 13.43411237798106583, 47.66530133659709634, -12.81628187352647252 ) ) ;
#54983 = FILL_AREA_STYLE ('',( #62486 ) ) ;
#54985 = CARTESIAN_POINT ( 'NONE',  ( 2.917880565312950480, 20.97041550158063217, -12.26659068614894821 ) ) ;
#54984 = DIRECTION ( 'NONE',  ( -1.000000000000000000, 0.000000000000000000, -0.000000000000000000 ) ) ;
#54986 = CARTESIAN_POINT ( 'NONE',  ( 15.44008868035555793, 21.39701867748817321, -9.422509992056140149 ) ) ;
#54987 = CARTESIAN_POINT ( 'NONE',  ( 13.79529636645031943, 65.34541550158063217, -14.16423886937409904 ) ) ;
#54988 = CARTESIAN_POINT ( 'NONE',  ( 1.472469842513823179, 61.42559781766745175, 4.923371831947296329 ) ) ;
#54989 = EDGE_CURVE ( 'NONE', #61653, #11334, #85906, .T. ) ;
#54990 = CARTESIAN_POINT ( 'NONE',  ( 0.000000000000000000, 0.000000000000000000, 0.000000000000000000 ) ) ;
#54991 = CARTESIAN_POINT ( 'NONE',  ( 5.076628168052704559, 40.17559781766745175, -8.527530157486179263 ) ) ;
#54992 = VECTOR ( 'NONE', #85576, 1000.000000000000000 ) ;
#54993 = CARTESIAN_POINT ( 'NONE',  ( -0.8801773607111009756, 33.06368534415484106, 1.068504757029289695E-15 ) ) ;
#54994 = CARTESIAN_POINT ( 'NONE',  ( 7.208316651077764980, 22.88393115100078745, 7.208316651077762316 ) ) ;
#54995 = ORIENTED_EDGE ( 'NONE', *, *, #88394, .T. ) ;
#54996 = SURFACE_STYLE_FILL_AREA ( #69529 ) ;
#54997 = CARTESIAN_POINT ( 'NONE',  ( 7.084665262690076126, 64.10535201082150536, 10.88017736071109987 ) ) ;
#54998 = CARTESIAN_POINT ( 'NONE',  ( 0.1532563361054100626, 60.80059781766744464, -2.638427012816831230 ) ) ;
#55000 = CARTESIAN_POINT ( 'NONE',  ( 19.42250999205614193, 45.14701867748817676, 5.440088680355555262 ) ) ;
#54999 = CARTESIAN_POINT ( 'NONE',  ( 2.035157376598822676, 52.43868534415483396, -7.964842623401177768 ) ) ;
#55002 = CARTESIAN_POINT ( 'NONE',  ( 22.81628187352648496, 46.83196800326376064, -3.434112377981050290 ) ) ;
#55001 = CARTESIAN_POINT ( 'NONE',  ( 10.00000000000000000, 11.81368534415483751, -10.88017736071110342 ) ) ;
#55003 = CARTESIAN_POINT ( 'NONE',  ( 17.08211943468705840, 20.13708216824730357, -12.26659068614894466 ) ) ;
#55004 = EDGE_CURVE ( 'NONE', #74689, #35385, #91741, .T. ) ;
#55005 = EDGE_CURVE ( 'NONE', #16073, #40514, #32391, .T. ) ;
#55006 = CARTESIAN_POINT ( 'NONE',  ( 22.81628187352647785, 51.62363466993042493, 6.195893100308588602E-16 ) ) ;
#55007 = ORIENTED_EDGE ( 'NONE', *, *, #56544, .F. ) ;
#55008 = CARTESIAN_POINT ( 'NONE',  ( 5.076628168052703671, 61.84226448433412315, 8.527530157486179263 ) ) ;
#55009 = CARTESIAN_POINT ( 'NONE',  ( 12.91533473730992121, 19.52201867748816611, 10.88017736071110164 ) ) ;
#55010 = CARTESIAN_POINT ( 'NONE',  ( -0.8801773607111008646, 33.27201867748817676, 2.915334737309923430 ) ) ;
#55012 = VERTEX_POINT ( 'NONE', #83238 ) ;
#55011 = EDGE_CURVE ( 'NONE', #89108, #36460, #11861, .T. ) ;
#55013 = CARTESIAN_POINT ( 'NONE',  ( 10.00000000000000000, 9.758931151000785675, -9.846743663894594434 ) ) ;
#55014 = CARTESIAN_POINT ( 'NONE',  ( 2.035157376598822676, 2.438685344154837953, -7.964842623401177768 ) ) ;
#55015 = CARTESIAN_POINT ( 'NONE',  ( -14.04391541078767958, 4.832815575535569023E-16, 3.608107528142744602 ) ) ;
#55016 = CARTESIAN_POINT ( 'NONE',  ( 17.20831665107776587, 12.88393115100078390, 7.208316651077764980 ) ) ;
#55017 = CARTESIAN_POINT ( 'NONE',  ( 10.00000000000000178, 64.31368534415483396, 10.88017736071110342 ) ) ;
#55018 = FACE_OUTER_BOUND ( 'NONE', #15857, .T. ) ;
#55019 = AXIS2_PLACEMENT_3D ( 'NONE', #76647, #40137, #24155 ) ;
#55020 =( NAMED_UNIT ( * ) SI_UNIT ( $, .STERADIAN. ) SOLID_ANGLE_UNIT ( ) );
#55021 = CARTESIAN_POINT ( 'NONE',  ( 7.084665262690076126, 62.02201867748816966, -10.88017736071110164 ) ) ;
#55023 = ORIENTED_EDGE ( 'NONE', *, *, #34646, .F. ) ;
#55022 = CARTESIAN_POINT ( 'NONE',  ( 0.1532563361054100626, 5.800597817667452638, -2.638427012816831230 ) ) ;
#55024 = CARTESIAN_POINT ( 'NONE',  ( 7.361572987183169658, 39.96726448433411605, -9.846743663894592657 ) ) ;
#55025 = ORIENTED_EDGE ( 'NONE', *, *, #389, .T. ) ;
#55026 = ORIENTED_EDGE ( 'NONE', *, *, #80701, .T. ) ;
#55027 = CARTESIAN_POINT ( 'NONE',  ( -12.25993886608612371, 14.63595249122789177, 8.642563219313544209 ) ) ;
#55028 = CARTESIAN_POINT ( 'NONE',  ( -4.164238869374098151, 1.595415501580634388, -3.795296366450310543 ) ) ;
#55029 = CARTESIAN_POINT ( 'NONE',  ( -1.099225684535947600, 63.70696800326376774, -6.408140936763238038 ) ) ;
#55030 = CARTESIAN_POINT ( 'NONE',  ( 13.79529636645031943, 10.34541550158063394, -14.16423886937409904 ) ) ;
#55031 = CARTESIAN_POINT ( 'NONE',  ( -4.164238869374098151, 21.59541550158063217, -3.795296366450310543 ) ) ;
#55032 = CYLINDRICAL_SURFACE ( 'NONE', #31070, 0.2500000000000002220 ) ;
#55034 = CARTESIAN_POINT ( 'NONE',  ( 0.5774900079438590739, 57.64701867748817676, -5.440088680355550821 ) ) ;
#55033 = DIRECTION ( 'NONE',  ( 0.000000000000000000, 0.000000000000000000, -1.000000000000000000 ) ) ;
#55035 = CARTESIAN_POINT ( 'NONE',  ( 4.559911319644449179, 18.89701867748817321, 9.422509992056141925 ) ) ;
#55036 = CARTESIAN_POINT ( 'NONE',  ( -8.900000000000002132, 80.99999999999994316, 0.000000000000000000 ) ) ;
#55037 = ORIENTED_EDGE ( 'NONE', *, *, #78683, .F. ) ;
#55038 = AXIS2_PLACEMENT_3D ( 'NONE', #19804, #26814, #58788 ) ;
#55039 = CARTESIAN_POINT ( 'NONE',  ( 17.20831665107776587, 7.883931151000784787, 7.208316651077764980 ) ) ;
#55040 = CARTESIAN_POINT ( 'NONE',  ( 6.565887622018943937, 28.08196800326375353, -12.81628187352647608 ) ) ;
#55041 = CARTESIAN_POINT ( 'NONE',  ( 12.63842701281683034, 42.46726448433412315, 9.846743663894596210 ) ) ;
#55042 = LINE ( 'NONE', #77547, #68157 ) ;
#55043 = CARTESIAN_POINT ( 'NONE',  ( 19.38216949554541557, 22.24863466993041428, -9.382169495545420901 ) ) ;
#55044 = CARTESIAN_POINT ( 'NONE',  ( -5.991992585808714189, 4.061121054423934144E-16, 13.20401548210291054 ) ) ;
#55045 = CARTESIAN_POINT ( 'NONE',  ( 14.92337183194729633, 27.67559781766745530, 8.527530157486181039 ) ) ;
#55046 = CARTESIAN_POINT ( 'NONE',  ( 1.472469842513823179, 0.5922644843341181575, -4.923371831947296329 ) ) ;
#55047 = ORIENTED_EDGE ( 'NONE', *, *, #24417, .F. ) ;
#55048 = ORIENTED_EDGE ( 'NONE', *, *, #83069, .T. ) ;
#55049 = ORIENTED_EDGE ( 'NONE', *, *, #42814, .T. ) ;
#55050 = CARTESIAN_POINT ( 'NONE',  ( 19.42250999205614193, 40.14701867748817676, 5.440088680355555262 ) ) ;
#55051 = CARTESIAN_POINT ( 'NONE',  ( -2.266590686148945544, 32.22041550158063927, 7.082119434687048631 ) ) ;
#55052 = CARTESIAN_POINT ( 'NONE',  ( 19.84674366389459266, 38.71726448433412315, -2.638427012816827677 ) ) ;
#55053 = CARTESIAN_POINT ( 'NONE',  ( -0.8801773607110991993, 67.85535201082151957, -2.915334737309923874 ) ) ;
#55055 = DIRECTION ( 'NONE',  ( -0.000000000000000000, -0.000000000000000000, -1.000000000000000000 ) ) ;
#55054 = CARTESIAN_POINT ( 'NONE',  ( 0.6178305044545818747, 48.49863466993042493, -9.382169495545419124 ) ) ;
#55056 = CARTESIAN_POINT ( 'NONE',  ( 0.5774900079438607392, 33.48035201082150536, 5.440088680355550821 ) ) ;
#55057 =( NAMED_UNIT ( * ) PLANE_ANGLE_UNIT ( ) SI_UNIT ( $, .RADIAN. ) );
#55058 = CARTESIAN_POINT ( 'NONE',  ( -2.816281873526471635, 18.91530133659708213, -3.434112377981056508 ) ) ;
#55059 = CARTESIAN_POINT ( 'NONE',  ( 22.81628187352648496, 16.83196800326374998, -3.434112377981050290 ) ) ;
#55060 = CARTESIAN_POINT ( 'NONE',  ( 7.361572987183169658, 34.96726448433411605, -9.846743663894592657 ) ) ;
#55061 = CARTESIAN_POINT ( 'NONE',  ( -10.88017736071110164, 2.855352010821508024, -2.915334737309917212 ) ) ;
#55062 = CARTESIAN_POINT ( 'NONE',  ( -2.816281873526473856, 44.33196800326375353, 3.434112377981055619 ) ) ;
#55063 = DIRECTION ( 'NONE',  ( 1.000000000000000000, 0.000000000000000000, 0.000000000000000000 ) ) ;
#55065 = CARTESIAN_POINT ( 'NONE',  ( -10.20000000000000107, 43.92361346574197256, 3.000000000000000000 ) ) ;
#55064 = CARTESIAN_POINT ( 'NONE',  ( 17.96484262340118221, 51.18868534415483396, -7.964842623401177768 ) ) ;
#55066 = ADVANCED_FACE ( 'NONE', ( #84721 ), #64848, .F. ) ;
#55067 = CARTESIAN_POINT ( 'NONE',  ( -13.61464873478161941, 0.3639308181217350557, -6.296136897218030271 ) ) ;
#55068 = FACE_OUTER_BOUND ( 'NONE', #79359, .T. ) ;
#55069 = CARTESIAN_POINT ( 'NONE',  ( 19.42250999205614548, 50.98035201082151247, -5.440088680355545492 ) ) ;
#55070 = CARTESIAN_POINT ( 'NONE',  ( 12.91533473730993009, 61.60535201082150536, -10.88017736071109987 ) ) ;
#55071 = LINE ( 'NONE', #71578, #15367 ) ;
#55072 = CIRCLE ( 'NONE', #47081, 0.2500000000000002220 ) ;
#55073 =( NAMED_UNIT ( * ) PLANE_ANGLE_UNIT ( ) SI_UNIT ( $, .RADIAN. ) );
#55074 = CARTESIAN_POINT ( 'NONE',  ( 0.5774900079438590739, 12.64701867748817321, -5.440088680355550821 ) ) ;
#55075 = CARTESIAN_POINT ( 'NONE',  ( 19.84674366389459621, 53.50893115100078745, 7.409399052514197653E-17 ) ) ;
#55077 = DIRECTION ( 'NONE',  ( 1.000000000000000000, 0.000000000000000000, -0.000000000000000000 ) ) ;
#55076 = CARTESIAN_POINT ( 'NONE',  ( 10.00000000000000178, 24.31368534415484106, 10.88017736071110342 ) ) ;
#55078 = CARTESIAN_POINT ( 'NONE',  ( 21.09922568453594849, 21.20696800326375353, 6.408140936763242479 ) ) ;
#55079 = VERTEX_POINT ( 'NONE', #61702 ) ;
#55080 = CARTESIAN_POINT ( 'NONE',  ( 10.00000000000000000, 31.81368534415483751, -10.88017736071110342 ) ) ;
#55082 = DIRECTION ( 'NONE',  ( 0.000000000000000000, 0.000000000000000000, 1.000000000000000000 ) ) ;
#55081 = CARTESIAN_POINT ( 'NONE',  ( 3.591859063236763294, 8.290301336597087456, -11.09922568453595026 ) ) ;
#55083 = CARTESIAN_POINT ( 'NONE',  ( 0.5774900079438607392, 18.48035201082150536, 5.440088680355550821 ) ) ;
#55084 = CARTESIAN_POINT ( 'NONE',  ( 12.91533473730993009, 41.60535201082149825, -10.88017736071109987 ) ) ;
#55085 = CARTESIAN_POINT ( 'NONE',  ( 13.79529636645031943, 45.34541550158062506, -14.16423886937409904 ) ) ;
#55086 = CARTESIAN_POINT ( 'NONE',  ( 10.00000000000000178, 42.25893115100078745, 9.846743663894594434 ) ) ;
#55087 = CARTESIAN_POINT ( 'NONE',  ( 12.91533473730992121, 59.52201867748816966, 10.88017736071110164 ) ) ;
#55088 = CARTESIAN_POINT ( 'NONE',  ( 0.8653096853333108740, 15.00000000000000533, 14.59999144042652475 ) ) ;
#55089 = CARTESIAN_POINT ( 'NONE',  ( -0.3689425029237881626, 22.42874883491397142, 10.36894250292379027 ) ) ;
#55090 = UNCERTAINTY_MEASURE_WITH_UNIT (LENGTH_MEASURE( 1.000000000000000082E-05 ), #4591, 'distance_accuracy_value', 'NONE');
#55091 =( NAMED_UNIT ( * ) PLANE_ANGLE_UNIT ( ) SI_UNIT ( $, .RADIAN. ) );
#55092 = CARTESIAN_POINT ( 'NONE',  ( 4.469999999999999751, 10.25000000000000000, 4.000000000000000000 ) ) ;
#55093 = ORIENTED_EDGE ( 'NONE', *, *, #11560, .T. ) ;
#55094 = CARTESIAN_POINT ( 'NONE',  ( 24.16423886937410614, 39.51208216824731068, -3.795296366450302550 ) ) ;
#55096 = ADVANCED_FACE ( 'NONE', ( #30219 ), #52731, .F. ) ;
#55095 = CARTESIAN_POINT ( 'NONE',  ( -0.3689425029237898834, 41.17874883491397497, -10.36894250292378850 ) ) ;
#55097 = CARTESIAN_POINT ( 'NONE',  ( 7.361572987183170547, 2.050597817667451750, 9.846743663894590881 ) ) ;
#55098 = CARTESIAN_POINT ( 'NONE',  ( 10.00000000000000000, 59.75893115100078745, -9.846743663894594434 ) ) ;
#55099 = CARTESIAN_POINT ( 'NONE',  ( 17.75000000000000355, 77.07179676972445748, -6.500000000000000888 ) ) ;
#55101 = CARTESIAN_POINT ( 'NONE',  ( 13.43411237798105340, 35.58196800326375353, 12.81628187352647963 ) ) ;
#55100 = CARTESIAN_POINT ( 'NONE',  ( -0.8801773607111009756, 63.06368534415484106, 1.068504757029289695E-15 ) ) ;
#55102 = CARTESIAN_POINT ( 'NONE',  ( 10.00000000000000178, 28.05374883491396787, 14.16423886937410082 ) ) ;
#55103 = CARTESIAN_POINT ( 'NONE',  ( 7.084665262690076126, 22.02201867748817321, -10.88017736071110164 ) ) ;
#55104 = ADVANCED_FACE ( 'NONE', ( #60236 ), #83451, .T. ) ;
#55105 = CARTESIAN_POINT ( 'NONE',  ( -0.5000000000000073275, 80.99999999999994316, 1.249999999999987121 ) ) ;
#55106 = CARTESIAN_POINT ( 'NONE',  ( 0.1532563361054082862, 1.217264484334117824, 2.638427012816831674 ) ) ;
#55107 = CARTESIAN_POINT ( 'NONE',  ( -4.923371831947292776, -13.15773551566587507, 8.527530157486181039 ) ) ;
#55108 = VERTEX_POINT ( 'NONE', #16739 ) ;
#55109 = TOROIDAL_SURFACE ( 'NONE', #98262, 14.49999999999999822, 0.5000000000000000000 ) ;
#55110 = DIRECTION ( 'NONE',  ( 0.000000000000000000, -1.000000000000000000, 0.000000000000000000 ) ) ;
#55111 = CIRCLE ( 'NONE', #67911, 19.99999999999999645 ) ;
#55112 = ORIENTED_EDGE ( 'NONE', *, *, #14696, .F. ) ;
#55113 = CARTESIAN_POINT ( 'NONE',  ( -4.164238869374099039, 6.803748834913967869, 8.674139862899312516E-16 ) ) ;
#55115 = CARTESIAN_POINT ( 'NONE',  ( 19.42250999205614548, 15.98035201082150714, -5.440088680355545492 ) ) ;
#55114 = CARTESIAN_POINT ( 'NONE',  ( 2.917880565312948704, 67.63708216824730357, 12.26659068614894643 ) ) ;
#55117 = CARTESIAN_POINT ( 'NONE',  ( 0.1532563361054100626, 60.80059781766744464, -2.638427012816831230 ) ) ;
#55116 = CARTESIAN_POINT ( 'NONE',  ( 10.00000000000000178, 37.25893115100078745, 9.846743663894594434 ) ) ;
#55118 = CARTESIAN_POINT ( 'NONE',  ( -13.07751017357372447, 15.00000000000000000, -6.263284095430686094 ) ) ;
#55119 = DIRECTION ( 'NONE',  ( -0.000000000000000000, -1.000000000000000000, -0.000000000000000000 ) ) ;
#55120 = B_SPLINE_CURVE_WITH_KNOTS ( 'NONE', 3,
 ( #40707, #86701, #16240, #71694 ),
 .UNSPECIFIED., .F., .F.,
 ( 4, 4 ),
 ( 5.444379262168902198E-17, 0.002562518741975294313 ),
 .UNSPECIFIED. ) ;
#55122 = CARTESIAN_POINT ( 'NONE',  ( 0.6178305044545818747, 8.498634669930421381, -9.382169495545419124 ) ) ;
#55121 = AXIS2_PLACEMENT_3D ( 'NONE', #7835, #53816, #69812 ) ;
#55123 = ORIENTED_EDGE ( 'NONE', *, *, #41553, .F. ) ;
#55124 = CARTESIAN_POINT ( 'NONE',  ( -4.164238869374099039, 41.80374883491397497, 8.674139862899312516E-16 ) ) ;
#55125 = ORIENTED_EDGE ( 'NONE', *, *, #71373, .F. ) ;
#55126 = CARTESIAN_POINT ( 'NONE',  ( 2.917880565312950480, 50.97041550158064638, -12.26659068614894821 ) ) ;
#55127 = ORIENTED_EDGE ( 'NONE', *, *, #44146, .T. ) ;
#55128 = CARTESIAN_POINT ( 'NONE',  ( 2.035157376598822676, 22.43868534415483396, -7.964842623401177768 ) ) ;
#55129 = LINE ( 'NONE', #47136, #77719 ) ;
#55130 = EDGE_CURVE ( 'NONE', #28596, #24676, #45683, .T. ) ;
#55131 = CARTESIAN_POINT ( 'NONE',  ( 10.00000000000000000, 31.81368534415483751, -10.88017736071110342 ) ) ;
#55132 = CARTESIAN_POINT ( 'NONE',  ( 1.472469842513823179, 55.59226448433412315, -4.923371831947296329 ) ) ;
#55133 = CARTESIAN_POINT ( 'NONE',  ( 7.084665262690076126, 39.10535201082150536, 10.88017736071109987 ) ) ;
#55134 = CARTESIAN_POINT ( 'NONE',  ( 2.035157376598824452, 68.68868534415484817, 7.964842623401179544 ) ) ;
#55135 = CARTESIAN_POINT ( 'NONE',  ( -0.8801773607111008646, 28.27201867748817321, 2.915334737309923430 ) ) ;
#55136 = EDGE_CURVE ( 'NONE', #38557, #63645, #94696, .T. ) ;
#55137 = FACE_OUTER_BOUND ( 'NONE', #3846, .T. ) ;
#55138 = VECTOR ( 'NONE', #86525, 1000.000000000000000 ) ;
#55139 =( NAMED_UNIT ( * ) PLANE_ANGLE_UNIT ( ) SI_UNIT ( $, .RADIAN. ) );
#55140 = CARTESIAN_POINT ( 'NONE',  ( -4.818768077838453401, -24.96217769840858125, 2.500000000000000888 ) ) ;
#55141 = ORIENTED_EDGE ( 'NONE', *, *, #49332, .T. ) ;
#55142 = DIRECTION ( 'NONE',  ( 1.000000000000000000, 0.000000000000000000, 0.000000000000000000 ) ) ;
#55143 = CARTESIAN_POINT ( 'NONE',  ( 1.472469842513823179, 46.42559781766745175, 4.923371831947296329 ) ) ;
#55144 = CARTESIAN_POINT ( 'NONE',  ( 7.551349515323100725, 15.00000000000000000, 12.08468537022911349 ) ) ;
#55145 = CARTESIAN_POINT ( 'NONE',  ( 3.591859063236763294, 48.29030133659708923, -11.09922568453595026 ) ) ;
#55146 = FILL_AREA_STYLE ('',( #39187 ) ) ;
#55147 = CARTESIAN_POINT ( 'NONE',  ( 1.514341385896460501, 15.00000000000000000, 15.92432625271834112 ) ) ;
#55148 = ORIENTED_EDGE ( 'NONE', *, *, #8493, .F. ) ;
#55149 = LINE ( 'NONE', #83700, #36444 ) ;
#55150 = DIRECTION ( 'NONE',  ( 1.000000000000000000, -0.000000000000000000, -0.000000000000000000 ) ) ;
#55151 = CARTESIAN_POINT ( 'NONE',  ( 10.00000000000000000, 49.75893115100078745, -9.846743663894594434 ) ) ;
#55152 = CARTESIAN_POINT ( 'NONE',  ( 17.08211943468705130, 43.47041550158063927, 12.26659068614894998 ) ) ;
#55153 = CARTESIAN_POINT ( 'NONE',  ( 5.076628168052703671, 61.84226448433412315, 8.527530157486179263 ) ) ;
#55154 = ORIENTED_EDGE ( 'NONE', *, *, #76610, .F. ) ;
#55155 =( REPRESENTATION_RELATIONSHIP ('NONE','NONE', #61309, #81163 ) REPRESENTATION_RELATIONSHIP_WITH_TRANSFORMATION ( #75212 )SHAPE_REPRESENTATION_RELATIONSHIP( ) );
#55156 = CARTESIAN_POINT ( 'NONE',  ( 0.1532563361054100626, 15.80059781766745353, -2.638427012816831230 ) ) ;
#55157 = CARTESIAN_POINT ( 'NONE',  ( 6.565887622018943937, 55.16530133659709634, 12.81628187352647430 ) ) ;
#55158 = AXIS2_PLACEMENT_3D ( 'NONE', #57747, #5754, #19758 ) ;
#55159 = CARTESIAN_POINT ( 'NONE',  ( 10.00000000000000178, 57.25893115100078745, 9.846743663894594434 ) ) ;
#55160 = CARTESIAN_POINT ( 'NONE',  ( 12.91533473730992121, 54.52201867748816255, 10.88017736071110164 ) ) ;
#55161 = CARTESIAN_POINT ( 'NONE',  ( -5.963430220938278126, 8.495456701841138880, 10.32896413005680358 ) ) ;
#55162 = AXIS2_PLACEMENT_3D ( 'NONE', #37762, #46712, #44743 ) ;
#55163 = ORIENTED_EDGE ( 'NONE', *, *, #23510, .T. ) ;
#55164 = CARTESIAN_POINT ( 'NONE',  ( 17.08211943468705130, 63.47041550158063927, 12.26659068614894998 ) ) ;
#55165 =( LENGTH_UNIT ( ) NAMED_UNIT ( * ) SI_UNIT ( .MILLI., .METRE. ) );
#55166 = CARTESIAN_POINT ( 'NONE',  ( 7.084665262690076126, 34.10535201082151247, 10.88017736071109987 ) ) ;
#55168 = CARTESIAN_POINT ( 'NONE',  ( 10.00000000000000000, 56.81368534415484106, -10.88017736071110342 ) ) ;
#55167 = CARTESIAN_POINT ( 'NONE',  ( 21.09922568453594849, 16.20696800326375353, 6.408140936763242479 ) ) ;
#55169 = DIRECTION ( 'NONE',  ( 1.000000000000000000, 0.000000000000000000, -0.000000000000000000 ) ) ;
#55170 = CARTESIAN_POINT ( 'NONE',  ( -11.35178980618966804, 14.49999999999999112, -9.804941009312102551 ) ) ;
#55171 = CARTESIAN_POINT ( 'NONE',  ( -14.97687855664610979, 14.63606903414041227, -0.8325315005902708121 ) ) ;
#55173 = CARTESIAN_POINT ( 'NONE',  ( 1.821158202401517601, 11.16688879859523276, 6.499999999999976019 ) ) ;
#55172 = CARTESIAN_POINT ( 'NONE',  ( 2.035157376598822676, 57.43868534415484106, -7.964842623401177768 ) ) ;
#55174 = CARTESIAN_POINT ( 'NONE',  ( 5.076628168052704559, 55.17559781766745175, -8.527530157486179263 ) ) ;
#55175 =( LENGTH_UNIT ( ) NAMED_UNIT ( * ) SI_UNIT ( .MILLI., .METRE. ) );
#55176 = CARTESIAN_POINT ( 'NONE',  ( 12.26659068614894466, 29.72041550158063927, -7.082119434687053960 ) ) ;
#55177 = CARTESIAN_POINT ( 'NONE',  ( 22.81628187352647785, 11.62363466993042138, 6.195893100308588602E-16 ) ) ;
#55178 = CARTESIAN_POINT ( 'NONE',  ( -0.8801773607111009756, 13.06368534415483929, 1.068504757029289695E-15 ) ) ;
#55179 = FILL_AREA_STYLE_COLOUR ( '', #83591 ) ;
#55180 = CARTESIAN_POINT ( 'NONE',  ( -2.266590686148945544, 37.22041550158063217, 7.082119434687048631 ) ) ;
#55181 = ADVANCED_FACE ( 'NONE', ( #87185 ), #93706, .T. ) ;
#55182 = CARTESIAN_POINT ( 'NONE',  ( 24.16423886937410614, 24.51208216824730002, -3.795296366450302550 ) ) ;
#55183 = CARTESIAN_POINT ( 'NONE',  ( 0.5774900079438607392, 3.480352010821504916, 5.440088680355550821 ) ) ;
#55184 = VECTOR ( 'NONE', #78597, 1000.000000000000000 ) ;
#55185 = CARTESIAN_POINT ( 'NONE',  ( 14.92337183194729988, 29.34226448433411960, -8.527530157486177487 ) ) ;
#55186 = CARTESIAN_POINT ( 'NONE',  ( 18.52753015748618282, 18.92559781766745175, -4.923371831947291888 ) ) ;
#55187 = CARTESIAN_POINT ( 'NONE',  ( 20.88017736071110519, 15.56368534415483751, 2.639326808657452039E-16 ) ) ;
#55188 = AXIS2_PLACEMENT_3D ( 'NONE', #82466, #89964, #67967 ) ;
#55189 = ORIENTED_EDGE ( 'NONE', *, *, #41267, .F. ) ;
#55190 = CARTESIAN_POINT ( 'NONE',  ( 7.361572987183170547, 37.05059781766744464, 9.846743663894590881 ) ) ;
#55191 = CARTESIAN_POINT ( 'NONE',  ( 7.084665262690076126, 34.10535201082151247, 10.88017736071109987 ) ) ;
#55192 = CARTESIAN_POINT ( 'NONE',  ( 18.52753015748618282, 58.92559781766745886, -4.923371831947291888 ) ) ;
#55194 = CARTESIAN_POINT ( 'NONE',  ( -11.22915323889568562, 15.00000000000000000, -8.773176023390764300 ) ) ;
#55193 = CARTESIAN_POINT ( 'NONE',  ( -4.164238869374099927, 22.01208216824730357, 3.795296366450308767 ) ) ;
#55195 = CARTESIAN_POINT ( 'NONE',  ( -2.962741594153171842, 15.00000000000000000, 13.93860331045670975 ) ) ;
#55196 = COLOUR_RGB ( '', 0.66274510, 0.83137255, 0.94901961) ;
#55197 = UNCERTAINTY_MEASURE_WITH_UNIT (LENGTH_MEASURE( 1.000000000000000082E-05 ), #63724, 'distance_accuracy_value', 'NONE');
#55198 =( BOUNDED_SURFACE ( )  B_SPLINE_SURFACE ( 1, 2, ( 
 ( #35849, #58841, #95371, #66337, #65351, #95879, #20858, #13348, #27360, #57853, #359, #14347, #90315, #38335, #91817, #75823, #44328, #53315, #98361, #8320, #837, #30311, #21853, #76318, #52820, #52333, #91311, #30808, #14854, #45326, #31297, #38824, #15348, #82827, #7836, #45832, #36846, #7345, #83823, #13849, #69315, #59821, #74832, #51841, #15830, #82328, #29324, #22840, #60812, #68828, #44818, #75325, #6838, #37845, #53818, #67843, #90818, #61306, #83328, #6336, #67336, #37352, #29819, #60328, #22348, #84330, #23338, #68336, #98857, #61797, #46317, #92305, #76803, #97861, #40788, #70803, #54295, #46799, #48761, #62286, #55791, #9297, #92790, #25788, #17794, #69813, #8804, #32773, #78783, #10778, #79268, #71768, #85301, #56283, #32277, #94262, #55285, #85794, #62785, #86779, #41294, #1336, #10290, #3278, #33742, #18282, #84810, #93777, #93284, #16316, #78281, #64243, #24808, #63268, #23832, #33264, #17307, #77292, #2320, #24319, #86286, #48269, #71287, #39317, #9796, #54785, #63756, #40295, #31787, #16808, #25304, #47283, #77785, #47784, #2811, #39807, #70308, #1824, #96253, #73723, #95243, #43724, #74210, #66221, #18778, #34235, #5254, #4264, #13227, #20738, #72731, #65228, #35732, #51231, #27238, #28226, #26750, #49260, #96751, #88730, #34737, #36229, #80744, #35229, #12732, #57245, #95754, #57733, #49739, #58725, #81715, #64731, #11259, #88237, #87253, #26261, #50230, #19745, #27732, #12239, #87742, #20242, #5740, #42749, #42262, #94761, #19254, #56759, #79760, #80246, #73230, #11753, #4758, #89229, #41777, #72247, #50745, #58214, #3781, #65727, #81233, #43229, #82216, #76687, #52706, #60208, #60695, #29699, #44211, #14734, #84213, #91194, #98240, #90703, #22231, #37721, #237, #83213, #83708, #13726, #45210, #30685, #59212, #68225, #75708, #52219, #7222, #15226, #29212, #6231, #53203, #7723, #98745, #89717, #30194, #14231, #23219, #15719, #22720, #36734, #45705, #67726, #67225, #76206, #38220, #68705, #61193, #46204, #53692, #91701, #97748, #8208, #66728, #51734, #97252, #28722, #21231, #74719, #59711, #90207, #21737, #82713, #44710, #75209, #6720, #37236, #55670, #77178, #1217, #31672, #93162, #40670, #54664, #77666, #63153, #39199, #55159, #94146, #38703, #78666, #25673, #79146, #47161, #24687, #10172, #62164, #2692, #86170, #69686, #33144, #93656, #56167, #9180, #92669, #92192, #86659, #39697, #69202, #726, #8685, #32158, #31182, #24197, #85180, #17679, #17192, #71168, #16691, #70185, #40174, #1702, #47672, #78167, #9676, #25191, #18164, #48642, #61672, #62660, #63638, #85673, #23718, #70678, #2199, #32660 ),
 ( #48153, #54177, #84689, #16199, #46681, #26152, #20620, #95631, #4148, #4643, #72613, #87131, #57618, #28107, #35107, #42148, #34613, #65108, #80629, #43113, #27119, #27614, #56646, #88117, #73602, #3164, #12125, #19626, #95122, #50119, #58100, #72129, #49142, #96133, #50620, #42626, #33626, #73104, #57127, #66101, #58607, #65606, #79643, #88607, #11632, #11142, #20117, #81111, #12612, #5127, #89109, #96630, #35615, #41661, #51110, #10658, #94642, #41172, #71655, #64125, #18654, #3656, #34121, #64613, #26629, #87624, #19138, #49615, #80125, #98625, #21113, #44088, #74597, #37110, #83590, #97627, #21616, #7101, #82096, #98113, #38102, #81597, #22602, #68590, #23099, #90089, #67606, #53079, #6111, #45583, #30074, #13607, #76078, #37603, #120, #52102, #36616, #36102, #30567, #82594, #13109, #43604, #51613, #75091, #74091, #67103, #29091, #75589, #45084, #61071, #59590, #68098, #59095, #97136, #91583, #29575, #6597, #60583, #44593, #89604, #60079, #5625, #91075, #14109, #90580, #22106, #52586, #15106, #83089, #7607, #28606, #14618, #66608, #46081, #24579, #16574, #39078, #32037, #2082, #16076, #92069, #40055, #93539, #77545, #76569, #55040, #1092, #10055, #2577, #62540, #23597, #78050, #54546, #54061, #93046, #32542, #47049, #9064, #33033, #40554, #17070, #84575, #9553, #47553, #38583, #39576, #85558, #15598, #71054, #61561, #8087, #53570, #17566, #84083, #31062, #70554, #63042, #25070, #46562, #77063, #8574, #70065, #55553, #69572, #92551, #86054, #31553, #1588, #63529, #69081, #48031, #94037, #616, #62049, #78544, #24079, #85063, #88501, #42514, #26042, #20004, #80517, #81002, #34007, #56533, #79028, #43003, #95009, #65992, #25558, #64011, #19029, #56051, #18534, #49025, #72998, #4036, #57995, #79531, #41551, #27010, #11031, #34499, #64990, #12504, #94523, #86542, #50504, #87022, #57014, #72017, #3547, #65497, #10540, #3059, #96017, #73487, #18049, #64503, #80013, #27500, #26517, #5014, #4528, #87516, #35497, #12015, #48526, #49506, #11516, #41050, #71549, #42040, #33514, #72504, #95517, #57508, #88005, #19516, #50013, #34992, #74977, #29959, #89492, #13495, #98006, #21001, #6482, #36987, #83470, #66491, #37985, #22486, #97018, #28973, #28495, #58988, #37490, #50992, #73987, #90460, #59967, #14991, #35989, #52471, #5512, #12990, #7489, #82480, #89977, #21996, #59476, #51489, #44477, #45462, #82976, #21494, #51991, #13999, #67484, #60465, #29459, #14496, #43486, #44967, #90953, #89000, #75470, #6986, #81984, #67979, #98505, #43974, #74476, #52959, #75961, #96519, #20506, #27992, #6001, #58488, #81487, #36495, #66987, #97509 ) ),
 .UNSPECIFIED., .F., .F., .F. ) 
 B_SPLINE_SURFACE_WITH_KNOTS ( ( 2, 2 ),
 ( 3, 2, 2, 2, 2, 2, 2, 2, 2, 2, 2, 2, 2, 2, 2, 2, 2, 2, 2, 2, 2, 2, 2, 2, 2, 2, 2, 2, 2, 2, 2, 2, 2, 2, 2, 2, 2, 2, 2, 2, 2, 2, 2, 2, 2, 2, 2, 2, 2, 2, 2, 2, 2, 2, 2, 2, 2, 2, 2, 2, 2, 2, 2, 2, 2, 2, 2, 2, 2, 2, 2, 2, 2, 2, 2, 2, 2, 2, 2, 2, 2, 2, 2, 2, 2, 2, 2, 2, 2, 2, 2, 2, 2, 2, 2, 2, 2, 2, 2, 2, 2, 2, 2, 2, 2, 2, 2, 2, 2, 2, 2, 2, 2, 2, 2, 2, 2, 2, 2, 2, 2, 2, 2, 2, 2, 2, 2, 2, 2, 2, 2, 2, 2, 2, 2, 2, 2, 2, 2, 2, 2, 2, 2, 2, 2, 2, 2, 2, 2, 2, 2, 2, 2, 2, 2, 2, 2, 2, 2, 2, 2, 2, 3 ),
 ( 0.000000000000000000, 1.000000000000000000 ),
 ( 0.000000000000000000, 0.005952380952380952051, 0.01190476190476190410, 0.01785714285714285615, 0.02380952380952380820, 0.02976190476190476025, 0.03571428571428571230, 0.04166666666666666435, 0.04761904761904761640, 0.05357142857142856845, 0.05952380952380952051, 0.06547619047619047949, 0.07142857142857142461, 0.07738095238095238360, 0.08333333333333332871, 0.08928571428571428770, 0.09523809523809523281, 0.1011904761904761918, 0.1071428571428571369, 0.1130952380952380959, 0.1190476190476190410, 0.1250000000000000000, 0.1309523809523809590, 0.1369047619047619180, 0.1428571428571428492, 0.1488095238095238082, 0.1547619047619047672, 0.1607142857142857262, 0.1666666666666666574, 0.1726190476190476164, 0.1785714285714285754, 0.1845238095238095344, 0.1904761904761904656, 0.1964285714285714246, 0.2023809523809523836, 0.2083333333333333426, 0.2142857142857142738, 0.2202380952380952328, 0.2261904761904761918, 0.2321428571428571508, 0.2380952380952380820, 0.2440476190476190410, 0.2500000000000000000, 0.2559523809523809312, 0.2619047619047619180, 0.2678571428571428492, 0.2738095238095238360, 0.2797619047619047672, 0.2857142857142856984, 0.2916666666666666852, 0.2976190476190476164, 0.3035714285714285476, 0.3095238095238095344, 0.3154761904761904656, 0.3214285714285714524, 0.3273809523809523836, 0.3333333333333333148, 0.3392857142857143016, 0.3452380952380952328, 0.3511904761904761640, 0.3571428571428571508, 0.3630952380952380820, 0.3690476190476190688, 0.3750000000000000000, 0.3809523809523809312, 0.3869047619047619180, 0.3928571428571428492, 0.3988095238095238360, 0.4047619047619047672, 0.4107142857142856984, 0.4166666666666666852, 0.4226190476190476164, 0.4285714285714285476, 0.4345238095238095344, 0.4404761904761904656, 0.4464285714285714524, 0.4523809523809523836, 0.4583333333333333148, 0.4642857142857143016, 0.4702380952380952328, 0.4761904761904761640, 0.4821428571428571508, 0.4880952380952380820, 0.4940476190476190688, 0.5000000000000000000, 0.5059523809523809312, 0.5119047619047618625, 0.5178571428571429047, 0.5238095238095238360, 0.5297619047619047672, 0.5357142857142856984, 0.5416666666666666297, 0.5476190476190476719, 0.5535714285714286031, 0.5595238095238095344, 0.5654761904761904656, 0.5714285714285713969, 0.5773809523809523281, 0.5833333333333333703, 0.5892857142857143016, 0.5952380952380952328, 0.6011904761904761640, 0.6071428571428570953, 0.6130952380952381375, 0.6190476190476190688, 0.6250000000000000000, 0.6309523809523809312, 0.6369047619047618625, 0.6428571428571429047, 0.6488095238095238360, 0.6547619047619047672, 0.6607142857142856984, 0.6666666666666666297, 0.6726190476190476719, 0.6785714285714286031, 0.6845238095238095344, 0.6904761904761904656, 0.6964285714285713969, 0.7023809523809523281, 0.7083333333333333703, 0.7142857142857143016, 0.7202380952380952328, 0.7261904761904761640, 0.7321428571428570953, 0.7380952380952381375, 0.7440476190476190688, 0.7500000000000000000, 0.7559523809523809312, 0.7619047619047618625, 0.7678571428571429047, 0.7738095238095238360, 0.7797619047619047672, 0.7857142857142856984, 0.7916666666666666297, 0.7976190476190476719, 0.8035714285714286031, 0.8095238095238095344, 0.8154761904761904656, 0.8214285714285713969, 0.8273809523809523281, 0.8333333333333333703, 0.8392857142857143016, 0.8452380952380952328, 0.8511904761904761640, 0.8571428571428570953, 0.8630952380952381375, 0.8690476190476190688, 0.8750000000000000000, 0.8809523809523809312, 0.8869047619047618625, 0.8928571428571429047, 0.8988095238095238360, 0.9047619047619047672, 0.9107142857142856984, 0.9166666666666666297, 0.9226190476190476719, 0.9285714285714286031, 0.9345238095238095344, 0.9404761904761904656, 0.9464285714285713969, 0.9523809523809523281, 0.9583333333333333703, 0.9642857142857143016 ),
 .UNSPECIFIED. ) 
 GEOMETRIC_REPRESENTATION_ITEM ( )  RATIONAL_B_SPLINE_SURFACE ( (
 ( 1.000000000000000000, 0.9659258262890683122, 1.000000000000000000, 0.9659258262890683122, 1.000000000000000000, 0.9659258262890683122, 1.000000000000000000, 0.9659258262890683122, 1.000000000000000000, 0.9659258262890683122, 1.000000000000000000, 0.9659258262890683122, 1.000000000000000000, 0.9659258262890683122, 1.000000000000000000, 0.9659258262890683122, 1.000000000000000000, 0.9659258262890683122, 1.000000000000000000, 0.9659258262890683122, 1.000000000000000000, 0.9659258262890683122, 1.000000000000000000, 0.9659258262890683122, 1.000000000000000000, 0.9659258262890683122, 1.000000000000000000, 0.9659258262890683122, 1.000000000000000000, 0.9659258262890683122, 1.000000000000000000, 0.9659258262890683122, 1.000000000000000000, 0.9659258262890683122, 1.000000000000000000, 0.9659258262890683122, 1.000000000000000000, 0.9659258262890683122, 1.000000000000000000, 0.9659258262890683122, 1.000000000000000000, 0.9659258262890683122, 1.000000000000000000, 0.9659258262890683122, 1.000000000000000000, 0.9659258262890683122, 1.000000000000000000, 0.9659258262890683122, 1.000000000000000000, 0.9659258262890683122, 1.000000000000000000, 0.9659258262890683122, 1.000000000000000000, 0.9659258262890683122, 1.000000000000000000, 0.9659258262890683122, 1.000000000000000000, 0.9659258262890683122, 1.000000000000000000, 0.9659258262890683122, 1.000000000000000000, 0.9659258262890683122, 1.000000000000000000, 0.9659258262890683122, 1.000000000000000000, 0.9659258262890683122, 1.000000000000000000, 0.9659258262890683122, 1.000000000000000000, 0.9659258262890683122, 1.000000000000000000, 0.9659258262890683122, 1.000000000000000000, 0.9659258262890683122, 1.000000000000000000, 0.9659258262890683122, 1.000000000000000000, 0.9659258262890683122, 1.000000000000000000, 0.9659258262890683122, 1.000000000000000000, 0.9659258262890683122, 1.000000000000000000, 0.9659258262890683122, 1.000000000000000000, 0.9659258262890683122, 1.000000000000000000, 0.9659258262890683122, 1.000000000000000000, 0.9659258262890683122, 1.000000000000000000, 0.9659258262890683122, 1.000000000000000000, 0.9659258262890683122, 1.000000000000000000, 0.9659258262890683122, 1.000000000000000000, 0.9659258262890683122, 1.000000000000000000, 0.9659258262890683122, 1.000000000000000000, 0.9659258262890683122, 1.000000000000000000, 0.9659258262890683122, 1.000000000000000000, 0.9659258262890683122, 1.000000000000000000, 0.9659258262890683122, 1.000000000000000000, 0.9659258262890683122, 1.000000000000000000, 0.9659258262890683122, 1.000000000000000000, 0.9659258262890683122, 1.000000000000000000, 0.9659258262890683122, 1.000000000000000000, 0.9659258262890683122, 1.000000000000000000, 0.9659258262890683122, 1.000000000000000000, 0.9659258262890683122, 1.000000000000000000, 0.9659258262890683122, 1.000000000000000000, 0.9659258262890683122, 1.000000000000000000, 0.9659258262890683122, 1.000000000000000000, 0.9659258262890683122, 1.000000000000000000, 0.9659258262890683122, 1.000000000000000000, 0.9659258262890683122, 1.000000000000000000, 0.9659258262890683122, 1.000000000000000000, 0.9659258262890683122, 1.000000000000000000, 0.9659258262890683122, 1.000000000000000000, 0.9659258262890683122, 1.000000000000000000, 0.9659258262890683122, 1.000000000000000000, 0.9659258262890683122, 1.000000000000000000, 0.9659258262890683122, 1.000000000000000000, 0.9659258262890683122, 1.000000000000000000, 0.9659258262890683122, 1.000000000000000000, 0.9659258262890683122, 1.000000000000000000, 0.9659258262890683122, 1.000000000000000000, 0.9659258262890683122, 1.000000000000000000, 0.9659258262890683122, 1.000000000000000000, 0.9659258262890683122, 1.000000000000000000, 0.9659258262890683122, 1.000000000000000000, 0.9659258262890683122, 1.000000000000000000, 0.9659258262890683122, 1.000000000000000000, 0.9659258262890683122, 1.000000000000000000, 0.9659258262890683122, 1.000000000000000000, 0.9659258262890683122, 1.000000000000000000, 0.9659258262890683122, 1.000000000000000000, 0.9659258262890683122, 1.000000000000000000, 0.9659258262890683122, 1.000000000000000000, 0.9659258262890683122, 1.000000000000000000, 0.9659258262890683122, 1.000000000000000000, 0.9659258262890683122, 1.000000000000000000, 0.9659258262890683122, 1.000000000000000000, 0.9659258262890683122, 1.000000000000000000, 0.9659258262890683122, 1.000000000000000000, 0.9659258262890683122, 1.000000000000000000, 0.9659258262890683122, 1.000000000000000000, 0.9659258262890683122, 1.000000000000000000, 0.9659258262890683122, 1.000000000000000000, 0.9659258262890683122, 1.000000000000000000, 0.9659258262890683122, 1.000000000000000000, 0.9659258262890683122, 1.000000000000000000, 0.9659258262890683122, 1.000000000000000000, 0.9659258262890683122, 1.000000000000000000, 0.9659258262890683122, 1.000000000000000000, 0.9659258262890683122, 1.000000000000000000, 0.9659258262890683122, 1.000000000000000000, 0.9659258262890683122, 1.000000000000000000, 0.9659258262890683122, 1.000000000000000000, 0.9659258262890683122, 1.000000000000000000, 0.9659258262890683122, 1.000000000000000000, 0.9659258262890683122, 1.000000000000000000, 0.9659258262890683122, 1.000000000000000000, 0.9659258262890683122, 1.000000000000000000, 0.9659258262890683122, 1.000000000000000000, 0.9659258262890683122, 1.000000000000000000, 0.9659258262890683122, 1.000000000000000000, 0.9659258262890683122, 1.000000000000000000, 0.9659258262890683122, 1.000000000000000000, 0.9659258262890683122, 1.000000000000000000, 0.9659258262890683122, 1.000000000000000000, 0.9659258262890683122, 1.000000000000000000, 0.9659258262890683122, 1.000000000000000000, 0.9659258262890683122, 1.000000000000000000, 0.9659258262890683122, 1.000000000000000000, 0.9659258262890683122, 1.000000000000000000, 0.9659258262890683122, 1.000000000000000000, 0.9659258262890683122, 1.000000000000000000, 0.9659258262890683122, 1.000000000000000000, 0.9659258262890683122, 1.000000000000000000, 0.9659258262890683122, 1.000000000000000000, 0.9659258262890683122, 1.000000000000000000, 0.9659258262890683122, 1.000000000000000000, 0.9659258262890683122, 1.000000000000000000, 0.9659258262890683122, 1.000000000000000000, 0.9659258262890683122, 1.000000000000000000, 0.9659258262890683122, 1.000000000000000000, 0.9659258262890683122, 1.000000000000000000, 0.9659258262890683122, 1.000000000000000000, 0.9659258262890683122, 1.000000000000000000, 0.9659258262890683122, 1.000000000000000000, 0.9659258262890683122, 1.000000000000000000, 0.9659258262890683122, 1.000000000000000000, 0.9659258262890683122, 1.000000000000000000, 0.9659258262890683122, 1.000000000000000000, 0.9659258262890683122, 1.000000000000000000, 0.9659258262890683122, 1.000000000000000000, 0.9659258262890683122, 1.000000000000000000, 0.9659258262890683122, 1.000000000000000000, 0.9659258262890683122, 1.000000000000000000, 0.9659258262890683122, 1.000000000000000000, 0.9659258262890683122, 1.000000000000000000, 0.9659258262890683122, 1.000000000000000000, 0.9659258262890683122, 1.000000000000000000, 0.9659258262890683122, 1.000000000000000000, 0.9659258262890683122, 1.000000000000000000, 0.9659258262890683122, 1.000000000000000000, 0.9659258262890683122, 1.000000000000000000, 0.9659258262890683122, 1.000000000000000000, 0.9659258262890683122, 1.000000000000000000, 0.9659258262890683122, 1.000000000000000000),
 ( 1.000000000000000000, 0.9659258262890683122, 1.000000000000000000, 0.9659258262890683122, 1.000000000000000000, 0.9659258262890683122, 1.000000000000000000, 0.9659258262890683122, 1.000000000000000000, 0.9659258262890683122, 1.000000000000000000, 0.9659258262890683122, 1.000000000000000000, 0.9659258262890683122, 1.000000000000000000, 0.9659258262890683122, 1.000000000000000000, 0.9659258262890683122, 1.000000000000000000, 0.9659258262890683122, 1.000000000000000000, 0.9659258262890683122, 1.000000000000000000, 0.9659258262890683122, 1.000000000000000000, 0.9659258262890683122, 1.000000000000000000, 0.9659258262890683122, 1.000000000000000000, 0.9659258262890683122, 1.000000000000000000, 0.9659258262890683122, 1.000000000000000000, 0.9659258262890683122, 1.000000000000000000, 0.9659258262890683122, 1.000000000000000000, 0.9659258262890683122, 1.000000000000000000, 0.9659258262890683122, 1.000000000000000000, 0.9659258262890683122, 1.000000000000000000, 0.9659258262890683122, 1.000000000000000000, 0.9659258262890683122, 1.000000000000000000, 0.9659258262890683122, 1.000000000000000000, 0.9659258262890683122, 1.000000000000000000, 0.9659258262890683122, 1.000000000000000000, 0.9659258262890683122, 1.000000000000000000, 0.9659258262890683122, 1.000000000000000000, 0.9659258262890683122, 1.000000000000000000, 0.9659258262890683122, 1.000000000000000000, 0.9659258262890683122, 1.000000000000000000, 0.9659258262890683122, 1.000000000000000000, 0.9659258262890683122, 1.000000000000000000, 0.9659258262890683122, 1.000000000000000000, 0.9659258262890683122, 1.000000000000000000, 0.9659258262890683122, 1.000000000000000000, 0.9659258262890683122, 1.000000000000000000, 0.9659258262890683122, 1.000000000000000000, 0.9659258262890683122, 1.000000000000000000, 0.9659258262890683122, 1.000000000000000000, 0.9659258262890683122, 1.000000000000000000, 0.9659258262890683122, 1.000000000000000000, 0.9659258262890683122, 1.000000000000000000, 0.9659258262890683122, 1.000000000000000000, 0.9659258262890683122, 1.000000000000000000, 0.9659258262890683122, 1.000000000000000000, 0.9659258262890683122, 1.000000000000000000, 0.9659258262890683122, 1.000000000000000000, 0.9659258262890683122, 1.000000000000000000, 0.9659258262890683122, 1.000000000000000000, 0.9659258262890683122, 1.000000000000000000, 0.9659258262890683122, 1.000000000000000000, 0.9659258262890683122, 1.000000000000000000, 0.9659258262890683122, 1.000000000000000000, 0.9659258262890683122, 1.000000000000000000, 0.9659258262890683122, 1.000000000000000000, 0.9659258262890683122, 1.000000000000000000, 0.9659258262890683122, 1.000000000000000000, 0.9659258262890683122, 1.000000000000000000, 0.9659258262890683122, 1.000000000000000000, 0.9659258262890683122, 1.000000000000000000, 0.9659258262890683122, 1.000000000000000000, 0.9659258262890683122, 1.000000000000000000, 0.9659258262890683122, 1.000000000000000000, 0.9659258262890683122, 1.000000000000000000, 0.9659258262890683122, 1.000000000000000000, 0.9659258262890683122, 1.000000000000000000, 0.9659258262890683122, 1.000000000000000000, 0.9659258262890683122, 1.000000000000000000, 0.9659258262890683122, 1.000000000000000000, 0.9659258262890683122, 1.000000000000000000, 0.9659258262890683122, 1.000000000000000000, 0.9659258262890683122, 1.000000000000000000, 0.9659258262890683122, 1.000000000000000000, 0.9659258262890683122, 1.000000000000000000, 0.9659258262890683122, 1.000000000000000000, 0.9659258262890683122, 1.000000000000000000, 0.9659258262890683122, 1.000000000000000000, 0.9659258262890683122, 1.000000000000000000, 0.9659258262890683122, 1.000000000000000000, 0.9659258262890683122, 1.000000000000000000, 0.9659258262890683122, 1.000000000000000000, 0.9659258262890683122, 1.000000000000000000, 0.9659258262890683122, 1.000000000000000000, 0.9659258262890683122, 1.000000000000000000, 0.9659258262890683122, 1.000000000000000000, 0.9659258262890683122, 1.000000000000000000, 0.9659258262890683122, 1.000000000000000000, 0.9659258262890683122, 1.000000000000000000, 0.9659258262890683122, 1.000000000000000000, 0.9659258262890683122, 1.000000000000000000, 0.9659258262890683122, 1.000000000000000000, 0.9659258262890683122, 1.000000000000000000, 0.9659258262890683122, 1.000000000000000000, 0.9659258262890683122, 1.000000000000000000, 0.9659258262890683122, 1.000000000000000000, 0.9659258262890683122, 1.000000000000000000, 0.9659258262890683122, 1.000000000000000000, 0.9659258262890683122, 1.000000000000000000, 0.9659258262890683122, 1.000000000000000000, 0.9659258262890683122, 1.000000000000000000, 0.9659258262890683122, 1.000000000000000000, 0.9659258262890683122, 1.000000000000000000, 0.9659258262890683122, 1.000000000000000000, 0.9659258262890683122, 1.000000000000000000, 0.9659258262890683122, 1.000000000000000000, 0.9659258262890683122, 1.000000000000000000, 0.9659258262890683122, 1.000000000000000000, 0.9659258262890683122, 1.000000000000000000, 0.9659258262890683122, 1.000000000000000000, 0.9659258262890683122, 1.000000000000000000, 0.9659258262890683122, 1.000000000000000000, 0.9659258262890683122, 1.000000000000000000, 0.9659258262890683122, 1.000000000000000000, 0.9659258262890683122, 1.000000000000000000, 0.9659258262890683122, 1.000000000000000000, 0.9659258262890683122, 1.000000000000000000, 0.9659258262890683122, 1.000000000000000000, 0.9659258262890683122, 1.000000000000000000, 0.9659258262890683122, 1.000000000000000000, 0.9659258262890683122, 1.000000000000000000, 0.9659258262890683122, 1.000000000000000000, 0.9659258262890683122, 1.000000000000000000, 0.9659258262890683122, 1.000000000000000000, 0.9659258262890683122, 1.000000000000000000, 0.9659258262890683122, 1.000000000000000000, 0.9659258262890683122, 1.000000000000000000, 0.9659258262890683122, 1.000000000000000000, 0.9659258262890683122, 1.000000000000000000, 0.9659258262890683122, 1.000000000000000000, 0.9659258262890683122, 1.000000000000000000, 0.9659258262890683122, 1.000000000000000000, 0.9659258262890683122, 1.000000000000000000, 0.9659258262890683122, 1.000000000000000000, 0.9659258262890683122, 1.000000000000000000, 0.9659258262890683122, 1.000000000000000000, 0.9659258262890683122, 1.000000000000000000, 0.9659258262890683122, 1.000000000000000000, 0.9659258262890683122, 1.000000000000000000, 0.9659258262890683122, 1.000000000000000000, 0.9659258262890683122, 1.000000000000000000, 0.9659258262890683122, 1.000000000000000000, 0.9659258262890683122, 1.000000000000000000, 0.9659258262890683122, 1.000000000000000000, 0.9659258262890683122, 1.000000000000000000, 0.9659258262890683122, 1.000000000000000000, 0.9659258262890683122, 1.000000000000000000, 0.9659258262890683122, 1.000000000000000000, 0.9659258262890683122, 1.000000000000000000, 0.9659258262890683122, 1.000000000000000000, 0.9659258262890683122, 1.000000000000000000, 0.9659258262890683122, 1.000000000000000000, 0.9659258262890683122, 1.000000000000000000, 0.9659258262890683122, 1.000000000000000000, 0.9659258262890683122, 1.000000000000000000, 0.9659258262890683122, 1.000000000000000000, 0.9659258262890683122, 1.000000000000000000, 0.9659258262890683122, 1.000000000000000000, 0.9659258262890683122, 1.000000000000000000, 0.9659258262890683122, 1.000000000000000000, 0.9659258262890683122, 1.000000000000000000, 0.9659258262890683122, 1.000000000000000000) ) ) 
 REPRESENTATION_ITEM ( '' )  SURFACE ( )  );
#55199 = CARTESIAN_POINT ( 'NONE',  ( 10.00000000000000000, 14.75893115100078568, -9.846743663894594434 ) ) ;
#55200 = CARTESIAN_POINT ( 'NONE',  ( 13.43411237798106583, 47.66530133659709634, -12.81628187352647252 ) ) ;
#55201 = CARTESIAN_POINT ( 'NONE',  ( 19.84674366389459621, 58.50893115100078745, 7.409399052514197653E-17 ) ) ;
#55202 = ORIENTED_EDGE ( 'NONE', *, *, #13781, .F. ) ;
#55203 = CARTESIAN_POINT ( 'NONE',  ( 9.209312257404453916, -9.300771453418956725, -4.000000000000000000 ) ) ;
#55204 = CARTESIAN_POINT ( 'NONE',  ( 14.22792531055121579, 15.00000000000000711, -3.387425595041105630 ) ) ;
#55205 = CARTESIAN_POINT ( 'NONE',  ( -2.266590686148945544, 66.38708216824730357, -7.082119434687050408 ) ) ;
#55206 = CARTESIAN_POINT ( 'NONE',  ( -4.164238869374098151, 16.59541550158063927, -3.795296366450310543 ) ) ;
#55207 = CARTESIAN_POINT ( 'NONE',  ( -0.8801773607110991993, 62.85535201082150536, -2.915334737309923874 ) ) ;
#55208 = CARTESIAN_POINT ( 'NONE',  ( 0.1532563361054100626, 35.80059781766745175, -2.638427012816831230 ) ) ;
#55209 = CARTESIAN_POINT ( 'NONE',  ( -0.8801773607111009756, 18.06368534415484106, 1.068504757029289695E-15 ) ) ;
#55210 = CARTESIAN_POINT ( 'NONE',  ( -7.684764310694712997, 14.63606916355955434, -12.88194075009949557 ) ) ;
#55211 = CARTESIAN_POINT ( 'NONE',  ( 17.20831665107776587, 62.88393115100078745, 7.208316651077764980 ) ) ;
#55212 = CARTESIAN_POINT ( 'NONE',  ( 14.92337183194729633, 2.675597817667451750, 8.527530157486181039 ) ) ;
#55213 = CARTESIAN_POINT ( 'NONE',  ( 6.565887622018943937, 60.16530133659707502, 12.81628187352647430 ) ) ;
#55214 = EDGE_LOOP ( 'NONE', ( #76555, #94965, #3219, #94614 ) ) ;
#55215 = ORIENTED_EDGE ( 'NONE', *, *, #64209, .T. ) ;
#55216 = DIRECTION ( 'NONE',  ( 0.000000000000000000, 1.000000000000000000, 0.000000000000000000 ) ) ;
#55217 = AXIS2_PLACEMENT_3D ( 'NONE', #27133, #35124, #80645 ) ;
#55218 = LINE ( 'NONE', #48210, #33 ) ;
#55220 = EDGE_CURVE ( 'NONE', #85529, #37825, #82858, .T. ) ;
#55219 = SURFACE_STYLE_USAGE ( .BOTH. , #33203 ) ;
#55221 = CARTESIAN_POINT ( 'NONE',  ( -0.3689425029237898834, 41.17874883491397497, -10.36894250292378850 ) ) ;
#55222 = CARTESIAN_POINT ( 'NONE',  ( 17.20831665107776587, 37.88393115100078745, 7.208316651077764980 ) ) ;
#55223 = CARTESIAN_POINT ( 'NONE',  ( 18.52753015748617571, 23.09226448433411960, 4.923371831947298993 ) ) ;
#55224 = DIRECTION ( 'NONE',  ( 0.000000000000000000, 0.000000000000000000, -1.000000000000000000 ) ) ;
#55226 = CARTESIAN_POINT ( 'NONE',  ( 14.92337183194729633, 62.67559781766745886, 8.527530157486181039 ) ) ;
#55225 = CARTESIAN_POINT ( 'NONE',  ( -0.8801773607111009756, 18.06368534415484106, 1.068504757029289695E-15 ) ) ;
#55227 = CARTESIAN_POINT ( 'NONE',  ( 14.29541133317241730, 14.76930270348881180, 4.345028136609633052 ) ) ;
#55228 = CARTESIAN_POINT ( 'NONE',  ( 20.36894250292379382, 43.67874883491397497, 10.36894250292379205 ) ) ;
#55229 = CARTESIAN_POINT ( 'NONE',  ( 6.204703633549690345, 52.84541550158062506, 14.16423886937410082 ) ) ;
#55230 = DIRECTION ( 'NONE',  ( 1.000000000000000000, 0.000000000000000000, 0.000000000000000000 ) ) ;
#55231 = CARTESIAN_POINT ( 'NONE',  ( -8.000000000000000000, 79.82179676972448590, 6.500000000000000888 ) ) ;
#55232 = CARTESIAN_POINT ( 'NONE',  ( 12.91533473730993009, 61.60535201082150536, -10.88017736071109987 ) ) ;
#55233 = EDGE_CURVE ( 'NONE', #74265, #37243, #35157, .T. ) ;
#55234 = CARTESIAN_POINT ( 'NONE',  ( 7.361572987183169658, 9.967264484334119601, -9.846743663894592657 ) ) ;
#55235 = CARTESIAN_POINT ( 'NONE',  ( -7.121448108955550360, -73.25984652122872376, 4.000000000000000888 ) ) ;
#55236 = VERTEX_POINT ( 'NONE', #51162 ) ;
#55237 = DIRECTION ( 'NONE',  ( 0.000000000000000000, 0.000000000000000000, 1.000000000000000000 ) ) ;
#55238 = VERTEX_POINT ( 'NONE', #73649 ) ;
#55239 = CARTESIAN_POINT ( 'NONE',  ( 18.52753015748617571, 8.092264484334117824, 4.923371831947298993 ) ) ;
#55240 = ORIENTED_EDGE ( 'NONE', *, *, #22608, .F. ) ;
#55241 = CIRCLE ( 'NONE', #32890, 15.00000000000000000 ) ;
#55242 = CARTESIAN_POINT ( 'NONE',  ( 24.16423886937410614, 24.30374883491396787, 8.672049930838204340E-16 ) ) ;
#55243 = CARTESIAN_POINT ( 'NONE',  ( 7.361572987183169658, 14.96726448433411960, -9.846743663894592657 ) ) ;
#55244 = CARTESIAN_POINT ( 'NONE',  ( -0.8801773607111009756, 48.06368534415484817, 1.068504757029289695E-15 ) ) ;
#55245 = DIRECTION ( 'NONE',  ( -0.000000000000000000, 0.000000000000000000, 1.000000000000000000 ) ) ;
#55246 = ORIENTED_EDGE ( 'NONE', *, *, #76004, .T. ) ;
#55247 = CARTESIAN_POINT ( 'NONE',  ( 10.00000000000000000, 46.81368534415484106, -10.88017736071110342 ) ) ;
#55248 = CARTESIAN_POINT ( 'NONE',  ( -2.962741594153171842, 0.000000000000000000, 13.93860331045670975 ) ) ;
#55249 = CARTESIAN_POINT ( 'NONE',  ( 11.09922568453595026, 1.206968003263759970, 6.408140936763232709 ) ) ;
#55250 = VERTEX_POINT ( 'NONE', #11688 ) ;
#55251 = CARTESIAN_POINT ( 'NONE',  ( 0.5774900079438607392, 43.48035201082151247, 5.440088680355550821 ) ) ;
#55252 = CARTESIAN_POINT ( 'NONE',  ( 20.36894250292379738, 4.928748834913967869, -10.36894250292379027 ) ) ;
#55253 = ORIENTED_EDGE ( 'NONE', *, *, #43319, .F. ) ;
#55254 = VERTEX_POINT ( 'NONE', #44135 ) ;
#55255 = CARTESIAN_POINT ( 'NONE',  ( 22.81628187352647785, 31.41530133659709279, 3.434112377981063169 ) ) ;
#55256 = CARTESIAN_POINT ( 'NONE',  ( -4.164238869374099039, 1.803748834913967647, 8.674139862899312516E-16 ) ) ;
#55257 = CARTESIAN_POINT ( 'NONE',  ( 19.84674366389459266, 13.71726448433411782, -2.638427012816827677 ) ) ;
#55258 = CARTESIAN_POINT ( 'NONE',  ( 13.14228782657339956, 15.00000000000000000, -7.230509711182238064 ) ) ;
#55259 = CARTESIAN_POINT ( 'NONE',  ( 8.879999999999991900, 21.00000000000000000, 2.899999999999999911 ) ) ;
#55260 = CARTESIAN_POINT ( 'NONE',  ( 12.63842701281683922, 14.55059781766744997, -9.846743663894590881 ) ) ;
#55261 = CARTESIAN_POINT ( 'NONE',  ( 20.88017736071110164, 45.35535201082149115, 2.915334737309930979 ) ) ;
#55262 = ADVANCED_FACE ( 'NONE', ( #97671 ), #81646, .T. ) ;
#55263 = AXIS2_PLACEMENT_3D ( 'NONE', #35922, #34432, #80450 ) ;
#55264 = AXIS2_PLACEMENT_3D ( 'NONE', #3856, #47857, #95333 ) ;
#55265 = VERTEX_POINT ( 'NONE', #66659 ) ;
#55266 = CARTESIAN_POINT ( 'NONE',  ( 14.49999999999999822, 11.50000000000000000, -5.000000000000000000 ) ) ;
#55267 = CARTESIAN_POINT ( 'NONE',  ( 20.88017736071110875, 50.77201867748817676, -2.915334737309920765 ) ) ;
#55268 = CARTESIAN_POINT ( 'NONE',  ( 18.29284471827482150, 40.40189080397284016, -6.499999999999946709 ) ) ;
#55269 = VECTOR ( 'NONE', #59793, 1000.000000000000000 ) ;
#55270 = CARTESIAN_POINT ( 'NONE',  ( 0.1532563361054083140, 6.008931151000784787, 1.131784320476157264E-15 ) ) ;
#55271 = CARTESIAN_POINT ( 'NONE',  ( 21.09922568453594849, 11.20696800326375531, 6.408140936763242479 ) ) ;
#55272 = CYLINDRICAL_SURFACE ( 'NONE', #5196, 15.00000000000000000 ) ;
#55273 = B_SPLINE_CURVE_WITH_KNOTS ( 'NONE', 3,
 ( #30284, #60786, #38306, #332 ),
 .UNSPECIFIED., .F., .F.,
 ( 4, 4 ),
 ( 2.710505431213761085E-19, 0.002657014572710960330 ),
 .UNSPECIFIED. ) ;
#55274 = CARTESIAN_POINT ( 'NONE',  ( 1.472469842513823179, 35.59226448433412315, -4.923371831947296329 ) ) ;
#55275 = CARTESIAN_POINT ( 'NONE',  ( 21.09922568453595559, 62.04030133659709634, -6.408140936763230044 ) ) ;
#55276 = CARTESIAN_POINT ( 'NONE',  ( -4.164238869374099927, 7.012082168247302683, 3.795296366450308767 ) ) ;
#55277 = CARTESIAN_POINT ( 'NONE',  ( 1.472469842513823179, 20.59226448433411960, -4.923371831947296329 ) ) ;
#55278 = CARTESIAN_POINT ( 'NONE',  ( 6.565887622018943937, 18.08196800326375708, -12.81628187352647608 ) ) ;
#55280 = CARTESIAN_POINT ( 'NONE',  ( -5.810136766783611684, -36.09274195109910721, -2.750000000000000444 ) ) ;
#55279 = CYLINDRICAL_SURFACE ( 'NONE', #81980, 0.2500000000000002220 ) ;
#55281 = CARTESIAN_POINT ( 'NONE',  ( 19.42250999205614548, 50.98035201082151247, -5.440088680355545492 ) ) ;
#55282 = CARTESIAN_POINT ( 'NONE',  ( 3.591859063236763294, -1.709698663402913210, -11.09922568453595026 ) ) ;
#55283 = DIRECTION ( 'NONE',  ( 0.000000000000000000, -0.000000000000000000, -1.000000000000000000 ) ) ;
#55284 = CARTESIAN_POINT ( 'NONE',  ( 5.076628168052704559, 35.17559781766745175, -8.527530157486179263 ) ) ;
#55285 = CARTESIAN_POINT ( 'NONE',  ( 10.00000000000000000, 19.75893115100078390, -9.846743663894594434 ) ) ;
#55286 = CARTESIAN_POINT ( 'NONE',  ( 17.96484262340118221, 19.93868534415484106, 7.964842623401181321 ) ) ;
#55287 = CARTESIAN_POINT ( 'NONE',  ( 19.38216949554541557, 17.24863466993041783, -9.382169495545420901 ) ) ;
#55288 =( NAMED_UNIT ( * ) PLANE_ANGLE_UNIT ( ) SI_UNIT ( $, .RADIAN. ) );
#55289 = CARTESIAN_POINT ( 'NONE',  ( -9.093709202272499681, 88.10000367580643399, 5.077063215882387404 ) ) ;
#55290 = CARTESIAN_POINT ( 'NONE',  ( -0.8801773607110991993, 17.85535201082150536, -2.915334737309923874 ) ) ;
#55291 = ORIENTED_EDGE ( 'NONE', *, *, #3089, .T. ) ;
#55292 = CARTESIAN_POINT ( 'NONE',  ( -0.8801773607110991993, 67.85535201082151957, -2.915334737309923874 ) ) ;
#55293 = DIRECTION ( 'NONE',  ( -1.000000000000000000, 0.000000000000000000, -0.000000000000000000 ) ) ;
#55295 = CARTESIAN_POINT ( 'NONE',  ( 4.559911319644449179, 17.23035201082150536, -9.422509992056141925 ) ) ;
#55294 = CARTESIAN_POINT ( 'NONE',  ( 19.84674366389459621, 43.50893115100078745, 7.409399052514197653E-17 ) ) ;
#55296 = DIRECTION ( 'NONE',  ( 0.000000000000000000, 1.000000000000000000, 0.000000000000000000 ) ) ;
#55297 = CARTESIAN_POINT ( 'NONE',  ( 12.91533473730993009, 51.60535201082149825, -10.88017736071109987 ) ) ;
#55299 = CARTESIAN_POINT ( 'NONE',  ( -4.431036607602660382, 0.5000000000000004441, 14.33059365769907956 ) ) ;
#55298 = CARTESIAN_POINT ( 'NONE',  ( 0.5774900079438607392, 8.480352010821505360, 5.440088680355550821 ) ) ;
#55300 = CARTESIAN_POINT ( 'NONE',  ( 7.361572987183170547, 17.05059781766745530, 9.846743663894590881 ) ) ;
#55301 = B_SPLINE_CURVE_WITH_KNOTS ( 'NONE', 3,
 ( #62925, #93426, #55930, #47915, #78916, #79417 ),
 .UNSPECIFIED., .F., .F.,
 ( 4, 2, 4 ),
 ( 3.409110551494653465E-05, 0.0004400426677367929684, 0.0008459942299586394564 ),
 .UNSPECIFIED. ) ;
#55302 = CARTESIAN_POINT ( 'NONE',  ( 17.20831665107776587, 32.88393115100078745, 7.208316651077764980 ) ) ;
#55303 = CARTESIAN_POINT ( 'NONE',  ( -5.817157072110618721, 0.5000000000000004441, -13.82608706751094552 ) ) ;
#55304 = CIRCLE ( 'NONE', #71246, 14.49999999999999822 ) ;
#55305 = DIRECTION ( 'NONE',  ( 0.000000000000000000, 0.000000000000000000, 1.000000000000000000 ) ) ;
#55306 = CARTESIAN_POINT ( 'NONE',  ( -0.3689425029237881626, 2.428748834913967869, 10.36894250292379027 ) ) ;
#55307 = ADVANCED_FACE ( 'NONE', ( #43163 ), #87672, .F. ) ;
#55308 = CARTESIAN_POINT ( 'NONE',  ( 2.917880565312948704, 17.63708216824730357, 12.26659068614894643 ) ) ;
#55309 = B_SPLINE_CURVE_WITH_KNOTS ( 'NONE', 3,
 ( #26631, #33628, #11634, #65608, #56648, #19630 ),
 .UNSPECIFIED., .F., .F.,
 ( 4, 2, 4 ),
 ( 3.409110551494649399E-05, 0.0004400426677367923721, 0.0008459942299586382638 ),
 .UNSPECIFIED. ) ;
#55310 = STYLED_ITEM ( 'NONE', ( #41641 ), #41283 ) ;
#55311 = CARTESIAN_POINT ( 'NONE',  ( 0.1532563361054100626, 35.80059781766745175, -2.638427012816831230 ) ) ;
#55312 = DIRECTION ( 'NONE',  ( 0.07845909572785238206, 0.000000000000000000, -0.9969173337331274087 ) ) ;
#55313 = ORIENTED_EDGE ( 'NONE', *, *, #71254, .F. ) ;
#55314 = CARTESIAN_POINT ( 'NONE',  ( -2.266590686148945544, 51.38708216824730357, -7.082119434687050408 ) ) ;
#55315 = ADVANCED_FACE ( 'NONE', ( #19185 ), #13846, .F. ) ;
#55316 = CARTESIAN_POINT ( 'NONE',  ( 19.84674366389459621, 23.50893115100078390, 7.409399052514197653E-17 ) ) ;
#55317 = DIRECTION ( 'NONE',  ( 0.000000000000000000, 1.000000000000000000, 0.000000000000000000 ) ) ;
#55319 = B_SPLINE_CURVE_WITH_KNOTS ( 'NONE', 3,
 ( #79111, #77625, #93621, #48608, #94603, #49105 ),
 .UNSPECIFIED., .F., .F.,
 ( 4, 2, 4 ),
 ( 0.0002800289709862447871, 0.0006862344838250761161, 0.001092439996663907391 ),
 .UNSPECIFIED. ) ;
#55318 = CARTESIAN_POINT ( 'NONE',  ( 10.00000000000000000, 41.81368534415484106, -10.88017736071110342 ) ) ;
#55320 = CARTESIAN_POINT ( 'NONE',  ( 3.591859063236761518, 59.95696800326375353, 11.09922568453594849 ) ) ;
#55321 = CARTESIAN_POINT ( 'NONE',  ( 4.559911319644449179, 22.23035201082150536, -9.422509992056141925 ) ) ;
#55322 = CARTESIAN_POINT ( 'NONE',  ( 3.591859063236761518, 54.95696800326376064, 11.09922568453594849 ) ) ;
#55323 = CARTESIAN_POINT ( 'NONE',  ( 3.591859063236761518, 4.956968003263753531, 11.09922568453594849 ) ) ;
#55324 = CARTESIAN_POINT ( 'NONE',  ( 5.076628168052704559, 15.17559781766745175, -8.527530157486179263 ) ) ;
#55325 = ORIENTED_EDGE ( 'NONE', *, *, #64872, .F. ) ;
#55326 = CARTESIAN_POINT ( 'NONE',  ( -2.815433093577211832, 14.49999999999999112, 14.73340885523754551 ) ) ;
#55327 = CARTESIAN_POINT ( 'NONE',  ( -8.000000000000000000, 0.000000000000000000, 6.250000000000000000 ) ) ;
#55328 = CARTESIAN_POINT ( 'NONE',  ( 17.08211943468705840, 55.13708216824731068, -12.26659068614894466 ) ) ;
#55329 = CARTESIAN_POINT ( 'NONE',  ( 22.26659068614894466, 33.88708216824730357, 7.082119434687054849 ) ) ;
#55330 = CARTESIAN_POINT ( 'NONE',  ( 7.084665262690076126, 22.02201867748817321, -10.88017736071110164 ) ) ;
#55331 = CARTESIAN_POINT ( 'NONE',  ( 2.035157376598822676, 52.43868534415483396, -7.964842623401177768 ) ) ;
#55332 = CARTESIAN_POINT ( 'NONE',  ( -4.000000000000000000, 36.75000000000000000, -2.750000000000000000 ) ) ;
#55333 = DIRECTION ( 'NONE',  ( 0.000000000000000000, 0.000000000000000000, 1.000000000000000000 ) ) ;
#55334 = CARTESIAN_POINT ( 'NONE',  ( -0.8801773607111009756, 68.06368534415484817, 1.068504757029289695E-15 ) ) ;
#55335 = CARTESIAN_POINT ( 'NONE',  ( 14.99999999999998224, 70.25000000000000000, 6.250000000000000000 ) ) ;
#55336 = CARTESIAN_POINT ( 'NONE',  ( 0.1532563361054083140, 16.00893115100078390, 1.131784320476157264E-15 ) ) ;
#55337 = CARTESIAN_POINT ( 'NONE',  ( 5.056330833731659702, 4.503963689120695453E-16, 13.58983143750703348 ) ) ;
#55338 = FACE_OUTER_BOUND ( 'NONE', #68072, .T. ) ;
#55339 = CARTESIAN_POINT ( 'NONE',  ( 5.076628168052703671, 21.84226448433411960, 8.527530157486179263 ) ) ;
#55340 = CARTESIAN_POINT ( 'NONE',  ( 1.472469842513823179, 45.59226448433412315, -4.923371831947296329 ) ) ;
#55341 = EDGE_CURVE ( 'NONE', #45656, #28421, #90479, .T. ) ;
#55342 = CARTESIAN_POINT ( 'NONE',  ( 0.5774900079438590739, 17.64701867748817321, -5.440088680355550821 ) ) ;
#55343 = VECTOR ( 'NONE', #54681, 1000.000000000000000 ) ;
#55344 = UNCERTAINTY_MEASURE_WITH_UNIT (LENGTH_MEASURE( 1.000000000000000082E-05 ), #13017, 'distance_accuracy_value', 'NONE');
#55345 = CARTESIAN_POINT ( 'NONE',  ( 21.09922568453595559, 32.04030133659708923, -6.408140936763230044 ) ) ;
#55346 = CARTESIAN_POINT ( 'NONE',  ( 2.035157376598822676, 47.43868534415484817, -7.964842623401177768 ) ) ;
#55348 = CARTESIAN_POINT ( 'NONE',  ( 7.361572987183170547, 7.050597817667451750, 9.846743663894590881 ) ) ;
#55347 = CARTESIAN_POINT ( 'NONE',  ( 13.79529636645031943, 50.34541550158064638, -14.16423886937409904 ) ) ;
#55349 = PLANE ( 'NONE',  #53383 ) ;
#55350 = PRESENTATION_LAYER_ASSIGNMENT (  '', '', ( #12223 ) ) ;
#55351 = CARTESIAN_POINT ( 'NONE',  ( 12.63842701281683034, 52.46726448433413026, 9.846743663894596210 ) ) ;
#55353 = CARTESIAN_POINT ( 'NONE',  ( 24.16423886937410614, 9.303748834913967869, 8.672049930838204340E-16 ) ) ;
#55352 = CARTESIAN_POINT ( 'NONE',  ( 17.20831665107776587, 29.13393115100078390, -7.208316651077762316 ) ) ;
#55354 = CARTESIAN_POINT ( 'NONE',  ( 20.36894250292379382, 18.67874883491397142, 10.36894250292379205 ) ) ;
#55355 = CARTESIAN_POINT ( 'NONE',  ( 19.84674366389459266, 33.71726448433410894, -2.638427012816827677 ) ) ;
#55356 = CARTESIAN_POINT ( 'NONE',  ( 20.88017736071110875, 45.77201867748816966, -2.915334737309920765 ) ) ;
#55357 = CARTESIAN_POINT ( 'NONE',  ( 4.559911319644449179, 13.89701867748817143, 9.422509992056141925 ) ) ;
#55358 = EDGE_CURVE ( 'NONE', #83368, #29627, #95266, .T. ) ;
#55359 = CARTESIAN_POINT ( 'NONE',  ( 4.559911319644449179, 43.89701867748816966, 9.422509992056141925 ) ) ;
#55360 = CARTESIAN_POINT ( 'NONE',  ( 17.96484262340118221, 24.93868534415484461, 7.964842623401181321 ) ) ;
#55361 = ORIENTED_EDGE ( 'NONE', *, *, #50666, .T. ) ;
#55362 = CARTESIAN_POINT ( 'NONE',  ( 6.565887622018943937, 30.16530133659708568, 12.81628187352647430 ) ) ;
#55363 =( GEOMETRIC_REPRESENTATION_CONTEXT ( 3 ) GLOBAL_UNCERTAINTY_ASSIGNED_CONTEXT ( ( #67132 ) ) GLOBAL_UNIT_ASSIGNED_CONTEXT ( ( #36406, #58904, #58397 ) ) REPRESENTATION_CONTEXT ( 'NONE', 'WORKASPACE' ) );
#55364 = CARTESIAN_POINT ( 'NONE',  ( 2.035157376598822676, 42.43868534415483396, -7.964842623401177768 ) ) ;
#55365 = VERTEX_POINT ( 'NONE', #57667 ) ;
#55366 = CARTESIAN_POINT ( 'NONE',  ( 19.38216949554541202, 60.99863466993042493, 9.382169495545424454 ) ) ;
#55367 = AXIS2_PLACEMENT_3D ( 'NONE', #13737, #73238, #96265 ) ;
#55368 = CARTESIAN_POINT ( 'NONE',  ( 6.869455772997054233, 15.00000000000000000, 14.44603661281844431 ) ) ;
#55369 = ORIENTED_EDGE ( 'NONE', *, *, #74509, .F. ) ;
#55370 = AXIS2_PLACEMENT_3D ( 'NONE', #3640, #72114, #64596 ) ;
#55371 = CARTESIAN_POINT ( 'NONE',  ( 12.91533473730992121, 44.52201867748816966, 10.88017736071110164 ) ) ;
#55372 = CARTESIAN_POINT ( 'NONE',  ( 15.44008868035555260, 4.730352010821504471, 9.422509992056143702 ) ) ;
#55373 = VECTOR ( 'NONE', #88609, 1000.000000000000114 ) ;
#55374 = CARTESIAN_POINT ( 'NONE',  ( 17.39651004071841456, 7.935752660568278216, 6.500000000000003553 ) ) ;
#55375 = CARTESIAN_POINT ( 'NONE',  ( -1.114591949024829054, 4.106534489568945963E-16, -14.45709807627966015 ) ) ;
#55376 = CARTESIAN_POINT ( 'NONE',  ( 20.36894250292379738, 54.92874883491396076, -10.36894250292379027 ) ) ;
#55378 = ORIENTED_EDGE ( 'NONE', *, *, #23068, .F. ) ;
#55377 = CARTESIAN_POINT ( 'NONE',  ( 2.791683348922237240, 10.38393115100078390, -7.208316651077763204 ) ) ;
#55379 = CARTESIAN_POINT ( 'NONE',  ( 6.204703633549690345, 7.845415501580634832, 14.16423886937410082 ) ) ;
#55380 = CARTESIAN_POINT ( 'NONE',  ( 0.1532563361054100626, 0.8005978176674514168, -2.638427012816831230 ) ) ;
#55381 = CARTESIAN_POINT ( 'NONE',  ( 4.559911319644449179, 13.89701867748817143, 9.422509992056141925 ) ) ;
#55382 = CARTESIAN_POINT ( 'NONE',  ( 10.00000000000000178, 42.25893115100078745, 9.846743663894594434 ) ) ;
#55383 = ORIENTED_EDGE ( 'NONE', *, *, #98365, .F. ) ;
#55384 = CARTESIAN_POINT ( 'NONE',  ( 14.92337183194729988, 44.34226448433412315, -8.527530157486177487 ) ) ;
#55385 = CARTESIAN_POINT ( 'NONE',  ( -0.8801773607111008646, 38.27201867748816255, 2.915334737309923430 ) ) ;
#55386 = CARTESIAN_POINT ( 'NONE',  ( 5.076628168052704559, 50.17559781766745886, -8.527530157486179263 ) ) ;
#55387 = CARTESIAN_POINT ( 'NONE',  ( 21.09922568453595559, 32.04030133659708923, -6.408140936763230044 ) ) ;
#55388 = CARTESIAN_POINT ( 'NONE',  ( 7.084665262690076126, 69.10535201082151957, 10.88017736071109987 ) ) ;
#55389 = CARTESIAN_POINT ( 'NONE',  ( 15.44008868035555793, 51.39701867748816966, -9.422509992056140149 ) ) ;
#55390 = CARTESIAN_POINT ( 'NONE',  ( 2.917880565312950480, 60.97041550158063927, -12.26659068614894821 ) ) ;
#55391 = EDGE_CURVE ( 'NONE', #31701, #84883, #12197, .T. ) ;
#55392 = AXIS2_PLACEMENT_3D ( 'NONE', #81090, #5605, #28085 ) ;
#55393 = CARTESIAN_POINT ( 'NONE',  ( 22.81628187352647785, 16.41530133659708923, 3.434112377981063169 ) ) ;
#55394 = DIRECTION ( 'NONE',  ( 0.000000000000000000, 0.000000000000000000, 1.000000000000000000 ) ) ;
#55395 = ORIENTED_EDGE ( 'NONE', *, *, #57228, .T. ) ;
#55396 = CARTESIAN_POINT ( 'NONE',  ( 19.38216949554541557, 32.24863466993041783, -9.382169495545420901 ) ) ;
#55397 = CARTESIAN_POINT ( 'NONE',  ( 4.559911319644449179, 17.23035201082150536, -9.422509992056141925 ) ) ;
#55398 = ORIENTED_EDGE ( 'NONE', *, *, #90328, .T. ) ;
#55399 = ORIENTED_EDGE ( 'NONE', *, *, #82293, .T. ) ;
#55400 = DIRECTION ( 'NONE',  ( 0.000000000000000000, 0.000000000000000000, 1.000000000000000000 ) ) ;
#55401 = CARTESIAN_POINT ( 'NONE',  ( 14.92337183194729633, 2.675597817667451750, 8.527530157486181039 ) ) ;
#55402 = CARTESIAN_POINT ( 'NONE',  ( 19.84674366389459266, 53.71726448433411605, -2.638427012816827677 ) ) ;
#55404 = CARTESIAN_POINT ( 'NONE',  ( 19.84674366389459266, 38.71726448433412315, -2.638427012816827677 ) ) ;
#55403 = CARTESIAN_POINT ( 'NONE',  ( 10.00000000000000178, 17.25893115100078745, 9.846743663894594434 ) ) ;
#55405 = CARTESIAN_POINT ( 'NONE',  ( 0.2751277870542889192, 28.21833443783938122, 6.499999999999990230 ) ) ;
#55406 = FACE_OUTER_BOUND ( 'NONE', #33890, .T. ) ;
#55407 = CARTESIAN_POINT ( 'NONE',  ( 2.518025504887150934, 0.000000000000000000, -4.837081990145593480 ) ) ;
#55409 =( NAMED_UNIT ( * ) SI_UNIT ( $, .STERADIAN. ) SOLID_ANGLE_UNIT ( ) );
#55408 = CARTESIAN_POINT ( 'NONE',  ( 7.361572987183170547, 27.05059781766745175, 9.846743663894590881 ) ) ;
#55411 = ORIENTED_EDGE ( 'NONE', *, *, #65959, .T. ) ;
#55410 = CARTESIAN_POINT ( 'NONE',  ( 5.076628168052703671, 51.84226448433412315, 8.527530157486179263 ) ) ;
#55412 = CIRCLE ( 'NONE', #34619, 0.2500000000000002220 ) ;
#55413 = CARTESIAN_POINT ( 'NONE',  ( -2.816281873526471635, 28.91530133659708213, -3.434112377981056508 ) ) ;
#55414 = DIRECTION ( 'NONE',  ( 0.6246950475544237324, 0.7808688094430306093, 0.000000000000000000 ) ) ;
#55415 = AXIS2_PLACEMENT_3D ( 'NONE', #90694, #76680, #31665 ) ;
#55416 = CARTESIAN_POINT ( 'NONE',  ( 20.36894250292379382, 43.67874883491397497, 10.36894250292379205 ) ) ;
#55417 = CARTESIAN_POINT ( 'NONE',  ( 19.84674366389459621, 13.50893115100078568, 7.409399052514197653E-17 ) ) ;
#55418 =( NAMED_UNIT ( * ) SI_UNIT ( $, .STERADIAN. ) SOLID_ANGLE_UNIT ( ) );
#55419 = CARTESIAN_POINT ( 'NONE',  ( 20.00000000000137845, 93.04550625941708120, 5.196918121118858203 ) ) ;
#55420 = CARTESIAN_POINT ( 'NONE',  ( 22.26659068614895176, 49.72041550158063927, -7.082119434687042414 ) ) ;
#55421 = CARTESIAN_POINT ( 'NONE',  ( 10.00000000000000000, 54.75893115100078745, -9.846743663894594434 ) ) ;
#55422 = CARTESIAN_POINT ( 'NONE',  ( 13.79529636645030344, 63.26208216824730357, 14.16423886937410614 ) ) ;
#55423 = CARTESIAN_POINT ( 'NONE',  ( 10.00000000000000000, 25.55374883491396787, -14.16423886937410082 ) ) ;
#55424 = CARTESIAN_POINT ( 'NONE',  ( 6.204703633549690345, 35.76208216824729647, -14.16423886937410259 ) ) ;
#55425 = CARTESIAN_POINT ( 'NONE',  ( 18.00000000000000000, 84.07179676972448590, -3.750000000000000000 ) ) ;
#55426 = EDGE_CURVE ( 'NONE', #80817, #62008, #9384, .T. ) ;
#55428 = CARTESIAN_POINT ( 'NONE',  ( 18.52753015748618282, 58.92559781766745886, -4.923371831947291888 ) ) ;
#55427 = CARTESIAN_POINT ( 'NONE',  ( -3.115783986955657170, 4.161706264368254368E-16, 14.16128137375395468 ) ) ;
#55429 = VECTOR ( 'NONE', #18919, 1000.000000000000114 ) ;
#55430 = VERTEX_POINT ( 'NONE', #82141 ) ;
#55431 = CARTESIAN_POINT ( 'NONE',  ( 20.88017736071110519, 35.56368534415484106, 2.639326808657452039E-16 ) ) ;
#55432 = CARTESIAN_POINT ( 'NONE',  ( -14.71525861348291819, 14.49999999999999112, -2.908807992686814003 ) ) ;
#55433 = CARTESIAN_POINT ( 'NONE',  ( 14.88232117145530786, 14.49999999999999822, -1.875237731503139438 ) ) ;
#55434 = CARTESIAN_POINT ( 'NONE',  ( 17.20831665107776587, 37.88393115100078745, 7.208316651077764980 ) ) ;
#55436 = CYLINDRICAL_SURFACE ( 'NONE', #9111, 100.0000000000000000 ) ;
#55435 = AXIS2_PLACEMENT_3D ( 'NONE', #45068, #30059, #75576 ) ;
#55437 = CARTESIAN_POINT ( 'NONE',  ( 12.26659068614894821, -6.112917831752690212, 7.082119434687044190 ) ) ;
#55438 = CIRCLE ( 'NONE', #76133, 14.49999999999999822 ) ;
#55439 = CARTESIAN_POINT ( 'NONE',  ( 18.52753015748618282, 48.92559781766745886, -4.923371831947291888 ) ) ;
#55440 = CARTESIAN_POINT ( 'NONE',  ( -3.750000000000000000, 9.750000000000000000, -3.750000000000000000 ) ) ;
#55441 = ADVANCED_FACE ( 'NONE', ( #65163 ), #50671, .F. ) ;
#55442 = ORIENTED_EDGE ( 'NONE', *, *, #56566, .T. ) ;
#55443 = CARTESIAN_POINT ( 'NONE',  ( 20.36894250292379738, 19.92874883491396787, -10.36894250292379027 ) ) ;
#55444 = EDGE_CURVE ( 'NONE', #72583, #88979, #12664, .T. ) ;
#55445 = EDGE_CURVE ( 'NONE', #43424, #72059, #65656, .T. ) ;
#55446 = DIRECTION ( 'NONE',  ( 1.000000000000000000, 0.000000000000000000, 0.000000000000000000 ) ) ;
#55448 = CYLINDRICAL_SURFACE ( 'NONE', #50288, 0.5000000000000004441 ) ;
#55447 = CARTESIAN_POINT ( 'NONE',  ( -0.1042174387088628529, 68.10736173766203194, 6.337391062633416894 ) ) ;
#55449 = CARTESIAN_POINT ( 'NONE',  ( -0.3689425029237881626, 67.42874883491396076, 10.36894250292379027 ) ) ;
#55450 = CARTESIAN_POINT ( 'NONE',  ( 22.81628187352647785, 26.62363466993042138, 6.195893100308588602E-16 ) ) ;
#55451 = DIRECTION ( 'NONE',  ( 0.000000000000000000, 1.000000000000000000, 0.000000000000000000 ) ) ;
#55452 = CARTESIAN_POINT ( 'NONE',  ( 19.42250999205614193, 65.14701867748817676, 5.440088680355555262 ) ) ;
#55453 = CARTESIAN_POINT ( 'NONE',  ( 21.92686044187656336, 41.97997603579416648, 3.195792623639536423 ) ) ;
#55454 = CARTESIAN_POINT ( 'NONE',  ( 4.219999999999999751, 10.00000000000000000, 2.500000000000000000 ) ) ;
#55455 = DIRECTION ( 'NONE',  ( -2.107602052970794797E-16, 1.000000000000000000, 0.000000000000000000 ) ) ;
#55456 = CARTESIAN_POINT ( 'NONE',  ( 10.00000000000000000, 65.55374883491396076, -14.16423886937410082 ) ) ;
#55457 = DIRECTION ( 'NONE',  ( 0.000000000000000000, 1.000000000000000000, -0.000000000000000000 ) ) ;
#55458 = CARTESIAN_POINT ( 'NONE',  ( 4.559911319644449179, 27.23035201082150536, -9.422509992056141925 ) ) ;
#55459 = CARTESIAN_POINT ( 'NONE',  ( 12.91533473730993009, 31.60535201082150891, -10.88017736071109987 ) ) ;
#55460 = CARTESIAN_POINT ( 'NONE',  ( 21.09922568453594849, 1.206968003263753531, 6.408140936763242479 ) ) ;
#55461 = CARTESIAN_POINT ( 'NONE',  ( 17.20831665107776587, 54.13393115100079456, -7.208316651077762316 ) ) ;
#55462 = CARTESIAN_POINT ( 'NONE',  ( -42.16485527613927076, 107.5383484153110061, -5.000000000000000888 ) ) ;
#55463 = CARTESIAN_POINT ( 'NONE',  ( 4.629999999999990123, 76.07179676972444327, -4.250000000000000000 ) ) ;
#55464 = VERTEX_POINT ( 'NONE', #58150 ) ;
#55465 = ADVANCED_FACE ( 'NONE', ( #6156 ), #93073, .T. ) ;
#55466 = CARTESIAN_POINT ( 'NONE',  ( 2.035157376598824452, 33.68868534415484106, 7.964842623401179544 ) ) ;
#55467 = CARTESIAN_POINT ( 'NONE',  ( 6.565887622018943937, 28.08196800326375353, -12.81628187352647608 ) ) ;
#55468 = CARTESIAN_POINT ( 'NONE',  ( 0.000000000000000000, 75.98134920320651986, 6.799195827237609180 ) ) ;
#55469 = CARTESIAN_POINT ( 'NONE',  ( 14.92337183194729633, 57.67559781766745886, 8.527530157486181039 ) ) ;
#55470 = CARTESIAN_POINT ( 'NONE',  ( 20.88017736071110164, 45.35535201082149115, 2.915334737309930979 ) ) ;
#55471 = CARTESIAN_POINT ( 'NONE',  ( 0.1532563361054082862, 11.21726448433411605, 2.638427012816831674 ) ) ;
#55472 = VECTOR ( 'NONE', #89886, 1000.000000000000227 ) ;
#55473 = CARTESIAN_POINT ( 'NONE',  ( -1.099225684535947600, 39.54030133659708923, 6.408140936763237150 ) ) ;
#55475 = FACE_OUTER_BOUND ( 'NONE', #87188, .T. ) ;
#55474 = CARTESIAN_POINT ( 'NONE',  ( 19.42250999205614193, 65.14701867748817676, 5.440088680355555262 ) ) ;
#55476 = CARTESIAN_POINT ( 'NONE',  ( 17.62281668512001076, 53.28593319516823357, 6.500000000000063061 ) ) ;
#55477 = CARTESIAN_POINT ( 'NONE',  ( -2.816281873526473856, 64.33196800326376774, 3.434112377981055619 ) ) ;
#55478 = ORIENTED_EDGE ( 'NONE', *, *, #96068, .F. ) ;
#55479 = DIRECTION ( 'NONE',  ( 0.9848077530122086864, 0.1736481776669272503, -0.000000000000000000 ) ) ;
#55480 = DIRECTION ( 'NONE',  ( 0.000000000000000000, 1.000000000000000000, 0.000000000000000000 ) ) ;
#55481 = CARTESIAN_POINT ( 'NONE',  ( 0.5774900079438590739, 7.647018677488171434, -5.440088680355550821 ) ) ;
#55483 = CARTESIAN_POINT ( 'NONE',  ( 22.26659068614894466, 13.88708216824730179, 7.082119434687054849 ) ) ;
#55482 = CARTESIAN_POINT ( 'NONE',  ( 21.09922568453595559, 42.04030133659708213, -6.408140936763230044 ) ) ;
#55484 = ADVANCED_FACE ( 'NONE', ( #62603 ), #93660, .T. ) ;
#55485 = CARTESIAN_POINT ( 'NONE',  ( 17.20831665107776587, 12.88393115100078390, 7.208316651077764980 ) ) ;
#55486 = CARTESIAN_POINT ( 'NONE',  ( 4.559911319644449179, 2.230352010821504471, -9.422509992056141925 ) ) ;
#55487 = CARTESIAN_POINT ( 'NONE',  ( 5.076628168052703671, 21.84226448433411960, 8.527530157486179263 ) ) ;
#55488 = CARTESIAN_POINT ( 'NONE',  ( 17.08211943468705130, 58.47041550158063927, 12.26659068614894998 ) ) ;
#55489 = ORIENTED_EDGE ( 'NONE', *, *, #86497, .F. ) ;
#55490 = SURFACE_STYLE_FILL_AREA ( #32966 ) ;
#55491 = CARTESIAN_POINT ( 'NONE',  ( -0.8801773607111009756, 23.06368534415484106, 1.068504757029289695E-15 ) ) ;
#55492 = CARTESIAN_POINT ( 'NONE',  ( 14.40939250469966026, 4.578996266948430760E-16, -1.618458416365756714 ) ) ;
#55493 =( BOUNDED_CURVE ( )  B_SPLINE_CURVE ( 2, ( #10713, #50678, #26207, #20174, #34673, #56221, #12178, #11196, #73163, #57182, #71708, #88171, #94702 ),
 .UNSPECIFIED., .F., .F. ) 
 B_SPLINE_CURVE_WITH_KNOTS ( ( 3, 2, 2, 2, 2, 2, 3 ),
 ( 0.6333333333333333037, 0.6388888888888888395, 0.6444444444444444864, 0.6500000000000000222, 0.6555555555555555580, 0.6611111111111110938, 0.6666666666666666297 ),
 .UNSPECIFIED. ) 
 CURVE ( )  GEOMETRIC_REPRESENTATION_ITEM ( )  RATIONAL_B_SPLINE_CURVE ( ( 1.000000000000000000, 0.9659258262890683122, 1.000000000000000000, 0.9659258262890683122, 1.000000000000000000, 0.9659258262890683122, 1.000000000000000000, 0.9659258262890683122, 1.000000000000000000, 0.9659258262890683122, 1.000000000000000000, 0.9659258262890683122, 1.000000000000000000 ) ) 
 REPRESENTATION_ITEM ( '' )  );
#55494 = ORIENTED_EDGE ( 'NONE', *, *, #67989, .F. ) ;
#55495 = ORIENTED_EDGE ( 'NONE', *, *, #23445, .F. ) ;
#55496 = CARTESIAN_POINT ( 'NONE',  ( 4.559911319644449179, 17.23035201082150536, -9.422509992056141925 ) ) ;
#55497 = CARTESIAN_POINT ( 'NONE',  ( 2.035157376598822676, 12.43868534415483751, -7.964842623401177768 ) ) ;
#55498 = CARTESIAN_POINT ( 'NONE',  ( 7.361572987183169658, 59.96726448433410894, -9.846743663894592657 ) ) ;
#55499 = CARTESIAN_POINT ( 'NONE',  ( 13.43411237798106583, 52.66530133659708213, -12.81628187352647252 ) ) ;
#55500 = CARTESIAN_POINT ( 'NONE',  ( -13.61464873478171889, 0.3640475087720990710, 6.296136897217741613 ) ) ;
#55502 = CARTESIAN_POINT ( 'NONE',  ( 22.26659068614895176, 14.72041550158063572, -7.082119434687042414 ) ) ;
#55501 = CARTESIAN_POINT ( 'NONE',  ( -6.000000000000014211, 80.07179676972448590, -6.250000000000000000 ) ) ;
#55503 = CARTESIAN_POINT ( 'NONE',  ( 19.42250999205614193, 20.14701867748817321, 5.440088680355555262 ) ) ;
#55504 = CARTESIAN_POINT ( 'NONE',  ( 2.035157376598824452, 23.68868534415484461, 7.964842623401179544 ) ) ;
#55505 = CARTESIAN_POINT ( 'NONE',  ( 7.361572987183169658, 49.96726448433410894, -9.846743663894592657 ) ) ;
#55506 = FILL_AREA_STYLE_COLOUR ( '', #20535 ) ;
#55507 = CARTESIAN_POINT ( 'NONE',  ( 5.076628168052704559, 35.17559781766745175, -8.527530157486179263 ) ) ;
#55508 = CARTESIAN_POINT ( 'NONE',  ( 14.92337183194729988, 4.342264484334117824, -8.527530157486177487 ) ) ;
#55509 = CARTESIAN_POINT ( 'NONE',  ( 2.638427012816829897, 24.55059781766745530, -9.846743663894592657 ) ) ;
#55510 = VECTOR ( 'NONE', #21187, 1000.000000000000000 ) ;
#55511 = ORIENTED_EDGE ( 'NONE', *, *, #14233, .T. ) ;
#55512 = CARTESIAN_POINT ( 'NONE',  ( -6.767445849361073407, 14.49999999999999112, -13.38662304974512729 ) ) ;
#55513 = CARTESIAN_POINT ( 'NONE',  ( 7.361572987183169658, 14.96726448433411960, -9.846743663894592657 ) ) ;
#55514 = CARTESIAN_POINT ( 'NONE',  ( 3.591859063236761518, -0.04303199673624671928, 11.09922568453594849 ) ) ;
#55515 = CARTESIAN_POINT ( 'NONE',  ( 0.5774900079438590739, 52.64701867748817676, -5.440088680355550821 ) ) ;
#55517 = CARTESIAN_POINT ( 'NONE',  ( 3.591859063236763294, 43.29030133659708923, -11.09922568453595026 ) ) ;
#55516 = CARTESIAN_POINT ( 'NONE',  ( 19.42250999205614548, 5.980352010821504471, -5.440088680355545492 ) ) ;
#55518 = CARTESIAN_POINT ( 'NONE',  ( 6.204703633549690345, 15.76208216824730179, -14.16423886937410259 ) ) ;
#55519 = AXIS2_PLACEMENT_3D ( 'NONE', #2921, #47891, #93892 ) ;
#55520 = CIRCLE ( 'NONE', #12387, 15.00000000000000000 ) ;
#55521 = CARTESIAN_POINT ( 'NONE',  ( 6.565887622018943937, 65.16530133659709634, 12.81628187352647430 ) ) ;
#55522 = ORIENTED_EDGE ( 'NONE', *, *, #30160, .T. ) ;
#55523 = CARTESIAN_POINT ( 'NONE',  ( 14.92337183194729633, 52.67559781766745175, 8.527530157486181039 ) ) ;
#55524 = CARTESIAN_POINT ( 'NONE',  ( 4.559911319644449179, 22.23035201082150536, -9.422509992056141925 ) ) ;
#55525 = ORIENTED_EDGE ( 'NONE', *, *, #16662, .T. ) ;
#55526 = CARTESIAN_POINT ( 'NONE',  ( 7.361572987183170547, 2.050597817667451750, 9.846743663894590881 ) ) ;
#55527 = CARTESIAN_POINT ( 'NONE',  ( 20.88017736071110164, 65.35535201082150536, 2.915334737309930979 ) ) ;
#55529 = EDGE_CURVE ( 'NONE', #1670, #1168, #2673, .T. ) ;
#55528 = DIRECTION ( 'NONE',  ( 0.000000000000000000, 0.000000000000000000, 1.000000000000000000 ) ) ;
#55530 = CARTESIAN_POINT ( 'NONE',  ( 12.63842701281683922, 4.550597817667451750, -9.846743663894590881 ) ) ;
#55531 = CARTESIAN_POINT ( 'NONE',  ( 12.63842701281683034, 2.467264484334118269, 9.846743663894596210 ) ) ;
#55532 = SURFACE_STYLE_USAGE ( .BOTH. , #56026 ) ;
#55533 = ADVANCED_FACE ( 'NONE', ( #24166 ), #71985, .F. ) ;
#55535 = CARTESIAN_POINT ( 'NONE',  ( -5.419894505350392855, 0.5000000000000004441, -13.98659156302466045 ) ) ;
#55534 = CARTESIAN_POINT ( 'NONE',  ( 12.91533473730992121, 59.52201867748816966, 10.88017736071110164 ) ) ;
#55536 = CARTESIAN_POINT ( 'NONE',  ( -0.8801773607111009756, 63.06368534415484106, 1.068504757029289695E-15 ) ) ;
#55538 = ORIENTED_EDGE ( 'NONE', *, *, #26548, .T. ) ;
#55537 = CARTESIAN_POINT ( 'NONE',  ( 2.791683348922237240, 5.383931151000785675, -7.208316651077763204 ) ) ;
#55539 = DIRECTION ( 'NONE',  ( -1.000000000000000000, 0.000000000000000000, 0.000000000000000000 ) ) ;
#55540 = CARTESIAN_POINT ( 'NONE',  ( 19.84674366389459266, 53.30059781766744464, 2.638427012816836559 ) ) ;
#55541 = ORIENTED_EDGE ( 'NONE', *, *, #31881, .F. ) ;
#55542 = PLANE ( 'NONE',  #26657 ) ;
#55543 = CARTESIAN_POINT ( 'NONE',  ( -4.164238869374099927, 2.012082168247300906, 3.795296366450308767 ) ) ;
#55544 = CARTESIAN_POINT ( 'NONE',  ( 3.591859063236763294, 53.29030133659708923, -11.09922568453595026 ) ) ;
#55545 = CARTESIAN_POINT ( 'NONE',  ( 17.08211943468705840, 5.137082168247300906, -12.26659068614894466 ) ) ;
#55546 = CARTESIAN_POINT ( 'NONE',  ( 24.16423886937410614, 14.30374883491396787, 8.672049930838204340E-16 ) ) ;
#55547 = CARTESIAN_POINT ( 'NONE',  ( 14.03351048042397231, 15.00000000000000000, -2.474486531753715024 ) ) ;
#55548 = FACE_OUTER_BOUND ( 'NONE', #58272, .T. ) ;
#55549 = CARTESIAN_POINT ( 'NONE',  ( 2.035157376598824452, 18.68868534415484106, 7.964842623401179544 ) ) ;
#55550 = DIRECTION ( 'NONE',  ( 1.000000000000000000, 0.000000000000000000, 0.000000000000000000 ) ) ;
#55551 = ORIENTED_EDGE ( 'NONE', *, *, #91196, .F. ) ;
#55552 = CARTESIAN_POINT ( 'NONE',  ( 5.076628168052703671, 21.84226448433411960, 8.527530157486179263 ) ) ;
#55553 = CARTESIAN_POINT ( 'NONE',  ( 16.40814093676323893, 35.79030133659708923, 11.09922568453595026 ) ) ;
#55554 = CARTESIAN_POINT ( 'NONE',  ( 10.00000000000000178, 42.25893115100078745, 9.846743663894594434 ) ) ;
#55555 = CARTESIAN_POINT ( 'NONE',  ( 19.84674366389459621, 58.50893115100078745, 7.409399052514197653E-17 ) ) ;
#55556 = CARTESIAN_POINT ( 'NONE',  ( 3.591859063236763294, 18.29030133659708568, -11.09922568453595026 ) ) ;
#55557 = CARTESIAN_POINT ( 'NONE',  ( -19.64999999999999858, 98.99999999999998579, 8.000000000000000000 ) ) ;
#55558 = VECTOR ( 'NONE', #79090, 1000.000000000000000 ) ;
#55559 = CARTESIAN_POINT ( 'NONE',  ( 1.472469842513823179, 26.42559781766745175, 4.923371831947296329 ) ) ;
#55560 = EDGE_CURVE ( 'NONE', #538, #37093, #79290, .T. ) ;
#55561 = CARTESIAN_POINT ( 'NONE',  ( 12.63842701281683034, 2.467264484334118269, 9.846743663894596210 ) ) ;
#55562 = ORIENTED_EDGE ( 'NONE', *, *, #82839, .T. ) ;
#55563 = EDGE_LOOP ( 'NONE', ( #18155, #16165, #88434, #70899 ) ) ;
#55564 = EDGE_CURVE ( 'NONE', #74650, #67193, #9150, .T. ) ;
#55565 = CARTESIAN_POINT ( 'NONE',  ( 10.00000000000000000, 36.81368534415484106, -10.88017736071110342 ) ) ;
#55566 = CARTESIAN_POINT ( 'NONE',  ( 6.204703633549690345, 32.84541550158063927, 14.16423886937410082 ) ) ;
#55567 = CARTESIAN_POINT ( 'NONE',  ( 5.076628168052704559, 45.17559781766745175, -8.527530157486179263 ) ) ;
#55568 = CARTESIAN_POINT ( 'NONE',  ( 19.84674366389459266, 18.71726448433411960, -2.638427012816827677 ) ) ;
#55570 = CARTESIAN_POINT ( 'NONE',  ( -7.750355510519348456, 84.07179676972448590, 4.000000000000000000 ) ) ;
#55569 = CARTESIAN_POINT ( 'NONE',  ( 22.81628187352647785, 51.41530133659708923, 3.434112377981063169 ) ) ;
#55571 = CARTESIAN_POINT ( 'NONE',  ( 10.00000000000000178, 29.31368534415483751, 10.88017736071110342 ) ) ;
#55572 = CARTESIAN_POINT ( 'NONE',  ( 17.99999999999999645, 99.99999999999998579, -8.000000000000000000 ) ) ;
#55573 = TOROIDAL_SURFACE ( 'NONE', #39668, 1.000000000000000000, 0.5000000000000000000 ) ;
#55574 = CARTESIAN_POINT ( 'NONE',  ( -1.099225684535947600, 24.54030133659708923, 6.408140936763237150 ) ) ;
#55575 = CARTESIAN_POINT ( 'NONE',  ( 18.52753015748618282, 38.92559781766745175, -4.923371831947291888 ) ) ;
#55576 = CARTESIAN_POINT ( 'NONE',  ( -5.440088680355547268, -1.102981322511818796, 9.422509992056143702 ) ) ;
#55577 = CARTESIAN_POINT ( 'NONE',  ( 21.09922568453595559, 47.04030133659708923, -6.408140936763230044 ) ) ;
#55578 = CARTESIAN_POINT ( 'NONE',  ( 4.841283923550437684, 14.76930270348882068, -14.13506365971146117 ) ) ;
#55580 = CARTESIAN_POINT ( 'NONE',  ( 19.72487221294570858, 9.782175860852373006, 6.500000000000000000 ) ) ;
#55579 = CARTESIAN_POINT ( 'NONE',  ( -0.8801773607111008646, 58.27201867748816966, 2.915334737309923430 ) ) ;
#55581 = AXIS2_PLACEMENT_3D ( 'NONE', #93173, #12512, #35506 ) ;
#55582 = DIRECTION ( 'NONE',  ( 0.000000000000000000, 1.000000000000000000, 0.000000000000000000 ) ) ;
#55583 = FACE_OUTER_BOUND ( 'NONE', #20706, .T. ) ;
#55584 = AXIS2_PLACEMENT_3D ( 'NONE', #92258, #77244, #8751 ) ;
#55585 = CARTESIAN_POINT ( 'NONE',  ( 20.88017736071110519, 55.56368534415484817, 2.639326808657452039E-16 ) ) ;
#55586 = CARTESIAN_POINT ( 'NONE',  ( 10.00000000000000000, 56.81368534415484106, -10.88017736071110342 ) ) ;
#55587 = CARTESIAN_POINT ( 'NONE',  ( 19.88701968852527102, 56.79427333184086280, 6.480634945678608538 ) ) ;
#55588 = CARTESIAN_POINT ( 'NONE',  ( 5.963430220938287007, 11.35497603579418247, 10.32896413005679825 ) ) ;
#55589 = EDGE_CURVE ( 'NONE', #44200, #95213, #55129, .T. ) ;
#55590 = CARTESIAN_POINT ( 'NONE',  ( 10.00000000000000000, 11.81368534415483751, -10.88017736071110342 ) ) ;
#55591 = CARTESIAN_POINT ( 'NONE',  ( 19.84674366389459266, 58.71726448433411605, -2.638427012816827677 ) ) ;
#55593 = DIRECTION ( 'NONE',  ( -1.000000000000000000, 0.000000000000000000, 0.000000000000000000 ) ) ;
#55592 = CARTESIAN_POINT ( 'NONE',  ( 19.42250999205614548, 25.98035201082150891, -5.440088680355545492 ) ) ;
#55594 = CARTESIAN_POINT ( 'NONE',  ( 16.40814093676324603, 27.45696800326375708, -11.09922568453594671 ) ) ;
#55595 = ORIENTED_EDGE ( 'NONE', *, *, #12529, .T. ) ;
#55596 = CARTESIAN_POINT ( 'NONE',  ( 2.035157376598822676, 57.43868534415484106, -7.964842623401177768 ) ) ;
#55597 = CARTESIAN_POINT ( 'NONE',  ( 19.84674366389459621, 38.50893115100078745, 7.409399052514197653E-17 ) ) ;
#55599 = DIRECTION ( 'NONE',  ( 1.000000000000000000, -3.469446951953623261E-15, -0.000000000000000000 ) ) ;
#55598 = CARTESIAN_POINT ( 'NONE',  ( -2.816281873526473856, 9.123634669930421381, 9.499525473075851096E-16 ) ) ;
#55600 = EDGE_CURVE ( 'NONE', #25279, #87966, #25005, .T. ) ;
#55601 = CARTESIAN_POINT ( 'NONE',  ( 2.035157376598822676, 12.43868534415483751, -7.964842623401177768 ) ) ;
#55602 = CARTESIAN_POINT ( 'NONE',  ( -0.8801773607111009756, 38.06368534415484106, 1.068504757029289695E-15 ) ) ;
#55603 = CARTESIAN_POINT ( 'NONE',  ( -2.266590686148945544, 56.38708216824731068, -7.082119434687050408 ) ) ;
#55604 = CARTESIAN_POINT ( 'NONE',  ( 12.63842701281683922, 39.55059781766744464, -9.846743663894590881 ) ) ;
#55605 = CARTESIAN_POINT ( 'NONE',  ( 20.88017736071110519, 55.56368534415484817, 2.639326808657452039E-16 ) ) ;
#55606 = LINE ( 'NONE', #95565, #13908 ) ;
#55607 = CARTESIAN_POINT ( 'NONE',  ( 17.08211943468705840, 15.13708216824730179, -12.26659068614894466 ) ) ;
#55608 = CARTESIAN_POINT ( 'NONE',  ( 0.000000000000000000, 14.49999999999999822, 0.000000000000000000 ) ) ;
#55609 = CARTESIAN_POINT ( 'NONE',  ( 19.72487221294570858, 11.86607318730075633, 6.500000000000000888 ) ) ;
#55610 = ORIENTED_EDGE ( 'NONE', *, *, #1199, .T. ) ;
#55611 = CARTESIAN_POINT ( 'NONE',  ( 10.00000000000000178, 53.05374883491396787, 14.16423886937410082 ) ) ;
#55612 = CARTESIAN_POINT ( 'NONE',  ( 10.00000000000000178, 33.05374883491396787, 14.16423886937410082 ) ) ;
#55613 = CARTESIAN_POINT ( 'NONE',  ( 19.84674366389459266, 18.30059781766745175, 2.638427012816836559 ) ) ;
#55614 = CARTESIAN_POINT ( 'NONE',  ( 0.6178305044545818747, 13.49863466993041783, -9.382169495545419124 ) ) ;
#55615 = CARTESIAN_POINT ( 'NONE',  ( 0.1532563361054100626, 60.80059781766744464, -2.638427012816831230 ) ) ;
#55616 = CARTESIAN_POINT ( 'NONE',  ( 0.000000000000000000, 0.000000000000000000, 5.000000000000000000 ) ) ;
#55618 = CARTESIAN_POINT ( 'NONE',  ( 6.565887622018943937, 33.08196800326374643, -12.81628187352647608 ) ) ;
#55617 = CARTESIAN_POINT ( 'NONE',  ( 12.91533473730992121, 59.52201867748816966, 10.88017736071110164 ) ) ;
#55619 = CARTESIAN_POINT ( 'NONE',  ( 20.36894250292379738, 24.92874883491396787, -10.36894250292379027 ) ) ;
#55620 = CARTESIAN_POINT ( 'NONE',  ( 2.035157376598824452, 28.68868534415484106, 7.964842623401179544 ) ) ;
#55621 = CARTESIAN_POINT ( 'NONE',  ( 6.000000000000000000, 60.50000000000000711, 6.500000000000000888 ) ) ;
#55622 = CARTESIAN_POINT ( 'NONE',  ( 17.20831665107776587, 2.883931151000785231, 7.208316651077764980 ) ) ;
#55623 = CARTESIAN_POINT ( 'NONE',  ( -2.638427012816824124, -12.94940218233254470, 9.846743663894596210 ) ) ;
#55624 = ORIENTED_EDGE ( 'NONE', *, *, #62283, .F. ) ;
#55625 = LINE ( 'NONE', #2651, #12594 ) ;
#55626 = ORIENTED_EDGE ( 'NONE', *, *, #53039, .T. ) ;
#55627 =( NAMED_UNIT ( * ) SI_UNIT ( $, .STERADIAN. ) SOLID_ANGLE_UNIT ( ) );
#55629 = CARTESIAN_POINT ( 'NONE',  ( -0.8801773607111008646, 18.27201867748817321, 2.915334737309923430 ) ) ;
#55628 = CARTESIAN_POINT ( 'NONE',  ( 4.559911319644449179, 3.897018677488171434, 9.422509992056141925 ) ) ;
#55631 = CARTESIAN_POINT ( 'NONE',  ( 3.591859063236763294, -1.709698663402913210, -11.09922568453595026 ) ) ;
#55630 = CARTESIAN_POINT ( 'NONE',  ( 19.84674366389459266, 33.71726448433410894, -2.638427012816827677 ) ) ;
#55632 = CARTESIAN_POINT ( 'NONE',  ( -6.869455772996959197, -0.03417435944610275333, -14.44603661281848517 ) ) ;
#55633 = CARTESIAN_POINT ( 'NONE',  ( -10.53011945866294852, -98.59345040283277228, 4.000000000000000000 ) ) ;
#55634 = CARTESIAN_POINT ( 'NONE',  ( 0.6178305044545838731, 9.748634669930416052, 9.382169495545420901 ) ) ;
#55635 = CARTESIAN_POINT ( 'NONE',  ( -3.434112377981047626, 30.16530133659709989, 12.81628187352647963 ) ) ;
#55636 = ORIENTED_EDGE ( 'NONE', *, *, #22255, .T. ) ;
#55637 = CARTESIAN_POINT ( 'NONE',  ( 24.16423886937409904, 49.09541550158063217, 3.795296366450317205 ) ) ;
#55638 = VERTEX_POINT ( 'NONE', #11484 ) ;
#55639 = CARTESIAN_POINT ( 'NONE',  ( 20.36894250292379382, 53.67874883491397497, 10.36894250292379205 ) ) ;
#55640 = VERTEX_POINT ( 'NONE', #19482 ) ;
#55641 = CARTESIAN_POINT ( 'NONE',  ( 19.42250999205614193, 30.14701867748817321, 5.440088680355555262 ) ) ;
#55642 = STYLED_ITEM ( 'NONE', ( #18607 ), #12884 ) ;
#55643 = CARTESIAN_POINT ( 'NONE',  ( 10.00000000000000178, 44.31368534415484106, 10.88017736071110342 ) ) ;
#55644 = CARTESIAN_POINT ( 'NONE',  ( 0.5774900079438607392, 33.48035201082150536, 5.440088680355550821 ) ) ;
#55645 = CARTESIAN_POINT ( 'NONE',  ( 10.00000000000000000, 66.81368534415484817, -10.88017736071110342 ) ) ;
#55646 = CARTESIAN_POINT ( 'NONE',  ( 15.44008868035555260, 24.73035201082150891, 9.422509992056143702 ) ) ;
#55647 = B_SPLINE_CURVE_WITH_KNOTS ( 'NONE', 3,
 ( #75911, #23911, #16403, #83417, #7436, #76889 ),
 .UNSPECIFIED., .F., .F.,
 ( 4, 2, 4 ),
 ( 0.0002800154274984825720, 0.0006862208078247651697, 0.001092426188151047767 ),
 .UNSPECIFIED. ) ;
#55648 = EDGE_CURVE ( 'NONE', #86906, #25488, #95485, .T. ) ;
#55649 = AXIS2_PLACEMENT_3D ( 'NONE', #8262, #782, #14292 ) ;
#55650 = VECTOR ( 'NONE', #67927, 1000.000000000000114 ) ;
#55652 = ORIENTED_EDGE ( 'NONE', *, *, #12326, .T. ) ;
#55651 = DIRECTION ( 'NONE',  ( 0.8703556959398941473, 0.000000000000000000, 0.4924235601034769316 ) ) ;
#55653 = CARTESIAN_POINT ( 'NONE',  ( 5.076628168052704559, 15.17559781766745175, -8.527530157486179263 ) ) ;
#55654 = CARTESIAN_POINT ( 'NONE',  ( -4.535014064427665303, -17.52590857053631623, 2.500000000000806910 ) ) ;
#55655 = VERTEX_POINT ( 'NONE', #3509 ) ;
#55656 =( LENGTH_UNIT ( ) NAMED_UNIT ( * ) SI_UNIT ( .MILLI., .METRE. ) );
#55657 = CARTESIAN_POINT ( 'NONE',  ( 17.20831665107776587, 44.13393115100078745, -7.208316651077762316 ) ) ;
#55658 = CARTESIAN_POINT ( 'NONE',  ( 0.000000000000000000, 14.49999999999999822, 0.000000000000000000 ) ) ;
#55659 =( NAMED_UNIT ( * ) PLANE_ANGLE_UNIT ( ) SI_UNIT ( $, .RADIAN. ) );
#55660 = CARTESIAN_POINT ( 'NONE',  ( 0.000000000000000000, 0.000000000000000000, -9.500000000000000000 ) ) ;
#55661 = LINE ( 'NONE', #18156, #89097 ) ;
#55662 = LINE ( 'NONE', #86161, #58614 ) ;
#55663 = CARTESIAN_POINT ( 'NONE',  ( 0.1532563361054083140, 56.00893115100078745, 1.131784320476157264E-15 ) ) ;
#55664 = CARTESIAN_POINT ( 'NONE',  ( 10.00000000000000000, 45.55374883491397497, -14.16423886937410082 ) ) ;
#55665 = DIRECTION ( 'NONE',  ( 0.000000000000000000, 0.000000000000000000, -1.000000000000000000 ) ) ;
#55666 = ORIENTED_EDGE ( 'NONE', *, *, #52621, .F. ) ;
#55667 = CARTESIAN_POINT ( 'NONE',  ( 19.88701968852526392, 41.79427333184086280, 6.480634945678624526 ) ) ;
#55668 = CARTESIAN_POINT ( 'NONE',  ( 5.076628168052703671, 21.84226448433411960, 8.527530157486179263 ) ) ;
#55669 = CARTESIAN_POINT ( 'NONE',  ( 21.09922568453595559, 52.04030133659708923, -6.408140936763230044 ) ) ;
#55670 = CARTESIAN_POINT ( 'NONE',  ( 5.076628168052704559, 55.17559781766745175, -8.527530157486179263 ) ) ;
#55671 = CARTESIAN_POINT ( 'NONE',  ( 7.084665262690076126, 64.10535201082150536, 10.88017736071109987 ) ) ;
#55672 = CARTESIAN_POINT ( 'NONE',  ( 2.791683348922237240, 50.38393115100078035, -7.208316651077763204 ) ) ;
#55673 = CARTESIAN_POINT ( 'NONE',  ( 20.24186590665277663, 14.73410085661203972, 6.114288769123037426 ) ) ;
#55674 = EDGE_CURVE ( 'NONE', #94197, #51199, #36837, .T. ) ;
#55675 = ORIENTED_EDGE ( 'NONE', *, *, #95309, .T. ) ;
#55676 = EDGE_CURVE ( 'NONE', #69353, #63612, #4320, .T. ) ;
#55677 = CARTESIAN_POINT ( 'NONE',  ( 2.917880565312950480, 65.97041550158063217, -12.26659068614894821 ) ) ;
#55678 = CARTESIAN_POINT ( 'NONE',  ( 4.999999999999999112, 0.000000000000000000, -6.500000000000000888 ) ) ;
#55679 = CARTESIAN_POINT ( 'NONE',  ( 4.559911319644449179, 42.23035201082151247, -9.422509992056141925 ) ) ;
#55681 = CARTESIAN_POINT ( 'NONE',  ( 11.06939482307794620, 12.70153705180264758, -3.010239261523810939 ) ) ;
#55680 = CARTESIAN_POINT ( 'NONE',  ( -1.099225684535947600, 8.706968003263753531, -6.408140936763238038 ) ) ;
#55682 = CARTESIAN_POINT ( 'NONE',  ( 10.70613742633258170, 4.237152514796235822E-16, -9.778988772285240216 ) ) ;
#55683 = LINE ( 'NONE', #4538, #31579 ) ;
#55684 = DIRECTION ( 'NONE',  ( 0.000000000000000000, 0.000000000000000000, -1.000000000000000000 ) ) ;
#55685 = CARTESIAN_POINT ( 'NONE',  ( 0.000000000000000000, 14.49999999999999822, 0.000000000000000000 ) ) ;
#55686 = AXIS2_PLACEMENT_3D ( 'NONE', #62701, #92231, #48193 ) ;
#55687 = CARTESIAN_POINT ( 'NONE',  ( 1.472469842513823179, 45.59226448433412315, -4.923371831947296329 ) ) ;
#55688 = SURFACE_STYLE_USAGE ( .BOTH. , #63656 ) ;
#55689 =( BOUNDED_CURVE ( )  B_SPLINE_CURVE ( 2, ( #76780, #1315, #62260, #53792, #92766, #93752, #85774, #32254, #85278 ),
 .UNSPECIFIED., .F., .F. ) 
 B_SPLINE_CURVE_WITH_KNOTS ( ( 3, 2, 2, 2, 3 ),
 ( 0.1177146600783225971, 0.1190476190476190410, 0.1250000000000000000, 0.1309523809523809590, 0.1322853399216775416 ),
 .UNSPECIFIED. ) 
 CURVE ( )  GEOMETRIC_REPRESENTATION_ITEM ( )  RATIONAL_B_SPLINE_CURVE ( ( 0.9881565478350731180, 0.9923695281211489805, 1.000000000000000000, 0.9659258262890683122, 1.000000000000000000, 0.9659258262890683122, 1.000000000000000000, 0.9923695281211482033, 0.9881565478350723408 ) ) 
 REPRESENTATION_ITEM ( '' )  );
#55690 = CARTESIAN_POINT ( 'NONE',  ( 14.16423886937410259, 29.30374883491396076, -2.602085213965210642E-15 ) ) ;
#55691 = CARTESIAN_POINT ( 'NONE',  ( 6.565887622018943937, 10.16530133659708746, 12.81628187352647430 ) ) ;
#55692 = CARTESIAN_POINT ( 'NONE',  ( 0.5774900079438590739, 12.64701867748817321, -5.440088680355550821 ) ) ;
#55693 = DIRECTION ( 'NONE',  ( -0.000000000000000000, -0.000000000000000000, -1.000000000000000000 ) ) ;
#55694 = EDGE_CURVE ( 'NONE', #1780, #54920, #57960, .T. ) ;
#55695 = CARTESIAN_POINT ( 'NONE',  ( 22.26659068614895176, 29.72041550158063572, -7.082119434687042414 ) ) ;
#55696 = CARTESIAN_POINT ( 'NONE',  ( 22.26659068614895176, 34.72041550158063927, -7.082119434687042414 ) ) ;
#55697 = CARTESIAN_POINT ( 'NONE',  ( 2.917880565312950480, 60.97041550158063927, -12.26659068614894821 ) ) ;
#55698 = CARTESIAN_POINT ( 'NONE',  ( 5.076628168052704559, 30.17559781766745175, -8.527530157486179263 ) ) ;
#55699 = CARTESIAN_POINT ( 'NONE',  ( 10.00000000000000178, 40.37363466993042493, 12.81628187352647608 ) ) ;
#55700 = CARTESIAN_POINT ( 'NONE',  ( 15.44008868035555260, 9.730352010821505360, 9.422509992056143702 ) ) ;
#55701 = ORIENTED_EDGE ( 'NONE', *, *, #42226, .F. ) ;
#55702 = CARTESIAN_POINT ( 'NONE',  ( 1.472469842513823179, 40.59226448433411605, -4.923371831947296329 ) ) ;
#55703 = CARTESIAN_POINT ( 'NONE',  ( 4.559911319644449179, 43.89701867748816966, 9.422509992056141925 ) ) ;
#55704 = CARTESIAN_POINT ( 'NONE',  ( 18.52753015748618282, 63.92559781766745886, -4.923371831947291888 ) ) ;
#55706 = CARTESIAN_POINT ( 'NONE',  ( -0.2418659066527792945, 18.09014588040357197, 6.114288769123030320 ) ) ;
#55705 = CARTESIAN_POINT ( 'NONE',  ( -2.266590686148945544, 26.38708216824730357, -7.082119434687050408 ) ) ;
#55707 = CARTESIAN_POINT ( 'NONE',  ( 18.61655166652077042, 34.87718327197428891, 6.499999999999981348 ) ) ;
#55708 = CARTESIAN_POINT ( 'NONE',  ( 19.84674366389459266, 18.71726448433411960, -2.638427012816827677 ) ) ;
#55709 = CARTESIAN_POINT ( 'NONE',  ( 13.43411237798105340, 45.58196800326374643, 12.81628187352647963 ) ) ;
#55710 = CARTESIAN_POINT ( 'NONE',  ( 10.00000000000000178, 52.25893115100078745, 9.846743663894594434 ) ) ;
#55711 = ORIENTED_EDGE ( 'NONE', *, *, #6012, .F. ) ;
#55712 = DIRECTION ( 'NONE',  ( 0.000000000000000000, 1.000000000000000000, 0.000000000000000000 ) ) ;
#55713 = FACE_OUTER_BOUND ( 'NONE', #10849, .T. ) ;
#55714 = CARTESIAN_POINT ( 'NONE',  ( 15.44008868035555260, 4.730352010821505360, 9.422509992056143702 ) ) ;
#55715 = CARTESIAN_POINT ( 'NONE',  ( 20.88017736071110519, 55.56368534415484817, 2.639326808657452039E-16 ) ) ;
#55716 = MECHANICAL_DESIGN_GEOMETRIC_PRESENTATION_REPRESENTATION (  '', ( #22173 ), #4619 ) ;
#55717 = CARTESIAN_POINT ( 'NONE',  ( 17.08211943468705840, 5.137082168247300906, -12.26659068614894466 ) ) ;
#55718 = CARTESIAN_POINT ( 'NONE',  ( 10.00000000000000178, 64.31368534415483396, 10.88017736071110342 ) ) ;
#55719 = CARTESIAN_POINT ( 'NONE',  ( 5.076628168052703671, 56.84226448433412315, 8.527530157486179263 ) ) ;
#55720 = CARTESIAN_POINT ( 'NONE',  ( 20.88017736071110164, 25.35535201082150891, 2.915334737309930979 ) ) ;
#55721 = DIRECTION ( 'NONE',  ( -1.000000000000000000, 0.000000000000000000, 0.000000000000000000 ) ) ;
#55722 = DIRECTION ( 'NONE',  ( 0.000000000000000000, 0.000000000000000000, -1.000000000000000000 ) ) ;
#55723 = ADVANCED_FACE ( 'NONE', ( #50464 ), #14549, .T. ) ;
#55724 = VECTOR ( 'NONE', #63111, 1000.000000000000227 ) ;
#55725 = EDGE_LOOP ( 'NONE', ( #66783, #15542, #76656, #30082 ) ) ;
#55726 = CIRCLE ( 'NONE', #10965, 0.5000000000000000000 ) ;
#55727 = CARTESIAN_POINT ( 'NONE',  ( 16.40814093676323893, 60.79030133659709634, 11.09922568453595026 ) ) ;
#55728 = VERTEX_POINT ( 'NONE', #1079 ) ;
#55729 = ORIENTED_EDGE ( 'NONE', *, *, #78016, .F. ) ;
#55730 = CARTESIAN_POINT ( 'NONE',  ( -4.000000000000000000, 10.00000000000000000, -2.750000000000000000 ) ) ;
#55731 = DIRECTION ( 'NONE',  ( 0.1132032137679171296, 0.000000000000000000, -0.9935718556765862353 ) ) ;
#55732 = PRESENTATION_STYLE_ASSIGNMENT (( #2256 ) ) ;
#55733 = CARTESIAN_POINT ( 'NONE',  ( 2.917880565312948704, 47.63708216824730357, 12.26659068614894643 ) ) ;
#55734 = CARTESIAN_POINT ( 'NONE',  ( 19.84674366389459266, 63.30059781766745886, 2.638427012816836559 ) ) ;
#55735 = CARTESIAN_POINT ( 'NONE',  ( 0.1532563361054083140, 26.00893115100078745, 1.131784320476157264E-15 ) ) ;
#55736 = CARTESIAN_POINT ( 'NONE',  ( -6.000000000000011546, 40.74999999999999289, -4.250000000000000000 ) ) ;
#55738 = CARTESIAN_POINT ( 'NONE',  ( 18.52753015748617571, 63.09226448433412315, 4.923371831947298993 ) ) ;
#55737 = CARTESIAN_POINT ( 'NONE',  ( 19.42250999205614548, 15.98035201082150714, -5.440088680355545492 ) ) ;
#55739 = CARTESIAN_POINT ( 'NONE',  ( -0.3289641300568005855, 35.10497603579416648, 5.963430220938281678 ) ) ;
#55740 = CARTESIAN_POINT ( 'NONE',  ( -4.164238869374099039, 36.80374883491396787, 8.674139862899312516E-16 ) ) ;
#55741 = CARTESIAN_POINT ( 'NONE',  ( 13.79529636645031943, 65.34541550158063217, -14.16423886937409904 ) ) ;
#55742 = LINE ( 'NONE', #62235, #43403 ) ;
#55743 = FACE_OUTER_BOUND ( 'NONE', #29242, .T. ) ;
#55744 = CARTESIAN_POINT ( 'NONE',  ( 10.00000000000000178, 64.31368534415483396, 10.88017736071110342 ) ) ;
#55745 = CARTESIAN_POINT ( 'NONE',  ( 12.63842701281683922, 14.55059781766744997, -9.846743663894590881 ) ) ;
#55746 = CARTESIAN_POINT ( 'NONE',  ( -4.262581422817185661, -13.85606188144532958, 3.999999999998386624 ) ) ;
#55747 = VERTEX_POINT ( 'NONE', #29562 ) ;
#55748 = FACE_OUTER_BOUND ( 'NONE', #15896, .T. ) ;
#55749 = ORIENTED_EDGE ( 'NONE', *, *, #18341, .F. ) ;
#55750 = CARTESIAN_POINT ( 'NONE',  ( 10.00000000000000000, 29.75893115100078745, -9.846743663894594434 ) ) ;
#55751 = ORIENTED_EDGE ( 'NONE', *, *, #98842, .F. ) ;
#55752 = CARTESIAN_POINT ( 'NONE',  ( 2.917880565312950480, 30.97041550158063572, -12.26659068614894821 ) ) ;
#55753 = CARTESIAN_POINT ( 'NONE',  ( 19.84674366389459266, 33.30059781766744464, 2.638427012816836559 ) ) ;
#55754 = CARTESIAN_POINT ( 'NONE',  ( 4.559911319644449179, 37.23035201082150536, -9.422509992056141925 ) ) ;
#55755 = DIRECTION ( 'NONE',  ( 1.000000000000000000, 0.000000000000000000, 0.000000000000000000 ) ) ;
#55756 = VERTEX_POINT ( 'NONE', #69560 ) ;
#55757 = CARTESIAN_POINT ( 'NONE',  ( 20.88017736071110164, 35.35535201082150536, 2.915334737309930979 ) ) ;
#55758 = CARTESIAN_POINT ( 'NONE',  ( 6.408140936763243367, -9.209698663402903662, 11.09922568453594494 ) ) ;
#55759 = VERTEX_POINT ( 'NONE', #30555 ) ;
#55760 = CARTESIAN_POINT ( 'NONE',  ( 0.5774900079438590739, 42.64701867748816966, -5.440088680355550821 ) ) ;
#55761 = CARTESIAN_POINT ( 'NONE',  ( 13.79529636645031943, 10.34541550158063394, -14.16423886937409904 ) ) ;
#55762 = ORIENTED_EDGE ( 'NONE', *, *, #30413, .T. ) ;
#55763 = ORIENTED_EDGE ( 'NONE', *, *, #38608, .F. ) ;
#55764 = CARTESIAN_POINT ( 'NONE',  ( 22.81628187352648496, 36.83196800326376064, -3.434112377981050290 ) ) ;
#55765 =( GEOMETRIC_REPRESENTATION_CONTEXT ( 3 ) GLOBAL_UNCERTAINTY_ASSIGNED_CONTEXT ( ( #41210 ) ) GLOBAL_UNIT_ASSIGNED_CONTEXT ( ( #45625, #82634, #44127 ) ) REPRESENTATION_CONTEXT ( 'NONE', 'WORKASPACE' ) );
#55766 = CARTESIAN_POINT ( 'NONE',  ( 5.076628168052703671, 26.84226448433411960, 8.527530157486179263 ) ) ;
#55767 = LINE ( 'NONE', #86753, #84982 ) ;
#55768 = DIRECTION ( 'NONE',  ( 0.000000000000000000, 0.000000000000000000, 1.000000000000000000 ) ) ;
#55769 = CARTESIAN_POINT ( 'NONE',  ( 7.361572987183169658, 34.96726448433411605, -9.846743663894592657 ) ) ;
#55770 = EDGE_CURVE ( 'NONE', #41488, #11366, #74504, .T. ) ;
#55771 = CARTESIAN_POINT ( 'NONE',  ( 21.92686044187657046, 65.16212336850779252, 4.562052436263912550E-16 ) ) ;
#55772 = DIRECTION ( 'NONE',  ( -0.000000000000000000, 1.000000000000000000, 0.000000000000000000 ) ) ;
#55773 = CARTESIAN_POINT ( 'NONE',  ( -43.84463630040269067, 106.6354719102472473, 4.599749066889684990 ) ) ;
#55774 = DIRECTION ( 'NONE',  ( -0.000000000000000000, 0.000000000000000000, 1.000000000000000000 ) ) ;
#55775 = CARTESIAN_POINT ( 'NONE',  ( 0.1532563361054083140, 1.008931151000784787, 1.131784320476157264E-15 ) ) ;
#55776 = CARTESIAN_POINT ( 'NONE',  ( -1.099225684535947600, 14.54030133659708568, 6.408140936763237150 ) ) ;
#55777 = LINE ( 'NONE', #24308, #96199 ) ;
#55778 = B_SPLINE_CURVE_WITH_KNOTS ( 'NONE', 3,
 ( #14489, #8934, #92431, #39451, #6980, #62416 ),
 .UNSPECIFIED., .F., .F.,
 ( 4, 2, 4 ),
 ( 0.0002800015744458462423, 0.0006862068192651793203, 0.001092412064084512290 ),
 .UNSPECIFIED. ) ;
#55779 = AXIS2_PLACEMENT_3D ( 'NONE', #58794, #34303, #12313 ) ;
#55780 = CARTESIAN_POINT ( 'NONE',  ( 14.92337183194729988, 44.34226448433412315, -8.527530157486177487 ) ) ;
#55781 = CARTESIAN_POINT ( 'NONE',  ( -0.1298530154764001854, 80.39370036920264795, -9.500000000000000000 ) ) ;
#55782 = CARTESIAN_POINT ( 'NONE',  ( -2.266590686148945544, 2.220415501580634388, 7.082119434687048631 ) ) ;
#55783 = CARTESIAN_POINT ( 'NONE',  ( 0.1532563361054100626, 20.80059781766744464, -2.638427012816831230 ) ) ;
#55784 = CARTESIAN_POINT ( 'NONE',  ( -2.816281873526473856, 39.33196800326374643, 3.434112377981055619 ) ) ;
#55786 = CARTESIAN_POINT ( 'NONE',  ( 14.16722289976685012, 15.00000000000000000, -4.928467845925517565 ) ) ;
#55785 = CARTESIAN_POINT ( 'NONE',  ( 0.000000000000000000, 80.32179676972448590, -4.250000000000000000 ) ) ;
#55787 = CARTESIAN_POINT ( 'NONE',  ( 0.5774900079438607392, 48.48035201082150536, 5.440088680355550821 ) ) ;
#55788 = CARTESIAN_POINT ( 'NONE',  ( 19.38216949554541557, 12.24863466993041961, -9.382169495545420901 ) ) ;
#55789 = CARTESIAN_POINT ( 'NONE',  ( 0.1532563361054082862, 41.21726448433411605, 2.638427012816831674 ) ) ;
#55790 = AXIS2_PLACEMENT_3D ( 'NONE', #25517, #39034, #62997 ) ;
#55791 = CARTESIAN_POINT ( 'NONE',  ( 1.472469842513823179, 16.42559781766745175, 4.923371831947296329 ) ) ;
#55792 = CARTESIAN_POINT ( 'NONE',  ( 15.44008868035555793, 26.39701867748817321, -9.422509992056140149 ) ) ;
#55793 = CARTESIAN_POINT ( 'NONE',  ( -2.816281873526473856, 34.12363466993042493, 9.499525473075851096E-16 ) ) ;
#55794 = CARTESIAN_POINT ( 'NONE',  ( 5.076628168052703671, 26.84226448433411960, 8.527530157486179263 ) ) ;
#55795 = LINE ( 'NONE', #54299, #77394 ) ;
#55796 = ADVANCED_FACE ( 'NONE', ( #38572 ), #84562, .T. ) ;
#55797 = CARTESIAN_POINT ( 'NONE',  ( 2.035157376598824452, 13.68868534415483751, 7.964842623401179544 ) ) ;
#55798 = ORIENTED_EDGE ( 'NONE', *, *, #79610, .F. ) ;
#55799 =( BOUNDED_CURVE ( )  B_SPLINE_CURVE ( 2, ( #4640, #35612, #37600, #82591, #44084, #29088, #30564, #52583, #117, #28603, #7098, #98110, #21613 ),
 .UNSPECIFIED., .F., .F. ) 
 B_SPLINE_CURVE_WITH_KNOTS ( ( 3, 2, 2, 2, 2, 2, 3 ),
 ( 0.5999999999999999778, 0.6055555555555555136, 0.6111111111111111605, 0.6166666666666666963, 0.6222222222222223431, 0.6277777777777778789, 0.6333333333333334147 ),
 .UNSPECIFIED. ) 
 CURVE ( )  GEOMETRIC_REPRESENTATION_ITEM ( )  RATIONAL_B_SPLINE_CURVE ( ( 1.000000000000000000, 0.9659258262890683122, 1.000000000000000000, 0.9659258262890683122, 1.000000000000000000, 0.9659258262890683122, 1.000000000000000000, 0.9659258262890683122, 1.000000000000000000, 0.9659258262890683122, 1.000000000000000000, 0.9659258262890676461, 1.000000000000000666 ) ) 
 REPRESENTATION_ITEM ( '' )  );
#55800 = CARTESIAN_POINT ( 'NONE',  ( 12.91533473730992121, 59.52201867748816966, 10.88017736071110164 ) ) ;
#55801 = CARTESIAN_POINT ( 'NONE',  ( 4.573260519722770034, -6.401749983361684215, 2.750000000000000444 ) ) ;
#55802 = EDGE_CURVE ( 'NONE', #36587, #339, #31049, .T. ) ;
#55804 = CARTESIAN_POINT ( 'NONE',  ( 12.91533473730993009, 11.60535201082150714, -10.88017736071109987 ) ) ;
#55803 = CARTESIAN_POINT ( 'NONE',  ( 19.84674366389459266, 38.71726448433412315, -2.638427012816827677 ) ) ;
#55805 = CARTESIAN_POINT ( 'NONE',  ( 20.88017736071110519, 40.56368534415484106, 2.639326808657452039E-16 ) ) ;
#55806 = AXIS2_PLACEMENT_3D ( 'NONE', #27197, #4725, #44172 ) ;
#55808 = CARTESIAN_POINT ( 'NONE',  ( 19.72487221294571569, 59.78217586085237656, 6.499999999999986677 ) ) ;
#55807 = CARTESIAN_POINT ( 'NONE',  ( -0.8801773607110991993, 17.85535201082150536, -2.915334737309923874 ) ) ;
#55809 = CARTESIAN_POINT ( 'NONE',  ( 1.472469842513823179, 40.59226448433411605, -4.923371831947296329 ) ) ;
#55810 = CARTESIAN_POINT ( 'NONE',  ( 4.999999999999999112, 11.50000000000000000, -6.500000000000000888 ) ) ;
#55811 = CARTESIAN_POINT ( 'NONE',  ( -0.1034006766821533585, 15.00000000000000000, -14.49963131600461175 ) ) ;
#55812 = CARTESIAN_POINT ( 'NONE',  ( 16.40814093676323893, 5.790301336597087456, 11.09922568453595026 ) ) ;
#55813 = CIRCLE ( 'NONE', #36697, 15.00000000000000000 ) ;
#55814 = CARTESIAN_POINT ( 'NONE',  ( 2.917880565312948704, 2.637082168247300906, 12.26659068614894643 ) ) ;
#55815 = CARTESIAN_POINT ( 'NONE',  ( 20.36894250292379382, 18.67874883491397142, 10.36894250292379205 ) ) ;
#55816 = CYLINDRICAL_SURFACE ( 'NONE', #6576, 0.5000000000000004441 ) ;
#55817 = ORIENTED_EDGE ( 'NONE', *, *, #56101, .F. ) ;
#55818 = CARTESIAN_POINT ( 'NONE',  ( 4.559911319644449179, 7.230352010821505360, -9.422509992056141925 ) ) ;
#55819 = CARTESIAN_POINT ( 'NONE',  ( 0.1532563361054083140, 16.00893115100078390, 1.131784320476157264E-15 ) ) ;
#55821 = CARTESIAN_POINT ( 'NONE',  ( -8.331109669465192269, 86.16998870897720053, -4.268594137767635743 ) ) ;
#55820 = DIRECTION ( 'NONE',  ( 0.000000000000000000, 1.000000000000000000, -0.000000000000000000 ) ) ;
#55822 = CARTESIAN_POINT ( 'NONE',  ( 2.035157376598822676, 42.43868534415483396, -7.964842623401177768 ) ) ;
#55823 = CARTESIAN_POINT ( 'NONE',  ( -46.44000000000001194, 93.00000000000000000, 9.500000000000000000 ) ) ;
#55824 = CARTESIAN_POINT ( 'NONE',  ( 17.96484262340118221, 29.93868534415484106, 7.964842623401181321 ) ) ;
#55825 = CARTESIAN_POINT ( 'NONE',  ( 16.40814093676323893, 50.79030133659708923, 11.09922568453595026 ) ) ;
#55826 = CARTESIAN_POINT ( 'NONE',  ( -2.816281873526471635, 8.915301336597083903, -3.434112377981056508 ) ) ;
#55827 = CARTESIAN_POINT ( 'NONE',  ( 17.20831665107776587, 9.133931151000787452, -7.208316651077762316 ) ) ;
#55828 = ORIENTED_EDGE ( 'NONE', *, *, #50125, .T. ) ;
#55829 = CARTESIAN_POINT ( 'NONE',  ( 13.75801628063881488, 4.740223025775510804E-16, -4.578972376164461622 ) ) ;
#55830 = DIRECTION ( 'NONE',  ( 0.000000000000000000, 0.000000000000000000, -1.000000000000000000 ) ) ;
#55831 = CARTESIAN_POINT ( 'NONE',  ( -4.164238869374099927, 57.01208216824731068, 3.795296366450308767 ) ) ;
#55832 = CARTESIAN_POINT ( 'NONE',  ( 20.36894250292379382, 28.67874883491396787, 10.36894250292379205 ) ) ;
#55833 = CARTESIAN_POINT ( 'NONE',  ( 17.96484262340118221, 24.93868534415484461, 7.964842623401181321 ) ) ;
#55834 = CARTESIAN_POINT ( 'NONE',  ( 20.88017736071110875, 45.77201867748816966, -2.915334737309920765 ) ) ;
#55835 = EDGE_CURVE ( 'NONE', #23568, #41037, #37589, .T. ) ;
#55836 = CARTESIAN_POINT ( 'NONE',  ( 10.88670032895693218, -94.01435490391448013, -3.999999999999999112 ) ) ;
#55837 = CARTESIAN_POINT ( 'NONE',  ( 5.076628168052704559, 10.17559781766745175, -8.527530157486179263 ) ) ;
#55838 = CARTESIAN_POINT ( 'NONE',  ( 18.52753015748617571, 18.09226448433411960, 4.923371831947298993 ) ) ;
#55839 = LINE ( 'NONE', #48320, #12347 ) ;
#55840 = FILL_AREA_STYLE ('',( #9346 ) ) ;
#55841 = CARTESIAN_POINT ( 'NONE',  ( 7.361572987183170547, 27.05059781766745175, 9.846743663894590881 ) ) ;
#55842 = CARTESIAN_POINT ( 'NONE',  ( 19.84674366389459266, 48.71726448433413026, -2.638427012816827677 ) ) ;
#55843 = EDGE_CURVE ( 'NONE', #92042, #5883, #61773, .T. ) ;
#55844 = CARTESIAN_POINT ( 'NONE',  ( 20.88017736071110519, 25.56368534415483751, 2.639326808657452039E-16 ) ) ;
#55845 = CARTESIAN_POINT ( 'NONE',  ( 21.09922568453594849, 36.20696800326375353, 6.408140936763242479 ) ) ;
#55846 = CARTESIAN_POINT ( 'NONE',  ( -0.8801773607110991993, 47.85535201082150536, -2.915334737309923874 ) ) ;
#55847 = CARTESIAN_POINT ( 'NONE',  ( 18.52753015748617571, 33.09226448433411605, 4.923371831947298993 ) ) ;
#55849 = CARTESIAN_POINT ( 'NONE',  ( 19.84674366389459621, 28.50893115100078745, 7.409399052514197653E-17 ) ) ;
#55848 = CARTESIAN_POINT ( 'NONE',  ( 6.204703633549690345, 50.76208216824730357, -14.16423886937410259 ) ) ;
#55850 = FACE_OUTER_BOUND ( 'NONE', #64109, .T. ) ;
#55851 = CARTESIAN_POINT ( 'NONE',  ( 0.1532563361054083140, 56.00893115100078745, 1.131784320476157264E-15 ) ) ;
#55853 = CARTESIAN_POINT ( 'NONE',  ( 22.26659068614895176, 4.720415501580633943, -7.082119434687042414 ) ) ;
#55852 = CARTESIAN_POINT ( 'NONE',  ( 2.791683348922240793, 26.63393115100078745, 7.208316651077764092 ) ) ;
#55854 = CARTESIAN_POINT ( 'NONE',  ( 17.08211943468705840, 20.13708216824730357, -12.26659068614894466 ) ) ;
#55855 = CARTESIAN_POINT ( 'NONE',  ( 7.361572987183170547, 37.05059781766744464, 9.846743663894590881 ) ) ;
#55856 = CARTESIAN_POINT ( 'NONE',  ( 19.42250999205614548, 40.98035201082150536, -5.440088680355545492 ) ) ;
#55857 = CARTESIAN_POINT ( 'NONE',  ( -0.8801773607111008646, 28.27201867748817321, 2.915334737309923430 ) ) ;
#55858 = EDGE_CURVE ( 'NONE', #56730, #74593, #62036, .T. ) ;
#55859 = CARTESIAN_POINT ( 'NONE',  ( 17.96484262340118221, 41.18868534415484106, -7.964842623401177768 ) ) ;
#55860 = CARTESIAN_POINT ( 'NONE',  ( -0.8801773607111008646, 33.27201867748817676, 2.915334737309923430 ) ) ;
#55861 = EDGE_LOOP ( 'NONE', ( #57396, #71838, #28196, #58092 ) ) ;
#55862 = CARTESIAN_POINT ( 'NONE',  ( 7.084665262690076126, 57.02201867748817676, -10.88017736071110164 ) ) ;
#55863 = VERTEX_POINT ( 'NONE', #54534 ) ;
#55864 = CARTESIAN_POINT ( 'NONE',  ( 22.81628187352647785, 56.62363466993042493, 6.195893100308588602E-16 ) ) ;
#55865 = CARTESIAN_POINT ( 'NONE',  ( 0.5774900079438590739, 62.64701867748817676, -5.440088680355550821 ) ) ;
#55866 = ORIENTED_EDGE ( 'NONE', *, *, #22376, .F. ) ;
#55867 = DIRECTION ( 'NONE',  ( -0.000000000000000000, 1.000000000000000000, -0.000000000000000000 ) ) ;
#55868 = DIRECTION ( 'NONE',  ( 0.5547001962252290364, 0.8320502943378437211, 0.000000000000000000 ) ) ;
#55869 = CARTESIAN_POINT ( 'NONE',  ( 14.82269085861172719, 14.63606914777062151, -2.299529454046953081 ) ) ;
#55870 = CARTESIAN_POINT ( 'NONE',  ( 17.08211943468705130, 63.47041550158063927, 12.26659068614894998 ) ) ;
#55871 = CARTESIAN_POINT ( 'NONE',  ( 10.00000000000000178, 12.25893115100078568, 9.846743663894594434 ) ) ;
#55872 = CARTESIAN_POINT ( 'NONE',  ( 17.08211943468705840, 10.13708216824730179, -12.26659068614894466 ) ) ;
#55873 = CARTESIAN_POINT ( 'NONE',  ( 10.00000000000000000, 4.758931151000784787, -9.846743663894594434 ) ) ;
#55874 = CARTESIAN_POINT ( 'NONE',  ( 7.084665262690076126, 7.022018677488169658, -10.88017736071110164 ) ) ;
#55875 = CARTESIAN_POINT ( 'NONE',  ( 0.1532563361054082862, 41.21726448433411605, 2.638427012816831674 ) ) ;
#55876 = VERTEX_POINT ( 'NONE', #92058 ) ;
#55877 = CIRCLE ( 'NONE', #33442, 0.2500000000000002220 ) ;
#55878 = CARTESIAN_POINT ( 'NONE',  ( 0.1532563361054100626, 50.80059781766745175, -2.638427012816831230 ) ) ;
#55879 = ORIENTED_EDGE ( 'NONE', *, *, #63120, .F. ) ;
#55880 = FACE_OUTER_BOUND ( 'NONE', #51314, .T. ) ;
#55881 = CARTESIAN_POINT ( 'NONE',  ( 15.44008868035555260, 34.73035201082151247, 9.422509992056143702 ) ) ;
#55882 = CARTESIAN_POINT ( 'NONE',  ( 0.1532563361054100626, 55.80059781766745175, -2.638427012816831230 ) ) ;
#55884 = DIRECTION ( 'NONE',  ( 0.000000000000000000, 1.000000000000000000, 0.000000000000000000 ) ) ;
#55883 = FACE_OUTER_BOUND ( 'NONE', #80478, .T. ) ;
#55885 = CARTESIAN_POINT ( 'NONE',  ( 0.5774900079438607392, 53.48035201082151247, 5.440088680355550821 ) ) ;
#55886 = CIRCLE ( 'NONE', #30, 1.750000000000000666 ) ;
#55887 = CARTESIAN_POINT ( 'NONE',  ( 15.44008868035555793, 11.39701867748817143, -9.422509992056140149 ) ) ;
#55888 = AXIS2_PLACEMENT_3D ( 'NONE', #85511, #83661, #14688 ) ;
#55889 = EDGE_CURVE ( 'NONE', #17245, #67057, #20245, .T. ) ;
#55890 = CARTESIAN_POINT ( 'NONE',  ( 16.40814093676324603, 37.45696800326376064, -11.09922568453594671 ) ) ;
#55891 = CARTESIAN_POINT ( 'NONE',  ( -1.354709868695410657, 0.5000000000000004441, -14.93870011653153362 ) ) ;
#55892 = ADVANCED_FACE ( 'NONE', ( #61057 ), #23583, .T. ) ;
#55893 = ORIENTED_EDGE ( 'NONE', *, *, #1810, .T. ) ;
#55894 = CARTESIAN_POINT ( 'NONE',  ( -2.816281873526473856, 24.33196800326375353, 3.434112377981055619 ) ) ;
#55895 = CARTESIAN_POINT ( 'NONE',  ( 17.96484262340118221, 34.93868534415482685, 7.964842623401181321 ) ) ;
#55896 = VERTEX_POINT ( 'NONE', #23087 ) ;
#55897 = CARTESIAN_POINT ( 'NONE',  ( -0.8801773607110991993, 67.85535201082151957, -2.915334737309923874 ) ) ;
#55898 = CARTESIAN_POINT ( 'NONE',  ( 1.472469842513823179, 61.42559781766745175, 4.923371831947296329 ) ) ;
#55900 = CARTESIAN_POINT ( 'NONE',  ( 1.472469842513823179, 36.42559781766745175, 4.923371831947296329 ) ) ;
#55899 = CARTESIAN_POINT ( 'NONE',  ( 18.52753015748617571, 13.09226448433411960, 4.923371831947298993 ) ) ;
#55901 = CARTESIAN_POINT ( 'NONE',  ( -11.30270631010403726, -57.08945084610907372, 3.750000000000001776 ) ) ;
#55902 = DIRECTION ( 'NONE',  ( 0.000000000000000000, 1.000000000000000000, 0.000000000000000000 ) ) ;
#55903 = CARTESIAN_POINT ( 'NONE',  ( 5.076628168052704559, 40.17559781766745175, -8.527530157486179263 ) ) ;
#55904 = CARTESIAN_POINT ( 'NONE',  ( 0.1916775849787266950, 52.25868815902069997, -6.499999999999991118 ) ) ;
#55905 = CARTESIAN_POINT ( 'NONE',  ( 4.879999999999994564, 43.00000000000000711, 6.500000000000000888 ) ) ;
#55906 = CARTESIAN_POINT ( 'NONE',  ( 2.791683348922237240, 25.38393115100078390, -7.208316651077763204 ) ) ;
#55907 = FACE_OUTER_BOUND ( 'NONE', #10245, .T. ) ;
#55909 = ORIENTED_EDGE ( 'NONE', *, *, #1891, .T. ) ;
#55908 = CARTESIAN_POINT ( 'NONE',  ( 0.1532563361054100626, 45.80059781766745886, -2.638427012816831230 ) ) ;
#55910 = DIRECTION ( 'NONE',  ( 1.000000000000000000, 2.569960705150826877E-16, -0.000000000000000000 ) ) ;
#55911 = CARTESIAN_POINT ( 'NONE',  ( 0.6178305044545838731, 24.74863466993042493, 9.382169495545420901 ) ) ;
#55912 = EDGE_CURVE ( 'NONE', #75712, #70278, #84014, .T. ) ;
#55913 = CARTESIAN_POINT ( 'NONE',  ( 17.20831665107776587, 42.88393115100077324, 7.208316651077764980 ) ) ;
#55914 = CARTESIAN_POINT ( 'NONE',  ( 0.1922240491738554657, 8.188781737317407661, 6.500000000000007105 ) ) ;
#55915 = CARTESIAN_POINT ( 'NONE',  ( -4.164238869374098151, 46.59541550158063927, -3.795296366450310543 ) ) ;
#55916 = CARTESIAN_POINT ( 'NONE',  ( 12.63842701281683034, 22.46726448433411605, 9.846743663894596210 ) ) ;
#55917 = FILL_AREA_STYLE_COLOUR ( '', #84415 ) ;
#55918 = CARTESIAN_POINT ( 'NONE',  ( 12.99999999999999822, 75.00000000000000000, -6.500000000000000888 ) ) ;
#55919 = EDGE_CURVE ( 'NONE', #80716, #34672, #56990, .T. ) ;
#55920 = CARTESIAN_POINT ( 'NONE',  ( -2.266590686148945544, 42.22041550158063217, 7.082119434687048631 ) ) ;
#55921 = CARTESIAN_POINT ( 'NONE',  ( 10.00000000000000000, 59.75893115100078745, -9.846743663894594434 ) ) ;
#55922 = CARTESIAN_POINT ( 'NONE',  ( 2.917880565312948704, 67.63708216824730357, 12.26659068614894643 ) ) ;
#55923 = CARTESIAN_POINT ( 'NONE',  ( -0.3689425029237881626, 17.42874883491397142, 10.36894250292379027 ) ) ;
#55924 = CARTESIAN_POINT ( 'NONE',  ( 2.917880565312948704, 37.63708216824731068, 12.26659068614894643 ) ) ;
#55925 = CARTESIAN_POINT ( 'NONE',  ( 0.1955144967548975432, 29.32703681773340776, -6.500000000002792433 ) ) ;
#55927 = CARTESIAN_POINT ( 'NONE',  ( 17.20831665107776587, 57.88393115100078745, 7.208316651077764980 ) ) ;
#55926 = CARTESIAN_POINT ( 'NONE',  ( 6.655516370397832837, -69.44235516224610194, 2.500000000000000000 ) ) ;
#55928 = ORIENTED_EDGE ( 'NONE', *, *, #44112, .T. ) ;
#55929 = CARTESIAN_POINT ( 'NONE',  ( -0.8801773607111009756, 38.06368534415484106, 1.068504757029289695E-15 ) ) ;
#55930 = CARTESIAN_POINT ( 'NONE',  ( 10.91061041304828727, 14.76930270348881002, -10.20767530377049148 ) ) ;
#55931 = CARTESIAN_POINT ( 'NONE',  ( 8.629999999999995453, 40.99999999999999289, 4.250000000000000000 ) ) ;
#55932 = CARTESIAN_POINT ( 'NONE',  ( 19.84674366389459266, 43.71726448433410894, -2.638427012816827677 ) ) ;
#55933 = FACE_OUTER_BOUND ( 'NONE', #27838, .T. ) ;
#55934 = CARTESIAN_POINT ( 'NONE',  ( -10.36894250292379205, 6.178748834913974086, -10.36894250292378672 ) ) ;
#55935 = CARTESIAN_POINT ( 'NONE',  ( 1.472469842513823179, 55.59226448433412315, -4.923371831947296329 ) ) ;
#55936 = CARTESIAN_POINT ( 'NONE',  ( 12.63842701281683922, 59.55059781766744464, -9.846743663894590881 ) ) ;
#55937 = AXIS2_PLACEMENT_3D ( 'NONE', #32208, #1753, #55721 ) ;
#55938 = ORIENTED_EDGE ( 'NONE', *, *, #82650, .F. ) ;
#55939 = CARTESIAN_POINT ( 'NONE',  ( -2.266590686148945544, 31.38708216824730002, -7.082119434687050408 ) ) ;
#55940 = DIRECTION ( 'NONE',  ( -1.501154311515388838E-13, 0.8042198116156755727, 0.5943319733994190113 ) ) ;
#55942 = CARTESIAN_POINT ( 'NONE',  ( 10.00000000000000178, 70.00000000000000000, 0.000000000000000000 ) ) ;
#55941 =( NAMED_UNIT ( * ) PLANE_ANGLE_UNIT ( ) SI_UNIT ( $, .RADIAN. ) );
#55943 = CARTESIAN_POINT ( 'NONE',  ( -0.8801773607111008646, 8.272018677488171434, 2.915334737309923430 ) ) ;
#55944 = CARTESIAN_POINT ( 'NONE',  ( 21.09922568453595559, 27.04030133659708568, -6.408140936763230044 ) ) ;
#55945 =( LENGTH_UNIT ( ) NAMED_UNIT ( * ) SI_UNIT ( .MILLI., .METRE. ) );
#55946 = CARTESIAN_POINT ( 'NONE',  ( 0.1532563361054082862, 16.21726448433411960, 2.638427012816831674 ) ) ;
#55947 = VECTOR ( 'NONE', #43394, 1000.000000000000227 ) ;
#55948 = AXIS2_PLACEMENT_3D ( 'NONE', #95293, #26796, #57292 ) ;
#55949 = CARTESIAN_POINT ( 'NONE',  ( -0.3289641300568005855, 9.271642702460841434, -5.963430220938281678 ) ) ;
#55950 = CARTESIAN_POINT ( 'NONE',  ( 17.39651004071841456, 14.08210964143329669, -6.500000000000003553 ) ) ;
#55951 = CARTESIAN_POINT ( 'NONE',  ( 17.96484262340118221, 14.93868534415484106, 7.964842623401181321 ) ) ;
#55952 = CARTESIAN_POINT ( 'NONE',  ( 0.000000000000000000, 0.5000000000000004441, 0.000000000000000000 ) ) ;
#55953 = CARTESIAN_POINT ( 'NONE',  ( 20.88017736071110519, 30.56368534415484106, 2.639326808657452039E-16 ) ) ;
#55954 = CARTESIAN_POINT ( 'NONE',  ( 2.035157376598822676, 42.43868534415483396, -7.964842623401177768 ) ) ;
#55955 = CARTESIAN_POINT ( 'NONE',  ( 19.38216949554541557, 2.248634669930420049, -9.382169495545420901 ) ) ;
#55956 = CARTESIAN_POINT ( 'NONE',  ( 2.791683348922237240, 65.38393115100078035, -7.208316651077763204 ) ) ;
#55957 = CARTESIAN_POINT ( 'NONE',  ( 10.00000000000000000, 62.87363466993042493, -12.81628187352647608 ) ) ;
#55958 = CARTESIAN_POINT ( 'NONE',  ( 1.472469842513823179, 15.59226448433411960, -4.923371831947296329 ) ) ;
#55960 = ORIENTED_EDGE ( 'NONE', *, *, #97888, .T. ) ;
#55959 = AXIS2_PLACEMENT_3D ( 'NONE', #20215, #12712, #5231 ) ;
#55961 = CARTESIAN_POINT ( 'NONE',  ( 7.084665262690076126, 29.10535201082150181, 10.88017736071109987 ) ) ;
#55962 = ADVANCED_FACE ( 'NONE', ( #46071 ), #15096, .F. ) ;
#55963 = CARTESIAN_POINT ( 'NONE',  ( -2.816281873526473856, 29.33196800326376064, 3.434112377981055619 ) ) ;
#55964 = LINE ( 'NONE', #70972, #67279 ) ;
#55965 = CARTESIAN_POINT ( 'NONE',  ( 18.52753015748617571, 58.09226448433411605, 4.923371831947298993 ) ) ;
#55966 = CARTESIAN_POINT ( 'NONE',  ( 7.084665262690076126, 67.02201867748817676, -10.88017736071110164 ) ) ;
#55967 = B_SPLINE_CURVE_WITH_KNOTS ( 'NONE', 3,
 ( #6433, #36945, #7442, #83426 ),
 .UNSPECIFIED., .F., .F.,
 ( 4, 4 ),
 ( 3.291406376790657244E-17, 0.001060528352562000462 ),
 .UNSPECIFIED. ) ;
#55968 = CARTESIAN_POINT ( 'NONE',  ( 19.84674366389459266, 13.71726448433411782, -2.638427012816827677 ) ) ;
#55969 = CARTESIAN_POINT ( 'NONE',  ( -2.816281873526471635, 28.91530133659708213, -3.434112377981056508 ) ) ;
#55971 = CARTESIAN_POINT ( 'NONE',  ( -46.94000000000001194, 100.4376529975800025, -8.999999999986080468 ) ) ;
#55970 = CARTESIAN_POINT ( 'NONE',  ( 15.44008868035555260, 64.73035201082151957, 9.422509992056143702 ) ) ;
#55972 = ORIENTED_EDGE ( 'NONE', *, *, #64637, .F. ) ;
#55973 = LINE ( 'NONE', #54962, #50077 ) ;
#55974 = CARTESIAN_POINT ( 'NONE',  ( 19.42250999205614193, 10.14701867748816966, 5.440088680355555262 ) ) ;
#55976 = CARTESIAN_POINT ( 'NONE',  ( 13.79529636645031943, 25.34541550158063572, -14.16423886937409904 ) ) ;
#55975 = CARTESIAN_POINT ( 'NONE',  ( 3.591859063236763294, 58.29030133659708923, -11.09922568453595026 ) ) ;
#55977 = CARTESIAN_POINT ( 'NONE',  ( 5.076628168052703671, 11.84226448433411960, 8.527530157486179263 ) ) ;
#55978 = CARTESIAN_POINT ( 'NONE',  ( 17.96484262340118221, 4.938685344154837509, 7.964842623401181321 ) ) ;
#55979 = CIRCLE ( 'NONE', #79942, 15.00000000000000000 ) ;
#55980 = CARTESIAN_POINT ( 'NONE',  ( 0.1532563361054100626, 20.80059781766744464, -2.638427012816831230 ) ) ;
#55981 = CARTESIAN_POINT ( 'NONE',  ( -4.164238869374099039, 61.80374883491397497, 8.674139862899312516E-16 ) ) ;
#55982 = EDGE_LOOP ( 'NONE', ( #76527, #49461, #5615, #60749 ) ) ;
#55983 = DIRECTION ( 'NONE',  ( 1.000000000000000000, 0.000000000000000000, 0.000000000000000000 ) ) ;
#55984 = CARTESIAN_POINT ( 'NONE',  ( 20.88017736071110519, 25.56368534415483751, 2.639326808657452039E-16 ) ) ;
#55985 = CARTESIAN_POINT ( 'NONE',  ( 1.821708436314935620, 31.66792564121895381, -6.500000000000005329 ) ) ;
#55986 = ORIENTED_EDGE ( 'NONE', *, *, #48650, .T. ) ;
#55987 = EDGE_LOOP ( 'NONE', ( #45236, #61515, #12486, #2424, #17768, #79682 ) ) ;
#55988 = CARTESIAN_POINT ( 'NONE',  ( 20.88017736071110875, 25.77201867748816966, -2.915334737309920765 ) ) ;
#55989 = CARTESIAN_POINT ( 'NONE',  ( 2.791683348922240793, 51.63393115100078745, 7.208316651077764092 ) ) ;
#55990 = VECTOR ( 'NONE', #78163, 1000.000000000000000 ) ;
#55991 = CARTESIAN_POINT ( 'NONE',  ( 21.09922568453594849, 51.20696800326375353, 6.408140936763242479 ) ) ;
#55992 = CARTESIAN_POINT ( 'NONE',  ( 13.59943737456455715, 0.04922511925147255579, 5.718514076972947002 ) ) ;
#55994 = CARTESIAN_POINT ( 'NONE',  ( 17.08211943468705130, 23.47041550158063572, 12.26659068614894998 ) ) ;
#55993 = DIRECTION ( 'NONE',  ( 0.000000000000000000, 0.000000000000000000, 1.000000000000000000 ) ) ;
#55995 = CARTESIAN_POINT ( 'NONE',  ( 12.91533473730993009, 36.60535201082151247, -10.88017736071109987 ) ) ;
#55996 = CARTESIAN_POINT ( 'NONE',  ( -0.8801773607110991993, 12.85535201082150358, -2.915334737309923874 ) ) ;
#55997 = CARTESIAN_POINT ( 'NONE',  ( 2.791683348922240793, 56.63393115100078035, 7.208316651077764092 ) ) ;
#55998 = CARTESIAN_POINT ( 'NONE',  ( 1.472469842513823179, 35.59226448433412315, -4.923371831947296329 ) ) ;
#55999 = DIRECTION ( 'NONE',  ( 0.000000000000000000, 1.000000000000000000, 0.000000000000000000 ) ) ;
#56000 = CARTESIAN_POINT ( 'NONE',  ( 18.52753015748617571, 3.092264484334118269, 4.923371831947298993 ) ) ;
#56001 = CARTESIAN_POINT ( 'NONE',  ( -9.382169495545422677, -36.50136533006957507, -9.382169495545417348 ) ) ;
#56002 = VERTEX_POINT ( 'NONE', #98611 ) ;
#56003 =( BOUNDED_CURVE ( )  B_SPLINE_CURVE ( 3, ( #88625, #80141, #50636, #34135 ),
 .UNSPECIFIED., .F., .T. ) 
 B_SPLINE_CURVE_WITH_KNOTS ( ( 4, 4 ),
 ( 4.712388980384689674, 5.730377828609853452 ),
 .UNSPECIFIED. ) 
 CURVE ( )  GEOMETRIC_REPRESENTATION_ITEM ( )  RATIONAL_B_SPLINE_CURVE ( ( 1.000000000000000000, 0.9154899770527749059, 0.9154899770527749059, 1.000000000000000000 ) ) 
 REPRESENTATION_ITEM ( '' )  );
#56004 = CARTESIAN_POINT ( 'NONE',  ( -0.8801773607110991993, 2.855352010821504471, -2.915334737309923874 ) ) ;
#56005 = CARTESIAN_POINT ( 'NONE',  ( 18.52753015748618282, 13.92559781766745175, -4.923371831947291888 ) ) ;
#56006 = ADVANCED_FACE ( 'NONE', ( #60571 ), #24566, .T. ) ;
#56007 = CARTESIAN_POINT ( 'NONE',  ( -1.099225684535947600, -1.293031996736246469, -6.408140936763238038 ) ) ;
#56008 = CARTESIAN_POINT ( 'NONE',  ( 0.5774900079438607392, 43.48035201082151247, 5.440088680355550821 ) ) ;
#56009 = CARTESIAN_POINT ( 'NONE',  ( -1.099225684535947600, 44.54030133659708923, 6.408140936763237150 ) ) ;
#56010 = CARTESIAN_POINT ( 'NONE',  ( 10.00000000000000000, 35.55374883491396787, -14.16423886937410082 ) ) ;
#56011 = FACE_OUTER_BOUND ( 'NONE', #74099, .T. ) ;
#56012 =( BOUNDED_SURFACE ( )  B_SPLINE_SURFACE ( 1, 2, ( 
 ( #51001, #82987, #59487, #44977, #29969, #60475, #90964, #68486, #81496, #36505, #22497, #21504, #43496, #13001, #58999, #43986, #6011, #66503, #15002, #7503, #97028, #37994, #13, #89988, #30461, #52001, #82491, #36000, #28505, #89501, #66997, #97520, #508, #92933, #46460, #30956, #62933, #54930, #7983, #45979, #69957, #16956, #47924, #17457, #9947, #23492, #93435, #69462, #32432, #47440, #31445, #22995, #8950, #39467, #78429, #62430, #77939, #54442, #68976, #40450, #53963, #982, #53461, #16463, #70950, #60961, #91962, #23970, #61454, #15969, #91470, #24959, #61945, #9445, #84953, #76954, #1476, #39946, #84471, #8464, #70449, #1968, #46943, #83971, #24465, #38970, #2469, #15497, #31930, #92446, #76468, #77437, #85447, #55443, #85947, #38482, #64877, #87407, #88393, #95404, #2954, #87887, #26900, #17938, #26404, #34390, #57397, #11407, #12391, #4421, #32926, #95910, #63426, #10435, #3920, #41930, #49893, #71440, #34887, #94905, #56903, #19405, #48911, #71909, #80404, #33403, #49400, #19892, #93930, #72886, #50385, #73378, #41447, #18924, #11906, #79901, #3432, #42408, #72392, #56431, #65381, #27389, #33891, #63903, #86438, #80894, #64396, #25456, #55939, #94414, #57882, #48422, #25930, #86918, #42896, #78925, #40942, #18429, #79426, #10922, #96904, #13881, #22375, #66370, #44850, #6870, #58875, #36379, #89866, #59858, #43374, #59362, #88887, #73877, #97897, #67367, #52852, #5404, #90345, #20890, #28383, #14882, #66874, #60352, #82864, #83358, #52361, #45351, #36878, #21882, #65877, #29355, #81379, #97391, #81865, #4905, #14381, #75355, #96404, #37381, #12879, #28859, #13378, #21381, #35877, #89377, #35386, #67871, #5884, #98392, #51878, #51378, #82360, #29848, #43863, #74357, #90846, #27879, #44364, #58367, #6364, #74865, #20397, #50885, #54321, #45857, #62812, #30839, #8345, #76348, #76830, #61825, #8831, #31325, #32307, #39345, #7864, #31814, #69839, #60844, #69342, #77316, #1363, #84835, #55314, #47310, #75856, #39827, #7376, #53342, #46825, #16343, #92817, #15376, #77809, #38852, #866, #62311, #91848, #15858, #24348, #38360, #92333, #93310, #37874, #16835, #24833, #17336, #84357, #23856, #54811, #85322, #46343, #9324, #70333, #388, #1849, #85822, #68368, #68857, #30338, #98887, #91344, #22871, #83850, #61337, #23364, #53848, #40816, #71315, #64762, #26284, #80279, #2833, #63781, #49285, #33289, #56785, #65256, #10315, #87769, #49770, #94290, #79297, #33765, #3804, #86313, #3303, #32799, #17816, #41806, #11286, #95784, #48298, #34260, #25813, #56309, #57764, #10806, #4294, #26777, #27265, #95274, #41324, #86805 ),
 ( #18307, #57275, #87280, #11780, #48789, #71796, #79784, #64272, #18801, #88267, #94784, #19284, #42287, #72274, #72759, #34768, #47805, #78805, #78306, #63294, #9825, #40326, #70830, #2343, #93803, #25334, #55818, #81262, #29731, #51259, #75241, #97779, #67755, #67255, #98274, #51758, #74748, #80775, #82243, #96282, #13259, #96783, #81743, #27760, #73753, #19771, #21769, #20769, #6259, #43751, #5284, #97278, #29244, #12761, #58245, #36762, #59741, #74237, #12268, #21261, #66248, #6751, #60239, #28752, #88763, #37268, #35760, #5770, #20274, #36259, #66755, #13757, #59244, #50258, #44243, #50771, #90236, #52248, #4785, #89743, #82742, #14263, #44740, #42778, #73262, #35260, #65757, #43259, #28258, #58754, #89258, #8715, #30222, #92704, #53727, #15748, #54207, #7754, #30716, #16229, #91226, #8239, #47196, #90734, #31703, #77699, #32189, #271, #46234, #92219, #38733, #61225, #61705, #76720, #15260, #84724, #60726, #23747, #76237, #22750, #24229, #46709, #37758, #75735, #758, #77209, #9210, #39723, #70216, #53233, #54695, #91730, #62195, #39233, #23252, #52735, #69234, #31209, #1735, #69721, #1247, #84244, #98774, #22260, #83738, #85217, #83242, #16721, #14765, #45238, #45741, #7254, #68254, #38248, #68739, #55191, #17222, #2228, #41205, #93191, #56675, #11172, #57158, #93689, #40698, #19169, #64644, #25223, #33660, #95155, #64156, #3196, #63671, #87164, #94674, #26183, #41692, #63182, #11667, #42180, #34150, #85708, #32687, #72162, #71201, #80157, #87656, #2724, #33178, #47701, #78695, #25706, #78193, #10693, #3689, #71685, #18195, #94175, #4177, #48675, #18690, #79675, #55703, #56197, #86690, #79178, #26664, #49173, #48183, #9706, #49649, #40204, #24718, #72644, #62691, #70710, #86199, #17711, #10205, #14143, #27149, #81141, #21145, #66132, #88148, #95664, #4677, #65639, #58131, #12156, #67130, #36136, #42661, #59623, #44119, #5159, #5657, #35645, #96662, #58641, #90120, #65144, #57651, #21647, #74629, #52131, #75122, #43142, #89140, #66643, #51141, #73633, #97167, #20650, #88640, #28635, #28142, #81630, #35139, #19660, #82628, #13137, #34648, #50150, #73137, #43635, #80661, #27645, #20148, #51644, #74121, #97657, #50653, #12644, #59124, #89633, #82125, #44627, #96163, #6142, #36645, #13635, #29121, #91613, #61589, #45112, #61104, #90613, #75618, #645, #69113, #24110, #7129, #92101, #22634, #68130, #16604, #38133, #62078, #84607, #54580, #54092, #85095, #38614, #23631, #67638, #31095, #83120, #151, #83622, #68621, #14649, #60612, #6630, #8603, #7643, #16108, #30599, #91108, #84117, #46594, #98658, #37633, #77093, #39113 ) ),
 .UNSPECIFIED., .F., .F., .T. ) 
 B_SPLINE_SURFACE_WITH_KNOTS ( ( 2, 2 ),
 ( 3, 2, 2, 2, 2, 2, 2, 2, 2, 2, 2, 2, 2, 2, 2, 2, 2, 2, 2, 2, 2, 2, 2, 2, 2, 2, 2, 2, 2, 2, 2, 2, 2, 2, 2, 2, 2, 2, 2, 2, 2, 2, 2, 2, 2, 2, 2, 2, 2, 2, 2, 2, 2, 2, 2, 2, 2, 2, 2, 2, 2, 2, 2, 2, 2, 2, 2, 2, 2, 2, 2, 2, 2, 2, 2, 2, 2, 2, 2, 2, 2, 2, 2, 2, 2, 2, 2, 2, 2, 2, 2, 2, 2, 2, 2, 2, 2, 2, 2, 2, 2, 2, 2, 2, 2, 2, 2, 2, 2, 2, 2, 2, 2, 2, 2, 2, 2, 2, 2, 2, 2, 2, 2, 2, 2, 2, 2, 2, 2, 2, 2, 2, 2, 2, 2, 2, 2, 2, 2, 2, 2, 2, 2, 2, 2, 2, 2, 2, 2, 2, 2, 2, 2, 2, 2, 2, 2, 2, 2, 2, 2, 2, 3 ),
 ( 0.000000000000000000, 1.000000000000000000 ),
 ( 0.000000000000000000, 0.005952380952380952051, 0.01190476190476190410, 0.01785714285714285615, 0.02380952380952380820, 0.02976190476190476025, 0.03571428571428571230, 0.04166666666666666435, 0.04761904761904761640, 0.05357142857142856845, 0.05952380952380952051, 0.06547619047619047949, 0.07142857142857142461, 0.07738095238095238360, 0.08333333333333332871, 0.08928571428571428770, 0.09523809523809523281, 0.1011904761904761918, 0.1071428571428571369, 0.1130952380952380959, 0.1190476190476190410, 0.1250000000000000000, 0.1309523809523809590, 0.1369047619047619180, 0.1428571428571428492, 0.1488095238095238082, 0.1547619047619047672, 0.1607142857142857262, 0.1666666666666666574, 0.1726190476190476164, 0.1785714285714285754, 0.1845238095238095344, 0.1904761904761904656, 0.1964285714285714246, 0.2023809523809523836, 0.2083333333333333426, 0.2142857142857142738, 0.2202380952380952328, 0.2261904761904761918, 0.2321428571428571508, 0.2380952380952380820, 0.2440476190476190410, 0.2500000000000000000, 0.2559523809523809312, 0.2619047619047619180, 0.2678571428571428492, 0.2738095238095238360, 0.2797619047619047672, 0.2857142857142856984, 0.2916666666666666852, 0.2976190476190476164, 0.3035714285714285476, 0.3095238095238095344, 0.3154761904761904656, 0.3214285714285714524, 0.3273809523809523836, 0.3333333333333333148, 0.3392857142857143016, 0.3452380952380952328, 0.3511904761904761640, 0.3571428571428571508, 0.3630952380952380820, 0.3690476190476190688, 0.3750000000000000000, 0.3809523809523809312, 0.3869047619047619180, 0.3928571428571428492, 0.3988095238095238360, 0.4047619047619047672, 0.4107142857142856984, 0.4166666666666666852, 0.4226190476190476164, 0.4285714285714285476, 0.4345238095238095344, 0.4404761904761904656, 0.4464285714285714524, 0.4523809523809523836, 0.4583333333333333148, 0.4642857142857143016, 0.4702380952380952328, 0.4761904761904761640, 0.4821428571428571508, 0.4880952380952380820, 0.4940476190476190688, 0.5000000000000000000, 0.5059523809523809312, 0.5119047619047618625, 0.5178571428571429047, 0.5238095238095238360, 0.5297619047619047672, 0.5357142857142856984, 0.5416666666666666297, 0.5476190476190476719, 0.5535714285714286031, 0.5595238095238095344, 0.5654761904761904656, 0.5714285714285713969, 0.5773809523809523281, 0.5833333333333333703, 0.5892857142857143016, 0.5952380952380952328, 0.6011904761904761640, 0.6071428571428570953, 0.6130952380952381375, 0.6190476190476190688, 0.6250000000000000000, 0.6309523809523809312, 0.6369047619047618625, 0.6428571428571429047, 0.6488095238095238360, 0.6547619047619047672, 0.6607142857142856984, 0.6666666666666666297, 0.6726190476190476719, 0.6785714285714286031, 0.6845238095238095344, 0.6904761904761904656, 0.6964285714285713969, 0.7023809523809523281, 0.7083333333333333703, 0.7142857142857143016, 0.7202380952380952328, 0.7261904761904761640, 0.7321428571428570953, 0.7380952380952381375, 0.7440476190476190688, 0.7500000000000000000, 0.7559523809523809312, 0.7619047619047618625, 0.7678571428571429047, 0.7738095238095238360, 0.7797619047619047672, 0.7857142857142856984, 0.7916666666666666297, 0.7976190476190476719, 0.8035714285714286031, 0.8095238095238095344, 0.8154761904761904656, 0.8214285714285713969, 0.8273809523809523281, 0.8333333333333333703, 0.8392857142857143016, 0.8452380952380952328, 0.8511904761904761640, 0.8571428571428570953, 0.8630952380952381375, 0.8690476190476190688, 0.8750000000000000000, 0.8809523809523809312, 0.8869047619047618625, 0.8928571428571429047, 0.8988095238095238360, 0.9047619047619047672, 0.9107142857142856984, 0.9166666666666666297, 0.9226190476190476719, 0.9285714285714286031, 0.9345238095238095344, 0.9404761904761904656, 0.9464285714285713969, 0.9523809523809523281, 0.9583333333333333703, 0.9642857142857143016 ),
 .UNSPECIFIED. ) 
 GEOMETRIC_REPRESENTATION_ITEM ( )  RATIONAL_B_SPLINE_SURFACE ( (
 ( 1.000000000000000000, 0.9659258262890683122, 1.000000000000000000, 0.9659258262890683122, 1.000000000000000000, 0.9659258262890683122, 1.000000000000000000, 0.9659258262890683122, 1.000000000000000000, 0.9659258262890683122, 1.000000000000000000, 0.9659258262890683122, 1.000000000000000000, 0.9659258262890683122, 1.000000000000000000, 0.9659258262890683122, 1.000000000000000000, 0.9659258262890683122, 1.000000000000000000, 0.9659258262890683122, 1.000000000000000000, 0.9659258262890683122, 1.000000000000000000, 0.9659258262890683122, 1.000000000000000000, 0.9659258262890683122, 1.000000000000000000, 0.9659258262890683122, 1.000000000000000000, 0.9659258262890683122, 1.000000000000000000, 0.9659258262890683122, 1.000000000000000000, 0.9659258262890683122, 1.000000000000000000, 0.9659258262890683122, 1.000000000000000000, 0.9659258262890683122, 1.000000000000000000, 0.9659258262890683122, 1.000000000000000000, 0.9659258262890683122, 1.000000000000000000, 0.9659258262890683122, 1.000000000000000000, 0.9659258262890683122, 1.000000000000000000, 0.9659258262890683122, 1.000000000000000000, 0.9659258262890683122, 1.000000000000000000, 0.9659258262890683122, 1.000000000000000000, 0.9659258262890683122, 1.000000000000000000, 0.9659258262890683122, 1.000000000000000000, 0.9659258262890683122, 1.000000000000000000, 0.9659258262890683122, 1.000000000000000000, 0.9659258262890683122, 1.000000000000000000, 0.9659258262890683122, 1.000000000000000000, 0.9659258262890683122, 1.000000000000000000, 0.9659258262890683122, 1.000000000000000000, 0.9659258262890683122, 1.000000000000000000, 0.9659258262890683122, 1.000000000000000000, 0.9659258262890683122, 1.000000000000000000, 0.9659258262890683122, 1.000000000000000000, 0.9659258262890683122, 1.000000000000000000, 0.9659258262890683122, 1.000000000000000000, 0.9659258262890683122, 1.000000000000000000, 0.9659258262890683122, 1.000000000000000000, 0.9659258262890683122, 1.000000000000000000, 0.9659258262890683122, 1.000000000000000000, 0.9659258262890683122, 1.000000000000000000, 0.9659258262890683122, 1.000000000000000000, 0.9659258262890683122, 1.000000000000000000, 0.9659258262890683122, 1.000000000000000000, 0.9659258262890683122, 1.000000000000000000, 0.9659258262890683122, 1.000000000000000000, 0.9659258262890683122, 1.000000000000000000, 0.9659258262890683122, 1.000000000000000000, 0.9659258262890683122, 1.000000000000000000, 0.9659258262890683122, 1.000000000000000000, 0.9659258262890683122, 1.000000000000000000, 0.9659258262890683122, 1.000000000000000000, 0.9659258262890683122, 1.000000000000000000, 0.9659258262890683122, 1.000000000000000000, 0.9659258262890683122, 1.000000000000000000, 0.9659258262890683122, 1.000000000000000000, 0.9659258262890683122, 1.000000000000000000, 0.9659258262890683122, 1.000000000000000000, 0.9659258262890683122, 1.000000000000000000, 0.9659258262890683122, 1.000000000000000000, 0.9659258262890683122, 1.000000000000000000, 0.9659258262890683122, 1.000000000000000000, 0.9659258262890683122, 1.000000000000000000, 0.9659258262890683122, 1.000000000000000000, 0.9659258262890683122, 1.000000000000000000, 0.9659258262890683122, 1.000000000000000000, 0.9659258262890683122, 1.000000000000000000, 0.9659258262890683122, 1.000000000000000000, 0.9659258262890683122, 1.000000000000000000, 0.9659258262890683122, 1.000000000000000000, 0.9659258262890683122, 1.000000000000000000, 0.9659258262890683122, 1.000000000000000000, 0.9659258262890683122, 1.000000000000000000, 0.9659258262890683122, 1.000000000000000000, 0.9659258262890683122, 1.000000000000000000, 0.9659258262890683122, 1.000000000000000000, 0.9659258262890683122, 1.000000000000000000, 0.9659258262890683122, 1.000000000000000000, 0.9659258262890683122, 1.000000000000000000, 0.9659258262890683122, 1.000000000000000000, 0.9659258262890683122, 1.000000000000000000, 0.9659258262890683122, 1.000000000000000000, 0.9659258262890683122, 1.000000000000000000, 0.9659258262890683122, 1.000000000000000000, 0.9659258262890683122, 1.000000000000000000, 0.9659258262890683122, 1.000000000000000000, 0.9659258262890683122, 1.000000000000000000, 0.9659258262890683122, 1.000000000000000000, 0.9659258262890683122, 1.000000000000000000, 0.9659258262890683122, 1.000000000000000000, 0.9659258262890683122, 1.000000000000000000, 0.9659258262890683122, 1.000000000000000000, 0.9659258262890683122, 1.000000000000000000, 0.9659258262890683122, 1.000000000000000000, 0.9659258262890683122, 1.000000000000000000, 0.9659258262890683122, 1.000000000000000000, 0.9659258262890683122, 1.000000000000000000, 0.9659258262890683122, 1.000000000000000000, 0.9659258262890683122, 1.000000000000000000, 0.9659258262890683122, 1.000000000000000000, 0.9659258262890683122, 1.000000000000000000, 0.9659258262890683122, 1.000000000000000000, 0.9659258262890683122, 1.000000000000000000, 0.9659258262890683122, 1.000000000000000000, 0.9659258262890683122, 1.000000000000000000, 0.9659258262890683122, 1.000000000000000000, 0.9659258262890683122, 1.000000000000000000, 0.9659258262890683122, 1.000000000000000000, 0.9659258262890683122, 1.000000000000000000, 0.9659258262890683122, 1.000000000000000000, 0.9659258262890683122, 1.000000000000000000, 0.9659258262890683122, 1.000000000000000000, 0.9659258262890683122, 1.000000000000000000, 0.9659258262890683122, 1.000000000000000000, 0.9659258262890683122, 1.000000000000000000, 0.9659258262890683122, 1.000000000000000000, 0.9659258262890683122, 1.000000000000000000, 0.9659258262890683122, 1.000000000000000000, 0.9659258262890683122, 1.000000000000000000, 0.9659258262890683122, 1.000000000000000000, 0.9659258262890683122, 1.000000000000000000, 0.9659258262890683122, 1.000000000000000000, 0.9659258262890683122, 1.000000000000000000, 0.9659258262890683122, 1.000000000000000000, 0.9659258262890683122, 1.000000000000000000, 0.9659258262890683122, 1.000000000000000000, 0.9659258262890683122, 1.000000000000000000, 0.9659258262890683122, 1.000000000000000000, 0.9659258262890683122, 1.000000000000000000, 0.9659258262890683122, 1.000000000000000000, 0.9659258262890683122, 1.000000000000000000, 0.9659258262890683122, 1.000000000000000000, 0.9659258262890683122, 1.000000000000000000, 0.9659258262890683122, 1.000000000000000000, 0.9659258262890683122, 1.000000000000000000, 0.9659258262890683122, 1.000000000000000000, 0.9659258262890683122, 1.000000000000000000, 0.9659258262890683122, 1.000000000000000000, 0.9659258262890683122, 1.000000000000000000, 0.9659258262890683122, 1.000000000000000000, 0.9659258262890683122, 1.000000000000000000, 0.9659258262890683122, 1.000000000000000000, 0.9659258262890683122, 1.000000000000000000, 0.9659258262890683122, 1.000000000000000000, 0.9659258262890683122, 1.000000000000000000, 0.9659258262890683122, 1.000000000000000000, 0.9659258262890683122, 1.000000000000000000, 0.9659258262890683122, 1.000000000000000000, 0.9659258262890683122, 1.000000000000000000, 0.9659258262890683122, 1.000000000000000000, 0.9659258262890683122, 1.000000000000000000, 0.9659258262890683122, 1.000000000000000000, 0.9659258262890683122, 1.000000000000000000, 0.9659258262890683122, 1.000000000000000000, 0.9659258262890683122, 1.000000000000000000, 0.9659258262890683122, 1.000000000000000000, 0.9659258262890683122, 1.000000000000000000, 0.9659258262890683122, 1.000000000000000000),
 ( 1.000000000000000000, 0.9659258262890683122, 1.000000000000000000, 0.9659258262890683122, 1.000000000000000000, 0.9659258262890683122, 1.000000000000000000, 0.9659258262890683122, 1.000000000000000000, 0.9659258262890683122, 1.000000000000000000, 0.9659258262890683122, 1.000000000000000000, 0.9659258262890683122, 1.000000000000000000, 0.9659258262890683122, 1.000000000000000000, 0.9659258262890683122, 1.000000000000000000, 0.9659258262890683122, 1.000000000000000000, 0.9659258262890683122, 1.000000000000000000, 0.9659258262890683122, 1.000000000000000000, 0.9659258262890683122, 1.000000000000000000, 0.9659258262890683122, 1.000000000000000000, 0.9659258262890683122, 1.000000000000000000, 0.9659258262890683122, 1.000000000000000000, 0.9659258262890683122, 1.000000000000000000, 0.9659258262890683122, 1.000000000000000000, 0.9659258262890683122, 1.000000000000000000, 0.9659258262890683122, 1.000000000000000000, 0.9659258262890683122, 1.000000000000000000, 0.9659258262890683122, 1.000000000000000000, 0.9659258262890683122, 1.000000000000000000, 0.9659258262890683122, 1.000000000000000000, 0.9659258262890683122, 1.000000000000000000, 0.9659258262890683122, 1.000000000000000000, 0.9659258262890683122, 1.000000000000000000, 0.9659258262890683122, 1.000000000000000000, 0.9659258262890683122, 1.000000000000000000, 0.9659258262890683122, 1.000000000000000000, 0.9659258262890683122, 1.000000000000000000, 0.9659258262890683122, 1.000000000000000000, 0.9659258262890683122, 1.000000000000000000, 0.9659258262890683122, 1.000000000000000000, 0.9659258262890683122, 1.000000000000000000, 0.9659258262890683122, 1.000000000000000000, 0.9659258262890683122, 1.000000000000000000, 0.9659258262890683122, 1.000000000000000000, 0.9659258262890683122, 1.000000000000000000, 0.9659258262890683122, 1.000000000000000000, 0.9659258262890683122, 1.000000000000000000, 0.9659258262890683122, 1.000000000000000000, 0.9659258262890683122, 1.000000000000000000, 0.9659258262890683122, 1.000000000000000000, 0.9659258262890683122, 1.000000000000000000, 0.9659258262890683122, 1.000000000000000000, 0.9659258262890683122, 1.000000000000000000, 0.9659258262890683122, 1.000000000000000000, 0.9659258262890683122, 1.000000000000000000, 0.9659258262890683122, 1.000000000000000000, 0.9659258262890683122, 1.000000000000000000, 0.9659258262890683122, 1.000000000000000000, 0.9659258262890683122, 1.000000000000000000, 0.9659258262890683122, 1.000000000000000000, 0.9659258262890683122, 1.000000000000000000, 0.9659258262890683122, 1.000000000000000000, 0.9659258262890683122, 1.000000000000000000, 0.9659258262890683122, 1.000000000000000000, 0.9659258262890683122, 1.000000000000000000, 0.9659258262890683122, 1.000000000000000000, 0.9659258262890683122, 1.000000000000000000, 0.9659258262890683122, 1.000000000000000000, 0.9659258262890683122, 1.000000000000000000, 0.9659258262890683122, 1.000000000000000000, 0.9659258262890683122, 1.000000000000000000, 0.9659258262890683122, 1.000000000000000000, 0.9659258262890683122, 1.000000000000000000, 0.9659258262890683122, 1.000000000000000000, 0.9659258262890683122, 1.000000000000000000, 0.9659258262890683122, 1.000000000000000000, 0.9659258262890683122, 1.000000000000000000, 0.9659258262890683122, 1.000000000000000000, 0.9659258262890683122, 1.000000000000000000, 0.9659258262890683122, 1.000000000000000000, 0.9659258262890683122, 1.000000000000000000, 0.9659258262890683122, 1.000000000000000000, 0.9659258262890683122, 1.000000000000000000, 0.9659258262890683122, 1.000000000000000000, 0.9659258262890683122, 1.000000000000000000, 0.9659258262890683122, 1.000000000000000000, 0.9659258262890683122, 1.000000000000000000, 0.9659258262890683122, 1.000000000000000000, 0.9659258262890683122, 1.000000000000000000, 0.9659258262890683122, 1.000000000000000000, 0.9659258262890683122, 1.000000000000000000, 0.9659258262890683122, 1.000000000000000000, 0.9659258262890683122, 1.000000000000000000, 0.9659258262890683122, 1.000000000000000000, 0.9659258262890683122, 1.000000000000000000, 0.9659258262890683122, 1.000000000000000000, 0.9659258262890683122, 1.000000000000000000, 0.9659258262890683122, 1.000000000000000000, 0.9659258262890683122, 1.000000000000000000, 0.9659258262890683122, 1.000000000000000000, 0.9659258262890683122, 1.000000000000000000, 0.9659258262890683122, 1.000000000000000000, 0.9659258262890683122, 1.000000000000000000, 0.9659258262890683122, 1.000000000000000000, 0.9659258262890683122, 1.000000000000000000, 0.9659258262890683122, 1.000000000000000000, 0.9659258262890683122, 1.000000000000000000, 0.9659258262890683122, 1.000000000000000000, 0.9659258262890683122, 1.000000000000000000, 0.9659258262890683122, 1.000000000000000000, 0.9659258262890683122, 1.000000000000000000, 0.9659258262890683122, 1.000000000000000000, 0.9659258262890683122, 1.000000000000000000, 0.9659258262890683122, 1.000000000000000000, 0.9659258262890683122, 1.000000000000000000, 0.9659258262890683122, 1.000000000000000000, 0.9659258262890683122, 1.000000000000000000, 0.9659258262890683122, 1.000000000000000000, 0.9659258262890683122, 1.000000000000000000, 0.9659258262890683122, 1.000000000000000000, 0.9659258262890683122, 1.000000000000000000, 0.9659258262890683122, 1.000000000000000000, 0.9659258262890683122, 1.000000000000000000, 0.9659258262890683122, 1.000000000000000000, 0.9659258262890683122, 1.000000000000000000, 0.9659258262890683122, 1.000000000000000000, 0.9659258262890683122, 1.000000000000000000, 0.9659258262890683122, 1.000000000000000000, 0.9659258262890683122, 1.000000000000000000, 0.9659258262890683122, 1.000000000000000000, 0.9659258262890683122, 1.000000000000000000, 0.9659258262890683122, 1.000000000000000000, 0.9659258262890683122, 1.000000000000000000, 0.9659258262890683122, 1.000000000000000000, 0.9659258262890683122, 1.000000000000000000, 0.9659258262890683122, 1.000000000000000000, 0.9659258262890683122, 1.000000000000000000, 0.9659258262890683122, 1.000000000000000000, 0.9659258262890683122, 1.000000000000000000, 0.9659258262890683122, 1.000000000000000000, 0.9659258262890683122, 1.000000000000000000, 0.9659258262890683122, 1.000000000000000000, 0.9659258262890683122, 1.000000000000000000, 0.9659258262890683122, 1.000000000000000000, 0.9659258262890683122, 1.000000000000000000, 0.9659258262890683122, 1.000000000000000000, 0.9659258262890683122, 1.000000000000000000, 0.9659258262890683122, 1.000000000000000000, 0.9659258262890683122, 1.000000000000000000, 0.9659258262890683122, 1.000000000000000000, 0.9659258262890683122, 1.000000000000000000, 0.9659258262890683122, 1.000000000000000000, 0.9659258262890683122, 1.000000000000000000, 0.9659258262890683122, 1.000000000000000000, 0.9659258262890683122, 1.000000000000000000, 0.9659258262890683122, 1.000000000000000000, 0.9659258262890683122, 1.000000000000000000, 0.9659258262890683122, 1.000000000000000000, 0.9659258262890683122, 1.000000000000000000, 0.9659258262890683122, 1.000000000000000000, 0.9659258262890683122, 1.000000000000000000, 0.9659258262890683122, 1.000000000000000000, 0.9659258262890683122, 1.000000000000000000, 0.9659258262890683122, 1.000000000000000000, 0.9659258262890683122, 1.000000000000000000, 0.9659258262890683122, 1.000000000000000000, 0.9659258262890683122, 1.000000000000000000, 0.9659258262890683122, 1.000000000000000000) ) ) 
 REPRESENTATION_ITEM ( '' )  SURFACE ( )  );
#56013 = AXIS2_PLACEMENT_3D ( 'NONE', #24602, #3085, #26068 ) ;
#56014 = ADVANCED_FACE ( 'NONE', ( #2565 ), #55542, .F. ) ;
#56015 = CARTESIAN_POINT ( 'NONE',  ( 10.00000000000000000, 57.87363466993042493, -12.81628187352647608 ) ) ;
#56016 = EDGE_CURVE ( 'NONE', #8937, #39745, #12320, .T. ) ;
#56017 = ORIENTED_EDGE ( 'NONE', *, *, #205, .T. ) ;
#56018 = CARTESIAN_POINT ( 'NONE',  ( 2.791683348922240793, 56.63393115100078035, 7.208316651077764092 ) ) ;
#56019 = CARTESIAN_POINT ( 'NONE',  ( 17.96484262340118221, 16.18868534415483396, -7.964842623401177768 ) ) ;
#56020 = CIRCLE ( 'NONE', #20897, 0.2500000000000002220 ) ;
#56021 = ORIENTED_EDGE ( 'NONE', *, *, #26849, .F. ) ;
#56022 = CARTESIAN_POINT ( 'NONE',  ( 2.035157376598824452, 68.68868534415484817, 7.964842623401179544 ) ) ;
#56023 = CIRCLE ( 'NONE', #51219, 0.2500000000000002220 ) ;
#56024 = CARTESIAN_POINT ( 'NONE',  ( 12.63842701281683034, 12.46726448433411782, 9.846743663894596210 ) ) ;
#56025 = CARTESIAN_POINT ( 'NONE',  ( 12.91533473730993009, 66.60535201082150536, -10.88017736071109987 ) ) ;
#56026 = SURFACE_SIDE_STYLE ('',( #78518 ) ) ;
#56028 = CARTESIAN_POINT ( 'NONE',  ( -5.419894505350420388, 0.3639313574487524350, -13.98659156302468887 ) ) ;
#56027 = CARTESIAN_POINT ( 'NONE',  ( 7.084665262690076126, 57.02201867748817676, -10.88017736071110164 ) ) ;
#56029 = CARTESIAN_POINT ( 'NONE',  ( 15.44008868035555260, 64.73035201082151957, 9.422509992056143702 ) ) ;
#56031 = ORIENTED_EDGE ( 'NONE', *, *, #74382, .F. ) ;
#56030 = CARTESIAN_POINT ( 'NONE',  ( 7.361572987183169658, 9.967264484334119601, -9.846743663894592657 ) ) ;
#56032 = DIRECTION ( 'NONE',  ( -1.000000000000000000, 0.000000000000000000, 0.000000000000000000 ) ) ;
#56034 = ADVANCED_FACE ( 'NONE', ( #70051 ), #64489, .F. ) ;
#56033 = CARTESIAN_POINT ( 'NONE',  ( 17.20831665107776587, 57.88393115100078745, 7.208316651077764980 ) ) ;
#56035 = ORIENTED_EDGE ( 'NONE', *, *, #39203, .T. ) ;
#56036 = ORIENTED_EDGE ( 'NONE', *, *, #91354, .F. ) ;
#56037 = LINE ( 'NONE', #63519, #77764 ) ;
#56038 = CARTESIAN_POINT ( 'NONE',  ( 13.79529636645031943, 5.345415501580634832, -14.16423886937409904 ) ) ;
#56039 = CARTESIAN_POINT ( 'NONE',  ( -2.816281873526471635, 63.91530133659708923, -3.434112377981056508 ) ) ;
#56040 = EDGE_CURVE ( 'NONE', #44664, #98330, #56037, .T. ) ;
#56041 = CARTESIAN_POINT ( 'NONE',  ( 24.16423886937410614, 4.303748834913967869, 8.672049930838204340E-16 ) ) ;
#56042 = CARTESIAN_POINT ( 'NONE',  ( 6.204703633549690345, 35.76208216824729647, -14.16423886937410259 ) ) ;
#56043 = CYLINDRICAL_SURFACE ( 'NONE', #18742, 0.2500000000000002220 ) ;
#56044 = CARTESIAN_POINT ( 'NONE',  ( 6.204703633549690345, 5.762082168247301794, -14.16423886937410259 ) ) ;
#56045 = CARTESIAN_POINT ( 'NONE',  ( 4.559911319644449179, 23.89701867748817321, 9.422509992056141925 ) ) ;
#56046 = FACE_OUTER_BOUND ( 'NONE', #23570, .T. ) ;
#56047 = ORIENTED_EDGE ( 'NONE', *, *, #84676, .F. ) ;
#56048 = CARTESIAN_POINT ( 'NONE',  ( 7.361572987183170547, 2.050597817667451750, 9.846743663894590881 ) ) ;
#56049 = CARTESIAN_POINT ( 'NONE',  ( 18.52753015748617571, 18.09226448433411960, 4.923371831947298993 ) ) ;
#56050 = AXIS2_PLACEMENT_3D ( 'NONE', #67114, #6611, #20633 ) ;
#56051 = CARTESIAN_POINT ( 'NONE',  ( 21.09922568453595559, 42.04030133659708213, -6.408140936763230044 ) ) ;
#56052 = CARTESIAN_POINT ( 'NONE',  ( 19.84674366389459266, 33.30059781766744464, 2.638427012816836559 ) ) ;
#56053 = LINE ( 'NONE', #48528, #31443 ) ;
#56054 = CARTESIAN_POINT ( 'NONE',  ( -1.099225684535947600, 24.54030133659708923, 6.408140936763237150 ) ) ;
#56055 = CARTESIAN_POINT ( 'NONE',  ( -7.082119434687044190, -27.36291783175269643, 12.26659068614894998 ) ) ;
#56056 = CARTESIAN_POINT ( 'NONE',  ( 0.1532563361054083140, 21.00893115100078745, 1.131784320476157264E-15 ) ) ;
#56057 = VECTOR ( 'NONE', #16966, 1000.000000000000114 ) ;
#56058 = CARTESIAN_POINT ( 'NONE',  ( -4.164238869374099927, 12.01208216824730357, 3.795296366450308767 ) ) ;
#56059 = ORIENTED_EDGE ( 'NONE', *, *, #28453, .T. ) ;
#56060 = CARTESIAN_POINT ( 'NONE',  ( 10.00000000000000178, 34.31368534415484106, 10.88017736071110342 ) ) ;
#56061 = CARTESIAN_POINT ( 'NONE',  ( 22.26659068614894466, 33.88708216824730357, 7.082119434687054849 ) ) ;
#56062 = CARTESIAN_POINT ( 'NONE',  ( 1.472469842513823179, 51.42559781766745886, 4.923371831947296329 ) ) ;
#56063 = CARTESIAN_POINT ( 'NONE',  ( 18.52753015748617571, 8.092264484334117824, 4.923371831947298993 ) ) ;
#56065 = CARTESIAN_POINT ( 'NONE',  ( 0.2751277870542891413, 24.36607318730131411, -6.499999999999989342 ) ) ;
#56064 = CARTESIAN_POINT ( 'NONE',  ( -1.099225684535947600, 59.54030133659708923, 6.408140936763237150 ) ) ;
#56066 = CARTESIAN_POINT ( 'NONE',  ( -0.8801773607111009756, 28.06368534415484106, 1.068504757029289695E-15 ) ) ;
#56067 = DIRECTION ( 'NONE',  ( 0.000000000000000000, 1.000000000000000000, 0.000000000000000000 ) ) ;
#56068 = CARTESIAN_POINT ( 'NONE',  ( 13.43411237798106583, 17.66530133659708923, -12.81628187352647252 ) ) ;
#56069 = CARTESIAN_POINT ( 'NONE',  ( 19.38216949554541202, 15.99863466993042138, 9.382169495545424454 ) ) ;
#56070 = CARTESIAN_POINT ( 'NONE',  ( 14.92337183194729988, 39.34226448433412315, -8.527530157486177487 ) ) ;
#56071 = CARTESIAN_POINT ( 'NONE',  ( -2.915334737309934532, 2.022018677488174099, -10.88017736071109987 ) ) ;
#56072 = CARTESIAN_POINT ( 'NONE',  ( 14.69266224296342571, 0.04962895675140013840, 1.335284760096239864 ) ) ;
#56074 = CARTESIAN_POINT ( 'NONE',  ( -10.82625193755174742, -96.00405735513187722, -4.000000000000000000 ) ) ;
#56073 = CARTESIAN_POINT ( 'NONE',  ( 15.44008868035555260, 64.73035201082151957, 9.422509992056143702 ) ) ;
#56075 = PLANE ( 'NONE',  #97708 ) ;
#56076 = DIRECTION ( 'NONE',  ( 0.000000000000000000, 0.000000000000000000, -1.000000000000000000 ) ) ;
#56077 = CARTESIAN_POINT ( 'NONE',  ( 2.035157376598824452, 58.68868534415482685, 7.964842623401179544 ) ) ;
#56078 = VECTOR ( 'NONE', #24490, 1000.000000000000000 ) ;
#56079 = CARTESIAN_POINT ( 'NONE',  ( -0.8801773607110991993, 57.85535201082149825, -2.915334737309923874 ) ) ;
#56080 = LINE ( 'NONE', #11548, #56871 ) ;
#56081 = CARTESIAN_POINT ( 'NONE',  ( 3.840373378095567336, 13.17686044187654559, -11.29165764256138260 ) ) ;
#56082 = CARTESIAN_POINT ( 'NONE',  ( 10.00000000000000000, 6.813685344154838397, -10.88017736071110342 ) ) ;
#56083 = CARTESIAN_POINT ( 'NONE',  ( 10.00000000000000000, 64.75893115100078035, -9.846743663894594434 ) ) ;
#56085 = CARTESIAN_POINT ( 'NONE',  ( -7.072473351904092986, -84.40137333043811907, -3.750000000000000444 ) ) ;
#56084 = CARTESIAN_POINT ( 'NONE',  ( -0.8801773607111009756, 23.06368534415484106, 1.068504757029289695E-15 ) ) ;
#56086 = SURFACE_STYLE_FILL_AREA ( #25594 ) ;
#56087 = STYLED_ITEM ( 'NONE', ( #2001 ), #47007 ) ;
#56088 = CARTESIAN_POINT ( 'NONE',  ( -1.099225684535947600, 18.70696800326375353, -6.408140936763238038 ) ) ;
#56089 = ORIENTED_EDGE ( 'NONE', *, *, #49798, .F. ) ;
#56090 = CARTESIAN_POINT ( 'NONE',  ( -0.8801773607110991993, 47.85535201082150536, -2.915334737309923874 ) ) ;
#56091 = CARTESIAN_POINT ( 'NONE',  ( 14.92337183194729988, 44.34226448433412315, -8.527530157486177487 ) ) ;
#56092 = CARTESIAN_POINT ( 'NONE',  ( 21.09922568453595559, 7.040301336597086568, -6.408140936763230044 ) ) ;
#56093 = CARTESIAN_POINT ( 'NONE',  ( 0.5774900079438590739, 32.64701867748816966, -5.440088680355550821 ) ) ;
#56094 = CARTESIAN_POINT ( 'NONE',  ( 20.88017736071110875, 40.77201867748818387, -2.915334737309920765 ) ) ;
#56095 = CARTESIAN_POINT ( 'NONE',  ( 24.16423886937410614, 49.51208216824730357, -3.795296366450302550 ) ) ;
#56096 = CARTESIAN_POINT ( 'NONE',  ( 10.00000000000000000, 34.75893115100078745, -9.846743663894594434 ) ) ;
#56097 = CARTESIAN_POINT ( 'NONE',  ( 17.96484262340118221, 54.93868534415484106, 7.964842623401181321 ) ) ;
#56098 = CARTESIAN_POINT ( 'NONE',  ( 19.42250999205614548, 55.98035201082150536, -5.440088680355545492 ) ) ;
#56099 = DIRECTION ( 'NONE',  ( 1.000000000000000000, 0.000000000000000000, 0.000000000000000000 ) ) ;
#56100 = CARTESIAN_POINT ( 'NONE',  ( 6.204703633549690345, 20.76208216824730357, -14.16423886937410259 ) ) ;
#56101 = EDGE_CURVE ( 'NONE', #53272, #31285, #87332, .T. ) ;
#56102 = DIRECTION ( 'NONE',  ( -0.000000000000000000, -1.000000000000000000, -0.000000000000000000 ) ) ;
#56103 = CARTESIAN_POINT ( 'NONE',  ( -46.82017113615791004, 100.6079546444643427, 9.324761308090124601 ) ) ;
#56104 = EDGE_LOOP ( 'NONE', ( #86528, #39075, #5396, #9747 ) ) ;
#56105 = CARTESIAN_POINT ( 'NONE',  ( 24.16423886937410614, 49.51208216824730357, -3.795296366450302550 ) ) ;
#56106 = CARTESIAN_POINT ( 'NONE',  ( -0.3689425029237898834, 31.17874883491396787, -10.36894250292378850 ) ) ;
#56107 = CARTESIAN_POINT ( 'NONE',  ( 12.63842701281683922, 19.55059781766745175, -9.846743663894590881 ) ) ;
#56108 = CARTESIAN_POINT ( 'NONE',  ( 22.81628187352648496, 21.83196800326374643, -3.434112377981050290 ) ) ;
#56109 = DIRECTION ( 'NONE',  ( 2.107602052970794797E-16, -1.000000000000000000, 0.000000000000000000 ) ) ;
#56110 = CYLINDRICAL_SURFACE ( 'NONE', #48224, 0.5000000000000004441 ) ;
#56112 = CARTESIAN_POINT ( 'NONE',  ( -2.816281873526473856, 34.12363466993042493, 9.499525473075851096E-16 ) ) ;
#56111 = CARTESIAN_POINT ( 'NONE',  ( 12.91533473730993009, 66.60535201082150536, -10.88017736071109987 ) ) ;
#56113 = CARTESIAN_POINT ( 'NONE',  ( 20.36894250292379738, 49.92874883491396787, -10.36894250292379027 ) ) ;
#56114 = CARTESIAN_POINT ( 'NONE',  ( 15.44008868035555260, 64.73035201082151957, 9.422509992056143702 ) ) ;
#56115 = CARTESIAN_POINT ( 'NONE',  ( 9.846743663894590881, -16.28273551566588040, -2.638427012816833894 ) ) ;
#56116 = CARTESIAN_POINT ( 'NONE',  ( 0.1532563361054100626, 5.800597817667452638, -2.638427012816831230 ) ) ;
#56117 = ORIENTED_EDGE ( 'NONE', *, *, #10931, .F. ) ;
#56118 = CARTESIAN_POINT ( 'NONE',  ( 17.20831665107776587, 22.88393115100078745, 7.208316651077764980 ) ) ;
#56119 = ORIENTED_EDGE ( 'NONE', *, *, #47320, .F. ) ;
#56121 = ADVANCED_FACE ( 'NONE', ( #94508 ), #18520, .T. ) ;
#56120 = FACE_OUTER_BOUND ( 'NONE', #94090, .T. ) ;
#56122 = EDGE_LOOP ( 'NONE', ( #15787, #23555, #46232, #11487 ) ) ;
#56123 = CARTESIAN_POINT ( 'NONE',  ( -2.266590686148945544, 7.220415501580634832, 7.082119434687048631 ) ) ;
#56125 = CARTESIAN_POINT ( 'NONE',  ( 20.88017736071110519, 5.563685344154838397, 2.639326808657452039E-16 ) ) ;
#56124 = CARTESIAN_POINT ( 'NONE',  ( 19.42250999205614548, 10.98035201082150536, -5.440088680355545492 ) ) ;
#56127 = CARTESIAN_POINT ( 'NONE',  ( 21.09922568453595559, 2.040301336597086568, -6.408140936763230044 ) ) ;
#56126 = CARTESIAN_POINT ( 'NONE',  ( 17.20831665107776587, 34.13393115100078745, -7.208316651077762316 ) ) ;
#56128 = FACE_OUTER_BOUND ( 'NONE', #53725, .T. ) ;
#56129 = PRESENTATION_LAYER_ASSIGNMENT (  '', '', ( #1820 ) ) ;
#56130 = DIRECTION ( 'NONE',  ( -0.000000000000000000, -0.000000000000000000, -1.000000000000000000 ) ) ;
#56131 = EDGE_CURVE ( 'NONE', #33705, #61749, #86040, .T. ) ;
#56132 = CARTESIAN_POINT ( 'NONE',  ( -2.816281873526473856, 14.33196800326375531, 3.434112377981055619 ) ) ;
#56133 = ADVANCED_FACE ( 'NONE', ( #3529 ), #79017, .T. ) ;
#56134 = ORIENTED_EDGE ( 'NONE', *, *, #28563, .F. ) ;
#56135 = CARTESIAN_POINT ( 'NONE',  ( 10.00000000000000178, 53.05374883491396787, 14.16423886937410082 ) ) ;
#56136 = ORIENTED_EDGE ( 'NONE', *, *, #40124, .T. ) ;
#56137 = CARTESIAN_POINT ( 'NONE',  ( 24.16423886937410614, 54.30374883491396787, 8.672049930838204340E-16 ) ) ;
#56138 = EDGE_LOOP ( 'NONE', ( #97789, #83439, #96863, #52546, #82164, #85044 ) ) ;
#56139 = CARTESIAN_POINT ( 'NONE',  ( 17.96484262340118221, 34.93868534415482685, 7.964842623401181321 ) ) ;
#56140 = CARTESIAN_POINT ( 'NONE',  ( 19.42250999205614548, 35.98035201082151247, -5.440088680355545492 ) ) ;
#56141 = CARTESIAN_POINT ( 'NONE',  ( 20.88017736071110519, 40.56368534415484106, 2.639326808657452039E-16 ) ) ;
#56142 = CARTESIAN_POINT ( 'NONE',  ( 4.559911319644449179, 63.89701867748817676, 9.422509992056141925 ) ) ;
#56143 = CARTESIAN_POINT ( 'NONE',  ( 10.00000000000000000, 21.81368534415484106, -10.88017736071110342 ) ) ;
#56145 = AXIS2_PLACEMENT_3D ( 'NONE', #98049, #91512, #45510 ) ;
#56144 = CARTESIAN_POINT ( 'NONE',  ( 0.2850016562179803481, 0.2303298976893956851, -14.93805486374024838 ) ) ;
#56146 = CIRCLE ( 'NONE', #48207, 20.49999999999999645 ) ;
#56147 = CARTESIAN_POINT ( 'NONE',  ( 14.92337183194729988, 9.342264484334119601, -8.527530157486177487 ) ) ;
#56148 = DIRECTION ( 'NONE',  ( 0.000000000000000000, 1.000000000000000000, 0.000000000000000000 ) ) ;
#56149 = ORIENTED_EDGE ( 'NONE', *, *, #8756, .T. ) ;
#56150 = CARTESIAN_POINT ( 'NONE',  ( 11.20666413564172537, -56.81049121600104002, 4.000000000000000000 ) ) ;
#56151 = CARTESIAN_POINT ( 'NONE',  ( 5.076628168052704559, 50.17559781766745886, -8.527530157486179263 ) ) ;
#56152 = CARTESIAN_POINT ( 'NONE',  ( 0.000000000000000000, 0.5000000000000004441, 0.000000000000000000 ) ) ;
#56153 = AXIS2_PLACEMENT_3D ( 'NONE', #16498, #93961, #17488 ) ;
#56154 = EDGE_CURVE ( 'NONE', #17335, #27398, #56552, .T. ) ;
#56155 = PRESENTATION_STYLE_ASSIGNMENT (( #66089 ) ) ;
#56156 = ORIENTED_EDGE ( 'NONE', *, *, #97151, .F. ) ;
#56157 = CARTESIAN_POINT ( 'NONE',  ( 34.56412365047464874, 28.99999999999999645, 7.000000000000000000 ) ) ;
#56158 = CARTESIAN_POINT ( 'NONE',  ( -45.94000000000000483, 103.9981609152045650, 5.961202730336928823 ) ) ;
#56159 = CARTESIAN_POINT ( 'NONE',  ( -4.000000000000000000, 78.07179676972445748, 6.500000000000000888 ) ) ;
#56160 = CARTESIAN_POINT ( 'NONE',  ( -2.266590686148945544, 41.38708216824729647, -7.082119434687050408 ) ) ;
#56161 = CARTESIAN_POINT ( 'NONE',  ( -13.14228782657351680, 14.49999999999999112, 7.230509711182154575 ) ) ;
#56162 = ORIENTED_EDGE ( 'NONE', *, *, #92818, .F. ) ;
#56164 = CIRCLE ( 'NONE', #60923, 0.2500000000000002220 ) ;
#56163 = CARTESIAN_POINT ( 'NONE',  ( 20.15039907845753930, 70.00000000000000000, -6.262539305110068177 ) ) ;
#56165 = CARTESIAN_POINT ( 'NONE',  ( 0.1532563361054100626, 20.80059781766744464, -2.638427012816831230 ) ) ;
#56166 = CARTESIAN_POINT ( 'NONE',  ( -14.16722289976688565, 0.5000000000000004441, 4.928467845925418089 ) ) ;
#56167 = CARTESIAN_POINT ( 'NONE',  ( 2.791683348922237240, 60.38393115100078745, -7.208316651077763204 ) ) ;
#56168 = CARTESIAN_POINT ( 'NONE',  ( -0.8801773607110991993, 67.85535201082151957, -2.915334737309923874 ) ) ;
#56169 = DIRECTION ( 'NONE',  ( 0.000000000000000000, -1.000000000000000000, 0.000000000000000000 ) ) ;
#56170 = CARTESIAN_POINT ( 'NONE',  ( 10.00000000000000178, 62.25893115100078745, 9.846743663894594434 ) ) ;
#56171 = CARTESIAN_POINT ( 'NONE',  ( 19.10478245763050964, 20.10160829253885950, 5.990408912944338304 ) ) ;
#56172 = VERTEX_POINT ( 'NONE', #85545 ) ;
#56173 = CARTESIAN_POINT ( 'NONE',  ( 10.00000000000000000, 65.55374883491396076, -14.16423886937410082 ) ) ;
#56174 = CARTESIAN_POINT ( 'NONE',  ( 0.000000000000000000, 0.5000000000000004441, 0.000000000000000000 ) ) ;
#56175 = CARTESIAN_POINT ( 'NONE',  ( 15.44008868035555793, 46.39701867748817676, -9.422509992056140149 ) ) ;
#56177 = CARTESIAN_POINT ( 'NONE',  ( 4.559911319644449179, 68.89701867748817676, 9.422509992056141925 ) ) ;
#56176 = CARTESIAN_POINT ( 'NONE',  ( 13.43411237798106583, 17.66530133659708923, -12.81628187352647252 ) ) ;
#56178 = CARTESIAN_POINT ( 'NONE',  ( -8.502721643904161297, 0.04962896249296521595, 12.05657636697095825 ) ) ;
#56179 = CARTESIAN_POINT ( 'NONE',  ( -14.73551000134585820, 14.95037106540114991, -0.7225335126799745655 ) ) ;
#56180 = CARTESIAN_POINT ( 'NONE',  ( -0.1038446121089069418, 54.24302437010793909, -6.337995344473775106 ) ) ;
#56181 = CARTESIAN_POINT ( 'NONE',  ( 2.791683348922240793, 51.63393115100078745, 7.208316651077764092 ) ) ;
#56182 = SURFACE_STYLE_FILL_AREA ( #33646 ) ;
#56183 = CARTESIAN_POINT ( 'NONE',  ( 3.795296366450314540, 28.26208216824730712, 14.16423886937410082 ) ) ;
#56184 = CARTESIAN_POINT ( 'NONE',  ( 22.81628187352647785, 6.415301336597088344, 3.434112377981063169 ) ) ;
#56186 = SURFACE_STYLE_FILL_AREA ( #47691 ) ;
#56185 = CARTESIAN_POINT ( 'NONE',  ( 2.035157376598824452, 18.68868534415484106, 7.964842623401179544 ) ) ;
#56187 = DIRECTION ( 'NONE',  ( 1.000000000000000000, -1.257568779154408793E-17, 0.000000000000000000 ) ) ;
#56188 = CARTESIAN_POINT ( 'NONE',  ( 10.00000000000000000, 35.55374883491396787, -14.16423886937410082 ) ) ;
#56189 = CARTESIAN_POINT ( 'NONE',  ( 6.204703633549690345, 30.76208216824730357, -14.16423886937410259 ) ) ;
#56190 = CARTESIAN_POINT ( 'NONE',  ( 24.16423886937409904, 59.09541550158063217, 3.795296366450317205 ) ) ;
#56191 = CARTESIAN_POINT ( 'NONE',  ( 17.20831665107776587, 42.88393115100077324, 7.208316651077764980 ) ) ;
#56192 = CARTESIAN_POINT ( 'NONE',  ( 13.43411237798105340, 40.58196800326375353, 12.81628187352647963 ) ) ;
#56193 = CARTESIAN_POINT ( 'NONE',  ( 17.96484262340118221, 11.18868534415483929, -7.964842623401177768 ) ) ;
#56194 = VECTOR ( 'NONE', #84530, 1000.000000000000000 ) ;
#56195 = VERTEX_POINT ( 'NONE', #10526 ) ;
#56196 = CARTESIAN_POINT ( 'NONE',  ( 2.791683348922240793, 36.63393115100078035, 7.208316651077764092 ) ) ;
#56197 = CARTESIAN_POINT ( 'NONE',  ( 7.084665262690076126, 44.10535201082151247, 10.88017736071109987 ) ) ;
#56198 = B_SPLINE_CURVE_WITH_KNOTS ( 'NONE', 3,
 ( #19765, #57756, #5277, #27256, #35754, #94777, #20266, #34253, #88259, #56779, #81254, #20761, #27752, #58236, #87274, #43251, #79778, #50250 ),
 .UNSPECIFIED., .F., .F.,
 ( 4, 2, 2, 2, 2, 2, 2, 2, 4 ),
 ( 2.775557561562891043E-17, 0.01113190067936639140, 0.02226380135873275504, 0.04452760271746546150, 0.06679140407619817144, 0.07792330475556452640, 0.08348925509524771083, 0.08627223026508930304, 0.08905520543493089525 ),
 .UNSPECIFIED. ) ;
#56199 = CARTESIAN_POINT ( 'NONE',  ( 0.6178305044545838731, 9.748634669930416052, 9.382169495545420901 ) ) ;
#56201 = CARTESIAN_POINT ( 'NONE',  ( 0.000000000000000000, 15.00000000000000000, 0.000000000000000000 ) ) ;
#56200 = CARTESIAN_POINT ( 'NONE',  ( 17.08211943468705840, 20.13708216824730357, -12.26659068614894466 ) ) ;
#56202 = CARTESIAN_POINT ( 'NONE',  ( -13.59972906620759936, 14.95037118612066784, -5.718800721552383060 ) ) ;
#56203 = CARTESIAN_POINT ( 'NONE',  ( 7.361572987183169658, 24.96726448433412315, -9.846743663894592657 ) ) ;
#56204 = CARTESIAN_POINT ( 'NONE',  ( 3.591859063236763294, 48.29030133659708923, -11.09922568453595026 ) ) ;
#56205 = CARTESIAN_POINT ( 'NONE',  ( 17.20831665107776587, 59.13393115100078745, -7.208316651077762316 ) ) ;
#56206 = ORIENTED_EDGE ( 'NONE', *, *, #66771, .F. ) ;
#56207 = CARTESIAN_POINT ( 'NONE',  ( 8.880000000000000782, 1.019547802438459216, -3.750000000000000000 ) ) ;
#56208 = CARTESIAN_POINT ( 'NONE',  ( -2.266590686148945544, 62.22041550158063927, 7.082119434687048631 ) ) ;
#56209 = CARTESIAN_POINT ( 'NONE',  ( 17.08211943468705130, 13.47041550158063572, 12.26659068614894998 ) ) ;
#56210 = CARTESIAN_POINT ( 'NONE',  ( 0.1532563361054100626, 0.8005978176674514168, -2.638427012816831230 ) ) ;
#56211 = CARTESIAN_POINT ( 'NONE',  ( 19.84674366389459621, 53.50893115100078745, 7.409399052514197653E-17 ) ) ;
#56212 = CARTESIAN_POINT ( 'NONE',  ( 15.44008868035555793, 16.39701867748817321, -9.422509992056140149 ) ) ;
#56213 = CARTESIAN_POINT ( 'NONE',  ( 20.30776406404415724, 70.00000000000000000, -6.000000000000001776 ) ) ;
#56214 = EDGE_CURVE ( 'NONE', #44561, #75676, #85048, .T. ) ;
#56215 = ORIENTED_EDGE ( 'NONE', *, *, #68560, .T. ) ;
#56216 = VECTOR ( 'NONE', #22212, 1000.000000000000000 ) ;
#56217 = PRESENTATION_STYLE_ASSIGNMENT (( #19681 ) ) ;
#56218 = VERTEX_POINT ( 'NONE', #32531 ) ;
#56219 = MECHANICAL_DESIGN_GEOMETRIC_PRESENTATION_REPRESENTATION (  '', ( #3484 ), #44997 ) ;
#56220 = ORIENTED_EDGE ( 'NONE', *, *, #91567, .T. ) ;
#56221 = CARTESIAN_POINT ( 'NONE',  ( 11.25000000000000178, 10.21346884451820181, 3.014428414850127691 ) ) ;
#56222 = CARTESIAN_POINT ( 'NONE',  ( 6.204703633549690345, 5.762082168247301794, -14.16423886937410259 ) ) ;
#56223 = CARTESIAN_POINT ( 'NONE',  ( -4.164238869374099039, 1.803748834913967647, 8.674139862899312516E-16 ) ) ;
#56224 = CARTESIAN_POINT ( 'NONE',  ( -0.3689425029237881626, 42.42874883491396787, 10.36894250292379027 ) ) ;
#56225 = CARTESIAN_POINT ( 'NONE',  ( 18.52753015748618282, 63.92559781766745886, -4.923371831947291888 ) ) ;
#56226 = CARTESIAN_POINT ( 'NONE',  ( 0.1532563361054083140, 21.00893115100078745, 1.131784320476157264E-15 ) ) ;
#56227 = CARTESIAN_POINT ( 'NONE',  ( -2.816281873526473856, 64.12363466993042493, 9.499525473075851096E-16 ) ) ;
#56229 = CARTESIAN_POINT ( 'NONE',  ( 0.6178305044545818747, -1.501365330069579951, -9.382169495545419124 ) ) ;
#56228 = CARTESIAN_POINT ( 'NONE',  ( 4.559911319644449179, 18.89701867748817321, 9.422509992056141925 ) ) ;
#56230 = CARTESIAN_POINT ( 'NONE',  ( 20.36894250292379738, 4.928748834913967869, -10.36894250292379027 ) ) ;
#56231 = CARTESIAN_POINT ( 'NONE',  ( -2.266590686148945544, 41.38708216824729647, -7.082119434687050408 ) ) ;
#56232 = CARTESIAN_POINT ( 'NONE',  ( 2.035157376598824452, 3.688685344154837953, 7.964842623401179544 ) ) ;
#56233 = DIRECTION ( 'NONE',  ( 0.000000000000000000, 0.000000000000000000, 1.000000000000000000 ) ) ;
#56234 = CIRCLE ( 'NONE', #13096, 15.00000000000000000 ) ;
#56235 = FACE_OUTER_BOUND ( 'NONE', #36028, .T. ) ;
#56236 = CARTESIAN_POINT ( 'NONE',  ( 4.559911319644449179, 58.89701867748817676, 9.422509992056141925 ) ) ;
#56237 = STYLED_ITEM ( 'NONE', ( #28665 ), #90872 ) ;
#56238 = CARTESIAN_POINT ( 'NONE',  ( 5.076628168052704559, 15.17559781766745175, -8.527530157486179263 ) ) ;
#56239 = CARTESIAN_POINT ( 'NONE',  ( 12.40504043596831885, 57.00871557427475977, -2.900000000000000799 ) ) ;
#56240 = EDGE_LOOP ( 'NONE', ( #6709, #4391, #42870, #89939, #42970, #85281, #9369, #67579, #27832, #28092 ) ) ;
#56241 = PLANE ( 'NONE',  #93748 ) ;
#56242 = PRESENTATION_LAYER_ASSIGNMENT (  '', '', ( #61006 ) ) ;
#56243 = VERTEX_POINT ( 'NONE', #25545 ) ;
#56244 = CARTESIAN_POINT ( 'NONE',  ( 14.92337183194729988, 19.34226448433411960, -8.527530157486177487 ) ) ;
#56245 = ORIENTED_EDGE ( 'NONE', *, *, #85954, .F. ) ;
#56246 = CARTESIAN_POINT ( 'NONE',  ( 13.79529636645030344, 38.26208216824729647, 14.16423886937410614 ) ) ;
#56247 = CARTESIAN_POINT ( 'NONE',  ( 18.52753015748617571, 33.09226448433411605, 4.923371831947298993 ) ) ;
#56248 = CARTESIAN_POINT ( 'NONE',  ( 12.91533473730992121, 39.52201867748817676, 10.88017736071110164 ) ) ;
#56249 = CARTESIAN_POINT ( 'NONE',  ( 4.559911319644449179, 47.23035201082150536, -9.422509992056141925 ) ) ;
#56250 = EDGE_CURVE ( 'NONE', #66530, #95512, #39561, .T. ) ;
#56251 = CARTESIAN_POINT ( 'NONE',  ( -0.1503990784575329198, 2.222660991849184864, -6.262539305110070842 ) ) ;
#56252 = CARTESIAN_POINT ( 'NONE',  ( -3.434112377981047626, 0.1653013365970882609, 12.81628187352647963 ) ) ;
#56253 = EDGE_CURVE ( 'NONE', #55896, #42155, #52222, .T. ) ;
#56254 = ORIENTED_EDGE ( 'NONE', *, *, #20227, .F. ) ;
#56255 = CARTESIAN_POINT ( 'NONE',  ( 2.917880565312950480, 0.9704155015806342766, -12.26659068614894821 ) ) ;
#56256 = ORIENTED_EDGE ( 'NONE', *, *, #18349, .F. ) ;
#56257 = EDGE_LOOP ( 'NONE', ( #59171, #23667, #82143, #42023 ) ) ;
#56258 = CARTESIAN_POINT ( 'NONE',  ( 22.81628187352647785, 26.62363466993042138, 6.195893100308588602E-16 ) ) ;
#56259 = CARTESIAN_POINT ( 'NONE',  ( 17.20831665107776587, 27.88393115100078390, 7.208316651077764980 ) ) ;
#56260 = PRODUCT_DEFINITION ( 'UNKNOWN', '', #88670, #37477 ) ;
#56261 = CARTESIAN_POINT ( 'NONE',  ( 6.565887622018943937, 45.16530133659708923, 12.81628187352647430 ) ) ;
#56262 = CARTESIAN_POINT ( 'NONE',  ( -46.34161155552185818, 104.0475784593833737, -5.921604558741679902 ) ) ;
#56263 = CARTESIAN_POINT ( 'NONE',  ( 19.84674366389459266, 28.30059781766745886, 2.638427012816836559 ) ) ;
#56264 = CARTESIAN_POINT ( 'NONE',  ( 15.44008868035555793, 56.39701867748817676, -9.422509992056140149 ) ) ;
#56265 =( GEOMETRIC_REPRESENTATION_CONTEXT ( 3 ) GLOBAL_UNCERTAINTY_ASSIGNED_CONTEXT ( ( #83456 ) ) GLOBAL_UNIT_ASSIGNED_CONTEXT ( ( #22558, #91536, #23052 ) ) REPRESENTATION_CONTEXT ( 'NONE', 'WORKASPACE' ) );
#56266 = CARTESIAN_POINT ( 'NONE',  ( 13.99999999999999822, 11.50000000000000000, -6.000000000000000000 ) ) ;
#56267 = CARTESIAN_POINT ( 'NONE',  ( 2.258648100792191471, 14.95077488074853456, 14.57890972981274125 ) ) ;
#56268 = EDGE_CURVE ( 'NONE', #30184, #28589, #17553, .T. ) ;
#56269 = DIRECTION ( 'NONE',  ( -0.000000000000000000, -1.000000000000000000, -0.000000000000000000 ) ) ;
#56270 = CARTESIAN_POINT ( 'NONE',  ( 2.035157376598824452, 68.68868534415484817, 7.964842623401179544 ) ) ;
#56271 = CARTESIAN_POINT ( 'NONE',  ( -2.816281873526473856, 14.12363466993041961, 9.499525473075851096E-16 ) ) ;
#56272 = DIRECTION ( 'NONE',  ( -0.000000000000000000, 1.000000000000000000, -0.000000000000000000 ) ) ;
#56273 = CARTESIAN_POINT ( 'NONE',  ( 5.076628168052704559, 40.17559781766745175, -8.527530157486179263 ) ) ;
#56274 = CARTESIAN_POINT ( 'NONE',  ( 8.564643372776615138, 15.00000000000000000, -12.31449893000740836 ) ) ;
#56275 = CARTESIAN_POINT ( 'NONE',  ( 17.08211943468705130, 3.470415501580634388, 12.26659068614894998 ) ) ;
#56276 = CARTESIAN_POINT ( 'NONE',  ( 10.00000000000000178, 37.25893115100078745, 9.846743663894594434 ) ) ;
#56277 = CARTESIAN_POINT ( 'NONE',  ( 13.43411237798106583, 37.66530133659708923, -12.81628187352647252 ) ) ;
#56279 = DIRECTION ( 'NONE',  ( -0.000000000000000000, -0.000000000000000000, 1.000000000000000000 ) ) ;
#56278 = PLANE ( 'NONE',  #51661 ) ;
#56280 = CARTESIAN_POINT ( 'NONE',  ( 4.559911319644449179, 52.23035201082151247, -9.422509992056141925 ) ) ;
#56281 = CARTESIAN_POINT ( 'NONE',  ( 16.40814093676324603, 12.45696800326375353, -11.09922568453594671 ) ) ;
#56282 = CARTESIAN_POINT ( 'NONE',  ( 1.472469842513823179, 40.59226448433411605, -4.923371831947296329 ) ) ;
#56283 = CARTESIAN_POINT ( 'NONE',  ( 17.20831665107776587, 19.13393115100078035, -7.208316651077762316 ) ) ;
#56284 = CARTESIAN_POINT ( 'NONE',  ( 2.035157376598824452, 33.68868534415484106, 7.964842623401179544 ) ) ;
#56285 = CARTESIAN_POINT ( 'NONE',  ( 16.40814093676323893, 35.79030133659708923, 11.09922568453595026 ) ) ;
#56286 = AXIS2_PLACEMENT_3D ( 'NONE', #74886, #30360, #52382 ) ;
#56287 = CARTESIAN_POINT ( 'NONE',  ( 5.076628168052704559, 20.17559781766745175, -8.527530157486179263 ) ) ;
#56288 = CARTESIAN_POINT ( 'NONE',  ( -8.641261271118773735, 87.40425324006859853, 4.716577832614896160 ) ) ;
#56289 = CARTESIAN_POINT ( 'NONE',  ( 2.035157376598824452, 23.68868534415484461, 7.964842623401179544 ) ) ;
#56290 = VECTOR ( 'NONE', #826, 999.9999999999998863 ) ;
#56291 = ORIENTED_EDGE ( 'NONE', *, *, #40621, .F. ) ;
#56292 = AXIS2_PLACEMENT_3D ( 'NONE', #44082, #36611, #75086 ) ;
#56293 = CARTESIAN_POINT ( 'NONE',  ( 0.5774900079438607392, 63.48035201082149825, 5.440088680355550821 ) ) ;
#56295 = CARTESIAN_POINT ( 'NONE',  ( 12.91533473730993009, 36.60535201082151247, -10.88017736071109987 ) ) ;
#56294 = CARTESIAN_POINT ( 'NONE',  ( 14.92337183194729633, 42.67559781766745886, 8.527530157486181039 ) ) ;
#56296 = FACE_OUTER_BOUND ( 'NONE', #62310, .T. ) ;
#56297 = AXIS2_PLACEMENT_3D ( 'NONE', #97387, #4901, #89859 ) ;
#56298 = CARTESIAN_POINT ( 'NONE',  ( -0.8801773607111008646, 43.27201867748817676, 2.915334737309923430 ) ) ;
#56300 = CARTESIAN_POINT ( 'NONE',  ( 20.10493008474206889, 59.71697413083878558, 6.336235997365758266 ) ) ;
#56299 = CARTESIAN_POINT ( 'NONE',  ( 20.88017736071110164, 10.35535201082150714, 2.915334737309930979 ) ) ;
#56301 = CARTESIAN_POINT ( 'NONE',  ( -15.81765804549835330, 15.00000000000000000, -2.383084218347030880 ) ) ;
#56302 =( GEOMETRIC_REPRESENTATION_CONTEXT ( 3 ) GLOBAL_UNCERTAINTY_ASSIGNED_CONTEXT ( ( #55090 ) ) GLOBAL_UNIT_ASSIGNED_CONTEXT ( ( #4591, #34067, #35053 ) ) REPRESENTATION_CONTEXT ( 'NONE', 'WORKASPACE' ) );
#56303 = CARTESIAN_POINT ( 'NONE',  ( 7.361572987183170547, 37.05059781766744464, 9.846743663894590881 ) ) ;
#56304 = CARTESIAN_POINT ( 'NONE',  ( -4.164238869374099927, 37.01208216824731068, 3.795296366450308767 ) ) ;
#56305 = CARTESIAN_POINT ( 'NONE',  ( 1.274849032794306947, 7.555090184799359676, -6.499999999999997335 ) ) ;
#56306 = CARTESIAN_POINT ( 'NONE',  ( -4.164238869374099039, 21.80374883491396787, 8.674139862899312516E-16 ) ) ;
#56307 = DIRECTION ( 'NONE',  ( -1.000000000000000000, 0.000000000000000000, -0.000000000000000000 ) ) ;
#56308 = ORIENTED_EDGE ( 'NONE', *, *, #5536, .F. ) ;
#56309 = CARTESIAN_POINT ( 'NONE',  ( -2.266590686148945544, 66.38708216824730357, -7.082119434687050408 ) ) ;
#56310 = CARTESIAN_POINT ( 'NONE',  ( 7.361572987183169658, 29.96726448433411960, -9.846743663894592657 ) ) ;
#56312 = CYLINDRICAL_SURFACE ( 'NONE', #78996, 0.2500000000000002220 ) ;
#56311 = CARTESIAN_POINT ( 'NONE',  ( -6.761389522993972001, 14.76930270348881180, 13.32372569557295527 ) ) ;
#56313 = CARTESIAN_POINT ( 'NONE',  ( -0.8801773607111009756, 63.06368534415484106, 1.068504757029289695E-15 ) ) ;
#56314 = CARTESIAN_POINT ( 'NONE',  ( 14.17193700899790265, 0.000000000000000000, -1.489530601564018175 ) ) ;
#56315 = CARTESIAN_POINT ( 'NONE',  ( 17.96484262340118221, 26.18868534415483396, -7.964842623401177768 ) ) ;
#56316 = CARTESIAN_POINT ( 'NONE',  ( 16.40814093676323893, 55.79030133659708923, 11.09922568453595026 ) ) ;
#56317 = CARTESIAN_POINT ( 'NONE',  ( 22.81628187352647785, 11.62363466993042138, 6.195893100308588602E-16 ) ) ;
#56318 = CARTESIAN_POINT ( 'NONE',  ( 5.076628168052704559, 10.17559781766745175, -8.527530157486179263 ) ) ;
#56319 = VERTEX_POINT ( 'NONE', #32023 ) ;
#56320 = CARTESIAN_POINT ( 'NONE',  ( 7.361572987183169658, -0.03273551566588185635, -9.846743663894592657 ) ) ;
#56321 = DIRECTION ( 'NONE',  ( -0.9981347984218673641, 0.000000000000000000, 0.06104853953484969120 ) ) ;
#56322 = CARTESIAN_POINT ( 'NONE',  ( 24.16423886937409904, 59.09541550158063217, 3.795296366450317205 ) ) ;
#56323 = CIRCLE ( 'NONE', #61090, 1.000000000000000888 ) ;
#56324 = CARTESIAN_POINT ( 'NONE',  ( 6.204703633549690345, 27.84541550158063217, 14.16423886937410082 ) ) ;
#56325 = CARTESIAN_POINT ( 'NONE',  ( 2.035157376598822676, 32.43868534415483396, -7.964842623401177768 ) ) ;
#56326 = CARTESIAN_POINT ( 'NONE',  ( 20.88017736071110164, 50.35535201082151247, 2.915334737309930979 ) ) ;
#56327 = CARTESIAN_POINT ( 'NONE',  ( 17.39651004071842166, 12.93575266056827822, 6.499999999999998224 ) ) ;
#56328 = DIRECTION ( 'NONE',  ( 0.6755902076156493630, 0.000000000000000000, 0.7372773368101340763 ) ) ;
#56329 = CARTESIAN_POINT ( 'NONE',  ( 7.361572987183170547, 12.05059781766744997, 9.846743663894590881 ) ) ;
#56330 = DIRECTION ( 'NONE',  ( 0.5547001962252290364, 0.8320502943378437211, 0.000000000000000000 ) ) ;
#56331 = CARTESIAN_POINT ( 'NONE',  ( 5.076628168052704559, 20.17559781766745175, -8.527530157486179263 ) ) ;
#56332 = CARTESIAN_POINT ( 'NONE',  ( -14.88232117145538069, 14.49999999999999112, 1.875237731503072158 ) ) ;
#56333 = CARTESIAN_POINT ( 'NONE',  ( 12.63842701281683922, 19.55059781766745175, -9.846743663894590881 ) ) ;
#56334 = CARTESIAN_POINT ( 'NONE',  ( 14.92337183194729633, 47.67559781766745175, 8.527530157486181039 ) ) ;
#56335 = ADVANCED_FACE ( 'NONE', ( #86533 ), #21911, .T. ) ;
#56336 = CARTESIAN_POINT ( 'NONE',  ( 15.44008868035555260, 24.73035201082150891, 9.422509992056143702 ) ) ;
#56337 = AXIS2_PLACEMENT_3D ( 'NONE', #96859, #50843, #96362 ) ;
#56338 = CARTESIAN_POINT ( 'NONE',  ( 0.6178305044545818747, 48.49863466993042493, -9.382169495545419124 ) ) ;
#56339 = CARTESIAN_POINT ( 'NONE',  ( 17.96484262340118221, 54.93868534415484106, 7.964842623401181321 ) ) ;
#56340 = CARTESIAN_POINT ( 'NONE',  ( 18.52753015748617571, 28.09226448433411960, 4.923371831947298993 ) ) ;
#56342 = CARTESIAN_POINT ( 'NONE',  ( 19.84674366389459266, 23.71726448433412315, -2.638427012816827677 ) ) ;
#56341 = CARTESIAN_POINT ( 'NONE',  ( 2.917880565312950480, 50.97041550158064638, -12.26659068614894821 ) ) ;
#56343 = CARTESIAN_POINT ( 'NONE',  ( -10.09048698379360687, 46.92328126389585208, 2.899999999999999467 ) ) ;
#56344 = CARTESIAN_POINT ( 'NONE',  ( 10.00000000000000178, 57.25893115100078745, 9.846743663894594434 ) ) ;
#56345 = CARTESIAN_POINT ( 'NONE',  ( 13.79529636645031943, 5.345415501580634832, -14.16423886937409904 ) ) ;
#56346 = CARTESIAN_POINT ( 'NONE',  ( -4.164238869374098151, 26.59541550158063217, -3.795296366450310543 ) ) ;
#56347 = CARTESIAN_POINT ( 'NONE',  ( 1.472469842513823179, 30.59226448433411960, -4.923371831947296329 ) ) ;
#56348 = CARTESIAN_POINT ( 'NONE',  ( 17.96484262340118221, 29.93868534415484106, 7.964842623401181321 ) ) ;
#56349 = CARTESIAN_POINT ( 'NONE',  ( 20.88017736071110164, 50.35535201082151247, 2.915334737309930979 ) ) ;
#56350 = CARTESIAN_POINT ( 'NONE',  ( 10.00000000000000178, 49.31368534415484106, 10.88017736071110342 ) ) ;
#56351 = ORIENTED_EDGE ( 'NONE', *, *, #11446, .F. ) ;
#56352 = CARTESIAN_POINT ( 'NONE',  ( 3.591859063236761518, 34.95696800326375353, 11.09922568453594849 ) ) ;
#56353 = CARTESIAN_POINT ( 'NONE',  ( 10.00000000000000000, 56.81368534415484106, -10.88017736071110342 ) ) ;
#56354 = ORIENTED_EDGE ( 'NONE', *, *, #90440, .F. ) ;
#56355 = CARTESIAN_POINT ( 'NONE',  ( 0.000000000000000000, 15.00000000000000000, 0.000000000000000000 ) ) ;
#56356 = CARTESIAN_POINT ( 'NONE',  ( 4.559911319644449179, 63.89701867748817676, 9.422509992056141925 ) ) ;
#56357 = PRESENTATION_LAYER_ASSIGNMENT (  '', '', ( #3684 ) ) ;
#56358 = VERTEX_POINT ( 'NONE', #94022 ) ;
#56359 = CARTESIAN_POINT ( 'NONE',  ( 2.035157376598824452, 58.68868534415482685, 7.964842623401179544 ) ) ;
#56360 = LINE ( 'NONE', #34313, #84911 ) ;
#56361 = EDGE_CURVE ( 'NONE', #53936, #2342, #43958, .T. ) ;
#56362 = CARTESIAN_POINT ( 'NONE',  ( 19.72487221294570858, 69.50000000000000000, -6.500000000000000888 ) ) ;
#56363 = CARTESIAN_POINT ( 'NONE',  ( 14.29730467489533652, 15.00000000000000000, -2.416004766803220072 ) ) ;
#56364 = CARTESIAN_POINT ( 'NONE',  ( -0.3689425029237881626, 67.42874883491396076, 10.36894250292379027 ) ) ;
#56365 = CARTESIAN_POINT ( 'NONE',  ( 14.92337183194729633, 7.675597817667451750, 8.527530157486181039 ) ) ;
#56366 = CARTESIAN_POINT ( 'NONE',  ( -4.164238869374099927, 2.012082168247300906, 3.795296366450308767 ) ) ;
#56367 = CARTESIAN_POINT ( 'NONE',  ( 12.63842701281683034, 7.467264484334118713, 9.846743663894596210 ) ) ;
#56368 = AXIS2_PLACEMENT_3D ( 'NONE', #94033, #55550, #86050 ) ;
#56369 = CARTESIAN_POINT ( 'NONE',  ( 4.559911319644449179, 8.897018677488171434, 9.422509992056141925 ) ) ;
#56370 = CARTESIAN_POINT ( 'NONE',  ( 17.20831665107776587, 49.13393115100078745, -7.208316651077762316 ) ) ;
#56371 = VERTEX_POINT ( 'NONE', #26995 ) ;
#56372 = TOROIDAL_SURFACE ( 'NONE', #78769, 6.599999999999995204, 0.2500000000000000000 ) ;
#56373 = CARTESIAN_POINT ( 'NONE',  ( 17.20831665107776587, 54.13393115100079456, -7.208316651077762316 ) ) ;
#56374 = VERTEX_POINT ( 'NONE', #88985 ) ;
#56375 = CARTESIAN_POINT ( 'NONE',  ( 0.000000000000000000, 0.5000000000000004441, 0.000000000000000000 ) ) ;
#56376 = AXIS2_PLACEMENT_3D ( 'NONE', #20551, #29504, #74524 ) ;
#56377 = CARTESIAN_POINT ( 'NONE',  ( 10.00000000000000178, 49.31368534415484106, 10.88017736071110342 ) ) ;
#56378 = CARTESIAN_POINT ( 'NONE',  ( 10.00000000000000178, 57.25893115100078745, 9.846743663894594434 ) ) ;
#56380 = CARTESIAN_POINT ( 'NONE',  ( 20.03743638938529870, 1.751975280310174465, 6.399506433553883156 ) ) ;
#56379 = PLANE ( 'NONE',  #11602 ) ;
#56381 = CARTESIAN_POINT ( 'NONE',  ( 17.96484262340118221, 56.18868534415484817, -7.964842623401177768 ) ) ;
#56382 = CARTESIAN_POINT ( 'NONE',  ( 20.88017736071110519, 5.563685344154838397, 2.639326808657452039E-16 ) ) ;
#56383 = CARTESIAN_POINT ( 'NONE',  ( 22.81628187352647785, 41.41530133659708923, 3.434112377981063169 ) ) ;
#56384 = CARTESIAN_POINT ( 'NONE',  ( -0.1023957841222606496, 10.13377557478296254, 6.340343622311898741 ) ) ;
#56385 = ORIENTED_EDGE ( 'NONE', *, *, #57768, .T. ) ;
#56386 = CARTESIAN_POINT ( 'NONE',  ( 6.565887622018943937, 35.16530133659708923, 12.81628187352647430 ) ) ;
#56387 = CARTESIAN_POINT ( 'NONE',  ( -0.8801773607111009756, 33.06368534415484106, 1.068504757029289695E-15 ) ) ;
#56388 = EDGE_LOOP ( 'NONE', ( #6010, #78370, #77059, #77253 ) ) ;
#56389 = CIRCLE ( 'NONE', #24425, 0.5000000000000004441 ) ;
#56390 = EDGE_CURVE ( 'NONE', #63645, #51757, #90546, .T. ) ;
#56391 = CARTESIAN_POINT ( 'NONE',  ( 12.63842701281683034, 62.46726448433410894, 9.846743663894596210 ) ) ;
#56393 = CARTESIAN_POINT ( 'NONE',  ( 5.076628168052703671, 56.84226448433412315, 8.527530157486179263 ) ) ;
#56392 = CARTESIAN_POINT ( 'NONE',  ( 2.791683348922237240, 10.38393115100078390, -7.208316651077763204 ) ) ;
#56394 = CARTESIAN_POINT ( 'NONE',  ( -11.58473852101197998, -69.55955830444820265, 3.750000000000000444 ) ) ;
#56395 = PRESENTATION_STYLE_ASSIGNMENT (( #95364 ) ) ;
#56396 = CARTESIAN_POINT ( 'NONE',  ( -14.26139399674453578, 15.00000000000000000, -2.619664342929994838 ) ) ;
#56397 = CARTESIAN_POINT ( 'NONE',  ( 0.000000000000000000, 14.49999999999999822, 0.000000000000000000 ) ) ;
#56398 = CIRCLE ( 'NONE', #83525, 15.00000000000000000 ) ;
#56399 = ADVANCED_FACE ( 'NONE', ( #49493 ), #4348, .T. ) ;
#56400 = CARTESIAN_POINT ( 'NONE',  ( 19.84674366389459266, 23.71726448433412315, -2.638427012816827677 ) ) ;
#56402 = VERTEX_POINT ( 'NONE', #73971 ) ;
#56401 = CARTESIAN_POINT ( 'NONE',  ( 5.076628168052704559, 60.17559781766745175, -8.527530157486179263 ) ) ;
#56403 = VECTOR ( 'NONE', #25898, 1000.000000000000114 ) ;
#56404 = CARTESIAN_POINT ( 'NONE',  ( 1.274849032794116210, 8.572280503510292249, 6.499999999999738876 ) ) ;
#56405 = CARTESIAN_POINT ( 'NONE',  ( 10.00000000000000178, 20.37363466993042138, 12.81628187352647608 ) ) ;
#56406 = CARTESIAN_POINT ( 'NONE',  ( 12.63842701281683034, 42.46726448433412315, 9.846743663894596210 ) ) ;
#56407 = CARTESIAN_POINT ( 'NONE',  ( -1.796787675079083879, 14.76984984742152385, -14.83218748772994466 ) ) ;
#56408 = CARTESIAN_POINT ( 'NONE',  ( 6.204703633549690345, 50.76208216824730357, -14.16423886937410259 ) ) ;
#56409 = CARTESIAN_POINT ( 'NONE',  ( 10.00000000000000178, 12.25893115100078568, 9.846743663894594434 ) ) ;
#56410 = EDGE_LOOP ( 'NONE', ( #60960, #23426, #60579, #59085 ) ) ;
#56411 = LINE ( 'NONE', #80384, #24888 ) ;
#56412 = CARTESIAN_POINT ( 'NONE',  ( 6.204703633549690345, 62.84541550158063927, 14.16423886937410082 ) ) ;
#56413 = CARTESIAN_POINT ( 'NONE',  ( 1.472469842513823179, 56.42559781766745886, 4.923371831947296329 ) ) ;
#56414 = CARTESIAN_POINT ( 'NONE',  ( 0.5774900079438590739, 7.647018677488171434, -5.440088680355550821 ) ) ;
#56415 = CARTESIAN_POINT ( 'NONE',  ( 2.917880565312950480, 35.97041550158063217, -12.26659068614894821 ) ) ;
#56417 = CARTESIAN_POINT ( 'NONE',  ( 18.04007052943794776, 34.00257860105345742, -5.767676674365461942 ) ) ;
#56416 = CARTESIAN_POINT ( 'NONE',  ( 17.08211943468705130, 33.47041550158063927, 12.26659068614894998 ) ) ;
#56418 = CARTESIAN_POINT ( 'NONE',  ( 0.2751277870542913062, 29.36607318730131411, -6.499999999999992006 ) ) ;
#56420 = CARTESIAN_POINT ( 'NONE',  ( 2.791683348922240793, 51.63393115100078745, 7.208316651077764092 ) ) ;
#56419 = CARTESIAN_POINT ( 'NONE',  ( 6.829574850505125028, -88.00372650098204019, 2.750000000000000888 ) ) ;
#56421 = VERTEX_POINT ( 'NONE', #57001 ) ;
#56422 = CARTESIAN_POINT ( 'NONE',  ( 20.88017736071110875, 40.77201867748818387, -2.915334737309920765 ) ) ;
#56423 = CARTESIAN_POINT ( 'NONE',  ( -12.34597252984326765, 0.04962896562384137150, -8.076773567935994436 ) ) ;
#56424 = CARTESIAN_POINT ( 'NONE',  ( -3.750000000000000000, 36.75000000000000000, 2.750000000000000000 ) ) ;
#56425 = CARTESIAN_POINT ( 'NONE',  ( 18.52753015748617571, 53.09226448433412315, 4.923371831947298993 ) ) ;
#56426 = CARTESIAN_POINT ( 'NONE',  ( 20.15039907845753930, 9.722660991849181755, 6.262539305110064625 ) ) ;
#56427 = CARTESIAN_POINT ( 'NONE',  ( -14.16423886937410082, 1.803748834913972088, 4.336808689942017736E-15 ) ) ;
#56428 = CARTESIAN_POINT ( 'NONE',  ( 12.63842701281683034, 57.46726448433411605, 9.846743663894596210 ) ) ;
#56429 = DIRECTION ( 'NONE',  ( 1.000000000000000000, 0.000000000000000000, 0.000000000000000000 ) ) ;
#56430 = ORIENTED_EDGE ( 'NONE', *, *, #87605, .T. ) ;
#56431 = CARTESIAN_POINT ( 'NONE',  ( 24.16423886937410614, 29.51208216824729647, -3.795296366450302550 ) ) ;
#56432 = CARTESIAN_POINT ( 'NONE',  ( 2.815433093577024426, 0.5000000000000004441, 14.73340885523751709 ) ) ;
#56434 = AXIS2_PLACEMENT_3D ( 'NONE', #39683, #22217, #93149 ) ;
#56433 = CARTESIAN_POINT ( 'NONE',  ( 17.96484262340118221, 14.93868534415484106, 7.964842623401181321 ) ) ;
#56435 = CARTESIAN_POINT ( 'NONE',  ( 3.591859063236763294, 23.29030133659708568, -11.09922568453595026 ) ) ;
#56436 = CARTESIAN_POINT ( 'NONE',  ( -11.92686044187655980, 9.896642702460841434, 3.195792623639539087 ) ) ;
#56437 = CARTESIAN_POINT ( 'NONE',  ( 2.791683348922237240, 5.383931151000785675, -7.208316651077763204 ) ) ;
#56438 = VECTOR ( 'NONE', #61439, 1000.000000000000000 ) ;
#56439 = FACE_OUTER_BOUND ( 'NONE', #88700, .T. ) ;
#56440 = CARTESIAN_POINT ( 'NONE',  ( -1.926860441876563801, 9.896642702460841434, 3.195792623639529761 ) ) ;
#56441 = CARTESIAN_POINT ( 'NONE',  ( 10.00000000000000178, 70.00000000000000000, 0.000000000000000000 ) ) ;
#56442 = CARTESIAN_POINT ( 'NONE',  ( -0.8801773607110991993, 12.85535201082150358, -2.915334737309923874 ) ) ;
#56443 = CARTESIAN_POINT ( 'NONE',  ( -1.354709868695741282, 14.63606900606166228, 14.93870011653154251 ) ) ;
#56444 = CARTESIAN_POINT ( 'NONE',  ( 12.91533473730992121, 44.52201867748816966, 10.88017736071110164 ) ) ;
#56445 = CARTESIAN_POINT ( 'NONE',  ( 7.084665262690076126, 32.02201867748816966, -10.88017736071110164 ) ) ;
#56446 = CARTESIAN_POINT ( 'NONE',  ( 7.361572987183169658, 64.96726448433412315, -9.846743663894592657 ) ) ;
#56447 = CARTESIAN_POINT ( 'NONE',  ( 2.791683348922240793, 61.63393115100079456, 7.208316651077764092 ) ) ;
#56448 = CARTESIAN_POINT ( 'NONE',  ( 6.565887622018943937, 65.16530133659709634, 12.81628187352647430 ) ) ;
#56449 = CARTESIAN_POINT ( 'NONE',  ( 0.1532563361054083140, 6.008931151000784787, 1.131784320476157264E-15 ) ) ;
#56450 = VERTEX_POINT ( 'NONE', #87502 ) ;
#56451 = CARTESIAN_POINT ( 'NONE',  ( 15.44008868035555793, 26.39701867748817321, -9.422509992056140149 ) ) ;
#56452 = ADVANCED_FACE ( 'NONE', ( #12487 ), #4900, .T. ) ;
#56453 = CARTESIAN_POINT ( 'NONE',  ( 16.40814093676324603, 27.45696800326375708, -11.09922568453594671 ) ) ;
#56454 = UNCERTAINTY_MEASURE_WITH_UNIT (LENGTH_MEASURE( 1.000000000000000082E-05 ), #43913, 'distance_accuracy_value', 'NONE');
#56455 = CARTESIAN_POINT ( 'NONE',  ( 0.1532563361054083140, 66.00893115100079456, 1.131784320476157264E-15 ) ) ;
#56456 = CARTESIAN_POINT ( 'NONE',  ( 4.559911319644449179, 68.89701867748817676, 9.422509992056141925 ) ) ;
#56457 = CARTESIAN_POINT ( 'NONE',  ( 17.20831665107776587, 14.13393115100078568, -7.208316651077762316 ) ) ;
#56458 = CARTESIAN_POINT ( 'NONE',  ( -1.099225684535947600, 33.70696800326375353, -6.408140936763238038 ) ) ;
#56459 = CARTESIAN_POINT ( 'NONE',  ( 5.076628168052704559, 5.175597817667451750, -8.527530157486179263 ) ) ;
#56460 = ORIENTED_EDGE ( 'NONE', *, *, #65647, .T. ) ;
#56461 = DIRECTION ( 'NONE',  ( 0.04361938736533305799, 0.000000000000000000, 0.9990482215818579093 ) ) ;
#56462 = CARTESIAN_POINT ( 'NONE',  ( -0.8801773607111009756, 13.06368534415483929, 1.068504757029289695E-15 ) ) ;
#56464 = CARTESIAN_POINT ( 'NONE',  ( -4.164238869374099039, 26.80374883491397142, 8.674139862899312516E-16 ) ) ;
#56463 = CARTESIAN_POINT ( 'NONE',  ( 16.40814093676323893, 60.79030133659709634, 11.09922568453595026 ) ) ;
#56465 = CARTESIAN_POINT ( 'NONE',  ( 2.791683348922240793, 16.63393115100078745, 7.208316651077764092 ) ) ;
#56466 = CARTESIAN_POINT ( 'NONE',  ( 15.44008868035555260, 9.730352010821505360, 9.422509992056143702 ) ) ;
#56467 = CARTESIAN_POINT ( 'NONE',  ( 14.92337183194729633, 27.67559781766745530, 8.527530157486181039 ) ) ;
#56468 = CARTESIAN_POINT ( 'NONE',  ( -0.3689425029237881626, 62.42874883491396787, 10.36894250292379027 ) ) ;
#56469 = ORIENTED_EDGE ( 'NONE', *, *, #34646, .T. ) ;
#56470 = CARTESIAN_POINT ( 'NONE',  ( 20.88017736071110164, 10.35535201082150714, 2.915334737309930979 ) ) ;
#56471 = CARTESIAN_POINT ( 'NONE',  ( 20.88017736071110164, 15.35535201082150358, 2.915334737309930979 ) ) ;
#56472 = EDGE_LOOP ( 'NONE', ( #12558, #65954, #75544, #97661 ) ) ;
#56473 = CARTESIAN_POINT ( 'NONE',  ( 2.791683348922237240, 65.38393115100078035, -7.208316651077763204 ) ) ;
#56474 = CARTESIAN_POINT ( 'NONE',  ( 10.00000000000000000, 21.81368534415484106, -10.88017736071110342 ) ) ;
#56475 = CARTESIAN_POINT ( 'NONE',  ( 0.1532563361054083140, 51.00893115100078745, 1.131784320476157264E-15 ) ) ;
#56476 = DIRECTION ( 'NONE',  ( -1.000000000000000000, 0.000000000000000000, 0.000000000000000000 ) ) ;
#56477 = ADVANCED_FACE ( 'NONE', ( #53953 ), #90954, .T. ) ;
#56478 = CARTESIAN_POINT ( 'NONE',  ( 16.40814093676324603, 47.45696800326375353, -11.09922568453594671 ) ) ;
#56479 = CARTESIAN_POINT ( 'NONE',  ( 9.879999999999988347, 26.99999999999999645, 2.900000000000000355 ) ) ;
#56480 = CARTESIAN_POINT ( 'NONE',  ( -2.266590686148945544, 16.38708216824730357, -7.082119434687050408 ) ) ;
#56481 = CARTESIAN_POINT ( 'NONE',  ( 0.5774900079438607392, 43.48035201082151247, 5.440088680355550821 ) ) ;
#56482 = CARTESIAN_POINT ( 'NONE',  ( 17.96484262340118221, 11.18868534415484106, -7.964842623401177768 ) ) ;
#56483 = CARTESIAN_POINT ( 'NONE',  ( 12.63842701281683034, 52.46726448433413026, 9.846743663894596210 ) ) ;
#56484 = CARTESIAN_POINT ( 'NONE',  ( 0.000000000000000000, 15.00000000000000000, 0.000000000000000000 ) ) ;
#56485 = CARTESIAN_POINT ( 'NONE',  ( 2.791683348922240793, 41.63393115100078745, 7.208316651077764092 ) ) ;
#56486 = EDGE_CURVE ( 'NONE', #65885, #47390, #38960, .T. ) ;
#56487 = CARTESIAN_POINT ( 'NONE',  ( 10.00000000000000178, 7.258931151000785675, 9.846743663894594434 ) ) ;
#56488 = CARTESIAN_POINT ( 'NONE',  ( -12.81628187352647252, -35.66803199673624647, 3.434112377981066722 ) ) ;
#56489 = ORIENTED_EDGE ( 'NONE', *, *, #42248, .T. ) ;
#56490 = CARTESIAN_POINT ( 'NONE',  ( 10.00000000000000000, 11.81368534415483751, -10.88017736071110342 ) ) ;
#56491 = CARTESIAN_POINT ( 'NONE',  ( 18.52753015748617571, 18.09226448433411960, 4.923371831947298993 ) ) ;
#56492 = CARTESIAN_POINT ( 'NONE',  ( 1.472469842513823179, 66.42559781766745175, 4.923371831947296329 ) ) ;
#56493 = CARTESIAN_POINT ( 'NONE',  ( 7.084665262690076126, 44.10535201082151247, 10.88017736071109987 ) ) ;
#56495 = CARTESIAN_POINT ( 'NONE',  ( 6.565887622018943937, 50.16530133659708213, 12.81628187352647430 ) ) ;
#56494 = CARTESIAN_POINT ( 'NONE',  ( 7.084665262690076126, 14.10535201082150358, 10.88017736071109987 ) ) ;
#56496 = CARTESIAN_POINT ( 'NONE',  ( -4.164238869374099039, 36.80374883491396787, 8.674139862899312516E-16 ) ) ;
#56497 = DIRECTION ( 'NONE',  ( 1.000000000000000000, 0.000000000000000000, 0.000000000000000000 ) ) ;
#56498 = STYLED_ITEM ( 'NONE', ( #34779 ), #96951 ) ;
#56499 = CARTESIAN_POINT ( 'NONE',  ( 22.81628187352648496, 61.83196800326376774, -3.434112377981050290 ) ) ;
#56500 = ORIENTED_EDGE ( 'NONE', *, *, #23303, .T. ) ;
#56501 = CARTESIAN_POINT ( 'NONE',  ( 19.84674366389459266, 63.30059781766745886, 2.638427012816836559 ) ) ;
#56502 = CARTESIAN_POINT ( 'NONE',  ( 10.00000000000000178, 34.31368534415484106, 10.88017736071110342 ) ) ;
#56503 = AXIS2_PLACEMENT_3D ( 'NONE', #31684, #32670, #47176 ) ;
#56504 = ORIENTED_EDGE ( 'NONE', *, *, #44715, .T. ) ;
#56506 = CARTESIAN_POINT ( 'NONE',  ( -0.1503990784575328643, 65.12777174578613426, 6.262539305110068177 ) ) ;
#56505 = CARTESIAN_POINT ( 'NONE',  ( 0.1532563361054100626, 0.8005978176674514168, -2.638427012816831230 ) ) ;
#56507 = CARTESIAN_POINT ( 'NONE',  ( -46.20903833114419967, 103.7402771300235713, 6.114030023718175499 ) ) ;
#56508 = CARTESIAN_POINT ( 'NONE',  ( 2.791683348922237240, 10.38393115100078390, -7.208316651077763204 ) ) ;
#56509 = CARTESIAN_POINT ( 'NONE',  ( 17.20831665107776587, 29.13393115100078390, -7.208316651077762316 ) ) ;
#56510 = CARTESIAN_POINT ( 'NONE',  ( 0.1532563361054100626, 10.80059781766745175, -2.638427012816831230 ) ) ;
#56511 = CARTESIAN_POINT ( 'NONE',  ( 7.361572987183170547, 7.050597817667451750, 9.846743663894590881 ) ) ;
#56512 = EDGE_CURVE ( 'NONE', #96626, #64701, #21997, .T. ) ;
#56513 = CARTESIAN_POINT ( 'NONE',  ( 15.44008868035555793, 51.39701867748816966, -9.422509992056140149 ) ) ;
#56514 = CARTESIAN_POINT ( 'NONE',  ( 10.00000000000000000, 61.81368534415484106, -10.88017736071110342 ) ) ;
#56516 = VERTEX_POINT ( 'NONE', #74978 ) ;
#56515 = CARTESIAN_POINT ( 'NONE',  ( 12.63842701281683034, 22.46726448433411605, 9.846743663894596210 ) ) ;
#56517 = CARTESIAN_POINT ( 'NONE',  ( 1.274849032794294290, 63.57228050351031357, 6.499999999999979572 ) ) ;
#56518 = CARTESIAN_POINT ( 'NONE',  ( 18.52753015748617571, 58.09226448433411605, 4.923371831947298993 ) ) ;
#56519 = VERTEX_POINT ( 'NONE', #52960 ) ;
#56520 = ORIENTED_EDGE ( 'NONE', *, *, #66707, .T. ) ;
#56521 = CARTESIAN_POINT ( 'NONE',  ( 9.159723438033203990, -0.03417435944610275333, -10.91613331444542645 ) ) ;
#56522 = CARTESIAN_POINT ( 'NONE',  ( 2.917880565312950480, 10.97041550158063572, -12.26659068614894821 ) ) ;
#56523 = UNCERTAINTY_MEASURE_WITH_UNIT (LENGTH_MEASURE( 1.000000000000000082E-05 ), #17464, 'distance_accuracy_value', 'NONE');
#56524 = DIRECTION ( 'NONE',  ( -0.9832549075639550606, 0.000000000000000000, 0.1822355254921448342 ) ) ;
#56525 = SURFACE_STYLE_FILL_AREA ( #81711 ) ;
#56526 = CARTESIAN_POINT ( 'NONE',  ( 22.26659068614894466, 28.88708216824730357, 7.082119434687054849 ) ) ;
#56527 = CARTESIAN_POINT ( 'NONE',  ( -2.266590686148945544, 1.387082168247301128, -7.082119434687050408 ) ) ;
#56528 = CARTESIAN_POINT ( 'NONE',  ( 0.5774900079438607392, 33.48035201082150536, 5.440088680355550821 ) ) ;
#56529 = ORIENTED_EDGE ( 'NONE', *, *, #7710, .T. ) ;
#56530 = CARTESIAN_POINT ( 'NONE',  ( 14.92337183194729633, 12.67559781766745353, 8.527530157486181039 ) ) ;
#56532 = CARTESIAN_POINT ( 'NONE',  ( 18.52753015748618282, 18.92559781766745175, -4.923371831947291888 ) ) ;
#56531 = CARTESIAN_POINT ( 'NONE',  ( 20.88017736071110164, 50.35535201082151247, 2.915334737309930979 ) ) ;
#56533 = CARTESIAN_POINT ( 'NONE',  ( 10.00000000000000178, 40.37363466993042493, 12.81628187352647608 ) ) ;
#56534 = CARTESIAN_POINT ( 'NONE',  ( 18.52753015748617571, 38.09226448433412315, 4.923371831947298993 ) ) ;
#56535 = CARTESIAN_POINT ( 'NONE',  ( 11.62112565934149089, -4.031876828930466656E-16, -8.881879596174739433 ) ) ;
#56536 = CARTESIAN_POINT ( 'NONE',  ( 19.42250999205614193, 60.14701867748817676, 5.440088680355555262 ) ) ;
#56537 = CARTESIAN_POINT ( 'NONE',  ( 3.591859063236761518, 24.95696800326375353, 11.09922568453594849 ) ) ;
#56538 = CARTESIAN_POINT ( 'NONE',  ( -10.36894250292379205, -33.82125116508603213, -10.36894250292378672 ) ) ;
#56539 = CARTESIAN_POINT ( 'NONE',  ( 18.52753015748618282, 23.92559781766745530, -4.923371831947291888 ) ) ;
#56540 = CARTESIAN_POINT ( 'NONE',  ( 13.79529636645030344, 13.26208216824729824, 14.16423886937410614 ) ) ;
#56541 = CARTESIAN_POINT ( 'NONE',  ( 0.5774900079438590739, 37.64701867748817676, -5.440088680355550821 ) ) ;
#56542 = CARTESIAN_POINT ( 'NONE',  ( 10.00000000000000178, 38.05374883491396787, 14.16423886937410082 ) ) ;
#56543 = CARTESIAN_POINT ( 'NONE',  ( 1.472469842513823179, 55.59226448433412315, -4.923371831947296329 ) ) ;
#56544 = EDGE_CURVE ( 'NONE', #18106, #63974, #14497, .T. ) ;
#56545 = CARTESIAN_POINT ( 'NONE',  ( 0.1532563361054083140, 11.00893115100078568, 1.131784320476157264E-15 ) ) ;
#56547 = DIRECTION ( 'NONE',  ( -0.000000000000000000, -0.000000000000000000, -1.000000000000000000 ) ) ;
#56546 = DIRECTION ( 'NONE',  ( 0.8070303256584298035, -0.5905099943842175847, 0.000000000000000000 ) ) ;
#56548 = CARTESIAN_POINT ( 'NONE',  ( 20.88017736071110519, 45.56368534415484106, 2.639326808657452039E-16 ) ) ;
#56549 = CARTESIAN_POINT ( 'NONE',  ( 9.879999999999991900, 20.99999999999999645, 0.000000000000000000 ) ) ;
#56550 = CARTESIAN_POINT ( 'NONE',  ( 22.81628187352648496, 26.83196800326374998, -3.434112377981050290 ) ) ;
#56551 = CARTESIAN_POINT ( 'NONE',  ( 0.1532563361054100626, 60.80059781766744464, -2.638427012816831230 ) ) ;
#56552 = B_SPLINE_CURVE_WITH_KNOTS ( 'NONE', 3,
 ( #3045, #55027, #49011, #72002, #26503, #78038 ),
 .UNSPECIFIED., .F., .F.,
 ( 4, 2, 4 ),
 ( 3.409110551494646011E-05, 0.0004400426677367931852, 0.0008459942299586398901 ),
 .UNSPECIFIED. ) ;
#56553 = CARTESIAN_POINT ( 'NONE',  ( -9.422509992056136596, 8.480352010821514241, 5.440088680355559703 ) ) ;
#56554 = CARTESIAN_POINT ( 'NONE',  ( 4.559911319644449179, 2.230352010821504471, -9.422509992056141925 ) ) ;
#56556 = CARTESIAN_POINT ( 'NONE',  ( 38.04706783004212411, 44.99999999999999289, -7.000000000000000000 ) ) ;
#56555 = CARTESIAN_POINT ( 'NONE',  ( 7.084665262690076126, 69.10535201082151957, 10.88017736071109987 ) ) ;
#56557 = CARTESIAN_POINT ( 'NONE',  ( -0.07285406091746288171, 0.4131759111665360140, 9.500000000000000000 ) ) ;
#56558 = EDGE_CURVE ( 'NONE', #65600, #60520, #88913, .T. ) ;
#56559 = CARTESIAN_POINT ( 'NONE',  ( 2.603489959281591659, 15.43575266056827999, -6.500000000000006217 ) ) ;
#56560 = CARTESIAN_POINT ( 'NONE',  ( 19.84674366389459621, 3.508931151000785231, 7.409399052514197653E-17 ) ) ;
#56561 = CARTESIAN_POINT ( 'NONE',  ( 4.559911319644449179, 57.23035201082150536, -9.422509992056141925 ) ) ;
#56562 = CARTESIAN_POINT ( 'NONE',  ( 18.00000000000000000, 77.37581971779152923, -4.190584158844754548 ) ) ;
#56563 = CARTESIAN_POINT ( 'NONE',  ( -14.82269085861170232, 15.00000000000000000, 2.299529454046861154 ) ) ;
#56564 = VECTOR ( 'NONE', #54904, 1000.000000000000000 ) ;
#56565 = CARTESIAN_POINT ( 'NONE',  ( 19.84674366389459266, 23.71726448433412315, -2.638427012816827677 ) ) ;
#56566 = EDGE_CURVE ( 'NONE', #87620, #95286, #42218, .T. ) ;
#56567 = EDGE_CURVE ( 'NONE', #47699, #98676, #71368, .T. ) ;
#56568 = CARTESIAN_POINT ( 'NONE',  ( 10.00000000000000178, 29.31368534415483751, 10.88017736071110342 ) ) ;
#56569 = B_SPLINE_CURVE_WITH_KNOTS ( 'NONE', 3,
 ( #45166, #30152, #37684, #16156, #22189, #22683 ),
 .UNSPECIFIED., .F., .F.,
 ( 4, 2, 4 ),
 ( 0.000000000000000000, 0.0002565770811491002636, 0.0005131541622982005273 ),
 .UNSPECIFIED. ) ;
#56570 = CARTESIAN_POINT ( 'NONE',  ( 22.81628187352647785, 1.623634669930420271, 6.195893100308588602E-16 ) ) ;
#56572 = CARTESIAN_POINT ( 'NONE',  ( -6.867514897637334137, -58.37540146638243499, -3.750000000000000888 ) ) ;
#56571 = CARTESIAN_POINT ( 'NONE',  ( 20.88017736071110164, 25.35535201082150891, 2.915334737309930979 ) ) ;
#56573 = CARTESIAN_POINT ( 'NONE',  ( 5.795997163830076460, 15.00000000000000000, 13.01802277140709663 ) ) ;
#56574 = CARTESIAN_POINT ( 'NONE',  ( 22.81628187352647785, 41.41530133659708923, 3.434112377981063169 ) ) ;
#56575 = VERTEX_POINT ( 'NONE', #55432 ) ;
#56576 = CARTESIAN_POINT ( 'NONE',  ( 20.88017736071110519, 45.56368534415484106, 2.639326808657452039E-16 ) ) ;
#56577 = CARTESIAN_POINT ( 'NONE',  ( 7.361572987183170547, 47.05059781766745175, 9.846743663894590881 ) ) ;
#56578 = AXIS2_PLACEMENT_3D ( 'NONE', #35516, #89016, #11537 ) ;
#56580 = CARTESIAN_POINT ( 'NONE',  ( 3.969999999999999751, 37.25000000000000000, -4.000000000000000000 ) ) ;
#56579 = CARTESIAN_POINT ( 'NONE',  ( 13.43411237798106583, 17.66530133659708923, -12.81628187352647252 ) ) ;
#56581 = CARTESIAN_POINT ( 'NONE',  ( -0.8801773607111008646, 33.27201867748817676, 2.915334737309923430 ) ) ;
#56582 = CARTESIAN_POINT ( 'NONE',  ( 10.00000000000000000, 50.55374883491396787, -14.16423886937410082 ) ) ;
#56583 = CARTESIAN_POINT ( 'NONE',  ( 18.52753015748618282, 43.92559781766745175, -4.923371831947291888 ) ) ;
#56584 = CARTESIAN_POINT ( 'NONE',  ( 0.1532563361054082862, 6.217264484334118713, 2.638427012816831674 ) ) ;
#56585 = CARTESIAN_POINT ( 'NONE',  ( 0.5774900079438590739, 47.64701867748817676, -5.440088680355550821 ) ) ;
#56586 = DIRECTION ( 'NONE',  ( -0.000000000000000000, -1.000000000000000000, -0.000000000000000000 ) ) ;
#56587 = CARTESIAN_POINT ( 'NONE',  ( -0.3689425029237898834, 11.17874883491396787, -10.36894250292378850 ) ) ;
#56588 = DIRECTION ( 'NONE',  ( 1.000000000000000000, 0.000000000000000000, 0.000000000000000000 ) ) ;
#56589 = CARTESIAN_POINT ( 'NONE',  ( 1.492507162822237943, 22.19955587570480660, -6.499999999999988454 ) ) ;
#56590 = ORIENTED_EDGE ( 'NONE', *, *, #72570, .F. ) ;
#56591 = CARTESIAN_POINT ( 'NONE',  ( -0.3689425029237881626, 52.42874883491396076, 10.36894250292379027 ) ) ;
#56592 = CARTESIAN_POINT ( 'NONE',  ( -4.164238869374098151, 56.59541550158063927, -3.795296366450310543 ) ) ;
#56593 = CARTESIAN_POINT ( 'NONE',  ( 10.00000000000000178, 12.25893115100078568, 9.846743663894594434 ) ) ;
#56594 = EDGE_CURVE ( 'NONE', #61056, #79877, #32632, .T. ) ;
#56595 = CARTESIAN_POINT ( 'NONE',  ( 5.795997163830076460, 0.000000000000000000, 13.01802277140709663 ) ) ;
#56596 = CARTESIAN_POINT ( 'NONE',  ( 1.274849032794317383, 27.55509018479935790, -6.500000000000010658 ) ) ;
#56598 = CARTESIAN_POINT ( 'NONE',  ( 16.40814093676323893, 35.79030133659708923, 11.09922568453595026 ) ) ;
#56597 = CARTESIAN_POINT ( 'NONE',  ( 10.00000000000000000, 1.813685344154837731, -10.88017736071110342 ) ) ;
#56599 = CARTESIAN_POINT ( 'NONE',  ( 10.00000000000000178, 48.05374883491396787, 14.16423886937410082 ) ) ;
#56600 = CARTESIAN_POINT ( 'NONE',  ( 4.096035146093531587, 4.098443466602401877E-16, -13.90943910019259278 ) ) ;
#56601 = CARTESIAN_POINT ( 'NONE',  ( 0.5774900079438590739, 67.64701867748817676, -5.440088680355550821 ) ) ;
#56602 = ADVANCED_FACE ( 'NONE', ( #85436 ), #28229, .T. ) ;
#56603 = CARTESIAN_POINT ( 'NONE',  ( -9.846743663894596210, 5.800597817667454414, -2.638427012816824124 ) ) ;
#56604 = ORIENTED_EDGE ( 'NONE', *, *, #89557, .F. ) ;
#56605 = PLANE ( 'NONE',  #53998 ) ;
#56606 = CARTESIAN_POINT ( 'NONE',  ( 7.361572987183170547, 17.05059781766745530, 9.846743663894590881 ) ) ;
#56607 = ORIENTED_EDGE ( 'NONE', *, *, #50672, .F. ) ;
#56609 = CARTESIAN_POINT ( 'NONE',  ( 12.91533473730993009, 6.605352010821504471, -10.88017736071109987 ) ) ;
#56608 = CARTESIAN_POINT ( 'NONE',  ( -4.164238869374099039, 66.80374883491396076, 8.674139862899312516E-16 ) ) ;
#56611 = CARTESIAN_POINT ( 'NONE',  ( 22.81628187352648496, 6.831968003263753531, -3.434112377981050290 ) ) ;
#56610 = CARTESIAN_POINT ( 'NONE',  ( 2.791683348922240793, 46.63393115100077324, 7.208316651077764092 ) ) ;
#56612 = CARTESIAN_POINT ( 'NONE',  ( 10.00000000000000178, 70.00000000000000000, 0.000000000000000000 ) ) ;
#56613 = AXIS2_PLACEMENT_3D ( 'NONE', #12304, #56819, #72792 ) ;
#56614 = CARTESIAN_POINT ( 'NONE',  ( -1.761054936948033278, 12.86682408883346440, 9.500000000000000000 ) ) ;
#56615 = CARTESIAN_POINT ( 'NONE',  ( 0.6178305044545818747, 23.49863466993041783, -9.382169495545419124 ) ) ;
#56616 = ORIENTED_EDGE ( 'NONE', *, *, #10522, .F. ) ;
#56617 = CARTESIAN_POINT ( 'NONE',  ( 20.36894250292379382, 63.67874883491396787, 10.36894250292379205 ) ) ;
#56618 = EDGE_LOOP ( 'NONE', ( #90667, #72424, #70840, #77038 ) ) ;
#56619 = CARTESIAN_POINT ( 'NONE',  ( 10.00000000000000000, 60.55374883491397497, -14.16423886937410082 ) ) ;
#56620 = ORIENTED_EDGE ( 'NONE', *, *, #24297, .F. ) ;
#56621 = CARTESIAN_POINT ( 'NONE',  ( -0.8801773607111009756, 38.06368534415484106, 1.068504757029289695E-15 ) ) ;
#56622 = CARTESIAN_POINT ( 'NONE',  ( 7.084665262690076126, 37.02201867748817676, -10.88017736071110164 ) ) ;
#56623 =( NAMED_UNIT ( * ) PLANE_ANGLE_UNIT ( ) SI_UNIT ( $, .RADIAN. ) );
#56624 = CARTESIAN_POINT ( 'NONE',  ( 10.00000000000000000, 26.81368534415484106, -10.88017736071110342 ) ) ;
#56625 = ADVANCED_FACE ( 'NONE', ( #16945 ), #2459, .T. ) ;
#56626 = DIRECTION ( 'NONE',  ( 0.9999619230641714207, 0.000000000000000000, -0.008726535498360278933 ) ) ;
#56627 =( GEOMETRIC_REPRESENTATION_CONTEXT ( 3 ) GLOBAL_UNCERTAINTY_ASSIGNED_CONTEXT ( ( #42504 ) ) GLOBAL_UNIT_ASSIGNED_CONTEXT ( ( #86783, #94266, #47288 ) ) REPRESENTATION_CONTEXT ( 'NONE', 'WORKASPACE' ) );
#56628 = CARTESIAN_POINT ( 'NONE',  ( 2.791683348922237240, 15.38393115100078212, -7.208316651077763204 ) ) ;
#56629 = ORIENTED_EDGE ( 'NONE', *, *, #71677, .F. ) ;
#56630 = CARTESIAN_POINT ( 'NONE',  ( 9.729341964107060647, -19.62354698957123134, 3.750000000000000000 ) ) ;
#56631 = CARTESIAN_POINT ( 'NONE',  ( 17.20831665107776587, 39.13393115100079456, -7.208316651077762316 ) ) ;
#56632 = VECTOR ( 'NONE', #78431, 1000.000000000000000 ) ;
#56633 = CARTESIAN_POINT ( 'NONE',  ( 18.17884179759845509, 53.66688879859523098, -6.500000000000054179 ) ) ;
#56634 = CARTESIAN_POINT ( 'NONE',  ( 0.6178305044545838731, 54.74863466993042493, 9.382169495545420901 ) ) ;
#56635 = FILL_AREA_STYLE ('',( #96618 ) ) ;
#56636 = ORIENTED_EDGE ( 'NONE', *, *, #35243, .F. ) ;
#56637 = CARTESIAN_POINT ( 'NONE',  ( -45.94000000000000483, 93.00000000000000000, 5.000000000000000000 ) ) ;
#56638 = CARTESIAN_POINT ( 'NONE',  ( 2.962741594152983993, 0.000000000000000000, 13.93860331045674883 ) ) ;
#56639 = CARTESIAN_POINT ( 'NONE',  ( 18.52753015748618282, 63.92559781766745886, -4.923371831947291888 ) ) ;
#56640 = CARTESIAN_POINT ( 'NONE',  ( -4.164238869374099927, 42.01208216824728936, 3.795296366450308767 ) ) ;
#56641 = FACE_OUTER_BOUND ( 'NONE', #78475, .T. ) ;
#56642 = ORIENTED_EDGE ( 'NONE', *, *, #45617, .T. ) ;
#56643 = LINE ( 'NONE', #72610, #4881 ) ;
#56644 = CARTESIAN_POINT ( 'NONE',  ( 0.1532563361054082862, 31.21726448433412315, 2.638427012816831674 ) ) ;
#56645 = CARTESIAN_POINT ( 'NONE',  ( 3.591859063236763294, 63.29030133659708923, -11.09922568453595026 ) ) ;
#56646 = CARTESIAN_POINT ( 'NONE',  ( 16.40814093676324603, 2.456968003263753531, -11.09922568453594671 ) ) ;
#56647 = CARTESIAN_POINT ( 'NONE',  ( 0.5774900079438607392, 63.48035201082149825, 5.440088680355550821 ) ) ;
#56648 = CARTESIAN_POINT ( 'NONE',  ( -10.27191093752546891, 15.00000000000000888, -10.41278984915639683 ) ) ;
#56649 = CARTESIAN_POINT ( 'NONE',  ( 1.472469842513823179, 55.59226448433412315, -4.923371831947296329 ) ) ;
#56650 = FACE_OUTER_BOUND ( 'NONE', #91947, .T. ) ;
#56651 = AXIS2_PLACEMENT_3D ( 'NONE', #75859, #7379, #84838 ) ;
#56652 = ORIENTED_EDGE ( 'NONE', *, *, #21816, .T. ) ;
#56653 = CARTESIAN_POINT ( 'NONE',  ( -0.3689425029237898834, 61.17874883491396076, -10.36894250292378850 ) ) ;
#56654 = DIRECTION ( 'NONE',  ( 1.000000000000000000, 0.000000000000000000, 0.000000000000000000 ) ) ;
#56655 = CARTESIAN_POINT ( 'NONE',  ( 19.42250999205614193, 45.14701867748817676, 5.440088680355555262 ) ) ;
#56657 = CARTESIAN_POINT ( 'NONE',  ( 7.545084738058070783, 12.99794841920399691, -9.011045663943741957 ) ) ;
#56656 = CARTESIAN_POINT ( 'NONE',  ( 3.591859063236761518, 19.95696800326375353, 11.09922568453594849 ) ) ;
#56658 = CARTESIAN_POINT ( 'NONE',  ( 13.55157833323629646, 14.76930270348882068, 6.292279346205477353 ) ) ;
#56659 = CARTESIAN_POINT ( 'NONE',  ( 10.00000000000000000, 44.75893115100078745, -9.846743663894594434 ) ) ;
#56660 = CARTESIAN_POINT ( 'NONE',  ( -12.26659068614894110, 27.22041550158063572, 7.082119434687058401 ) ) ;
#56661 = CARTESIAN_POINT ( 'NONE',  ( 22.81628187352647785, 16.41530133659708923, 3.434112377981063169 ) ) ;
#56662 = CARTESIAN_POINT ( 'NONE',  ( -8.107947183327409491, -3.126532598402040897, -3.750000000000000000 ) ) ;
#56663 = ADVANCED_FACE ( 'NONE', ( #46933 ), #39938, .T. ) ;
#56664 = CARTESIAN_POINT ( 'NONE',  ( -0.8801773607110991993, 22.85535201082150181, -2.915334737309923874 ) ) ;
#56665 = FACE_OUTER_BOUND ( 'NONE', #73673, .T. ) ;
#56666 = CIRCLE ( 'NONE', #4013, 0.1000000000000001166 ) ;
#56667 = CARTESIAN_POINT ( 'NONE',  ( 10.00000000000000000, 40.55374883491397497, -14.16423886937410082 ) ) ;
#56668 = CARTESIAN_POINT ( 'NONE',  ( 22.26659068614894466, 28.88708216824730357, 7.082119434687054849 ) ) ;
#56669 = CARTESIAN_POINT ( 'NONE',  ( 2.035157376598822676, 17.43868534415483751, -7.964842623401177768 ) ) ;
#56670 = CARTESIAN_POINT ( 'NONE',  ( 19.84674366389459621, 38.50893115100078745, 7.409399052514197653E-17 ) ) ;
#56671 = CARTESIAN_POINT ( 'NONE',  ( 19.38216949554541202, 40.99863466993042493, 9.382169495545424454 ) ) ;
#56672 = CARTESIAN_POINT ( 'NONE',  ( 0.5774900079438590739, 7.647018677488171434, -5.440088680355550821 ) ) ;
#56673 = EDGE_CURVE ( 'NONE', #9131, #6299, #10683, .T. ) ;
#56674 = CARTESIAN_POINT ( 'NONE',  ( 14.92337183194729988, 39.34226448433412315, -8.527530157486177487 ) ) ;
#56675 = CARTESIAN_POINT ( 'NONE',  ( 19.42250999205614193, 35.14701867748816966, 5.440088680355555262 ) ) ;
#56676 = CARTESIAN_POINT ( 'NONE',  ( -2.816281873526473856, 9.123634669930421381, 9.499525473075851096E-16 ) ) ;
#56677 = CARTESIAN_POINT ( 'NONE',  ( 20.36894250292379382, 23.67874883491397142, 10.36894250292379205 ) ) ;
#56678 = CARTESIAN_POINT ( 'NONE',  ( -13.78891971893203028, 14.63606857305640574, -5.904717858191753876 ) ) ;
#56679 = EDGE_CURVE ( 'NONE', #65284, #52058, #55301, .T. ) ;
#56680 = CARTESIAN_POINT ( 'NONE',  ( 0.1532563361054083140, 26.00893115100078745, 1.131784320476157264E-15 ) ) ;
#56681 = CARTESIAN_POINT ( 'NONE',  ( -2.816281873526473856, 54.33196800326376064, 3.434112377981055619 ) ) ;
#56682 = CARTESIAN_POINT ( 'NONE',  ( 2.791683348922240793, 51.63393115100078745, 7.208316651077764092 ) ) ;
#56683 = ORIENTED_EDGE ( 'NONE', *, *, #36933, .F. ) ;
#56684 = DIRECTION ( 'NONE',  ( 0.000000000000000000, -1.000000000000000000, 0.000000000000000000 ) ) ;
#56685 =( NAMED_UNIT ( * ) PLANE_ANGLE_UNIT ( ) SI_UNIT ( $, .RADIAN. ) );
#56686 = CARTESIAN_POINT ( 'NONE',  ( -2.266590686148945544, 61.38708216824730357, -7.082119434687050408 ) ) ;
#56687 = CARTESIAN_POINT ( 'NONE',  ( 6.204703633549690345, 12.84541550158063572, 14.16423886937410082 ) ) ;
#56688 = CARTESIAN_POINT ( 'NONE',  ( 0.1532563361054083140, 6.008931151000784787, 1.131784320476157264E-15 ) ) ;
#56689 = CARTESIAN_POINT ( 'NONE',  ( 19.84674366389459266, 43.71726448433410894, -2.638427012816827677 ) ) ;
#56690 = CARTESIAN_POINT ( 'NONE',  ( 15.44008868035555260, 39.73035201082150536, 9.422509992056143702 ) ) ;
#56691 = DIRECTION ( 'NONE',  ( 0.7604059656000385914, 0.000000000000000000, -0.6494480483301746654 ) ) ;
#56692 = CARTESIAN_POINT ( 'NONE',  ( 14.92337183194729988, 64.34226448433412315, -8.527530157486177487 ) ) ;
#56693 = STYLED_ITEM ( 'NONE', ( #13293 ), #10682 ) ;
#56694 = ADVANCED_FACE ( 'NONE', ( #9937 ), #13976, .T. ) ;
#56695 = ORIENTED_EDGE ( 'NONE', *, *, #45407, .F. ) ;
#56696 = CARTESIAN_POINT ( 'NONE',  ( 6.507517414235559627, -58.30789062360079100, 2.499999999999999556 ) ) ;
#56697 = ORIENTED_EDGE ( 'NONE', *, *, #85182, .T. ) ;
#56698 = ORIENTED_EDGE ( 'NONE', *, *, #83671, .F. ) ;
#56699 = CARTESIAN_POINT ( 'NONE',  ( 6.189940676892025984, 0.04962882325992712396, 13.39186120659007351 ) ) ;
#56700 = CARTESIAN_POINT ( 'NONE',  ( 24.16423886937410614, 9.303748834913967869, 8.672049930838204340E-16 ) ) ;
#56701 = CARTESIAN_POINT ( 'NONE',  ( 20.36894250292379382, 3.678748834913967869, 10.36894250292379205 ) ) ;
#56702 =( GEOMETRIC_REPRESENTATION_CONTEXT ( 3 ) GLOBAL_UNCERTAINTY_ASSIGNED_CONTEXT ( ( #14481 ) ) GLOBAL_UNIT_ASSIGNED_CONTEXT ( ( #4762, #27242, #80749 ) ) REPRESENTATION_CONTEXT ( 'NONE', 'WORKASPACE' ) );
#56703 = CARTESIAN_POINT ( 'NONE',  ( 13.79529636645030344, 43.26208216824730357, 14.16423886937410614 ) ) ;
#56704 = CARTESIAN_POINT ( 'NONE',  ( 19.84674366389459266, 53.30059781766744464, 2.638427012816836559 ) ) ;
#56705 = CARTESIAN_POINT ( 'NONE',  ( 1.472469842513823179, 41.42559781766745886, 4.923371831947296329 ) ) ;
#56707 = CARTESIAN_POINT ( 'NONE',  ( 7.361572987183170547, 62.05059781766745886, 9.846743663894590881 ) ) ;
#56706 = CARTESIAN_POINT ( 'NONE',  ( 12.91533473730992121, 29.52201867748817321, 10.88017736071110164 ) ) ;
#56708 = CARTESIAN_POINT ( 'NONE',  ( 10.00000000000000000, 0.5537488349139675359, -14.16423886937410082 ) ) ;
#56709 = CARTESIAN_POINT ( 'NONE',  ( 13.79529636645030344, 38.26208216824729647, 14.16423886937410614 ) ) ;
#56710 = CARTESIAN_POINT ( 'NONE',  ( 2.035157376598822676, 7.438685344154837509, -7.964842623401177768 ) ) ;
#56711 = CARTESIAN_POINT ( 'NONE',  ( 12.63842701281683922, 64.55059781766745175, -9.846743663894590881 ) ) ;
#56712 = CARTESIAN_POINT ( 'NONE',  ( 0.000000000000000000, 99.74999999999998579, 7.750000000000000000 ) ) ;
#56713 = CARTESIAN_POINT ( 'NONE',  ( 20.88017736071110164, 65.35535201082150536, 2.915334737309930979 ) ) ;
#56714 = EDGE_CURVE ( 'NONE', #44083, #59040, #14783, .T. ) ;
#56715 = CARTESIAN_POINT ( 'NONE',  ( 0.1532563361054082862, 26.21726448433411605, 2.638427012816831674 ) ) ;
#56716 = FACE_OUTER_BOUND ( 'NONE', #23796, .T. ) ;
#56717 = ORIENTED_EDGE ( 'NONE', *, *, #49890, .T. ) ;
#56718 = ORIENTED_EDGE ( 'NONE', *, *, #96197, .F. ) ;
#56719 = CARTESIAN_POINT ( 'NONE',  ( 19.84674366389459266, 18.30059781766745175, 2.638427012816836559 ) ) ;
#56720 = ORIENTED_EDGE ( 'NONE', *, *, #77588, .T. ) ;
#56721 = CARTESIAN_POINT ( 'NONE',  ( 24.16423886937409904, 39.09541550158062506, 3.795296366450317205 ) ) ;
#56722 = CARTESIAN_POINT ( 'NONE',  ( 5.076628168052704559, 30.17559781766745175, -8.527530157486179263 ) ) ;
#56723 = CARTESIAN_POINT ( 'NONE',  ( 20.88017736071110519, 60.56368534415484106, 2.639326808657452039E-16 ) ) ;
#56724 = CARTESIAN_POINT ( 'NONE',  ( -9.876730923139145801, 0.5000000000000004441, -11.28938378619076843 ) ) ;
#56725 = EDGE_CURVE ( 'NONE', #30576, #76841, #60288, .T. ) ;
#56726 = CARTESIAN_POINT ( 'NONE',  ( 10.00000000000000178, 39.31368534415484106, 10.88017736071110342 ) ) ;
#56727 = CARTESIAN_POINT ( 'NONE',  ( 0.1532563361054100626, 45.80059781766745886, -2.638427012816831230 ) ) ;
#56728 = TOROIDAL_SURFACE ( 'NONE', #87056, 3.750000000000001776, 0.2500000000000000000 ) ;
#56729 = CARTESIAN_POINT ( 'NONE',  ( -3.434112377981067610, -1.918031996736249356, -12.81628187352647252 ) ) ;
#56730 = VERTEX_POINT ( 'NONE', #10399 ) ;
#56731 = CARTESIAN_POINT ( 'NONE',  ( -4.164238869374099927, 22.01208216824730357, 3.795296366450308767 ) ) ;
#56732 = ORIENTED_EDGE ( 'NONE', *, *, #53334, .T. ) ;
#56733 = ORIENTED_EDGE ( 'NONE', *, *, #70277, .F. ) ;
#56734 = CARTESIAN_POINT ( 'NONE',  ( 22.81628187352648496, 31.83196800326375353, -3.434112377981050290 ) ) ;
#56735 = CARTESIAN_POINT ( 'NONE',  ( 5.076628168052703671, 21.84226448433411960, 8.527530157486179263 ) ) ;
#56736 = CARTESIAN_POINT ( 'NONE',  ( 16.40814093676324603, 47.45696800326375353, -11.09922568453594671 ) ) ;
#56737 = CARTESIAN_POINT ( 'NONE',  ( -46.34323875807880455, 103.6109741468810483, -6.190393423093145664 ) ) ;
#56738 = CARTESIAN_POINT ( 'NONE',  ( 18.52753015748618282, 28.92559781766745175, -4.923371831947291888 ) ) ;
#56739 = CARTESIAN_POINT ( 'NONE',  ( 17.96484262340118221, 64.93868534415483396, 7.964842623401181321 ) ) ;
#56740 = VECTOR ( 'NONE', #34651, 1000.000000000000000 ) ;
#56741 =( NAMED_UNIT ( * ) SI_UNIT ( $, .STERADIAN. ) SOLID_ANGLE_UNIT ( ) );
#56742 = DIRECTION ( 'NONE',  ( -1.000000000000000000, 0.000000000000000000, 0.000000000000000000 ) ) ;
#56743 = CARTESIAN_POINT ( 'NONE',  ( -43.18060676906663531, 107.2752179745913708, 4.519309965511820515 ) ) ;
#56744 = CARTESIAN_POINT ( 'NONE',  ( -0.1503990784575328643, 45.12777174578613426, 6.262539305110068177 ) ) ;
#56745 = CARTESIAN_POINT ( 'NONE',  ( -0.8801773607111008646, 68.27201867748817676, 2.915334737309923430 ) ) ;
#56746 = CARTESIAN_POINT ( 'NONE',  ( 22.81628187352647785, 16.41530133659708923, 3.434112377981063169 ) ) ;
#56747 = DIRECTION ( 'NONE',  ( 0.000000000000000000, 0.000000000000000000, -1.000000000000000000 ) ) ;
#56748 = EDGE_CURVE ( 'NONE', #76742, #49408, #41106, .T. ) ;
#56749 = CARTESIAN_POINT ( 'NONE',  ( 19.84674366389459621, 38.50893115100078745, 7.409399052514197653E-17 ) ) ;
#56750 = CARTESIAN_POINT ( 'NONE',  ( 3.640395162852214650, 107.5383484153110061, -5.000000000000000000 ) ) ;
#56751 = CARTESIAN_POINT ( 'NONE',  ( 17.08211943468705130, 13.47041550158063572, 12.26659068614894998 ) ) ;
#56752 = CARTESIAN_POINT ( 'NONE',  ( 5.076628168052703671, 26.84226448433411960, 8.527530157486179263 ) ) ;
#56753 = CARTESIAN_POINT ( 'NONE',  ( 6.565887622018943937, 28.08196800326375353, -12.81628187352647608 ) ) ;
#56754 = CARTESIAN_POINT ( 'NONE',  ( 26.00000000000000355, 35.99999999999997158, -10.00000000000000000 ) ) ;
#56755 = CARTESIAN_POINT ( 'NONE',  ( 7.084665262690076126, 67.02201867748817676, -10.88017736071110164 ) ) ;
#56756 = CARTESIAN_POINT ( 'NONE',  ( 13.43411237798105340, 5.581968003263753531, 12.81628187352647963 ) ) ;
#56757 = CARTESIAN_POINT ( 'NONE',  ( 4.856092091438229730, 15.00000000000000178, 13.79590085420556811 ) ) ;
#56758 = EDGE_CURVE ( 'NONE', #12076, #70662, #79419, .T. ) ;
#56759 = CARTESIAN_POINT ( 'NONE',  ( 19.84674366389459266, 38.71726448433412315, -2.638427012816827677 ) ) ;
#56760 = CARTESIAN_POINT ( 'NONE',  ( -0.8801773607110991993, 27.85535201082150181, -2.915334737309923874 ) ) ;
#56761 = CARTESIAN_POINT ( 'NONE',  ( -1.099225684535947600, 24.54030133659708923, 6.408140936763237150 ) ) ;
#56762 = CIRCLE ( 'NONE', #90295, 0.5000000000000004441 ) ;
#56763 = CARTESIAN_POINT ( 'NONE',  ( 2.791683348922240793, 16.63393115100078745, 7.208316651077764092 ) ) ;
#56764 = CARTESIAN_POINT ( 'NONE',  ( -12.19495285927274431, 90.49761223356982498, 7.228801115472508698 ) ) ;
#56765 = CARTESIAN_POINT ( 'NONE',  ( -0.8801773607111009756, 28.06368534415484106, 1.068504757029289695E-15 ) ) ;
#56766 = CIRCLE ( 'NONE', #50414, 0.4999999999999998335 ) ;
#56767 = ORIENTED_EDGE ( 'NONE', *, *, #40571, .T. ) ;
#56768 = CARTESIAN_POINT ( 'NONE',  ( -0.8801773607110991993, 57.85535201082149825, -2.915334737309923874 ) ) ;
#56769 = CARTESIAN_POINT ( 'NONE',  ( -0.8801773607111008646, 3.272018677488171434, 2.915334737309923430 ) ) ;
#56771 = CARTESIAN_POINT ( 'NONE',  ( 20.88017736071110519, 35.56368534415484106, 2.639326808657452039E-16 ) ) ;
#56770 = CARTESIAN_POINT ( 'NONE',  ( 14.92337183194729988, 39.34226448433412315, -8.527530157486177487 ) ) ;
#56772 =( NAMED_UNIT ( * ) PLANE_ANGLE_UNIT ( ) SI_UNIT ( $, .RADIAN. ) );
#56773 = CARTESIAN_POINT ( 'NONE',  ( 15.44008868035555793, 41.39701867748817676, -9.422509992056140149 ) ) ;
#56775 = DIRECTION ( 'NONE',  ( 0.000000000000000000, 1.000000000000000000, -0.000000000000000000 ) ) ;
#56774 = CARTESIAN_POINT ( 'NONE',  ( 4.559911319644449179, 8.897018677488173211, 9.422509992056141925 ) ) ;
#56776 = CARTESIAN_POINT ( 'NONE',  ( 6.000000000000000000, 61.00000000000000711, -6.000000000000000000 ) ) ;
#56777 = CARTESIAN_POINT ( 'NONE',  ( 18.52753015748618282, 43.92559781766745175, -4.923371831947291888 ) ) ;
#56779 = CARTESIAN_POINT ( 'NONE',  ( 5.114754712244249824, -17.52455492747532517, 3.750000000000000444 ) ) ;
#56778 = CARTESIAN_POINT ( 'NONE',  ( 17.08211943468705130, 48.47041550158063927, 12.26659068614894998 ) ) ;
#56780 = DIRECTION ( 'NONE',  ( 0.000000000000000000, 0.000000000000000000, -1.000000000000000000 ) ) ;
#56781 = CARTESIAN_POINT ( 'NONE',  ( 2.917880565312950480, 30.97041550158063572, -12.26659068614894821 ) ) ;
#56782 = EDGE_CURVE ( 'NONE', #1372, #67800, #12385, .T. ) ;
#56783 = CARTESIAN_POINT ( 'NONE',  ( -3.500000000000001776, 0.08936006763181135459, 2.750000000000000888 ) ) ;
#56784 = ORIENTED_EDGE ( 'NONE', *, *, #3766, .T. ) ;
#56785 = CARTESIAN_POINT ( 'NONE',  ( -0.3689425029237881626, 62.42874883491396787, 10.36894250292379027 ) ) ;
#56786 = CARTESIAN_POINT ( 'NONE',  ( 12.63842701281683922, 29.55059781766745175, -9.846743663894590881 ) ) ;
#56788 = CARTESIAN_POINT ( 'NONE',  ( -8.641261271118773735, 87.40425324006859853, -4.716577832614896160 ) ) ;
#56787 = CARTESIAN_POINT ( 'NONE',  ( -6.767445849361341637, 14.49999999999999112, 13.38662304974498873 ) ) ;
#56789 = CARTESIAN_POINT ( 'NONE',  ( 12.91533473730992121, 64.52201867748817676, 10.88017736071110164 ) ) ;
#56790 = CARTESIAN_POINT ( 'NONE',  ( 10.00000000000000178, 65.37363466993042493, 12.81628187352647608 ) ) ;
#56791 = EDGE_CURVE ( 'NONE', #58660, #10735, #61324, .T. ) ;
#56792 = CARTESIAN_POINT ( 'NONE',  ( 19.42250999205614548, 25.98035201082150891, -5.440088680355545492 ) ) ;
#56793 = CARTESIAN_POINT ( 'NONE',  ( 21.09922568453594849, 61.20696800326376064, 6.408140936763242479 ) ) ;
#56794 = CARTESIAN_POINT ( 'NONE',  ( 22.81628187352648496, 6.831968003263753531, -3.434112377981050290 ) ) ;
#56795 = CARTESIAN_POINT ( 'NONE',  ( 7.361572987183169658, 9.967264484334119601, -9.846743663894592657 ) ) ;
#56796 = ORIENTED_EDGE ( 'NONE', *, *, #47002, .F. ) ;
#56797 = FACE_OUTER_BOUND ( 'NONE', #28562, .T. ) ;
#56798 = DIRECTION ( 'NONE',  ( 1.000000000000000000, -0.000000000000000000, 0.000000000000000000 ) ) ;
#56799 = CARTESIAN_POINT ( 'NONE',  ( 13.79529636645031943, 65.34541550158063217, -14.16423886937409904 ) ) ;
#56800 = CARTESIAN_POINT ( 'NONE',  ( 22.26659068614894466, 23.88708216824730357, 7.082119434687054849 ) ) ;
#56801 = CARTESIAN_POINT ( 'NONE',  ( 2.035157376598822676, 37.43868534415484106, -7.964842623401177768 ) ) ;
#56802 = CARTESIAN_POINT ( 'NONE',  ( 17.96484262340118221, 51.18868534415483396, -7.964842623401177768 ) ) ;
#56803 = CYLINDRICAL_SURFACE ( 'NONE', #36747, 15.00000000000000000 ) ;
#56804 = FACE_OUTER_BOUND ( 'NONE', #32164, .T. ) ;
#56805 = CARTESIAN_POINT ( 'NONE',  ( 12.63842701281683034, 7.467264484334118713, 9.846743663894596210 ) ) ;
#56806 = DIRECTION ( 'NONE',  ( -1.000000000000000000, 6.938893903907221278E-15, -6.938893903907221278E-15 ) ) ;
#56807 = CARTESIAN_POINT ( 'NONE',  ( 18.52753015748617571, 28.09226448433411960, 4.923371831947298993 ) ) ;
#56808 = SURFACE_STYLE_USAGE ( .BOTH. , #72778 ) ;
#56809 = CARTESIAN_POINT ( 'NONE',  ( 1.472469842513823179, 25.59226448433412315, -4.923371831947296329 ) ) ;
#56810 = CARTESIAN_POINT ( 'NONE',  ( 7.361572987183170547, 47.05059781766745175, 9.846743663894590881 ) ) ;
#56811 = AXIS2_PLACEMENT_3D ( 'NONE', #3791, #12742, #57256 ) ;
#56812 = CARTESIAN_POINT ( 'NONE',  ( 4.559911319644449179, 28.89701867748817321, 9.422509992056141925 ) ) ;
#56813 = CARTESIAN_POINT ( 'NONE',  ( 22.81628187352647785, 46.41530133659708213, 3.434112377981063169 ) ) ;
#56814 = AXIS2_PLACEMENT_3D ( 'NONE', #83274, #36793, #21295 ) ;
#56815 = CARTESIAN_POINT ( 'NONE',  ( 19.84674366389459621, 33.50893115100078745, 7.409399052514197653E-17 ) ) ;
#56818 = EDGE_CURVE ( 'NONE', #76742, #14585, #66637, .T. ) ;
#56817 = CARTESIAN_POINT ( 'NONE',  ( 7.361572987183169658, 24.96726448433412315, -9.846743663894592657 ) ) ;
#56816 = CARTESIAN_POINT ( 'NONE',  ( 24.16423886937410614, 59.51208216824728936, -3.795296366450302550 ) ) ;
#56819 = DIRECTION ( 'NONE',  ( -0.000000000000000000, -1.000000000000000000, -0.000000000000000000 ) ) ;
#56820 = CARTESIAN_POINT ( 'NONE',  ( 5.076628168052704559, 65.17559781766745175, -8.527530157486179263 ) ) ;
#56821 = CARTESIAN_POINT ( 'NONE',  ( 22.26659068614894466, 33.88708216824730357, 7.082119434687054849 ) ) ;
#56822 = CARTESIAN_POINT ( 'NONE',  ( 12.63842701281683034, 32.46726448433412315, 9.846743663894596210 ) ) ;
#56823 = DIRECTION ( 'NONE',  ( 0.5519369853120559277, 0.000000000000000000, 0.8338858220671695465 ) ) ;
#56824 = CARTESIAN_POINT ( 'NONE',  ( -0.8801773607111008646, 23.27201867748817676, 2.915334737309923430 ) ) ;
#56825 = B_SPLINE_CURVE_WITH_KNOTS ( 'NONE', 3,
 ( #19317, #41839, #64306, #28293, #49803, #20803 ),
 .UNSPECIFIED., .F., .F.,
 ( 4, 2, 4 ),
 ( 0.000000000000000000, 0.0002701661927229424918, 0.0005403323854458849836 ),
 .UNSPECIFIED. ) ;
#56826 = EDGE_CURVE ( 'NONE', #50486, #5813, #21973, .T. ) ;
#56827 = CARTESIAN_POINT ( 'NONE',  ( 17.96484262340118221, 61.18868534415482685, -7.964842623401177768 ) ) ;
#56828 = CARTESIAN_POINT ( 'NONE',  ( 0.5774900079438607392, 48.48035201082150536, 5.440088680355550821 ) ) ;
#56829 = EDGE_LOOP ( 'NONE', ( #49555, #41021 ) ) ;
#56830 = CARTESIAN_POINT ( 'NONE',  ( 16.40814093676324603, 47.45696800326375353, -11.09922568453594671 ) ) ;
#56831 = CARTESIAN_POINT ( 'NONE',  ( 15.44008868035555260, 49.73035201082150536, 9.422509992056143702 ) ) ;
#56832 = VERTEX_POINT ( 'NONE', #17423 ) ;
#56833 = CARTESIAN_POINT ( 'NONE',  ( 2.791683348922237240, 0.3839311510007847872, -7.208316651077763204 ) ) ;
#56834 = CARTESIAN_POINT ( 'NONE',  ( 20.88017736071110875, 65.77201867748817676, -2.915334737309920765 ) ) ;
#56835 = VECTOR ( 'NONE', #70923, 1000.000000000000114 ) ;
#56836 = ORIENTED_EDGE ( 'NONE', *, *, #61902, .T. ) ;
#56837 = VECTOR ( 'NONE', #57326, 1000.000000000000000 ) ;
#56838 = CARTESIAN_POINT ( 'NONE',  ( -0.8801773607110991993, 67.85535201082151957, -2.915334737309923874 ) ) ;
#56839 = CARTESIAN_POINT ( 'NONE',  ( 17.96484262340118221, 6.188685344154836621, -7.964842623401177768 ) ) ;
#56840 = CARTESIAN_POINT ( 'NONE',  ( 14.35840480524204210, 14.49999999999999112, 4.340070442838943165 ) ) ;
#56841 = CYLINDRICAL_SURFACE ( 'NONE', #72810, 0.5000000000000004441 ) ;
#56842 = CARTESIAN_POINT ( 'NONE',  ( -0.8801773607111008646, 13.27201867748817321, 2.915334737309923430 ) ) ;
#56843 = CARTESIAN_POINT ( 'NONE',  ( 0.1532563361054083140, 6.008931151000784787, 1.131784320476157264E-15 ) ) ;
#56844 = CARTESIAN_POINT ( 'NONE',  ( 10.00000000000000000, 0.5537488349139675359, -14.16423886937410082 ) ) ;
#56845 = CARTESIAN_POINT ( 'NONE',  ( 1.472469842513823179, 6.425597817667451750, 4.923371831947296329 ) ) ;
#56846 = CARTESIAN_POINT ( 'NONE',  ( 4.559911319644449179, 7.230352010821504471, -9.422509992056141925 ) ) ;
#56847 = CARTESIAN_POINT ( 'NONE',  ( 5.076628168052703671, 51.84226448433412315, 8.527530157486179263 ) ) ;
#56848 = ORIENTED_EDGE ( 'NONE', *, *, #16304, .T. ) ;
#56849 = CARTESIAN_POINT ( 'NONE',  ( 17.20831665107776587, 47.88393115100078745, 7.208316651077764980 ) ) ;
#56850 = ORIENTED_EDGE ( 'NONE', *, *, #2152, .F. ) ;
#56851 = DIRECTION ( 'NONE',  ( 0.000000000000000000, 1.000000000000000000, 0.000000000000000000 ) ) ;
#56852 = CARTESIAN_POINT ( 'NONE',  ( 0.5774900079438607392, 58.48035201082151247, 5.440088680355550821 ) ) ;
#56853 = CARTESIAN_POINT ( 'NONE',  ( 5.076628168052704559, 55.17559781766745175, -8.527530157486179263 ) ) ;
#56855 = CARTESIAN_POINT ( 'NONE',  ( -9.288883250831421634, 2.385537343846901415, -6.626163283838958584 ) ) ;
#56854 = CARTESIAN_POINT ( 'NONE',  ( 0.5774900079438607392, 8.480352010821505360, 5.440088680355550821 ) ) ;
#56856 = CARTESIAN_POINT ( 'NONE',  ( 7.084665262690076126, 62.02201867748816966, -10.88017736071110164 ) ) ;
#56857 = CARTESIAN_POINT ( 'NONE',  ( 12.91533473730992121, 4.522018677488170546, 10.88017736071110164 ) ) ;
#56858 = CARTESIAN_POINT ( 'NONE',  ( -2.816281873526473856, 39.33196800326374643, 3.434112377981055619 ) ) ;
#56859 = CARTESIAN_POINT ( 'NONE',  ( 17.96484262340118221, 34.93868534415482685, 7.964842623401181321 ) ) ;
#56860 = DIRECTION ( 'NONE',  ( -0.000000000000000000, -1.000000000000000000, -0.000000000000000000 ) ) ;
#56861 = ORIENTED_EDGE ( 'NONE', *, *, #23089, .F. ) ;
#56862 = CARTESIAN_POINT ( 'NONE',  ( 19.38216949554541557, 42.24863466993041783, -9.382169495545420901 ) ) ;
#56863 = CARTESIAN_POINT ( 'NONE',  ( 15.44008868035555260, 39.73035201082150536, 9.422509992056143702 ) ) ;
#56864 = ORIENTED_EDGE ( 'NONE', *, *, #59229, .T. ) ;
#56865 = CARTESIAN_POINT ( 'NONE',  ( 19.84674366389459266, 8.717264484334116048, -2.638427012816827677 ) ) ;
#56866 = CARTESIAN_POINT ( 'NONE',  ( 17.20831665107776587, 64.13393115100079456, -7.208316651077762316 ) ) ;
#56868 = CARTESIAN_POINT ( 'NONE',  ( 10.00000000000000000, 44.75893115100078745, -9.846743663894594434 ) ) ;
#56867 = CARTESIAN_POINT ( 'NONE',  ( 10.00000000000000000, 14.75893115100078568, -9.846743663894594434 ) ) ;
#56869 = CARTESIAN_POINT ( 'NONE',  ( -10.81543368776825886, -98.37186030702901007, 3.750000000000000444 ) ) ;
#56870 = CARTESIAN_POINT ( 'NONE',  ( 14.09356342482598379, 0.04922511925147127210, -4.360913911515380548 ) ) ;
#56871 = VECTOR ( 'NONE', #12040, 1000.000000000000114 ) ;
#56872 = CARTESIAN_POINT ( 'NONE',  ( 5.279540384298785582, 0.000000000000000000, -1.365381980696706687 ) ) ;
#56873 = ADVANCED_FACE ( 'NONE', ( #39914 ), #39538, .T. ) ;
#56875 = CARTESIAN_POINT ( 'NONE',  ( 7.361572987183170547, 2.050597817667451750, 9.846743663894590881 ) ) ;
#56874 = CARTESIAN_POINT ( 'NONE',  ( 10.00000000000000178, 27.25893115100078390, 9.846743663894594434 ) ) ;
#56877 = VERTEX_POINT ( 'NONE', #86883 ) ;
#56876 = CARTESIAN_POINT ( 'NONE',  ( 7.361572987183169658, 54.96726448433413026, -9.846743663894592657 ) ) ;
#56878 = PRESENTATION_STYLE_ASSIGNMENT (( #93901 ) ) ;
#56879 = CARTESIAN_POINT ( 'NONE',  ( 22.81628187352647785, 21.41530133659708923, 3.434112377981063169 ) ) ;
#56880 = CARTESIAN_POINT ( 'NONE',  ( 10.00000000000000000, 44.75893115100078745, -9.846743663894594434 ) ) ;
#56881 = CARTESIAN_POINT ( 'NONE',  ( 5.625000000000006217, 6.784700295649323643, 9.742785792574933268 ) ) ;
#56882 = CARTESIAN_POINT ( 'NONE',  ( -2.266590686148945544, 62.22041550158063927, 7.082119434687048631 ) ) ;
#56883 = CARTESIAN_POINT ( 'NONE',  ( 17.20831665107776587, 22.88393115100078745, 7.208316651077764980 ) ) ;
#56884 = COLOUR_RGB ( '', 0.09019608, 0.27058824, 0.51372549) ;
#56885 = CARTESIAN_POINT ( 'NONE',  ( -1.926860441876564023, 39.68830936912750929, 1.004413902775740781E-15 ) ) ;
#56886 = CARTESIAN_POINT ( 'NONE',  ( -4.164238869374099039, 61.80374883491397497, 8.674139862899312516E-16 ) ) ;
#56887 = CARTESIAN_POINT ( 'NONE',  ( 17.20831665107776587, 62.88393115100078745, 7.208316651077764980 ) ) ;
#56888 = CARTESIAN_POINT ( 'NONE',  ( 0.5774900079438607392, 3.480352010821504916, 5.440088680355550821 ) ) ;
#56889 = CARTESIAN_POINT ( 'NONE',  ( -0.3689425029237898834, 31.17874883491396787, -10.36894250292378850 ) ) ;
#56890 = CARTESIAN_POINT ( 'NONE',  ( 17.08211943468705840, 45.13708216824730357, -12.26659068614894466 ) ) ;
#56891 = FACE_OUTER_BOUND ( 'NONE', #48992, .T. ) ;
#56893 = CARTESIAN_POINT ( 'NONE',  ( 7.361572987183169658, 59.96726448433410894, -9.846743663894592657 ) ) ;
#56892 = DIRECTION ( 'NONE',  ( 0.000000000000000000, 1.000000000000000000, 0.000000000000000000 ) ) ;
#56894 = AXIS2_PLACEMENT_3D ( 'NONE', #43744, #67749, #74739 ) ;
#56895 = CARTESIAN_POINT ( 'NONE',  ( 20.88017736071110875, 45.77201867748816966, -2.915334737309920765 ) ) ;
#56896 = CARTESIAN_POINT ( 'NONE',  ( 19.65595514172846592, 92.20290667148093178, -5.361975859778444153 ) ) ;
#56897 = CARTESIAN_POINT ( 'NONE',  ( 5.076628168052703671, 51.84226448433412315, 8.527530157486179263 ) ) ;
#56898 = CARTESIAN_POINT ( 'NONE',  ( -2.816281873526473856, 64.12363466993042493, 9.499525473075851096E-16 ) ) ;
#56899 = VECTOR ( 'NONE', #57753, 1000.000000000000000 ) ;
#56900 = CARTESIAN_POINT ( 'NONE',  ( 5.076628168052703671, 56.84226448433412315, 8.527530157486179263 ) ) ;
#56901 = CARTESIAN_POINT ( 'NONE',  ( 19.84674366389459266, 63.30059781766745886, 2.638427012816836559 ) ) ;
#56902 = EDGE_CURVE ( 'NONE', #34926, #69049, #76208, .T. ) ;
#56903 = CARTESIAN_POINT ( 'NONE',  ( 10.00000000000000000, 25.55374883491396787, -14.16423886937410082 ) ) ;
#56904 = AXIS2_PLACEMENT_3D ( 'NONE', #42127, #27097, #64593 ) ;
#56905 = CARTESIAN_POINT ( 'NONE',  ( -14.97687855664615064, 14.49999999999999112, 0.8325315005899805998 ) ) ;
#56907 = CARTESIAN_POINT ( 'NONE',  ( -10.91036564011027465, 14.76984962000593704, -10.20716212663452360 ) ) ;
#56906 = CARTESIAN_POINT ( 'NONE',  ( -3.887834249506515683, -8.254296980867451339, -2.499999999999195310 ) ) ;
#56908 = CARTESIAN_POINT ( 'NONE',  ( 12.91533473730992121, 14.52201867748817143, 10.88017736071110164 ) ) ;
#56909 = CARTESIAN_POINT ( 'NONE',  ( 19.38216949554541202, 20.99863466993042138, 9.382169495545424454 ) ) ;
#56910 = EDGE_CURVE ( 'NONE', #42104, #65885, #26373, .T. ) ;
#56911 = CARTESIAN_POINT ( 'NONE',  ( -13.95806775979391823, 15.00000000000000888, -4.371577651620918381 ) ) ;
#56912 = CARTESIAN_POINT ( 'NONE',  ( 12.63842701281683034, 12.46726448433411782, 9.846743663894596210 ) ) ;
#56913 = CARTESIAN_POINT ( 'NONE',  ( 6.829574850505125028, -88.00372650098209704, -3.750000000000000000 ) ) ;
#56914 = CARTESIAN_POINT ( 'NONE',  ( 6.204703633549690345, 32.84541550158063927, 14.16423886937410082 ) ) ;
#56915 = CARTESIAN_POINT ( 'NONE',  ( 1.472469842513823179, 21.42559781766745175, 4.923371831947296329 ) ) ;
#56916 = SURFACE_SIDE_STYLE ('',( #94916 ) ) ;
#56917 = CARTESIAN_POINT ( 'NONE',  ( 7.084665262690076126, 4.105352010821503583, 10.88017736071109987 ) ) ;
#56918 = CARTESIAN_POINT ( 'NONE',  ( -1.175037534397337380, 15.00000000000000178, 14.57833316477036334 ) ) ;
#56919 = CARTESIAN_POINT ( 'NONE',  ( 20.88017736071110875, 45.77201867748816966, -2.915334737309920765 ) ) ;
#56920 = CARTESIAN_POINT ( 'NONE',  ( 15.44008868035555260, 39.73035201082150536, 9.422509992056143702 ) ) ;
#56921 = CARTESIAN_POINT ( 'NONE',  ( 0.6178305044545838731, -0.2513653300695798953, 9.382169495545420901 ) ) ;
#56922 = CARTESIAN_POINT ( 'NONE',  ( 13.61464873478162652, 15.00000000000000000, 6.296136897217931683 ) ) ;
#56923 = FACE_OUTER_BOUND ( 'NONE', #38619, .T. ) ;
#56924 = CARTESIAN_POINT ( 'NONE',  ( 5.076628168052703671, 11.84226448433411960, 8.527530157486179263 ) ) ;
#56925 = DIRECTION ( 'NONE',  ( 0.000000000000000000, 0.000000000000000000, 1.000000000000000000 ) ) ;
#56926 = CARTESIAN_POINT ( 'NONE',  ( 0.5774900079438607392, 48.48035201082150536, 5.440088680355550821 ) ) ;
#56927 = AXIS2_PLACEMENT_3D ( 'NONE', #82941, #90922, #59441 ) ;
#56928 = COLOUR_RGB ( '', 0.31764706, 0.68627451, 0.89019608) ;
#56929 = AXIS2_PLACEMENT_3D ( 'NONE', #20623, #5627, #68100 ) ;
#56930 = CARTESIAN_POINT ( 'NONE',  ( 22.81628187352648496, 11.83196800326375531, -3.434112377981050290 ) ) ;
#56931 = CARTESIAN_POINT ( 'NONE',  ( 20.88017736071110875, 60.77201867748817676, -2.915334737309920765 ) ) ;
#56932 = CARTESIAN_POINT ( 'NONE',  ( 5.076628168052704559, 30.17559781766745175, -8.527530157486179263 ) ) ;
#56933 = CARTESIAN_POINT ( 'NONE',  ( 3.591859063236761518, 39.95696800326375353, 11.09922568453594849 ) ) ;
#56934 = CARTESIAN_POINT ( 'NONE',  ( 2.791683348922237240, 0.3839311510007847872, -7.208316651077763204 ) ) ;
#56935 = ORIENTED_EDGE ( 'NONE', *, *, #96342, .F. ) ;
#56936 = FILL_AREA_STYLE ('',( #41961 ) ) ;
#56937 = CARTESIAN_POINT ( 'NONE',  ( 13.55255535720595184, 15.00000000000000000, -4.403492169842965431 ) ) ;
#56938 = CARTESIAN_POINT ( 'NONE',  ( 4.559911319644449179, 12.23035201082150536, -9.422509992056141925 ) ) ;
#56940 = CARTESIAN_POINT ( 'NONE',  ( -0.3689425029237898834, 21.17874883491396432, -10.36894250292378850 ) ) ;
#56939 = CARTESIAN_POINT ( 'NONE',  ( 19.38216949554541202, 55.99863466993041072, 9.382169495545424454 ) ) ;
#56941 = CARTESIAN_POINT ( 'NONE',  ( 17.20831665107776587, 24.13393115100078035, -7.208316651077762316 ) ) ;
#56942 = CARTESIAN_POINT ( 'NONE',  ( 10.00000000000000178, 9.313685344154839285, 10.88017736071110342 ) ) ;
#56943 = CARTESIAN_POINT ( 'NONE',  ( -0.8801773607111009756, 8.063685344154837509, 1.068504757029289695E-15 ) ) ;
#56944 = ORIENTED_EDGE ( 'NONE', *, *, #45088, .F. ) ;
#56945 = AXIS2_PLACEMENT_3D ( 'NONE', #59141, #19679, #35664 ) ;
#56946 = CARTESIAN_POINT ( 'NONE',  ( 4.559911319644449179, 18.89701867748817321, 9.422509992056141925 ) ) ;
#56947 = EDGE_CURVE ( 'NONE', #77856, #56575, #79220, .T. ) ;
#56948 = CARTESIAN_POINT ( 'NONE',  ( 7.084665262690076126, 19.10535201082150181, 10.88017736071109987 ) ) ;
#56949 = DIRECTION ( 'NONE',  ( 0.000000000000000000, -1.000000000000000000, 0.000000000000000000 ) ) ;
#56950 = ORIENTED_EDGE ( 'NONE', *, *, #12002, .T. ) ;
#56951 = CARTESIAN_POINT ( 'NONE',  ( 1.472469842513823179, 66.42559781766745175, 4.923371831947296329 ) ) ;
#56952 = CARTESIAN_POINT ( 'NONE',  ( 4.559911319644449179, 23.89701867748817321, 9.422509992056141925 ) ) ;
#56953 = CARTESIAN_POINT ( 'NONE',  ( 2.791683348922237240, 60.38393115100078745, -7.208316651077763204 ) ) ;
#56954 = CARTESIAN_POINT ( 'NONE',  ( 10.00000000000000000, 52.87363466993041783, -12.81628187352647608 ) ) ;
#56955 = DIRECTION ( 'NONE',  ( -0.000000000000000000, -0.000000000000000000, 1.000000000000000000 ) ) ;
#56956 = CARTESIAN_POINT ( 'NONE',  ( 20.36894250292379382, 33.67874883491396076, 10.36894250292379205 ) ) ;
#56957 = CARTESIAN_POINT ( 'NONE',  ( 17.96484262340118221, 41.18868534415484106, -7.964842623401177768 ) ) ;
#56958 = CARTESIAN_POINT ( 'NONE',  ( 0.5774900079438607392, 13.48035201082150358, 5.440088680355550821 ) ) ;
#56959 = CARTESIAN_POINT ( 'NONE',  ( 18.52753015748618282, 53.92559781766745175, -4.923371831947291888 ) ) ;
#56960 = AXIS2_PLACEMENT_3D ( 'NONE', #77982, #86484, #70000 ) ;
#56961 =( BOUNDED_SURFACE ( )  B_SPLINE_SURFACE ( 1, 2, ( 
 ( #10471, #9987, #55486, #47478, #1521, #64434, #17498, #87444, #46983, #85490, #70987, #77477, #70490, #2010, #25966, #55978, #79458, #32475, #62970, #48462, #93475, #86480, #94942, #25001, #86952, #48950, #85986, #2509, #32961, #2993, #16999, #63466, #92975, #77978, #71477, #33443, #56942, #47962, #56466, #93968, #17978, #8988, #41482, #18465, #71949, #39505, #24506, #33929, #69995, #54968, #43901, #95945, #34924, #65917, #27428, #80933, #26938, #72929, #18959, #20928, #19931, #73916, #12427, #4458, #96446, #66415, #80444, #57438, #5445, #58915, #42934, #11448, #20434, #65422, #74401, #66911, #27917, #87929, #43416, #50426, #19446, #58409, #96946, #73415, #4942, #97431, #5925, #81418, #49938, #35916, #12919, #3957, #35422, #50922, #28419, #88925, #28896, #89414, #49438, #81906, #79941, #95446, #51417, #13415, #36418, #11941, #42446, #57922, #59401, #41965, #88432, #72431, #34427, #64919, #7418, #46381, #89905, #30878, #76868, #82902, #45387, #91883, #6910, #29886, #15419, #90384, #37915, #8384, #21420, #61374, #38894, #31364, #98431, #75893, #91382, #68402, #60388, #60883, #98923, #14419, #53379, #52887, #90886, #21922, #44402, #69380, #22413, #51914, #82399, #29392, #83399, #13924, #44888, #75391, #7902, #30380, #23405, #37421, #67907, #22912, #14919, #83890, #903, #52401, #53889, #84395, #45901, #76387, #38397, #68899, #59894, #428, #74903, #15894, #6403, #36914, #67406, #97936, #17856, #77854, #24383, #71836, #25852, #70870, #62854, #79337, #39384, #9870, #10847, #55859, #86846, #39867, #9363, #40369, #70375, #24876, #69878, #16877, #61864, #63821, #93351, #48342, #55359, #47352, #2385, #10356, #54851, #1398, #78847, #2877, #85863, #54363, #63341, #1892, #18350, #41368, #32839, #31853, #86355, #17376, #62352, #93847, #40855, #47845, #78349, #3344, #48827, #25373, #92855, #71360, #33327, #46865, #94335, #56349, #92369, #23895, #84872, #16381, #77357, #8867, #85364, #32350, #4827, #42819, #50812, #72312, #95319, #19327, #3844, #35803, #27803, #79825, #18841, #73304, #88804, #20811, #89300, #81784, #26820, #66290, #42325, #5323, #20314, #4338, #94825, #80813, #12311, #51300, #35302, #81303, #27305, #41846, #13298, #57313, #72799, #26328, #88313, #43786, #33807, #64800, #28300, #64313, #50300, #65794, #43299, #56827, #96328, #58286, #12799, #74278, #73792, #96824, #11329, #87324, #49321, #58793, #87806, #34302, #49811, #80318, #11819, #34809, #65297, #95824, #57805, #19811, #6297, #53767, #84283, #76273, #28788, #44285, #83775, #14304, #23289, #30753, #82785, #75281, #45782, #61260, #37305, #38285, #36799, #59288, #7790 ),
 ( #83282, #15782, #68780, #5807, #312, #36298, #82281, #75774, #14806, #22791, #74788, #67293, #97820, #60276, #91768, #21805, #44775, #30262, #29283, #22300, #46271, #66795, #97315, #89786, #21302, #6791, #90775, #7295, #52773, #67794, #37794, #45278, #59779, #68292, #98314, #29768, #90271, #51795, #13798, #98813, #52285, #60766, #91266, #53268, #15298, #8754, #71239, #8274, #93231, #55234, #86236, #38772, #9745, #70755, #32725, #86731, #17747, #40247, #23784, #33217, #63711, #78734, #39272, #47735, #10243, #78232, #17260, #77738, #2269, #63223, #93728, #55745, #77247, #25745, #56238, #48225, #793, #16269, #40736, #85254, #94214, #2763, #54734, #47235, #18234, #76756, #9249, #69273, #69761, #31246, #61742, #25259, #16762, #92260, #62730, #54249, #84761, #1289, #39758, #70258, #1774, #46750, #85748, #62239, #31743, #32230, #92745, #24269, #24756, #89058, #82044, #5579, #18729, #44042, #29525, #36055, #95194, #36562, #81546, #3232, #10729, #49209, #79713, #72202, #26221, #82545, #51558, #56715, #75040, #59546, #20573, #21063, #51056, #13056, #74044, #6546, #79217, #71723, #37058, #87205, #13556, #34191, #11213, #52053, #74545, #94714, #33698, #59051, #6063, #67555, #98066, #60032, #41731, #14062, #58552, #21564, #67051, #43550, #41246, #97085, #28556, #90528, #97576, #29037, #66557, #3730, #48715, #64684, #89553, #90041, #28056, #44544, #64198, #84032, #15553, #1541, #77495, #84527, #91023, #77013, #16024, #7052, #46037, #23546, #46513, #567, #31985, #92501, #22062, #85014, #52536, #98574, #92017, #31013, #39028, #60531, #83539, #15060, #76522, #24031, #38049, #61021, #8527, #22554, #38536, #9007, #83044, #62002, #39523, #62491, #30518, #8038, #54018, #69032, #91533, #69523, #61509, #45531, #1038, #31501, #23048, #53024, #75538, #70017, #53521, #14560, #45029, #76029, #54499, #37556, #7562, #68541, #16527, #47003, #68046, #72, #30025, #94469, #86005, #3011, #11465, #55505, #33947, #94958, #47983, #25510, #78978, #48969, #32493, #48479, #77998, #62988, #86969, #56483, #41983, #93494, #79478, #10006, #17516, #3978, #56959, #33460, #93988, #72447, #70507, #40999, #34446, #18483, #18977, #71004, #40508, #71497, #2527, #55997, #2031, #78492, #92995, #26460, #86499, #10977, #17997, #32980, #63957, #41498, #63484, #25017, #71967, #64452, #10488, #85507, #25987, #3490, #49455, #24529, #87462, #79961, #54988, #17017, #47495, #9504, #40005, #82417, #35440, #6420, #64937, #4476, #58428, #95465, #57940, #88448, #81924, #43432, #97450, #19948, #80949, #66430, #50443, #73933, #13941, #27446, #5945, #66929, #12446, #96464, #50940 ) ),
 .UNSPECIFIED., .F., .F., .F. ) 
 B_SPLINE_SURFACE_WITH_KNOTS ( ( 2, 2 ),
 ( 3, 2, 2, 2, 2, 2, 2, 2, 2, 2, 2, 2, 2, 2, 2, 2, 2, 2, 2, 2, 2, 2, 2, 2, 2, 2, 2, 2, 2, 2, 2, 2, 2, 2, 2, 2, 2, 2, 2, 2, 2, 2, 2, 2, 2, 2, 2, 2, 2, 2, 2, 2, 2, 2, 2, 2, 2, 2, 2, 2, 2, 2, 2, 2, 2, 2, 2, 2, 2, 2, 2, 2, 2, 2, 2, 2, 2, 2, 2, 2, 2, 2, 2, 2, 2, 2, 2, 2, 2, 2, 2, 2, 2, 2, 2, 2, 2, 2, 2, 2, 2, 2, 2, 2, 2, 2, 2, 2, 2, 2, 2, 2, 2, 2, 2, 2, 2, 2, 2, 2, 2, 2, 2, 2, 2, 2, 2, 2, 2, 2, 2, 2, 2, 2, 2, 2, 2, 2, 2, 2, 2, 2, 2, 2, 2, 2, 2, 2, 2, 2, 2, 2, 2, 2, 2, 2, 2, 2, 2, 2, 2, 2, 3 ),
 ( 0.000000000000000000, 1.000000000000000000 ),
 ( 0.000000000000000000, 0.005952380952380952051, 0.01190476190476190410, 0.01785714285714285615, 0.02380952380952380820, 0.02976190476190476025, 0.03571428571428571230, 0.04166666666666666435, 0.04761904761904761640, 0.05357142857142856845, 0.05952380952380952051, 0.06547619047619047949, 0.07142857142857142461, 0.07738095238095238360, 0.08333333333333332871, 0.08928571428571428770, 0.09523809523809523281, 0.1011904761904761918, 0.1071428571428571369, 0.1130952380952380959, 0.1190476190476190410, 0.1250000000000000000, 0.1309523809523809590, 0.1369047619047619180, 0.1428571428571428492, 0.1488095238095238082, 0.1547619047619047672, 0.1607142857142857262, 0.1666666666666666574, 0.1726190476190476164, 0.1785714285714285754, 0.1845238095238095344, 0.1904761904761904656, 0.1964285714285714246, 0.2023809523809523836, 0.2083333333333333426, 0.2142857142857142738, 0.2202380952380952328, 0.2261904761904761918, 0.2321428571428571508, 0.2380952380952380820, 0.2440476190476190410, 0.2500000000000000000, 0.2559523809523809312, 0.2619047619047619180, 0.2678571428571428492, 0.2738095238095238360, 0.2797619047619047672, 0.2857142857142856984, 0.2916666666666666852, 0.2976190476190476164, 0.3035714285714285476, 0.3095238095238095344, 0.3154761904761904656, 0.3214285714285714524, 0.3273809523809523836, 0.3333333333333333148, 0.3392857142857143016, 0.3452380952380952328, 0.3511904761904761640, 0.3571428571428571508, 0.3630952380952380820, 0.3690476190476190688, 0.3750000000000000000, 0.3809523809523809312, 0.3869047619047619180, 0.3928571428571428492, 0.3988095238095238360, 0.4047619047619047672, 0.4107142857142856984, 0.4166666666666666852, 0.4226190476190476164, 0.4285714285714285476, 0.4345238095238095344, 0.4404761904761904656, 0.4464285714285714524, 0.4523809523809523836, 0.4583333333333333148, 0.4642857142857143016, 0.4702380952380952328, 0.4761904761904761640, 0.4821428571428571508, 0.4880952380952380820, 0.4940476190476190688, 0.5000000000000000000, 0.5059523809523809312, 0.5119047619047618625, 0.5178571428571429047, 0.5238095238095238360, 0.5297619047619047672, 0.5357142857142856984, 0.5416666666666666297, 0.5476190476190476719, 0.5535714285714286031, 0.5595238095238095344, 0.5654761904761904656, 0.5714285714285713969, 0.5773809523809523281, 0.5833333333333333703, 0.5892857142857143016, 0.5952380952380952328, 0.6011904761904761640, 0.6071428571428570953, 0.6130952380952381375, 0.6190476190476190688, 0.6250000000000000000, 0.6309523809523809312, 0.6369047619047618625, 0.6428571428571429047, 0.6488095238095238360, 0.6547619047619047672, 0.6607142857142856984, 0.6666666666666666297, 0.6726190476190476719, 0.6785714285714286031, 0.6845238095238095344, 0.6904761904761904656, 0.6964285714285713969, 0.7023809523809523281, 0.7083333333333333703, 0.7142857142857143016, 0.7202380952380952328, 0.7261904761904761640, 0.7321428571428570953, 0.7380952380952381375, 0.7440476190476190688, 0.7500000000000000000, 0.7559523809523809312, 0.7619047619047618625, 0.7678571428571429047, 0.7738095238095238360, 0.7797619047619047672, 0.7857142857142856984, 0.7916666666666666297, 0.7976190476190476719, 0.8035714285714286031, 0.8095238095238095344, 0.8154761904761904656, 0.8214285714285713969, 0.8273809523809523281, 0.8333333333333333703, 0.8392857142857143016, 0.8452380952380952328, 0.8511904761904761640, 0.8571428571428570953, 0.8630952380952381375, 0.8690476190476190688, 0.8750000000000000000, 0.8809523809523809312, 0.8869047619047618625, 0.8928571428571429047, 0.8988095238095238360, 0.9047619047619047672, 0.9107142857142856984, 0.9166666666666666297, 0.9226190476190476719, 0.9285714285714286031, 0.9345238095238095344, 0.9404761904761904656, 0.9464285714285713969, 0.9523809523809523281, 0.9583333333333333703, 0.9642857142857143016 ),
 .UNSPECIFIED. ) 
 GEOMETRIC_REPRESENTATION_ITEM ( )  RATIONAL_B_SPLINE_SURFACE ( (
 ( 1.000000000000000000, 0.9659258262890683122, 1.000000000000000000, 0.9659258262890683122, 1.000000000000000000, 0.9659258262890683122, 1.000000000000000000, 0.9659258262890683122, 1.000000000000000000, 0.9659258262890683122, 1.000000000000000000, 0.9659258262890683122, 1.000000000000000000, 0.9659258262890683122, 1.000000000000000000, 0.9659258262890683122, 1.000000000000000000, 0.9659258262890683122, 1.000000000000000000, 0.9659258262890683122, 1.000000000000000000, 0.9659258262890683122, 1.000000000000000000, 0.9659258262890683122, 1.000000000000000000, 0.9659258262890683122, 1.000000000000000000, 0.9659258262890683122, 1.000000000000000000, 0.9659258262890683122, 1.000000000000000000, 0.9659258262890683122, 1.000000000000000000, 0.9659258262890683122, 1.000000000000000000, 0.9659258262890683122, 1.000000000000000000, 0.9659258262890683122, 1.000000000000000000, 0.9659258262890683122, 1.000000000000000000, 0.9659258262890683122, 1.000000000000000000, 0.9659258262890683122, 1.000000000000000000, 0.9659258262890683122, 1.000000000000000000, 0.9659258262890683122, 1.000000000000000000, 0.9659258262890683122, 1.000000000000000000, 0.9659258262890683122, 1.000000000000000000, 0.9659258262890683122, 1.000000000000000000, 0.9659258262890683122, 1.000000000000000000, 0.9659258262890683122, 1.000000000000000000, 0.9659258262890683122, 1.000000000000000000, 0.9659258262890683122, 1.000000000000000000, 0.9659258262890683122, 1.000000000000000000, 0.9659258262890683122, 1.000000000000000000, 0.9659258262890683122, 1.000000000000000000, 0.9659258262890683122, 1.000000000000000000, 0.9659258262890683122, 1.000000000000000000, 0.9659258262890683122, 1.000000000000000000, 0.9659258262890683122, 1.000000000000000000, 0.9659258262890683122, 1.000000000000000000, 0.9659258262890683122, 1.000000000000000000, 0.9659258262890683122, 1.000000000000000000, 0.9659258262890683122, 1.000000000000000000, 0.9659258262890683122, 1.000000000000000000, 0.9659258262890683122, 1.000000000000000000, 0.9659258262890683122, 1.000000000000000000, 0.9659258262890683122, 1.000000000000000000, 0.9659258262890683122, 1.000000000000000000, 0.9659258262890683122, 1.000000000000000000, 0.9659258262890683122, 1.000000000000000000, 0.9659258262890683122, 1.000000000000000000, 0.9659258262890683122, 1.000000000000000000, 0.9659258262890683122, 1.000000000000000000, 0.9659258262890683122, 1.000000000000000000, 0.9659258262890683122, 1.000000000000000000, 0.9659258262890683122, 1.000000000000000000, 0.9659258262890683122, 1.000000000000000000, 0.9659258262890683122, 1.000000000000000000, 0.9659258262890683122, 1.000000000000000000, 0.9659258262890683122, 1.000000000000000000, 0.9659258262890683122, 1.000000000000000000, 0.9659258262890683122, 1.000000000000000000, 0.9659258262890683122, 1.000000000000000000, 0.9659258262890683122, 1.000000000000000000, 0.9659258262890683122, 1.000000000000000000, 0.9659258262890683122, 1.000000000000000000, 0.9659258262890683122, 1.000000000000000000, 0.9659258262890683122, 1.000000000000000000, 0.9659258262890683122, 1.000000000000000000, 0.9659258262890683122, 1.000000000000000000, 0.9659258262890683122, 1.000000000000000000, 0.9659258262890683122, 1.000000000000000000, 0.9659258262890683122, 1.000000000000000000, 0.9659258262890683122, 1.000000000000000000, 0.9659258262890683122, 1.000000000000000000, 0.9659258262890683122, 1.000000000000000000, 0.9659258262890683122, 1.000000000000000000, 0.9659258262890683122, 1.000000000000000000, 0.9659258262890683122, 1.000000000000000000, 0.9659258262890683122, 1.000000000000000000, 0.9659258262890683122, 1.000000000000000000, 0.9659258262890683122, 1.000000000000000000, 0.9659258262890683122, 1.000000000000000000, 0.9659258262890683122, 1.000000000000000000, 0.9659258262890683122, 1.000000000000000000, 0.9659258262890683122, 1.000000000000000000, 0.9659258262890683122, 1.000000000000000000, 0.9659258262890683122, 1.000000000000000000, 0.9659258262890683122, 1.000000000000000000, 0.9659258262890683122, 1.000000000000000000, 0.9659258262890683122, 1.000000000000000000, 0.9659258262890683122, 1.000000000000000000, 0.9659258262890683122, 1.000000000000000000, 0.9659258262890683122, 1.000000000000000000, 0.9659258262890683122, 1.000000000000000000, 0.9659258262890683122, 1.000000000000000000, 0.9659258262890683122, 1.000000000000000000, 0.9659258262890683122, 1.000000000000000000, 0.9659258262890683122, 1.000000000000000000, 0.9659258262890683122, 1.000000000000000000, 0.9659258262890683122, 1.000000000000000000, 0.9659258262890683122, 1.000000000000000000, 0.9659258262890683122, 1.000000000000000000, 0.9659258262890683122, 1.000000000000000000, 0.9659258262890683122, 1.000000000000000000, 0.9659258262890683122, 1.000000000000000000, 0.9659258262890683122, 1.000000000000000000, 0.9659258262890683122, 1.000000000000000000, 0.9659258262890683122, 1.000000000000000000, 0.9659258262890683122, 1.000000000000000000, 0.9659258262890683122, 1.000000000000000000, 0.9659258262890683122, 1.000000000000000000, 0.9659258262890683122, 1.000000000000000000, 0.9659258262890683122, 1.000000000000000000, 0.9659258262890683122, 1.000000000000000000, 0.9659258262890683122, 1.000000000000000000, 0.9659258262890683122, 1.000000000000000000, 0.9659258262890683122, 1.000000000000000000, 0.9659258262890683122, 1.000000000000000000, 0.9659258262890683122, 1.000000000000000000, 0.9659258262890683122, 1.000000000000000000, 0.9659258262890683122, 1.000000000000000000, 0.9659258262890683122, 1.000000000000000000, 0.9659258262890683122, 1.000000000000000000, 0.9659258262890683122, 1.000000000000000000, 0.9659258262890683122, 1.000000000000000000, 0.9659258262890683122, 1.000000000000000000, 0.9659258262890683122, 1.000000000000000000, 0.9659258262890683122, 1.000000000000000000, 0.9659258262890683122, 1.000000000000000000, 0.9659258262890683122, 1.000000000000000000, 0.9659258262890683122, 1.000000000000000000, 0.9659258262890683122, 1.000000000000000000, 0.9659258262890683122, 1.000000000000000000, 0.9659258262890683122, 1.000000000000000000, 0.9659258262890683122, 1.000000000000000000, 0.9659258262890683122, 1.000000000000000000, 0.9659258262890683122, 1.000000000000000000, 0.9659258262890683122, 1.000000000000000000, 0.9659258262890683122, 1.000000000000000000, 0.9659258262890683122, 1.000000000000000000, 0.9659258262890683122, 1.000000000000000000, 0.9659258262890683122, 1.000000000000000000, 0.9659258262890683122, 1.000000000000000000, 0.9659258262890683122, 1.000000000000000000, 0.9659258262890683122, 1.000000000000000000, 0.9659258262890683122, 1.000000000000000000, 0.9659258262890683122, 1.000000000000000000, 0.9659258262890683122, 1.000000000000000000, 0.9659258262890683122, 1.000000000000000000, 0.9659258262890683122, 1.000000000000000000, 0.9659258262890683122, 1.000000000000000000, 0.9659258262890683122, 1.000000000000000000, 0.9659258262890683122, 1.000000000000000000, 0.9659258262890683122, 1.000000000000000000, 0.9659258262890683122, 1.000000000000000000, 0.9659258262890683122, 1.000000000000000000, 0.9659258262890683122, 1.000000000000000000, 0.9659258262890683122, 1.000000000000000000, 0.9659258262890683122, 1.000000000000000000, 0.9659258262890683122, 1.000000000000000000, 0.9659258262890683122, 1.000000000000000000, 0.9659258262890683122, 1.000000000000000000),
 ( 1.000000000000000000, 0.9659258262890683122, 1.000000000000000000, 0.9659258262890683122, 1.000000000000000000, 0.9659258262890683122, 1.000000000000000000, 0.9659258262890683122, 1.000000000000000000, 0.9659258262890683122, 1.000000000000000000, 0.9659258262890683122, 1.000000000000000000, 0.9659258262890683122, 1.000000000000000000, 0.9659258262890683122, 1.000000000000000000, 0.9659258262890683122, 1.000000000000000000, 0.9659258262890683122, 1.000000000000000000, 0.9659258262890683122, 1.000000000000000000, 0.9659258262890683122, 1.000000000000000000, 0.9659258262890683122, 1.000000000000000000, 0.9659258262890683122, 1.000000000000000000, 0.9659258262890683122, 1.000000000000000000, 0.9659258262890683122, 1.000000000000000000, 0.9659258262890683122, 1.000000000000000000, 0.9659258262890683122, 1.000000000000000000, 0.9659258262890683122, 1.000000000000000000, 0.9659258262890683122, 1.000000000000000000, 0.9659258262890683122, 1.000000000000000000, 0.9659258262890683122, 1.000000000000000000, 0.9659258262890683122, 1.000000000000000000, 0.9659258262890683122, 1.000000000000000000, 0.9659258262890683122, 1.000000000000000000, 0.9659258262890683122, 1.000000000000000000, 0.9659258262890683122, 1.000000000000000000, 0.9659258262890683122, 1.000000000000000000, 0.9659258262890683122, 1.000000000000000000, 0.9659258262890683122, 1.000000000000000000, 0.9659258262890683122, 1.000000000000000000, 0.9659258262890683122, 1.000000000000000000, 0.9659258262890683122, 1.000000000000000000, 0.9659258262890683122, 1.000000000000000000, 0.9659258262890683122, 1.000000000000000000, 0.9659258262890683122, 1.000000000000000000, 0.9659258262890683122, 1.000000000000000000, 0.9659258262890683122, 1.000000000000000000, 0.9659258262890683122, 1.000000000000000000, 0.9659258262890683122, 1.000000000000000000, 0.9659258262890683122, 1.000000000000000000, 0.9659258262890683122, 1.000000000000000000, 0.9659258262890683122, 1.000000000000000000, 0.9659258262890683122, 1.000000000000000000, 0.9659258262890683122, 1.000000000000000000, 0.9659258262890683122, 1.000000000000000000, 0.9659258262890683122, 1.000000000000000000, 0.9659258262890683122, 1.000000000000000000, 0.9659258262890683122, 1.000000000000000000, 0.9659258262890683122, 1.000000000000000000, 0.9659258262890683122, 1.000000000000000000, 0.9659258262890683122, 1.000000000000000000, 0.9659258262890683122, 1.000000000000000000, 0.9659258262890683122, 1.000000000000000000, 0.9659258262890683122, 1.000000000000000000, 0.9659258262890683122, 1.000000000000000000, 0.9659258262890683122, 1.000000000000000000, 0.9659258262890683122, 1.000000000000000000, 0.9659258262890683122, 1.000000000000000000, 0.9659258262890683122, 1.000000000000000000, 0.9659258262890683122, 1.000000000000000000, 0.9659258262890683122, 1.000000000000000000, 0.9659258262890683122, 1.000000000000000000, 0.9659258262890683122, 1.000000000000000000, 0.9659258262890683122, 1.000000000000000000, 0.9659258262890683122, 1.000000000000000000, 0.9659258262890683122, 1.000000000000000000, 0.9659258262890683122, 1.000000000000000000, 0.9659258262890683122, 1.000000000000000000, 0.9659258262890683122, 1.000000000000000000, 0.9659258262890683122, 1.000000000000000000, 0.9659258262890683122, 1.000000000000000000, 0.9659258262890683122, 1.000000000000000000, 0.9659258262890683122, 1.000000000000000000, 0.9659258262890683122, 1.000000000000000000, 0.9659258262890683122, 1.000000000000000000, 0.9659258262890683122, 1.000000000000000000, 0.9659258262890683122, 1.000000000000000000, 0.9659258262890683122, 1.000000000000000000, 0.9659258262890683122, 1.000000000000000000, 0.9659258262890683122, 1.000000000000000000, 0.9659258262890683122, 1.000000000000000000, 0.9659258262890683122, 1.000000000000000000, 0.9659258262890683122, 1.000000000000000000, 0.9659258262890683122, 1.000000000000000000, 0.9659258262890683122, 1.000000000000000000, 0.9659258262890683122, 1.000000000000000000, 0.9659258262890683122, 1.000000000000000000, 0.9659258262890683122, 1.000000000000000000, 0.9659258262890683122, 1.000000000000000000, 0.9659258262890683122, 1.000000000000000000, 0.9659258262890683122, 1.000000000000000000, 0.9659258262890683122, 1.000000000000000000, 0.9659258262890683122, 1.000000000000000000, 0.9659258262890683122, 1.000000000000000000, 0.9659258262890683122, 1.000000000000000000, 0.9659258262890683122, 1.000000000000000000, 0.9659258262890683122, 1.000000000000000000, 0.9659258262890683122, 1.000000000000000000, 0.9659258262890683122, 1.000000000000000000, 0.9659258262890683122, 1.000000000000000000, 0.9659258262890683122, 1.000000000000000000, 0.9659258262890683122, 1.000000000000000000, 0.9659258262890683122, 1.000000000000000000, 0.9659258262890683122, 1.000000000000000000, 0.9659258262890683122, 1.000000000000000000, 0.9659258262890683122, 1.000000000000000000, 0.9659258262890683122, 1.000000000000000000, 0.9659258262890683122, 1.000000000000000000, 0.9659258262890683122, 1.000000000000000000, 0.9659258262890683122, 1.000000000000000000, 0.9659258262890683122, 1.000000000000000000, 0.9659258262890683122, 1.000000000000000000, 0.9659258262890683122, 1.000000000000000000, 0.9659258262890683122, 1.000000000000000000, 0.9659258262890683122, 1.000000000000000000, 0.9659258262890683122, 1.000000000000000000, 0.9659258262890683122, 1.000000000000000000, 0.9659258262890683122, 1.000000000000000000, 0.9659258262890683122, 1.000000000000000000, 0.9659258262890683122, 1.000000000000000000, 0.9659258262890683122, 1.000000000000000000, 0.9659258262890683122, 1.000000000000000000, 0.9659258262890683122, 1.000000000000000000, 0.9659258262890683122, 1.000000000000000000, 0.9659258262890683122, 1.000000000000000000, 0.9659258262890683122, 1.000000000000000000, 0.9659258262890683122, 1.000000000000000000, 0.9659258262890683122, 1.000000000000000000, 0.9659258262890683122, 1.000000000000000000, 0.9659258262890683122, 1.000000000000000000, 0.9659258262890683122, 1.000000000000000000, 0.9659258262890683122, 1.000000000000000000, 0.9659258262890683122, 1.000000000000000000, 0.9659258262890683122, 1.000000000000000000, 0.9659258262890683122, 1.000000000000000000, 0.9659258262890683122, 1.000000000000000000, 0.9659258262890683122, 1.000000000000000000, 0.9659258262890683122, 1.000000000000000000, 0.9659258262890683122, 1.000000000000000000, 0.9659258262890683122, 1.000000000000000000, 0.9659258262890683122, 1.000000000000000000, 0.9659258262890683122, 1.000000000000000000, 0.9659258262890683122, 1.000000000000000000, 0.9659258262890683122, 1.000000000000000000, 0.9659258262890683122, 1.000000000000000000, 0.9659258262890683122, 1.000000000000000000, 0.9659258262890683122, 1.000000000000000000, 0.9659258262890683122, 1.000000000000000000, 0.9659258262890683122, 1.000000000000000000, 0.9659258262890683122, 1.000000000000000000, 0.9659258262890683122, 1.000000000000000000, 0.9659258262890683122, 1.000000000000000000, 0.9659258262890683122, 1.000000000000000000, 0.9659258262890683122, 1.000000000000000000, 0.9659258262890683122, 1.000000000000000000, 0.9659258262890683122, 1.000000000000000000, 0.9659258262890683122, 1.000000000000000000, 0.9659258262890683122, 1.000000000000000000, 0.9659258262890683122, 1.000000000000000000, 0.9659258262890683122, 1.000000000000000000, 0.9659258262890683122, 1.000000000000000000) ) ) 
 REPRESENTATION_ITEM ( '' )  SURFACE ( )  );
#56962 = CARTESIAN_POINT ( 'NONE',  ( -11.62551083756942027, -75.79479195806536040, -3.750000000000000444 ) ) ;
#56963 = CARTESIAN_POINT ( 'NONE',  ( 14.92337183194729988, 54.34226448433412315, -8.527530157486177487 ) ) ;
#56964 = CARTESIAN_POINT ( 'NONE',  ( 1.472469842513823179, 5.592264484334118713, -4.923371831947296329 ) ) ;
#56965 = CARTESIAN_POINT ( 'NONE',  ( 9.382169495545419124, -34.00136533006956796, 9.382169495545417348 ) ) ;
#56966 = ORIENTED_EDGE ( 'NONE', *, *, #7589, .F. ) ;
#56967 = CARTESIAN_POINT ( 'NONE',  ( 15.44008868035555260, 14.73035201082150536, 9.422509992056143702 ) ) ;
#56968 = CARTESIAN_POINT ( 'NONE',  ( 17.20831665107776587, 12.88393115100078390, 7.208316651077764980 ) ) ;
#56969 = CARTESIAN_POINT ( 'NONE',  ( -2.816281873526473856, 4.123634669930420493, 9.499525473075851096E-16 ) ) ;
#56970 = CARTESIAN_POINT ( 'NONE',  ( 4.559911319644449179, 42.23035201082151247, -9.422509992056141925 ) ) ;
#56972 = CARTESIAN_POINT ( 'NONE',  ( 3.591859063236763294, 48.29030133659708923, -11.09922568453595026 ) ) ;
#56971 = CARTESIAN_POINT ( 'NONE',  ( 19.42250999205614193, 15.14701867748817143, 5.440088680355555262 ) ) ;
#56973 = CARTESIAN_POINT ( 'NONE',  ( 13.79529636645030344, 38.26208216824729647, 14.16423886937410614 ) ) ;
#56975 = CARTESIAN_POINT ( 'NONE',  ( -1.099225684535947600, 54.54030133659708923, 6.408140936763237150 ) ) ;
#56974 = AXIS2_PLACEMENT_3D ( 'NONE', #80116, #42140, #72605 ) ;
#56976 = ORIENTED_EDGE ( 'NONE', *, *, #51816, .F. ) ;
#56977 = CARTESIAN_POINT ( 'NONE',  ( 0.1532563361054100626, 60.80059781766744464, -2.638427012816831230 ) ) ;
#56978 = CARTESIAN_POINT ( 'NONE',  ( 6.565887622018943937, 65.16530133659709634, 12.81628187352647430 ) ) ;
#56979 = CARTESIAN_POINT ( 'NONE',  ( -0.8801773607111009756, 28.06368534415484106, 1.068504757029289695E-15 ) ) ;
#56980 = CARTESIAN_POINT ( 'NONE',  ( 10.00000000000000000, 59.75893115100078745, -9.846743663894594434 ) ) ;
#56981 = ORIENTED_EDGE ( 'NONE', *, *, #18789, .T. ) ;
#56983 = CARTESIAN_POINT ( 'NONE',  ( -5.559536763064313547, -36.09058695999160449, 2.499999999999999112 ) ) ;
#56982 = CARTESIAN_POINT ( 'NONE',  ( 0.1532563361054100626, 5.800597817667452638, -2.638427012816831230 ) ) ;
#56984 = CARTESIAN_POINT ( 'NONE',  ( 14.92337183194729633, 22.67559781766745175, 8.527530157486181039 ) ) ;
#56985 = CARTESIAN_POINT ( 'NONE',  ( 19.84674366389459266, 8.717264484334116048, -2.638427012816827677 ) ) ;
#56986 = TOROIDAL_SURFACE ( 'NONE', #92119, 14.49999999999999822, 0.5000000000000000000 ) ;
#56987 = SURFACE_STYLE_FILL_AREA ( #88473 ) ;
#56988 = EDGE_CURVE ( 'NONE', #3803, #48202, #38674, .T. ) ;
#56991 = CARTESIAN_POINT ( 'NONE',  ( 1.274849032794292736, 37.55509018479936145, -6.499999999999977796 ) ) ;
#56990 = CIRCLE ( 'NONE', #82564, 14.49999999999999822 ) ;
#56989 = CARTESIAN_POINT ( 'NONE',  ( 2.035157376598824452, 53.68868534415484817, 7.964842623401179544 ) ) ;
#56992 = CARTESIAN_POINT ( 'NONE',  ( 17.96484262340118221, 64.93868534415483396, 7.964842623401181321 ) ) ;
#56994 = EDGE_LOOP ( 'NONE', ( #3398, #35918, #93971, #40064 ) ) ;
#56993 = CARTESIAN_POINT ( 'NONE',  ( 18.52753015748618282, 13.92559781766745175, -4.923371831947291888 ) ) ;
#56995 = PRESENTATION_LAYER_ASSIGNMENT (  '', '', ( #95329 ) ) ;
#56996 = CARTESIAN_POINT ( 'NONE',  ( 14.62617646268089011, 0.3639308321805998503, 3.327906561566976951 ) ) ;
#56997 = TOROIDAL_SURFACE ( 'NONE', #76138, 14.49999999999999822, 0.5000000000000000000 ) ;
#56998 = CARTESIAN_POINT ( 'NONE',  ( 7.361572987183169658, 59.96726448433410894, -9.846743663894592657 ) ) ;
#56999 = ORIENTED_EDGE ( 'NONE', *, *, #4609, .F. ) ;
#57000 = ORIENTED_EDGE ( 'NONE', *, *, #13850, .T. ) ;
#57001 = CARTESIAN_POINT ( 'NONE',  ( -9.159723438033054776, 0.000000000000000000, -10.91613331444555079 ) ) ;
#57002 = CARTESIAN_POINT ( 'NONE',  ( 20.36894250292379382, 18.67874883491397142, 10.36894250292379205 ) ) ;
#57003 = CARTESIAN_POINT ( 'NONE',  ( 0.5600000000000083800, 105.0000000000000000, -4.500000000000001776 ) ) ;
#57004 = CARTESIAN_POINT ( 'NONE',  ( 6.204703633549690345, 17.84541550158063217, 14.16423886937410082 ) ) ;
#57005 = CARTESIAN_POINT ( 'NONE',  ( -4.164238869374099927, 27.01208216824730357, 3.795296366450308767 ) ) ;
#57006 = SURFACE_STYLE_FILL_AREA ( #34491 ) ;
#57007 = CARTESIAN_POINT ( 'NONE',  ( 7.084665262690076126, 37.02201867748817676, -10.88017736071110164 ) ) ;
#57008 = PRESENTATION_STYLE_ASSIGNMENT (( #18044 ) ) ;
#57009 = EDGE_LOOP ( 'NONE', ( #52077, #28150, #96810, #88592 ) ) ;
#57010 = CARTESIAN_POINT ( 'NONE',  ( 0.1532563361054083140, 21.00893115100078745, 1.131784320476157264E-15 ) ) ;
#57011 =( GEOMETRIC_REPRESENTATION_CONTEXT ( 3 ) GLOBAL_UNCERTAINTY_ASSIGNED_CONTEXT ( ( #80161 ) ) GLOBAL_UNIT_ASSIGNED_CONTEXT ( ( #16742, #63691, #77230 ) ) REPRESENTATION_CONTEXT ( 'NONE', 'WORKASPACE' ) );
#57013 = CARTESIAN_POINT ( 'NONE',  ( 2.791683348922240793, 16.63393115100078745, 7.208316651077764092 ) ) ;
#57012 = CARTESIAN_POINT ( 'NONE',  ( 15.44008868035555260, 54.73035201082150536, 9.422509992056143702 ) ) ;
#57014 = CARTESIAN_POINT ( 'NONE',  ( 13.43411237798105340, 45.58196800326374643, 12.81628187352647963 ) ) ;
#57015 = CARTESIAN_POINT ( 'NONE',  ( 0.1532563361054082862, 41.21726448433411605, 2.638427012816831674 ) ) ;
#57016 = DIRECTION ( 'NONE',  ( 0.000000000000000000, 0.000000000000000000, 1.000000000000000000 ) ) ;
#57017 = CARTESIAN_POINT ( 'NONE',  ( 0.6178305044545838731, 29.74863466993042138, 9.382169495545420901 ) ) ;
#57018 = CARTESIAN_POINT ( 'NONE',  ( 3.795296366450314540, -31.73791783175269288, 14.16423886937410082 ) ) ;
#57019 = CARTESIAN_POINT ( 'NONE',  ( 2.791683348922237240, 20.38393115100078745, -7.208316651077763204 ) ) ;
#57020 = CARTESIAN_POINT ( 'NONE',  ( 13.79529636645030344, 18.26208216824730002, 14.16423886937410614 ) ) ;
#57021 = EDGE_CURVE ( 'NONE', #63243, #62370, #93756, .T. ) ;
#57022 = VERTEX_POINT ( 'NONE', #72356 ) ;
#57023 =( GEOMETRIC_REPRESENTATION_CONTEXT ( 3 ) GLOBAL_UNCERTAINTY_ASSIGNED_CONTEXT ( ( #69114 ) ) GLOBAL_UNIT_ASSIGNED_CONTEXT ( ( #57296, #4314, #3825 ) ) REPRESENTATION_CONTEXT ( 'NONE', 'WORKASPACE' ) );
#57024 = CARTESIAN_POINT ( 'NONE',  ( 17.96484262340118221, 44.93868534415483396, 7.964842623401181321 ) ) ;
#57025 = CARTESIAN_POINT ( 'NONE',  ( 17.96484262340118221, 54.93868534415484106, 7.964842623401181321 ) ) ;
#57026 = CARTESIAN_POINT ( 'NONE',  ( 17.08211943468705130, 48.47041550158063927, 12.26659068614894998 ) ) ;
#57027 = CARTESIAN_POINT ( 'NONE',  ( 18.52753015748618282, 58.92559781766745886, -4.923371831947291888 ) ) ;
#57028 = CARTESIAN_POINT ( 'NONE',  ( 0.1532563361054100626, 10.80059781766745175, -2.638427012816831230 ) ) ;
#57030 = CARTESIAN_POINT ( 'NONE',  ( -11.80960303780298126, 90.32667112043513669, 7.004222671090198027 ) ) ;
#57029 = CARTESIAN_POINT ( 'NONE',  ( 10.00000000000000178, 60.37363466993041783, 12.81628187352647608 ) ) ;
#57031 = CARTESIAN_POINT ( 'NONE',  ( 7.084665262690076126, 47.02201867748818387, -10.88017736071110164 ) ) ;
#57032 = ADVANCED_FACE ( 'NONE', ( #3889 ), #52297, .F. ) ;
#57033 = CARTESIAN_POINT ( 'NONE',  ( -6.356754967080490815, -50.93964766207073325, -2.500000000000000000 ) ) ;
#57034 = CARTESIAN_POINT ( 'NONE',  ( 0.1532563361054100626, 55.80059781766745175, -2.638427012816831230 ) ) ;
#57035 = CARTESIAN_POINT ( 'NONE',  ( -10.88017736071110342, 18.06368534415484106, 3.903127820947815962E-15 ) ) ;
#57036 =( NAMED_UNIT ( * ) PLANE_ANGLE_UNIT ( ) SI_UNIT ( $, .RADIAN. ) );
#57037 = CARTESIAN_POINT ( 'NONE',  ( 0.5774900079438607392, 68.48035201082150536, 5.440088680355550821 ) ) ;
#57038 = CARTESIAN_POINT ( 'NONE',  ( 7.084665262690076126, 2.022018677488170990, -10.88017736071110164 ) ) ;
#57039 = DIRECTION ( 'NONE',  ( -0.000000000000000000, -1.000000000000000000, -0.000000000000000000 ) ) ;
#57040 = CARTESIAN_POINT ( 'NONE',  ( 0.5774900079438607392, 68.48035201082150536, 5.440088680355550821 ) ) ;
#57041 = AXIS2_PLACEMENT_3D ( 'NONE', #16732, #62702, #47209 ) ;
#57042 = CARTESIAN_POINT ( 'NONE',  ( 17.20831665107776587, 4.133931151000785675, -7.208316651077762316 ) ) ;
#57043 = CARTESIAN_POINT ( 'NONE',  ( 18.00000000000000000, 77.66934307245453795, -4.068269658013956125 ) ) ;
#57044 = CARTESIAN_POINT ( 'NONE',  ( 10.00000000000000178, 37.25893115100078745, 9.846743663894594434 ) ) ;
#57045 = MECHANICAL_DESIGN_GEOMETRIC_PRESENTATION_REPRESENTATION (  '', ( #44277 ), #93386 ) ;
#57046 = CARTESIAN_POINT ( 'NONE',  ( 2.035157376598822676, 17.43868534415483751, -7.964842623401177768 ) ) ;
#57047 = CARTESIAN_POINT ( 'NONE',  ( 10.00000000000000178, 0.3736346699304200492, 12.81628187352647608 ) ) ;
#57049 = DIRECTION ( 'NONE',  ( -0.000000000000000000, -1.000000000000000000, -0.000000000000000000 ) ) ;
#57048 = CARTESIAN_POINT ( 'NONE',  ( 17.96484262340118221, 41.18868534415484106, -7.964842623401177768 ) ) ;
#57050 = CYLINDRICAL_SURFACE ( 'NONE', #59284, 0.5000000000000004441 ) ;
#57051 = CARTESIAN_POINT ( 'NONE',  ( 6.565887622018943937, 35.16530133659708923, 12.81628187352647430 ) ) ;
#57052 = EDGE_LOOP ( 'NONE', ( #3853, #61173, #55215, #25663, #93879, #39573 ) ) ;
#57053 = CARTESIAN_POINT ( 'NONE',  ( 10.00000000000000178, 54.31368534415484106, 10.88017736071110342 ) ) ;
#57055 = FILL_AREA_STYLE ('',( #89037 ) ) ;
#57054 = CARTESIAN_POINT ( 'NONE',  ( 13.43411237798106583, 22.66530133659708923, -12.81628187352647252 ) ) ;
#57056 = CARTESIAN_POINT ( 'NONE',  ( 15.44008868035555260, 24.73035201082150891, 9.422509992056143702 ) ) ;
#57057 = CARTESIAN_POINT ( 'NONE',  ( 24.16423886937410614, 64.51208216824728936, -3.795296366450302550 ) ) ;
#57058 = AXIS2_PLACEMENT_3D ( 'NONE', #8783, #39302, #52803 ) ;
#57059 = CARTESIAN_POINT ( 'NONE',  ( 1.472469842513823179, 40.59226448433411605, -4.923371831947296329 ) ) ;
#57060 = CARTESIAN_POINT ( 'NONE',  ( 10.00000000000000000, 4.758931151000784787, -9.846743663894594434 ) ) ;
#57061 = CARTESIAN_POINT ( 'NONE',  ( -0.8801773607110991993, 62.85535201082150536, -2.915334737309923874 ) ) ;
#57062 = CARTESIAN_POINT ( 'NONE',  ( -4.838527690343426002, 14.49999999999999112, -14.19819177887740302 ) ) ;
#57063 = CARTESIAN_POINT ( 'NONE',  ( 10.00000000000000178, 33.05374883491396787, 14.16423886937410082 ) ) ;
#57064 = B_SPLINE_CURVE_WITH_KNOTS ( 'NONE', 3,
 ( #1293, #78738, #16272, #84764, #86239, #93731 ),
 .UNSPECIFIED., .F., .F.,
 ( 4, 2, 4 ),
 ( 3.409110551494646011E-05, 0.0004400426677367923179, 0.0008459942299586381553 ),
 .UNSPECIFIED. ) ;
#57065 = CIRCLE ( 'NONE', #79414, 15.00000000000000000 ) ;
#57066 = EDGE_CURVE ( 'NONE', #94701, #88316, #62898, .T. ) ;
#57067 = TOROIDAL_SURFACE ( 'NONE', #69867, 14.49999999999999822, 0.5000000000000000000 ) ;
#57068 = CARTESIAN_POINT ( 'NONE',  ( -9.323033696085090583, 0.04962895454604727974, 11.43408728005506880 ) ) ;
#57069 = CARTESIAN_POINT ( 'NONE',  ( -3.500000000000000444, 0.08393865084444233904, -3.750000000002423839 ) ) ;
#57070 = CIRCLE ( 'NONE', #88980, 1.750000000000000666 ) ;
#57071 = ORIENTED_EDGE ( 'NONE', *, *, #10978, .F. ) ;
#57072 = VERTEX_POINT ( 'NONE', #24923 ) ;
#57073 = CARTESIAN_POINT ( 'NONE',  ( 6.204703633549690345, 42.84541550158063217, 14.16423886937410082 ) ) ;
#57074 = CARTESIAN_POINT ( 'NONE',  ( 13.79529636645031943, 45.34541550158062506, -14.16423886937409904 ) ) ;
#57075 = CARTESIAN_POINT ( 'NONE',  ( 14.92337183194729633, 12.67559781766745353, 8.527530157486181039 ) ) ;
#57076 = CARTESIAN_POINT ( 'NONE',  ( -1.099225684535947600, 13.70696800326375353, -6.408140936763238038 ) ) ;
#57077 = DIRECTION ( 'NONE',  ( 0.000000000000000000, 0.000000000000000000, 1.000000000000000000 ) ) ;
#57078 = FACE_OUTER_BOUND ( 'NONE', #63791, .T. ) ;
#57080 = CARTESIAN_POINT ( 'NONE',  ( 10.00000000000000178, 30.37363466993042138, 12.81628187352647608 ) ) ;
#57079 = CARTESIAN_POINT ( 'NONE',  ( 20.88017736071110519, 5.563685344154837509, 2.639326808657452039E-16 ) ) ;
#57081 = CARTESIAN_POINT ( 'NONE',  ( 6.204703633549690345, 40.76208216824731778, -14.16423886937410259 ) ) ;
#57082 =( NAMED_UNIT ( * ) SI_UNIT ( $, .STERADIAN. ) SOLID_ANGLE_UNIT ( ) );
#57083 = ADVANCED_FACE ( 'NONE', ( #55406 ), #85909, .F. ) ;
#57084 = CARTESIAN_POINT ( 'NONE',  ( 7.208316651077764980, -2.116068848999217877, 7.208316651077762316 ) ) ;
#57085 = ORIENTED_EDGE ( 'NONE', *, *, #62588, .F. ) ;
#57086 = CARTESIAN_POINT ( 'NONE',  ( 17.75000000000000000, 77.07179676972445748, 6.500000000000000888 ) ) ;
#57087 = CARTESIAN_POINT ( 'NONE',  ( 1.472469842513823179, 25.59226448433412315, -4.923371831947296329 ) ) ;
#57088 = FILL_AREA_STYLE ('',( #88568 ) ) ;
#57089 = ORIENTED_EDGE ( 'NONE', *, *, #34413, .T. ) ;
#57091 = CARTESIAN_POINT ( 'NONE',  ( 2.035157376598824452, 13.68868534415483751, 7.964842623401179544 ) ) ;
#57090 = CARTESIAN_POINT ( 'NONE',  ( 10.00000000000000000, 11.81368534415483751, -10.88017736071110342 ) ) ;
#57093 = CARTESIAN_POINT ( 'NONE',  ( 10.00000000000000178, 5.373634669930420493, 12.81628187352647608 ) ) ;
#57092 = CARTESIAN_POINT ( 'NONE',  ( 5.076628168052703671, 46.84226448433412315, 8.527530157486179263 ) ) ;
#57094 = LINE ( 'NONE', #64088, #61522 ) ;
#57095 = CARTESIAN_POINT ( 'NONE',  ( 13.43411237798106583, 17.66530133659708923, -12.81628187352647252 ) ) ;
#57096 = ORIENTED_EDGE ( 'NONE', *, *, #89212, .T. ) ;
#57097 = CARTESIAN_POINT ( 'NONE',  ( 22.26659068614895176, 64.72041550158064638, -7.082119434687042414 ) ) ;
#57098 = EDGE_LOOP ( 'NONE', ( #60916, #20343, #72113, #68051 ) ) ;
#57099 = CARTESIAN_POINT ( 'NONE',  ( -4.164238869374099927, 52.01208216824729647, 3.795296366450308767 ) ) ;
#57100 = ORIENTED_EDGE ( 'NONE', *, *, #60095, .T. ) ;
#57101 = CARTESIAN_POINT ( 'NONE',  ( 2.035157376598824452, 28.68868534415484106, 7.964842623401179544 ) ) ;
#57102 = CARTESIAN_POINT ( 'NONE',  ( 10.00000000000000000, 46.81368534415484106, -10.88017736071110342 ) ) ;
#57103 = VECTOR ( 'NONE', #38223, 1000.000000000000000 ) ;
#57104 = CARTESIAN_POINT ( 'NONE',  ( 10.00000000000000000, 46.81368534415484106, -10.88017736071110342 ) ) ;
#57105 = CARTESIAN_POINT ( 'NONE',  ( 2.035157376598822676, 47.43868534415484817, -7.964842623401177768 ) ) ;
#57106 = EDGE_CURVE ( 'NONE', #44178, #41402, #82621, .T. ) ;
#57107 = DIRECTION ( 'NONE',  ( 0.000000000000000000, 0.000000000000000000, -1.000000000000000000 ) ) ;
#57108 = CARTESIAN_POINT ( 'NONE',  ( 2.791683348922237240, 10.38393115100078390, -7.208316651077763204 ) ) ;
#57109 = VERTEX_POINT ( 'NONE', #50349 ) ;
#57110 = CARTESIAN_POINT ( 'NONE',  ( 10.95672398092068711, -56.81605919578149155, 4.000000000000000000 ) ) ;
#57111 = CARTESIAN_POINT ( 'NONE',  ( 0.1532563361054100626, 45.80059781766745886, -2.638427012816831230 ) ) ;
#57112 = ADVANCED_FACE ( 'NONE', ( #91186 ), #53682, .T. ) ;
#57113 = CARTESIAN_POINT ( 'NONE',  ( 4.879999999999991900, 76.07179676972444327, 6.500000000000000888 ) ) ;
#57114 = CARTESIAN_POINT ( 'NONE',  ( -2.816281873526473856, 54.12363466993041783, 9.499525473075851096E-16 ) ) ;
#57115 = CARTESIAN_POINT ( 'NONE',  ( -3.990799379706100325, -9.967613007074422882, 3.750000000000000444 ) ) ;
#57116 = VECTOR ( 'NONE', #65682, 1000.000000000000000 ) ;
#57117 = CARTESIAN_POINT ( 'NONE',  ( -1.780824192092292924, 0.5000000000000004441, -14.89391369643515795 ) ) ;
#57118 = CARTESIAN_POINT ( 'NONE',  ( -3.771484213771641336, -6.414706846149704766, 3.750000000000001332 ) ) ;
#57119 = CARTESIAN_POINT ( 'NONE',  ( 0.1532563361054100626, 65.80059781766745175, -2.638427012816831230 ) ) ;
#57120 = CARTESIAN_POINT ( 'NONE',  ( 13.79529636645030344, 58.26208216824728936, 14.16423886937410614 ) ) ;
#57121 = CARTESIAN_POINT ( 'NONE',  ( 0.3093388210927633941, 15.00000000000000000, 14.99680997725065978 ) ) ;
#57122 = ORIENTED_EDGE ( 'NONE', *, *, #44244, .T. ) ;
#57123 = CARTESIAN_POINT ( 'NONE',  ( 14.47650479471825058, 14.49999999999999112, 3.928206833722148517 ) ) ;
#57124 = CARTESIAN_POINT ( 'NONE',  ( 10.00000000000000178, 27.25893115100078390, 9.846743663894594434 ) ) ;
#57125 = ADVANCED_FACE ( 'NONE', ( #7209 ), #65042, .T. ) ;
#57126 = DIRECTION ( 'NONE',  ( 0.000000000000000000, 0.000000000000000000, 1.000000000000000000 ) ) ;
#57127 = CARTESIAN_POINT ( 'NONE',  ( 16.40814093676323893, 5.790301336597087456, 11.09922568453595026 ) ) ;
#57128 = CARTESIAN_POINT ( 'NONE',  ( 4.559911319644449179, 67.23035201082150536, -9.422509992056141925 ) ) ;
#57129 = COLOUR_RGB ( '', 0.08235294, 0.09019608, 0.10196078) ;
#57130 = SURFACE_STYLE_USAGE ( .BOTH. , #49145 ) ;
#57131 = CARTESIAN_POINT ( 'NONE',  ( 10.00000000000000000, 14.75893115100078568, -9.846743663894594434 ) ) ;
#57132 = CARTESIAN_POINT ( 'NONE',  ( 12.63842701281683922, 54.55059781766745175, -9.846743663894590881 ) ) ;
#57133 = AXIS2_PLACEMENT_3D ( 'NONE', #56712, #80697, #65679 ) ;
#57134 = FACE_OUTER_BOUND ( 'NONE', #4903, .T. ) ;
#57135 = ORIENTED_EDGE ( 'NONE', *, *, #41014, .T. ) ;
#57136 = CARTESIAN_POINT ( 'NONE',  ( -0.8801773607111008646, 3.272018677488171434, 2.915334737309923430 ) ) ;
#57137 = CARTESIAN_POINT ( 'NONE',  ( -2.266590686148945544, 11.38708216824730179, -7.082119434687050408 ) ) ;
#57138 = CARTESIAN_POINT ( 'NONE',  ( 10.00000000000000178, 12.25893115100078568, 9.846743663894594434 ) ) ;
#57139 = CARTESIAN_POINT ( 'NONE',  ( 12.91533473730993009, 46.60535201082150536, -10.88017736071109987 ) ) ;
#57141 = CARTESIAN_POINT ( 'NONE',  ( 11.12471383767606525, 12.50000000000035527, 1.674288514511126591 ) ) ;
#57140 = CARTESIAN_POINT ( 'NONE',  ( 10.00000000000000000, 27.87363466993042138, -12.81628187352647608 ) ) ;
#57142 = EDGE_CURVE ( 'NONE', #54254, #55655, #96373, .T. ) ;
#57143 = CARTESIAN_POINT ( 'NONE',  ( 13.21236992757673789, 15.00000000000000000, -5.338143956176714333 ) ) ;
#57144 = CARTESIAN_POINT ( 'NONE',  ( 19.84674366389459621, 53.50893115100078745, 7.409399052514197653E-17 ) ) ;
#57145 = CARTESIAN_POINT ( 'NONE',  ( 18.52753015748617571, 8.092264484334117824, 4.923371831947298993 ) ) ;
#57146 = CARTESIAN_POINT ( 'NONE',  ( -2.915334737309917656, -25.89464798917849109, 10.88017736071110164 ) ) ;
#57147 = CARTESIAN_POINT ( 'NONE',  ( 16.40814093676324603, 22.45696800326375353, -11.09922568453594671 ) ) ;
#57148 = CARTESIAN_POINT ( 'NONE',  ( 14.93928340878672323, 0.2306972965111900864, -0.2363597353049662619 ) ) ;
#57150 = CARTESIAN_POINT ( 'NONE',  ( 12.74305857943750730, 15.00000000000000178, -7.177950183686862218 ) ) ;
#57149 = CARTESIAN_POINT ( 'NONE',  ( 10.00000000000000178, 29.31368534415483751, 10.88017736071110342 ) ) ;
#57151 = CARTESIAN_POINT ( 'NONE',  ( -7.684764310694707667, 15.00000000000000000, -12.88194075009945472 ) ) ;
#57152 = CARTESIAN_POINT ( 'NONE',  ( 13.79529636645031943, 55.34541550158062506, -14.16423886937409904 ) ) ;
#57153 = CARTESIAN_POINT ( 'NONE',  ( 24.16423886937410614, 29.51208216824729647, -3.795296366450302550 ) ) ;
#57154 = CARTESIAN_POINT ( 'NONE',  ( 7.361572987183170547, 37.05059781766744464, 9.846743663894590881 ) ) ;
#57155 = CARTESIAN_POINT ( 'NONE',  ( 22.81628187352647785, 31.41530133659709279, 3.434112377981063169 ) ) ;
#57156 = CARTESIAN_POINT ( 'NONE',  ( 15.44008868035555260, 29.73035201082150891, 9.422509992056143702 ) ) ;
#57157 = CARTESIAN_POINT ( 'NONE',  ( 1.472469842513823179, 55.59226448433412315, -4.923371831947296329 ) ) ;
#57158 = CARTESIAN_POINT ( 'NONE',  ( 20.88017736071110519, 35.56368534415484106, 2.639326808657452039E-16 ) ) ;
#57159 = CARTESIAN_POINT ( 'NONE',  ( 22.81628187352647785, 6.623634669930420493, 6.195893100308588602E-16 ) ) ;
#57160 = CARTESIAN_POINT ( 'NONE',  ( 20.36894250292379738, 19.92874883491396787, -10.36894250292379027 ) ) ;
#57161 = CARTESIAN_POINT ( 'NONE',  ( -14.56195259121200714, 15.00000000000000888, -1.374002722866895176 ) ) ;
#57162 = CARTESIAN_POINT ( 'NONE',  ( 14.92337183194729633, 27.67559781766745530, 8.527530157486181039 ) ) ;
#57163 =( LENGTH_UNIT ( ) NAMED_UNIT ( * ) SI_UNIT ( .MILLI., .METRE. ) );
#57164 = CARTESIAN_POINT ( 'NONE',  ( -2.816281873526473856, 4.331968003263754419, 3.434112377981055619 ) ) ;
#57165 = ORIENTED_EDGE ( 'NONE', *, *, #53994, .F. ) ;
#57166 = DIRECTION ( 'NONE',  ( 0.000000000000000000, -1.000000000000000000, 0.000000000000000000 ) ) ;
#57167 = CARTESIAN_POINT ( 'NONE',  ( 4.474002695404426966, -3.767820133606233579, 2.750000000000000000 ) ) ;
#57168 = CARTESIAN_POINT ( 'NONE',  ( 0.5774900079438607392, 18.48035201082150536, 5.440088680355550821 ) ) ;
#57170 = CARTESIAN_POINT ( 'NONE',  ( 12.34086200392821908, -0.03417435944610275333, 7.125000000000058620 ) ) ;
#57169 = CARTESIAN_POINT ( 'NONE',  ( 10.00000000000000000, 5.553748834913967869, -14.16423886937410082 ) ) ;
#57171 = CARTESIAN_POINT ( 'NONE',  ( 2.791683348922240793, 6.633931151000785675, 7.208316651077764092 ) ) ;
#57172 = CARTESIAN_POINT ( 'NONE',  ( 0.1532563361054082862, 51.21726448433412315, 2.638427012816831674 ) ) ;
#57173 = CARTESIAN_POINT ( 'NONE',  ( 19.42250999205614548, 30.98035201082150536, -5.440088680355545492 ) ) ;
#57174 = CARTESIAN_POINT ( 'NONE',  ( 5.803070148808231465, 3.918713670743053586E-16, 13.28812917035392260 ) ) ;
#57175 = CARTESIAN_POINT ( 'NONE',  ( 0.1532563361054083140, 66.00893115100079456, 1.131784320476157264E-15 ) ) ;
#57176 = EDGE_CURVE ( 'NONE', #23173, #35624, #70904, .T. ) ;
#57177 = ORIENTED_EDGE ( 'NONE', *, *, #4488, .F. ) ;
#57178 = AXIS2_PLACEMENT_3D ( 'NONE', #18973, #26456, #79957 ) ;
#57179 = CARTESIAN_POINT ( 'NONE',  ( 8.157990163924704774, 14.76930270348882068, 12.51739793958118874 ) ) ;
#57180 = ORIENTED_EDGE ( 'NONE', *, *, #14389, .F. ) ;
#57181 = ORIENTED_EDGE ( 'NONE', *, *, #89345, .T. ) ;
#57182 = CARTESIAN_POINT ( 'NONE',  ( 8.235571585149870089, 11.04680217785154106, -8.235571585149873641 ) ) ;
#57183 = CARTESIAN_POINT ( 'NONE',  ( 6.204703633549690345, 12.84541550158063572, 14.16423886937410082 ) ) ;
#57184 = CARTESIAN_POINT ( 'NONE',  ( -4.164238869374099927, 7.012082168247302683, 3.795296366450308767 ) ) ;
#57185 = CARTESIAN_POINT ( 'NONE',  ( 24.16423886937410614, 59.51208216824728936, -3.795296366450302550 ) ) ;
#57186 = CARTESIAN_POINT ( 'NONE',  ( 1.472469842513823179, 51.42559781766745886, 4.923371831947296329 ) ) ;
#57187 = CARTESIAN_POINT ( 'NONE',  ( 18.52753015748617571, 38.09226448433412315, 4.923371831947298993 ) ) ;
#57188 = CARTESIAN_POINT ( 'NONE',  ( -0.2418659066527493184, 0.1163318810232758099, 6.114288769123083611 ) ) ;
#57190 = CARTESIAN_POINT ( 'NONE',  ( 1.472469842513823179, 65.59226448433412315, -4.923371831947296329 ) ) ;
#57189 = CARTESIAN_POINT ( 'NONE',  ( 0.5774900079438607392, 38.48035201082150536, 5.440088680355550821 ) ) ;
#57191 = CARTESIAN_POINT ( 'NONE',  ( 24.16423886937409904, 49.09541550158063217, 3.795296366450317205 ) ) ;
#57192 = CARTESIAN_POINT ( 'NONE',  ( 2.917880565312950480, 65.97041550158063217, -12.26659068614894821 ) ) ;
#57193 = DIRECTION ( 'NONE',  ( 0.000000000000000000, 0.000000000000000000, 1.000000000000000000 ) ) ;
#57194 = CARTESIAN_POINT ( 'NONE',  ( 2.035157376598824452, 58.68868534415482685, 7.964842623401179544 ) ) ;
#57195 = VECTOR ( 'NONE', #95587, 1000.000000000000000 ) ;
#57196 = CARTESIAN_POINT ( 'NONE',  ( -7.208316651077756099, -33.36606884899921255, 7.208316651077766757 ) ) ;
#57197 = ORIENTED_EDGE ( 'NONE', *, *, #94928, .T. ) ;
#57198 = DIRECTION ( 'NONE',  ( 0.000000000000000000, 1.000000000000000000, -0.000000000000000000 ) ) ;
#57199 = ORIENTED_EDGE ( 'NONE', *, *, #76248, .F. ) ;
#57200 = CARTESIAN_POINT ( 'NONE',  ( 5.076628168052703671, 26.84226448433411960, 8.527530157486179263 ) ) ;
#57201 = VERTEX_POINT ( 'NONE', #80860 ) ;
#57202 = CARTESIAN_POINT ( 'NONE',  ( 2.917880565312950480, 35.97041550158063217, -12.26659068614894821 ) ) ;
#57203 = CARTESIAN_POINT ( 'NONE',  ( 19.84674366389459621, 38.50893115100078745, 7.409399052514197653E-17 ) ) ;
#57204 = CARTESIAN_POINT ( 'NONE',  ( 0.5774900079438607392, 58.48035201082151247, 5.440088680355550821 ) ) ;
#57205 = TOROIDAL_SURFACE ( 'NONE', #14112, 14.49999999999999822, 0.5000000000000000000 ) ;
#57206 = DIRECTION ( 'NONE',  ( 0.000000000000000000, 0.000000000000000000, -1.000000000000000000 ) ) ;
#57207 = VECTOR ( 'NONE', #72448, 1000.000000000000000 ) ;
#57208 = CARTESIAN_POINT ( 'NONE',  ( 17.96484262340118221, 61.18868534415482685, -7.964842623401177768 ) ) ;
#57209 = CARTESIAN_POINT ( 'NONE',  ( 1.472469842513823179, 41.42559781766745886, 4.923371831947296329 ) ) ;
#57210 = CARTESIAN_POINT ( 'NONE',  ( 13.43411237798105340, 55.58196800326374643, 12.81628187352647963 ) ) ;
#57211 = CARTESIAN_POINT ( 'NONE',  ( -12.81628187352647252, 14.33196800326375175, 3.434112377981066722 ) ) ;
#57212 = ORIENTED_EDGE ( 'NONE', *, *, #20916, .F. ) ;
#57213 = CARTESIAN_POINT ( 'NONE',  ( 22.26659068614894466, 18.88708216824730002, 7.082119434687054849 ) ) ;
#57214 = VERTEX_POINT ( 'NONE', #53195 ) ;
#57215 = VERTEX_POINT ( 'NONE', #68695 ) ;
#57216 = CARTESIAN_POINT ( 'NONE',  ( 3.591859063236761518, 24.95696800326375353, 11.09922568453594849 ) ) ;
#57217 = SURFACE_STYLE_USAGE ( .BOTH. , #49233 ) ;
#57218 = CARTESIAN_POINT ( 'NONE',  ( 17.20831665107776587, 17.88393115100078745, 7.208316651077764980 ) ) ;
#57219 = CARTESIAN_POINT ( 'NONE',  ( 2.035157376598824452, 18.68868534415484106, 7.964842623401179544 ) ) ;
#57220 = CARTESIAN_POINT ( 'NONE',  ( 13.43411237798105340, 55.58196800326374643, 12.81628187352647963 ) ) ;
#57221 = CARTESIAN_POINT ( 'NONE',  ( -46.30928139467842186, 104.0823827281712397, -5.529860068218139801 ) ) ;
#57222 = CARTESIAN_POINT ( 'NONE',  ( 2.791683348922240793, 26.63393115100078745, 7.208316651077764092 ) ) ;
#57223 =( BOUNDED_CURVE ( )  B_SPLINE_CURVE ( 2, ( #77191, #741, #84706, #31194, #54192, #7234, #82725, #16210, #46694, #69701, #68240, #1231, #90220 ),
 .UNSPECIFIED., .F., .F. ) 
 B_SPLINE_CURVE_WITH_KNOTS ( ( 3, 2, 2, 2, 2, 2, 3 ),
 ( 0.5666666666666667629, 0.5722222222222222987, 0.5777777777777778345, 0.5833333333333334814, 0.5888888888888889062, 0.5944444444444444420, 0.5999999999999999778 ),
 .UNSPECIFIED. ) 
 CURVE ( )  GEOMETRIC_REPRESENTATION_ITEM ( )  RATIONAL_B_SPLINE_CURVE ( ( 0.9999999999999993339, 0.9659258262890688673, 1.000000000000000000, 0.9659258262890682012, 1.000000000000000000, 0.9659258262890682012, 1.000000000000000000, 0.9659258262890682012, 1.000000000000000000, 0.9659258262890682012, 1.000000000000000000, 0.9659258262890682012, 1.000000000000000000 ) ) 
 REPRESENTATION_ITEM ( '' )  );
#57224 = CARTESIAN_POINT ( 'NONE',  ( -14.88232117145538069, 14.49999999999999112, 1.875237731503072158 ) ) ;
#57225 = EDGE_CURVE ( 'NONE', #20106, #62619, #98734, .T. ) ;
#57226 = CARTESIAN_POINT ( 'NONE',  ( 2.035157376598824452, 68.68868534415484817, 7.964842623401179544 ) ) ;
#57227 = FACE_OUTER_BOUND ( 'NONE', #18610, .T. ) ;
#57228 = EDGE_CURVE ( 'NONE', #25245, #75142, #95868, .T. ) ;
#57229 = CARTESIAN_POINT ( 'NONE',  ( 7.551349515323100725, -0.03417435944610275333, 12.08468537022911349 ) ) ;
#57230 = CARTESIAN_POINT ( 'NONE',  ( -0.8801773607111009756, 68.06368534415484817, 1.068504757029289695E-15 ) ) ;
#57231 = EDGE_CURVE ( 'NONE', #78202, #65662, #58334, .T. ) ;
#57232 = CARTESIAN_POINT ( 'NONE',  ( 6.565887622018943937, 30.16530133659708568, 12.81628187352647430 ) ) ;
#57233 = DIRECTION ( 'NONE',  ( -0.000000000000000000, -1.000000000000000000, -0.000000000000000000 ) ) ;
#57234 = CARTESIAN_POINT ( 'NONE',  ( 18.52753015748618282, 38.92559781766745175, -4.923371831947291888 ) ) ;
#57235 = CARTESIAN_POINT ( 'NONE',  ( 19.42250999205614193, 35.14701867748816966, 5.440088680355555262 ) ) ;
#57236 = CARTESIAN_POINT ( 'NONE',  ( -4.164238869374099927, 27.01208216824730357, 3.795296366450308767 ) ) ;
#57237 = CARTESIAN_POINT ( 'NONE',  ( 14.92337183194729633, 27.67559781766745530, 8.527530157486181039 ) ) ;
#57238 = CARTESIAN_POINT ( 'NONE',  ( 19.38216949554541557, 27.24863466993041783, -9.382169495545420901 ) ) ;
#57240 = DIRECTION ( 'NONE',  ( -1.000000000000000000, 6.608470384673545847E-17, 0.000000000000000000 ) ) ;
#57239 = PLANE ( 'NONE',  #38897 ) ;
#57241 = CARTESIAN_POINT ( 'NONE',  ( 2.035157376598822676, 67.43868534415484817, -7.964842623401177768 ) ) ;
#57242 = CARTESIAN_POINT ( 'NONE',  ( -1.099225684535947600, 9.540301336597087456, 6.408140936763237150 ) ) ;
#57243 = EDGE_CURVE ( 'NONE', #50673, #81593, #9989, .T. ) ;
#57244 = CARTESIAN_POINT ( 'NONE',  ( 14.02068044289385718, 14.49999999999999112, -5.331089937175661930 ) ) ;
#57245 = CARTESIAN_POINT ( 'NONE',  ( 17.20831665107776587, 34.13393115100078745, -7.208316651077762316 ) ) ;
#57246 = CARTESIAN_POINT ( 'NONE',  ( 20.88017736071110875, 30.77201867748816966, -2.915334737309920765 ) ) ;
#57247 = CARTESIAN_POINT ( 'NONE',  ( -2.816281873526473856, 24.12363466993042138, 9.499525473075851096E-16 ) ) ;
#57248 = CARTESIAN_POINT ( 'NONE',  ( 17.20831665107776587, 34.13393115100078745, -7.208316651077762316 ) ) ;
#57249 = APPLICATION_PROTOCOL_DEFINITION ( 'draft international standard', 'automotive_design', 1998, #21905 ) ;
#57250 = CARTESIAN_POINT ( 'NONE',  ( -13.14228782657351680, 14.49999999999999112, 7.230509711182154575 ) ) ;
#57251 = CARTESIAN_POINT ( 'NONE',  ( 2.035157376598824452, 33.68868534415484106, 7.964842623401179544 ) ) ;
#57252 = CARTESIAN_POINT ( 'NONE',  ( 17.96484262340118221, 59.93868534415484106, 7.964842623401181321 ) ) ;
#57253 = CARTESIAN_POINT ( 'NONE',  ( 17.96484262340118221, 6.188685344154836621, -7.964842623401177768 ) ) ;
#57255 = CARTESIAN_POINT ( 'NONE',  ( 2.035157376598824452, 33.68868534415484106, 7.964842623401179544 ) ) ;
#57254 = CARTESIAN_POINT ( 'NONE',  ( 12.63842701281683034, 57.46726448433411605, 9.846743663894596210 ) ) ;
#57256 = DIRECTION ( 'NONE',  ( 0.000000000000000000, 0.000000000000000000, 1.000000000000000000 ) ) ;
#57257 = EDGE_CURVE ( 'NONE', #36584, #71988, #61183, .T. ) ;
#57258 = CARTESIAN_POINT ( 'NONE',  ( 7.084665262690076126, 44.10535201082151247, 10.88017736071109987 ) ) ;
#57259 = AXIS2_PLACEMENT_3D ( 'NONE', #36349, #66844, #97364 ) ;
#57261 = CARTESIAN_POINT ( 'NONE',  ( 20.00000000000000355, 87.39023020535090325, -4.970182472450021649 ) ) ;
#57260 = CARTESIAN_POINT ( 'NONE',  ( 4.559911319644449179, 7.230352010821505360, -9.422509992056141925 ) ) ;
#57262 = CARTESIAN_POINT ( 'NONE',  ( 0.1532563361054100626, 0.8005978176674514168, -2.638427012816831230 ) ) ;
#57263 = FILL_AREA_STYLE_COLOUR ( '', #50554 ) ;
#57264 = CARTESIAN_POINT ( 'NONE',  ( 17.20831665107776587, 52.88393115100078035, 7.208316651077764980 ) ) ;
#57265 = CARTESIAN_POINT ( 'NONE',  ( 24.16423886937410614, 49.51208216824730357, -3.795296366450302550 ) ) ;
#57267 = CARTESIAN_POINT ( 'NONE',  ( 19.72487221294571214, 24.78217586085238011, 6.499999999999993783 ) ) ;
#57266 = AXIS2_PLACEMENT_3D ( 'NONE', #30142, #98192, #91150 ) ;
#57268 = ADVANCED_FACE ( 'NONE', ( #50855 ), #35848, .T. ) ;
#57269 = AXIS2_PLACEMENT_3D ( 'NONE', #68206, #14217, #44697 ) ;
#57270 = CARTESIAN_POINT ( 'NONE',  ( -4.164238869374099927, 32.01208216824730357, 3.795296366450308767 ) ) ;
#57271 = CARTESIAN_POINT ( 'NONE',  ( 0.6178305044545818747, 3.498634669930420049, -9.382169495545419124 ) ) ;
#57272 = B_SPLINE_CURVE_WITH_KNOTS ( 'NONE', 3,
 ( #65039, #79581, #40603, #86101, #79077, #10590 ),
 .UNSPECIFIED., .F., .F.,
 ( 4, 2, 4 ),
 ( 3.409110551493610598E-05, 0.0004400426677367820722, 0.0008459942299586279638 ),
 .UNSPECIFIED. ) ;
#57273 = CARTESIAN_POINT ( 'NONE',  ( -7.072473369627247486, -84.40137233605018707, 2.750000000000000000 ) ) ;
#57274 = ORIENTED_EDGE ( 'NONE', *, *, #31556, .T. ) ;
#57275 = CARTESIAN_POINT ( 'NONE',  ( 7.084665262690076126, 2.022018677488171434, -10.88017736071110164 ) ) ;
#57276 = CARTESIAN_POINT ( 'NONE',  ( 0.1532563361054100626, 30.80059781766744820, -2.638427012816831230 ) ) ;
#57278 = CARTESIAN_POINT ( 'NONE',  ( -9.247107438774047949, 88.00886336720424197, -5.024692236534948009 ) ) ;
#57277 = CARTESIAN_POINT ( 'NONE',  ( -0.1503990784575279516, 53.10158574516643171, 6.262539305110076171 ) ) ;
#57279 = CARTESIAN_POINT ( 'NONE',  ( 20.88017736071110164, 65.35535201082150536, 2.915334737309930979 ) ) ;
#57280 = CARTESIAN_POINT ( 'NONE',  ( -8.502626202121188470, 0.04922511925147058515, -12.05617882333549851 ) ) ;
#57281 = CARTESIAN_POINT ( 'NONE',  ( 12.91533473730992121, 24.52201867748816966, 10.88017736071110164 ) ) ;
#57282 = CARTESIAN_POINT ( 'NONE',  ( 10.00000000000000000, 57.87363466993042493, -12.81628187352647608 ) ) ;
#57283 = CARTESIAN_POINT ( 'NONE',  ( 16.40814093676324603, 7.456968003263754419, -11.09922568453594671 ) ) ;
#57284 = CARTESIAN_POINT ( 'NONE',  ( 0.1532563361054100626, 30.80059781766744820, -2.638427012816831230 ) ) ;
#57285 = VERTEX_POINT ( 'NONE', #95875 ) ;
#57286 = SURFACE_SIDE_STYLE ('',( #79796 ) ) ;
#57287 = CARTESIAN_POINT ( 'NONE',  ( -10.97221242068696512, -3.876446283109303924E-15, -9.670525607392942646 ) ) ;
#57288 = CARTESIAN_POINT ( 'NONE',  ( -2.266590686148945544, 62.22041550158063927, 7.082119434687048631 ) ) ;
#57289 = CARTESIAN_POINT ( 'NONE',  ( 6.204703633549690345, 32.84541550158063927, 14.16423886937410082 ) ) ;
#57290 = CARTESIAN_POINT ( 'NONE',  ( 0.5774900079438590739, 32.64701867748816966, -5.440088680355550821 ) ) ;
#57291 = CARTESIAN_POINT ( 'NONE',  ( 4.559911319644449179, 53.89701867748817676, 9.422509992056141925 ) ) ;
#57292 = DIRECTION ( 'NONE',  ( -0.2503800040544323924, 0.000000000000000000, -0.9681476403781101858 ) ) ;
#57293 = CARTESIAN_POINT ( 'NONE',  ( 18.52753015748617571, 48.09226448433412315, 4.923371831947298993 ) ) ;
#57294 = CARTESIAN_POINT ( 'NONE',  ( 19.84674366389459266, 8.717264484334116048, -2.638427012816827677 ) ) ;
#57295 = FILL_AREA_STYLE_COLOUR ( '', #35409 ) ;
#57296 =( LENGTH_UNIT ( ) NAMED_UNIT ( * ) SI_UNIT ( .MILLI., .METRE. ) );
#57297 = LINE ( 'NONE', #20294, #502 ) ;
#57298 = CARTESIAN_POINT ( 'NONE',  ( 19.84674366389459266, 18.30059781766745175, 2.638427012816836559 ) ) ;
#57299 = CARTESIAN_POINT ( 'NONE',  ( 18.52753015748618282, 53.92559781766745175, -4.923371831947291888 ) ) ;
#57300 = COLOUR_RGB ( '', 0.72549020, 0.75294118, 0.79215686) ;
#57301 = UNCERTAINTY_MEASURE_WITH_UNIT (LENGTH_MEASURE( 1.000000000000000082E-05 ), #3153, 'distance_accuracy_value', 'NONE');
#57302 = CARTESIAN_POINT ( 'NONE',  ( 22.81628187352648496, 46.83196800326376064, -3.434112377981050290 ) ) ;
#57303 = CARTESIAN_POINT ( 'NONE',  ( -0.8801773607110991993, 67.85535201082151957, -2.915334737309923874 ) ) ;
#57304 = CARTESIAN_POINT ( 'NONE',  ( 10.00000000000000000, 34.75893115100078745, -9.846743663894594434 ) ) ;
#57306 = CARTESIAN_POINT ( 'NONE',  ( 2.791683348922240793, 26.63393115100078745, 7.208316651077764092 ) ) ;
#57305 = CARTESIAN_POINT ( 'NONE',  ( 20.36894250292379382, 53.67874883491397497, 10.36894250292379205 ) ) ;
#57307 = CARTESIAN_POINT ( 'NONE',  ( 0.000000000000000000, 14.49999999999999822, 0.000000000000000000 ) ) ;
#57308 = CARTESIAN_POINT ( 'NONE',  ( 17.20831665107776587, 62.88393115100078745, 7.208316651077764980 ) ) ;
#57309 = CARTESIAN_POINT ( 'NONE',  ( -0.3689425029237881626, 27.42874883491397142, 10.36894250292379027 ) ) ;
#57310 = CARTESIAN_POINT ( 'NONE',  ( 5.076628168052704559, 25.17559781766745175, -8.527530157486179263 ) ) ;
#57311 = CARTESIAN_POINT ( 'NONE',  ( 17.39651004071841456, 7.935752660568278216, 6.500000000000003553 ) ) ;
#57312 = CARTESIAN_POINT ( 'NONE',  ( 2.035157376598824452, 23.68868534415484461, 7.964842623401179544 ) ) ;
#57313 = CARTESIAN_POINT ( 'NONE',  ( 2.035157376598824452, 58.68868534415482685, 7.964842623401179544 ) ) ;
#57314 = CARTESIAN_POINT ( 'NONE',  ( 19.42250999205614548, 50.98035201082151247, -5.440088680355545492 ) ) ;
#57315 = ORIENTED_EDGE ( 'NONE', *, *, #13416, .T. ) ;
#57316 = CARTESIAN_POINT ( 'NONE',  ( 13.43411237798105340, 50.58196800326375353, 12.81628187352647963 ) ) ;
#57317 = CARTESIAN_POINT ( 'NONE',  ( 2.035157376598822676, 57.43868534415484106, -7.964842623401177768 ) ) ;
#57318 = VERTEX_POINT ( 'NONE', #66335 ) ;
#57319 = EDGE_CURVE ( 'NONE', #70448, #89913, #45757, .T. ) ;
#57320 = DIRECTION ( 'NONE',  ( -0.8870108331782246003, 0.000000000000000000, 0.4617486132350285266 ) ) ;
#57321 = CARTESIAN_POINT ( 'NONE',  ( 2.035157376598822676, 62.43868534415483396, -7.964842623401177768 ) ) ;
#57322 = ORIENTED_EDGE ( 'NONE', *, *, #81181, .F. ) ;
#57323 = CARTESIAN_POINT ( 'NONE',  ( -0.8801773607110991993, 57.85535201082149825, -2.915334737309923874 ) ) ;
#57324 = CARTESIAN_POINT ( 'NONE',  ( -0.8801773607111008646, 8.272018677488171434, 2.915334737309923430 ) ) ;
#57325 = CARTESIAN_POINT ( 'NONE',  ( 2.599899806584774264, 0.4361964623231012195, -6.495912400107028084 ) ) ;
#57326 = DIRECTION ( 'NONE',  ( 0.000000000000000000, -1.000000000000000000, 0.000000000000000000 ) ) ;
#57327 = CARTESIAN_POINT ( 'NONE',  ( 12.91533473730993009, 6.605352010821504471, -10.88017736071109987 ) ) ;
#57328 = CARTESIAN_POINT ( 'NONE',  ( 12.63842701281683922, 4.550597817667451750, -9.846743663894590881 ) ) ;
#57329 = CARTESIAN_POINT ( 'NONE',  ( 13.79529636645030344, 23.26208216824730002, 14.16423886937410614 ) ) ;
#57330 = CARTESIAN_POINT ( 'NONE',  ( 7.084665262690076126, 24.10535201082150181, 10.88017736071109987 ) ) ;
#57331 = CARTESIAN_POINT ( 'NONE',  ( 10.00000000000000178, 57.25893115100078745, 9.846743663894594434 ) ) ;
#57332 = ORIENTED_EDGE ( 'NONE', *, *, #21963, .F. ) ;
#57333 = CARTESIAN_POINT ( 'NONE',  ( 10.00000000000000178, 67.25893115100079456, 9.846743663894594434 ) ) ;
#57334 = VERTEX_POINT ( 'NONE', #57850 ) ;
#57335 = COLOUR_RGB ( '', 0.31764706, 0.68627451, 0.89019608) ;
#57336 = CARTESIAN_POINT ( 'NONE',  ( 17.39651004071890128, 29.08210964143323096, -6.499999999999448441 ) ) ;
#57337 = CARTESIAN_POINT ( 'NONE',  ( 2.035157376598824452, 58.68868534415482685, 7.964842623401179544 ) ) ;
#57338 = CARTESIAN_POINT ( 'NONE',  ( 12.63842701281683034, 52.46726448433413026, 9.846743663894596210 ) ) ;
#57339 = EDGE_CURVE ( 'NONE', #5309, #9323, #44293, .T. ) ;
#57340 = CARTESIAN_POINT ( 'NONE',  ( 16.40814093676323893, 40.79030133659708923, 11.09922568453595026 ) ) ;
#57342 = DIRECTION ( 'NONE',  ( 3.552713678800500929E-15, 0.000000000000000000, 1.000000000000000000 ) ) ;
#57341 = CARTESIAN_POINT ( 'NONE',  ( 2.035157376598824452, 13.68868534415483751, 7.964842623401179544 ) ) ;
#57343 = CARTESIAN_POINT ( 'NONE',  ( -0.8801773607110991993, 62.85535201082150536, -2.915334737309923874 ) ) ;
#57344 = CARTESIAN_POINT ( 'NONE',  ( -0.8801773607111009756, 3.063685344154838397, 1.068504757029289695E-15 ) ) ;
#57345 = PRESENTATION_LAYER_ASSIGNMENT (  '', '', ( #65331 ) ) ;
#57346 = AXIS2_PLACEMENT_3D ( 'NONE', #71152, #48137, #55142 ) ;
#57347 = ADVANCED_FACE ( 'NONE', ( #61661 ), #46194, .F. ) ;
#57348 = CARTESIAN_POINT ( 'NONE',  ( 6.565887622018943937, 43.08196800326374643, -12.81628187352647608 ) ) ;
#57349 = CARTESIAN_POINT ( 'NONE',  ( 17.96484262340118221, 36.18868534415484106, -7.964842623401177768 ) ) ;
#57350 = DIRECTION ( 'NONE',  ( 0.000000000000000000, 0.000000000000000000, 1.000000000000000000 ) ) ;
#57351 = ORIENTED_EDGE ( 'NONE', *, *, #97512, .T. ) ;
#57352 = CARTESIAN_POINT ( 'NONE',  ( 22.81628187352647785, 46.62363466993041783, 6.195893100308588602E-16 ) ) ;
#57353 = CARTESIAN_POINT ( 'NONE',  ( 20.88017736071110519, 35.56368534415484106, 2.639326808657452039E-16 ) ) ;
#57354 = EDGE_CURVE ( 'NONE', #47816, #651, #10161, .T. ) ;
#57355 = CARTESIAN_POINT ( 'NONE',  ( 1.472469842513823179, 56.42559781766745886, 4.923371831947296329 ) ) ;
#57356 = ORIENTED_EDGE ( 'NONE', *, *, #55843, .F. ) ;
#57357 = CARTESIAN_POINT ( 'NONE',  ( 0.1532563361054082862, 61.21726448433412315, 2.638427012816831674 ) ) ;
#57359 = CARTESIAN_POINT ( 'NONE',  ( 5.076628168052704559, 50.17559781766745886, -8.527530157486179263 ) ) ;
#57358 = DIRECTION ( 'NONE',  ( 0.000000000000000000, -1.000000000000000000, 0.000000000000000000 ) ) ;
#57360 = CARTESIAN_POINT ( 'NONE',  ( 15.44008868035555793, 16.39701867748817321, -9.422509992056140149 ) ) ;
#57361 = DIRECTION ( 'NONE',  ( 1.000000000000000000, -0.000000000000000000, -0.000000000000000000 ) ) ;
#57362 = CARTESIAN_POINT ( 'NONE',  ( 9.876730923139286134, 14.49999999999999112, 11.28938378619072935 ) ) ;
#57363 = VECTOR ( 'NONE', #96941, 1000.000000000000000 ) ;
#57365 = CARTESIAN_POINT ( 'NONE',  ( 7.361572987183169658, 14.96726448433411960, -9.846743663894592657 ) ) ;
#57364 = CARTESIAN_POINT ( 'NONE',  ( 2.791683348922237240, 45.38393115100079456, -7.208316651077763204 ) ) ;
#57366 = CARTESIAN_POINT ( 'NONE',  ( 19.72487221294571569, 34.78217586085237656, 6.499999999999993783 ) ) ;
#57368 = ORIENTED_EDGE ( 'NONE', *, *, #2016, .F. ) ;
#57367 = CARTESIAN_POINT ( 'NONE',  ( 0.1532563361054100626, 65.80059781766745175, -2.638427012816831230 ) ) ;
#57369 = CARTESIAN_POINT ( 'NONE',  ( 13.50249619331275674, 15.00000000000000888, -5.623250243473474796 ) ) ;
#57370 = CARTESIAN_POINT ( 'NONE',  ( 10.00000000000000000, 32.87363466993042493, -12.81628187352647608 ) ) ;
#57371 = CARTESIAN_POINT ( 'NONE',  ( 17.20831665107776587, 37.88393115100078745, 7.208316651077764980 ) ) ;
#57372 = CARTESIAN_POINT ( 'NONE',  ( 6.689969769698956625, -0.03417435944610275333, -12.58200319823970226 ) ) ;
#57373 = CARTESIAN_POINT ( 'NONE',  ( 10.00000000000000000, 65.55374883491396076, -14.16423886937410082 ) ) ;
#57374 = CARTESIAN_POINT ( 'NONE',  ( 1.472469842513823179, 25.59226448433412315, -4.923371831947296329 ) ) ;
#57375 = CARTESIAN_POINT ( 'NONE',  ( 0.000000000000000000, 0.5000000000000004441, 0.000000000000000000 ) ) ;
#57376 = CARTESIAN_POINT ( 'NONE',  ( 2.917880565312950480, 55.97041550158063217, -12.26659068614894821 ) ) ;
#57377 = CARTESIAN_POINT ( 'NONE',  ( -3.999999999999999112, 78.07179676972445748, 4.250000000000000000 ) ) ;
#57378 = EDGE_CURVE ( 'NONE', #84180, #1194, #2681, .T. ) ;
#57379 = CARTESIAN_POINT ( 'NONE',  ( 19.42250999205614548, 5.980352010821504471, -5.440088680355545492 ) ) ;
#57380 = CARTESIAN_POINT ( 'NONE',  ( 6.204703633549690345, 32.84541550158063927, 14.16423886937410082 ) ) ;
#57382 = DIRECTION ( 'NONE',  ( 0.000000000000000000, -1.000000000000000000, 0.000000000000000000 ) ) ;
#57381 = CARTESIAN_POINT ( 'NONE',  ( 13.79529636645030344, 43.26208216824730357, 14.16423886937410614 ) ) ;
#57383 = DIRECTION ( 'NONE',  ( -1.000000000000000000, -0.000000000000000000, -0.000000000000000000 ) ) ;
#57384 = COLOUR_RGB ( '', 0.66274510, 0.83137255, 0.94901961) ;
#57385 = B_SPLINE_CURVE_WITH_KNOTS ( 'NONE', 3,
 ( #12973, #28955, #50975, #67467, #97987, #35477 ),
 .UNSPECIFIED., .F., .F.,
 ( 4, 2, 4 ),
 ( 0.0002800187770242821444, 0.0006862241901199757875, 0.001092429603215669268 ),
 .UNSPECIFIED. ) ;
#57386 = CARTESIAN_POINT ( 'NONE',  ( 18.52753015748617571, 13.09226448433411960, 4.923371831947298993 ) ) ;
#57388 = CARTESIAN_POINT ( 'NONE',  ( 0.1532563361054100626, 55.80059781766745175, -2.638427012816831230 ) ) ;
#57387 = CARTESIAN_POINT ( 'NONE',  ( -8.209432707284690878, 0.5000000000000004441, -12.55409154915497183 ) ) ;
#57389 = CARTESIAN_POINT ( 'NONE',  ( 4.559911319644449179, 48.89701867748817676, 9.422509992056141925 ) ) ;
#57390 = CARTESIAN_POINT ( 'NONE',  ( 0.000000000000000000, 15.00000000000000000, 0.000000000000000000 ) ) ;
#57391 = AXIS2_PLACEMENT_3D ( 'NONE', #74876, #52371, #6375 ) ;
#57392 = CARTESIAN_POINT ( 'NONE',  ( 19.84674366389459266, 48.30059781766745175, 2.638427012816836559 ) ) ;
#57393 = CARTESIAN_POINT ( 'NONE',  ( -3.469446951953614189E-15, 82.00000000000000000, -5.000000000000000000 ) ) ;
#57394 = CARTESIAN_POINT ( 'NONE',  ( 12.63842701281683922, 49.55059781766744464, -9.846743663894590881 ) ) ;
#57395 = CARTESIAN_POINT ( 'NONE',  ( -0.1034006766821534140, 4.816303916663454299E-16, 14.49963131600461175 ) ) ;
#57396 = ORIENTED_EDGE ( 'NONE', *, *, #18651, .F. ) ;
#57397 = CARTESIAN_POINT ( 'NONE',  ( 2.917880565312948704, 22.63708216824730002, 12.26659068614894643 ) ) ;
#57398 = FACE_OUTER_BOUND ( 'NONE', #83691, .T. ) ;
#57400 = CARTESIAN_POINT ( 'NONE',  ( -6.382347221874250742, 14.63595249122788999, -13.57444820018236875 ) ) ;
#57399 = CARTESIAN_POINT ( 'NONE',  ( -5.079065453171176969, -28.67168118942974075, -2.500000000000000888 ) ) ;
#57401 = CARTESIAN_POINT ( 'NONE',  ( 10.00000000000000000, 21.81368534415484106, -10.88017736071110342 ) ) ;
#57402 = CARTESIAN_POINT ( 'NONE',  ( 0.6178305044545838731, 29.74863466993042138, 9.382169495545420901 ) ) ;
#57403 = CARTESIAN_POINT ( 'NONE',  ( 21.92686044187657046, 62.39664270246084499, -3.195792623639524432 ) ) ;
#57404 = CARTESIAN_POINT ( 'NONE',  ( 14.92337183194729633, 7.675597817667451750, 8.527530157486181039 ) ) ;
#57405 = CARTESIAN_POINT ( 'NONE',  ( 10.00000000000000000, 52.87363466993041783, -12.81628187352647608 ) ) ;
#57406 = ORIENTED_EDGE ( 'NONE', *, *, #59050, .F. ) ;
#57407 = CARTESIAN_POINT ( 'NONE',  ( 5.680373671027947324, -28.65980262291034819, -3.749999999996780353 ) ) ;
#57408 = CARTESIAN_POINT ( 'NONE',  ( 13.79529636645030344, 23.26208216824730002, 14.16423886937410614 ) ) ;
#57409 = CARTESIAN_POINT ( 'NONE',  ( 70.08911253270099451, 0.3894472361808953842, 10.00000000000000000 ) ) ;
#57410 = DIRECTION ( 'NONE',  ( 0.000000000000000000, 0.000000000000000000, -1.000000000000000000 ) ) ;
#57411 = CARTESIAN_POINT ( 'NONE',  ( 4.559911319644449179, 8.897018677488173211, 9.422509992056141925 ) ) ;
#57412 = FACE_OUTER_BOUND ( 'NONE', #96914, .T. ) ;
#57413 = DIRECTION ( 'NONE',  ( 0.000000000000000000, 1.000000000000000000, 0.000000000000000000 ) ) ;
#57414 = CARTESIAN_POINT ( 'NONE',  ( 20.88017736071110164, 45.35535201082149115, 2.915334737309930979 ) ) ;
#57415 = CARTESIAN_POINT ( 'NONE',  ( 12.91533473730992121, 44.52201867748816966, 10.88017736071110164 ) ) ;
#57416 = CARTESIAN_POINT ( 'NONE',  ( 0.6178305044545818747, 8.498634669930421381, -9.382169495545419124 ) ) ;
#57417 = CARTESIAN_POINT ( 'NONE',  ( 19.84674366389459266, 63.30059781766745886, 2.638427012816836559 ) ) ;
#57418 = CARTESIAN_POINT ( 'NONE',  ( -46.30928139467842897, 104.0823827281712255, -5.529860068218140690 ) ) ;
#57419 = CARTESIAN_POINT ( 'NONE',  ( 2.791683348922240793, 16.63393115100078745, 7.208316651077764092 ) ) ;
#57420 = CARTESIAN_POINT ( 'NONE',  ( 2.603489959281199972, 21.58210964143324873, 6.499999999999559464 ) ) ;
#57421 = CARTESIAN_POINT ( 'NONE',  ( -0.8801773607111009756, 43.06368534415484106, 1.068504757029289695E-15 ) ) ;
#57422 = UNCERTAINTY_MEASURE_WITH_UNIT (LENGTH_MEASURE( 1.000000000000000082E-05 ), #29839, 'distance_accuracy_value', 'NONE');
#57423 = CARTESIAN_POINT ( 'NONE',  ( 16.40814093676323893, 5.790301336597087456, 11.09922568453595026 ) ) ;
#57424 = B_SPLINE_CURVE_WITH_KNOTS ( 'NONE', 3,
 ( #94664, #26173, #95144, #87153, #3680, #64634 ),
 .UNSPECIFIED., .F., .F.,
 ( 4, 2, 4 ),
 ( 3.409110551496107651E-05, 0.0004400426677367867885, 0.0008459942299586125682 ),
 .UNSPECIFIED. ) ;
#57425 = CARTESIAN_POINT ( 'NONE',  ( 20.88017736071110164, 65.35535201082150536, 2.915334737309930979 ) ) ;
#57426 = CARTESIAN_POINT ( 'NONE',  ( 1.472469842513823179, 31.42559781766745530, 4.923371831947296329 ) ) ;
#57427 = CARTESIAN_POINT ( 'NONE',  ( 3.591859063236761518, 44.95696800326376064, 11.09922568453594849 ) ) ;
#57429 = LINE ( 'NONE', #70479, #71921 ) ;
#57428 = CARTESIAN_POINT ( 'NONE',  ( 17.20831665107776587, 2.883931151000785231, 7.208316651077764980 ) ) ;
#57430 = VERTEX_POINT ( 'NONE', #70668 ) ;
#57431 = CARTESIAN_POINT ( 'NONE',  ( 1.274849032794280523, 48.57228050351032067, 6.499999999999960032 ) ) ;
#57432 = FACE_OUTER_BOUND ( 'NONE', #66604, .T. ) ;
#57433 = CARTESIAN_POINT ( 'NONE',  ( 10.00000000000000000, 16.81368534415483751, -10.88017736071110342 ) ) ;
#57435 = CARTESIAN_POINT ( 'NONE',  ( 22.26659068614894466, 23.88708216824730357, 7.082119434687054849 ) ) ;
#57434 = CARTESIAN_POINT ( 'NONE',  ( 22.81628187352648496, 56.83196800326374643, -3.434112377981050290 ) ) ;
#57436 = CARTESIAN_POINT ( 'NONE',  ( 10.00000000000000178, 27.25893115100078390, 9.846743663894594434 ) ) ;
#57437 = VECTOR ( 'NONE', #51396, 1000.000000000000000 ) ;
#57438 = CARTESIAN_POINT ( 'NONE',  ( 20.88017736071110875, 15.77201867748817143, -2.915334737309920765 ) ) ;
#57439 = CARTESIAN_POINT ( 'NONE',  ( 0.5774900079438590739, 2.647018677488171434, -5.440088680355550821 ) ) ;
#57440 = ORIENTED_EDGE ( 'NONE', *, *, #5923, .T. ) ;
#57441 = VECTOR ( 'NONE', #40886, 1000.000000000000114 ) ;
#57442 = CARTESIAN_POINT ( 'NONE',  ( -0.8801773607110991993, 12.85535201082150358, -2.915334737309923874 ) ) ;
#57443 = EDGE_CURVE ( 'NONE', #16387, #29547, #23706, .T. ) ;
#57444 = CARTESIAN_POINT ( 'NONE',  ( 15.44008868035555260, 19.73035201082150536, 9.422509992056143702 ) ) ;
#57446 = CARTESIAN_POINT ( 'NONE',  ( 2.035157376598822676, 27.43868534415483396, -7.964842623401177768 ) ) ;
#57445 = CYLINDRICAL_SURFACE ( 'NONE', #90371, 11.92686044187656513 ) ;
#57447 = ORIENTED_EDGE ( 'NONE', *, *, #64451, .F. ) ;
#57448 = CARTESIAN_POINT ( 'NONE',  ( 20.15039907845753220, 26.74884699246889141, 6.262539305110078836 ) ) ;
#57449 = CARTESIAN_POINT ( 'NONE',  ( -0.8801773607111008646, 23.27201867748817676, 2.915334737309923430 ) ) ;
#57450 = CARTESIAN_POINT ( 'NONE',  ( 7.361572987183170547, 62.05059781766745886, 9.846743663894590881 ) ) ;
#57451 = CARTESIAN_POINT ( 'NONE',  ( -0.1503990784575328643, 70.00000000000000000, -6.262539305110068177 ) ) ;
#57452 = SURFACE_SIDE_STYLE ('',( #95460 ) ) ;
#57453 = CARTESIAN_POINT ( 'NONE',  ( 10.00000000000000000, 30.55374883491397142, -14.16423886937410082 ) ) ;
#57454 = CARTESIAN_POINT ( 'NONE',  ( -0.8801773607111009756, 38.06368534415484106, 1.068504757029289695E-15 ) ) ;
#57455 = CARTESIAN_POINT ( 'NONE',  ( 15.44008868035555793, 21.39701867748817321, -9.422509992056140149 ) ) ;
#57456 = CARTESIAN_POINT ( 'NONE',  ( 20.10239578412224404, 42.63377557478297319, -6.340343622311914729 ) ) ;
#57457 = CARTESIAN_POINT ( 'NONE',  ( 20.15039907845753575, 62.62777174578612716, -6.262539305110073506 ) ) ;
#57458 = CARTESIAN_POINT ( 'NONE',  ( 18.52753015748617571, 43.09226448433412315, 4.923371831947298993 ) ) ;
#57459 = CARTESIAN_POINT ( 'NONE',  ( -0.1049300847420624877, 22.21697413083879624, -6.336235997365760042 ) ) ;
#57460 = CARTESIAN_POINT ( 'NONE',  ( 19.84674366389459266, 13.71726448433411782, -2.638427012816827677 ) ) ;
#57461 = CARTESIAN_POINT ( 'NONE',  ( -3.434112377981067610, -31.91803199673623936, -12.81628187352647252 ) ) ;
#57462 = CARTESIAN_POINT ( 'NONE',  ( -0.8801773607110991993, 12.85535201082150358, -2.915334737309923874 ) ) ;
#57463 = CARTESIAN_POINT ( 'NONE',  ( 1.472469842513823179, 15.59226448433411960, -4.923371831947296329 ) ) ;
#57464 = CARTESIAN_POINT ( 'NONE',  ( 2.791683348922237240, 65.38393115100078035, -7.208316651077763204 ) ) ;
#57465 = CARTESIAN_POINT ( 'NONE',  ( 4.559911319644449179, 62.23035201082150536, -9.422509992056141925 ) ) ;
#57467 = CARTESIAN_POINT ( 'NONE',  ( 13.43411237798106583, 57.66530133659708923, -12.81628187352647252 ) ) ;
#57466 = CARTESIAN_POINT ( 'NONE',  ( -0.8801773607110991993, 17.85535201082150536, -2.915334737309923874 ) ) ;
#57468 = CARTESIAN_POINT ( 'NONE',  ( -4.164238869374099039, 31.80374883491396432, 8.674139862899312516E-16 ) ) ;
#57469 = DIRECTION ( 'NONE',  ( 0.000000000000000000, 0.000000000000000000, 1.000000000000000000 ) ) ;
#57470 = EDGE_CURVE ( 'NONE', #75287, #32106, #32650, .T. ) ;
#57471 = CARTESIAN_POINT ( 'NONE',  ( 3.591859063236761518, 59.95696800326375353, 11.09922568453594849 ) ) ;
#57472 = VERTEX_POINT ( 'NONE', #39188 ) ;
#57473 = CARTESIAN_POINT ( 'NONE',  ( 0.1532563361054082862, 66.21726448433413736, 2.638427012816831674 ) ) ;
#57474 = CARTESIAN_POINT ( 'NONE',  ( -0.2418659066527510948, 15.11633188102327452, 6.114288769123080058 ) ) ;
#57475 = EDGE_CURVE ( 'NONE', #26330, #55756, #88975, .T. ) ;
#57476 = CARTESIAN_POINT ( 'NONE',  ( 2.035157376598822676, 37.43868534415484106, -7.964842623401177768 ) ) ;
#57477 = CARTESIAN_POINT ( 'NONE',  ( 0.1532563361054083140, 66.00893115100079456, 1.131784320476157264E-15 ) ) ;
#57478 = ORIENTED_EDGE ( 'NONE', *, *, #7373, .F. ) ;
#57479 = CARTESIAN_POINT ( 'NONE',  ( 10.00000000000000000, 14.75893115100078568, -9.846743663894594434 ) ) ;
#57480 = CARTESIAN_POINT ( 'NONE',  ( 11.92686044187656336, 7.188309369127517279, -2.602085213965210642E-15 ) ) ;
#57481 = CARTESIAN_POINT ( 'NONE',  ( 10.00000000000000178, 7.258931151000785675, 9.846743663894594434 ) ) ;
#57482 = CARTESIAN_POINT ( 'NONE',  ( 7.361572987183170547, 22.05059781766745530, 9.846743663894590881 ) ) ;
#57483 = CARTESIAN_POINT ( 'NONE',  ( 2.791683348922240793, 11.63393115100078568, 7.208316651077764092 ) ) ;
#57484 = CARTESIAN_POINT ( 'NONE',  ( 5.076628168052704559, 5.175597817667451750, -8.527530157486179263 ) ) ;
#57486 = DIRECTION ( 'NONE',  ( 0.000000000000000000, 0.000000000000000000, 1.000000000000000000 ) ) ;
#57485 = CARTESIAN_POINT ( 'NONE',  ( 20.88017736071110164, 55.35535201082149825, 2.915334737309930979 ) ) ;
#57487 = CARTESIAN_POINT ( 'NONE',  ( 2.791683348922237240, 0.3839311510007847872, -7.208316651077763204 ) ) ;
#57489 = ORIENTED_EDGE ( 'NONE', *, *, #3565, .T. ) ;
#57488 = CARTESIAN_POINT ( 'NONE',  ( 12.63842701281683034, 17.46726448433411250, 9.846743663894596210 ) ) ;
#57490 = LINE ( 'NONE', #11995, #21454 ) ;
#57491 = CARTESIAN_POINT ( 'NONE',  ( 6.565887622018943937, 0.1653013365970866511, 12.81628187352647430 ) ) ;
#57492 = ORIENTED_EDGE ( 'NONE', *, *, #5168, .T. ) ;
#57493 = DIRECTION ( 'NONE',  ( 0.000000000000000000, 0.000000000000000000, 1.000000000000000000 ) ) ;
#57494 = CARTESIAN_POINT ( 'NONE',  ( 20.36894250292379738, 14.92874883491396432, -10.36894250292379027 ) ) ;
#57495 = UNCERTAINTY_MEASURE_WITH_UNIT (LENGTH_MEASURE( 1.000000000000000082E-05 ), #94795, 'distance_accuracy_value', 'NONE');
#57496 = CARTESIAN_POINT ( 'NONE',  ( 2.189108318723648861, -3.258959264560919371E-15, 14.46085460646900245 ) ) ;
#57497 = CARTESIAN_POINT ( 'NONE',  ( 10.00000000000000178, 18.05374883491396787, 14.16423886937410082 ) ) ;
#57498 = CARTESIAN_POINT ( 'NONE',  ( -4.164238869374099039, 31.80374883491396432, 8.674139862899312516E-16 ) ) ;
#57499 = LINE ( 'NONE', #73978, #7108 ) ;
#57500 = CARTESIAN_POINT ( 'NONE',  ( 24.16423886937410614, 4.303748834913967869, 8.672049930838204340E-16 ) ) ;
#57501 = CARTESIAN_POINT ( 'NONE',  ( 15.44008868035555260, 29.73035201082150891, 9.422509992056143702 ) ) ;
#57502 = DIRECTION ( 'NONE',  ( -0.8320502943378436100, 0.5547001962252291474, -0.000000000000000000 ) ) ;
#57503 = CARTESIAN_POINT ( 'NONE',  ( 2.791683348922237240, 10.38393115100078390, -7.208316651077763204 ) ) ;
#57506 = TOROIDAL_SURFACE ( 'NONE', #97507, 1.499999999999996669, 0.5000000000000000000 ) ;
#57505 = CARTESIAN_POINT ( 'NONE',  ( 5.076628168052703671, 16.84226448433411960, 8.527530157486179263 ) ) ;
#57504 = CARTESIAN_POINT ( 'NONE',  ( -0.8801773607111008646, 53.27201867748816966, 2.915334737309923430 ) ) ;
#57507 = CARTESIAN_POINT ( 'NONE',  ( 2.035157376598822676, 17.43868534415483751, -7.964842623401177768 ) ) ;
#57508 = CARTESIAN_POINT ( 'NONE',  ( 21.09922568453594849, 51.20696800326375353, 6.408140936763242479 ) ) ;
#57509 = CARTESIAN_POINT ( 'NONE',  ( 0.1532563361054082862, 46.21726448433411605, 2.638427012816831674 ) ) ;
#57510 = CARTESIAN_POINT ( 'NONE',  ( 19.84674366389459266, 58.30059781766745886, 2.638427012816836559 ) ) ;
#57511 = CARTESIAN_POINT ( 'NONE',  ( 0.6178305044545818747, 28.49863466993041783, -9.382169495545419124 ) ) ;
#57512 = SHAPE_REPRESENTATION ( '1.4 Rivet', ( #27931 ), #93381 ) ;
#57513 = CARTESIAN_POINT ( 'NONE',  ( 14.16423886937410082, -35.48791783175269643, -3.795296366450314096 ) ) ;
#57514 = CARTESIAN_POINT ( 'NONE',  ( 1.472469842513823179, 36.42559781766745175, 4.923371831947296329 ) ) ;
#57515 = CARTESIAN_POINT ( 'NONE',  ( 24.16423886937410614, 9.303748834913967869, 8.672049930838204340E-16 ) ) ;
#57516 = VERTEX_POINT ( 'NONE', #32146 ) ;
#57517 = ORIENTED_EDGE ( 'NONE', *, *, #31500, .F. ) ;
#57518 = CARTESIAN_POINT ( 'NONE',  ( -9.000000000000001776, 80.99999999999994316, -1.249999999999987121 ) ) ;
#57519 = CARTESIAN_POINT ( 'NONE',  ( 7.084665262690076126, 52.02201867748816255, -10.88017736071110164 ) ) ;
#57520 = CARTESIAN_POINT ( 'NONE',  ( 20.88017736071110875, 55.77201867748816966, -2.915334737309920765 ) ) ;
#57521 = CARTESIAN_POINT ( 'NONE',  ( -0.3689425029237881626, 42.42874883491396787, 10.36894250292379027 ) ) ;
#57522 = CARTESIAN_POINT ( 'NONE',  ( 1.472469842513823179, 56.42559781766745886, 4.923371831947296329 ) ) ;
#57523 = CARTESIAN_POINT ( 'NONE',  ( 21.09922568453594849, 61.20696800326376064, 6.408140936763242479 ) ) ;
#57524 = CARTESIAN_POINT ( 'NONE',  ( 4.559911319644449179, 47.23035201082150536, -9.422509992056141925 ) ) ;
#57525 = CARTESIAN_POINT ( 'NONE',  ( -3.377746357650261988, -3.629174488344641070, -2.499999999999998668 ) ) ;
#57526 = CARTESIAN_POINT ( 'NONE',  ( 0.6178305044545818747, 23.49863466993041783, -9.382169495545419124 ) ) ;
#57527 = CARTESIAN_POINT ( 'NONE',  ( 12.63842701281683922, 49.55059781766744464, -9.846743663894590881 ) ) ;
#57528 = CARTESIAN_POINT ( 'NONE',  ( 3.469446951953614189E-15, 19.31368534415484106, 10.88017736071110342 ) ) ;
#57529 = CARTESIAN_POINT ( 'NONE',  ( 12.91533473730992121, 4.522018677488169658, 10.88017736071110164 ) ) ;
#57530 = CARTESIAN_POINT ( 'NONE',  ( -12.00809552683950088, 0.3639308727178954261, -8.989195838243722037 ) ) ;
#57531 = CARTESIAN_POINT ( 'NONE',  ( 4.559911319644449179, 7.230352010821504471, -9.422509992056141925 ) ) ;
#57532 = DIRECTION ( 'NONE',  ( 1.953992523340275511E-14, 0.000000000000000000, 1.000000000000000000 ) ) ;
#57533 = CARTESIAN_POINT ( 'NONE',  ( 18.52753015748618282, 3.925597817667451306, -4.923371831947291888 ) ) ;
#57534 = CARTESIAN_POINT ( 'NONE',  ( 15.44008868035555793, 66.39701867748817676, -9.422509992056140149 ) ) ;
#57535 = CARTESIAN_POINT ( 'NONE',  ( 17.99999999999999645, 78.68095262111053501, -3.967704011867417613 ) ) ;
#57536 = CARTESIAN_POINT ( 'NONE',  ( 17.20831665107776587, 39.13393115100079456, -7.208316651077762316 ) ) ;
#57537 = CARTESIAN_POINT ( 'NONE',  ( 15.44008868035555793, 16.39701867748817321, -9.422509992056140149 ) ) ;
#57538 = CARTESIAN_POINT ( 'NONE',  ( 2.791683348922237240, 65.38393115100078035, -7.208316651077763204 ) ) ;
#57540 = CARTESIAN_POINT ( 'NONE',  ( 8.979999999999991545, 21.00000000000000000, 3.000000000000000000 ) ) ;
#57539 = CARTESIAN_POINT ( 'NONE',  ( 0.5774900079438590739, 37.64701867748817676, -5.440088680355550821 ) ) ;
#57541 = CARTESIAN_POINT ( 'NONE',  ( 21.09922568453594849, 41.20696800326375353, 6.408140936763242479 ) ) ;
#57542 = VERTEX_POINT ( 'NONE', #92180 ) ;
#57543 = CARTESIAN_POINT ( 'NONE',  ( 10.00000000000000000, 46.81368534415484106, -10.88017736071110342 ) ) ;
#57545 = FACE_OUTER_BOUND ( 'NONE', #81647, .T. ) ;
#57544 = CARTESIAN_POINT ( 'NONE',  ( -2.816281873526473856, 14.33196800326375531, 3.434112377981055619 ) ) ;
#57546 = CARTESIAN_POINT ( 'NONE',  ( 19.84674366389459621, 3.508931151000785231, 7.409399052514197653E-17 ) ) ;
#57547 = CARTESIAN_POINT ( 'NONE',  ( 4.559911319644449179, 27.23035201082150536, -9.422509992056141925 ) ) ;
#57548 = CARTESIAN_POINT ( 'NONE',  ( -2.266590686148945544, 66.38708216824730357, -7.082119434687050408 ) ) ;
#57549 = CARTESIAN_POINT ( 'NONE',  ( 12.63842701281683922, 54.55059781766745175, -9.846743663894590881 ) ) ;
#57550 = CARTESIAN_POINT ( 'NONE',  ( 18.52753015748617571, 3.092264484334118269, 4.923371831947298993 ) ) ;
#57551 = CARTESIAN_POINT ( 'NONE',  ( 15.44008868035555260, 64.73035201082151957, 9.422509992056143702 ) ) ;
#57552 = DIRECTION ( 'NONE',  ( -1.257568779154408793E-17, -1.000000000000000000, 0.000000000000000000 ) ) ;
#57553 = CARTESIAN_POINT ( 'NONE',  ( 2.917880565312950480, 35.97041550158063217, -12.26659068614894821 ) ) ;
#57554 = ADVANCED_FACE ( 'NONE', ( #71156 ), #62648, .T. ) ;
#57555 = DIRECTION ( 'NONE',  ( -4.174438572590588592E-14, 0.000000000000000000, 1.000000000000000000 ) ) ;
#57556 = CARTESIAN_POINT ( 'NONE',  ( 13.75503023589411633, 0.04922511925147142475, -5.333408231410735389 ) ) ;
#57557 = CIRCLE ( 'NONE', #78261, 14.49999999999999822 ) ;
#57558 = EDGE_LOOP ( 'NONE', ( #70541, #56836, #81752, #55442 ) ) ;
#57559 = CARTESIAN_POINT ( 'NONE',  ( 20.36894250292379738, 44.92874883491396787, -10.36894250292379027 ) ) ;
#57560 = CARTESIAN_POINT ( 'NONE',  ( 13.79529636645031943, 55.34541550158062506, -14.16423886937409904 ) ) ;
#57561 = CARTESIAN_POINT ( 'NONE',  ( 10.00000000000000000, 19.75893115100078390, -9.846743663894594434 ) ) ;
#57562 = B_SPLINE_CURVE_WITH_KNOTS ( 'NONE', 3,
 ( #12628, #73620, #95136, #12139, #18671, #5142 ),
 .UNSPECIFIED., .F., .F.,
 ( 4, 2, 4 ),
 ( 3.409110551496119849E-05, 0.0004400426677367863006, 0.0008459942299586114840 ),
 .UNSPECIFIED. ) ;
#57563 = CARTESIAN_POINT ( 'NONE',  ( -13.11254139118232231, 91.00000000000000000, 8.000000000000000000 ) ) ;
#57564 = CARTESIAN_POINT ( 'NONE',  ( -1.926860441876564023, 42.87045670184114243, 3.195792623639529761 ) ) ;
#57565 = CARTESIAN_POINT ( 'NONE',  ( 0.5774900079438590739, 67.64701867748817676, -5.440088680355550821 ) ) ;
#57566 = CARTESIAN_POINT ( 'NONE',  ( 24.16423886937410614, 49.51208216824730357, -3.795296366450302550 ) ) ;
#57567 =( BOUNDED_CURVE ( )  B_SPLINE_CURVE ( 2, ( #2936, #65362, #50364, #58346, #56885, #49382, #20374, #50868, #87388 ),
 .UNSPECIFIED., .F., .F. ) 
 B_SPLINE_CURVE_WITH_KNOTS ( ( 3, 2, 2, 2, 3 ),
 ( 0.3687123655116599230, 0.3690476190476190688, 0.3750000000000000000, 0.3809523809523809312, 0.3812876344883400770 ),
 .UNSPECIFIED. ) 
 CURVE ( )  GEOMETRIC_REPRESENTATION_ITEM ( )  RATIONAL_B_SPLINE_CURVE ( ( 0.9963778908391760503, 0.9980808541467920403, 1.000000000000000000, 0.9659258262890683122, 1.000000000000000000, 0.9659258262890683122, 1.000000000000000000, 0.9980808541467920403, 0.9963778908391760503 ) ) 
 REPRESENTATION_ITEM ( '' )  );
#57568 = CARTESIAN_POINT ( 'NONE',  ( 2.791683348922237240, 10.38393115100078390, -7.208316651077763204 ) ) ;
#57569 = VECTOR ( 'NONE', #21400, 1000.000000000000000 ) ;
#57570 = VECTOR ( 'NONE', #14532, 1000.000000000000000 ) ;
#57571 = CARTESIAN_POINT ( 'NONE',  ( -4.923371831947292776, -3.157735515665872850, 8.527530157486181039 ) ) ;
#57572 = ORIENTED_EDGE ( 'NONE', *, *, #62588, .T. ) ;
#57573 = LINE ( 'NONE', #41620, #57195 ) ;
#57574 = ORIENTED_EDGE ( 'NONE', *, *, #19398, .T. ) ;
#57575 = B_SPLINE_CURVE_WITH_KNOTS ( 'NONE', 3,
 ( #34516, #95537, #88519, #65009, #20523, #28512, #42057, #27025, #57033, #43021, #19534, #19047, #81018, #96535, #80533, #12031, #59006, #57525, #12519, #51008, #5528, #3567 ),
 .UNSPECIFIED., .F., .F.,
 ( 4, 2, 2, 2, 2, 2, 2, 2, 2, 2, 4 ),
 ( 0.000000000000000000, 0.005576344000565805654, 0.01115268800113161131, 0.02230537600226322262, 0.04461075200452644524, 0.05576344000565804093, 0.06691612800678964357, 0.07806881600792124620, 0.08364516000848705446, 0.08643333200876995859, 0.08922150400905284884 ),
 .UNSPECIFIED. ) ;
#57576 = AXIS2_PLACEMENT_3D ( 'NONE', #54140, #39159, #26122 ) ;
#57577 = ORIENTED_EDGE ( 'NONE', *, *, #77763, .F. ) ;
#57579 = CARTESIAN_POINT ( 'NONE',  ( 20.88017736071110164, 20.35535201082150891, 2.915334737309930979 ) ) ;
#57578 = CARTESIAN_POINT ( 'NONE',  ( 15.44008868035555260, 19.73035201082150536, 9.422509992056143702 ) ) ;
#57581 = CARTESIAN_POINT ( 'NONE',  ( 16.40814093676324603, 7.456968003263754419, -11.09922568453594671 ) ) ;
#57580 = CARTESIAN_POINT ( 'NONE',  ( 12.63842701281683034, 47.46726448433412315, 9.846743663894596210 ) ) ;
#57582 = CARTESIAN_POINT ( 'NONE',  ( -6.000000000000009770, 41.24999999999999289, 6.500000000000000888 ) ) ;
#57583 = EDGE_CURVE ( 'NONE', #1778, #38557, #85661, .T. ) ;
#57584 = EDGE_CURVE ( 'NONE', #84722, #91634, #85172, .T. ) ;
#57585 = CARTESIAN_POINT ( 'NONE',  ( 19.38216949554541202, 15.99863466993042138, 9.382169495545424454 ) ) ;
#57586 = VERTEX_POINT ( 'NONE', #63628 ) ;
#57587 = CARTESIAN_POINT ( 'NONE',  ( 1.472469842513823179, 36.42559781766745175, 4.923371831947296329 ) ) ;
#57588 = CARTESIAN_POINT ( 'NONE',  ( 22.26659068614894466, 63.88708216824730357, 7.082119434687054849 ) ) ;
#57589 = ORIENTED_EDGE ( 'NONE', *, *, #25272, .T. ) ;
#57590 = CARTESIAN_POINT ( 'NONE',  ( 7.084665262690076126, 4.105352010821503583, 10.88017736071109987 ) ) ;
#57591 = VERTEX_POINT ( 'NONE', #16681 ) ;
#57592 = CARTESIAN_POINT ( 'NONE',  ( 10.00000000000000178, 39.31368534415484106, 10.88017736071110342 ) ) ;
#57593 = CARTESIAN_POINT ( 'NONE',  ( -0.8801773607110991993, 47.85535201082150536, -2.915334737309923874 ) ) ;
#57594 = CARTESIAN_POINT ( 'NONE',  ( 4.559911319644449179, 53.89701867748817676, 9.422509992056141925 ) ) ;
#57595 = CARTESIAN_POINT ( 'NONE',  ( -3.115783986955657170, 4.161706264368254368E-16, 14.16128137375395468 ) ) ;
#57596 = CARTESIAN_POINT ( 'NONE',  ( 0.5774900079438590739, 42.64701867748816966, -5.440088680355550821 ) ) ;
#57597 = CIRCLE ( 'NONE', #84744, 15.00000000000000000 ) ;
#57598 = CARTESIAN_POINT ( 'NONE',  ( 1.821708436314909640, 46.66792564121895026, -6.499999999999926281 ) ) ;
#57599 = LINE ( 'NONE', #59078, #13815 ) ;
#57600 = CARTESIAN_POINT ( 'NONE',  ( 17.20831665107776587, 14.13393115100078568, -7.208316651077762316 ) ) ;
#57601 = ORIENTED_EDGE ( 'NONE', *, *, #90389, .F. ) ;
#57602 = CARTESIAN_POINT ( 'NONE',  ( 11.04397247079906030, -89.88416767672931940, 4.000000000000000000 ) ) ;
#57603 = CARTESIAN_POINT ( 'NONE',  ( 12.63842701281683034, 62.46726448433410894, 9.846743663894596210 ) ) ;
#57604 = CARTESIAN_POINT ( 'NONE',  ( 10.00000000000000178, 70.00000000000000000, 0.000000000000000000 ) ) ;
#57605 = CARTESIAN_POINT ( 'NONE',  ( -6.445967608602039434, -48.01283281809150338, 3.750000000000000444 ) ) ;
#57606 = ORIENTED_EDGE ( 'NONE', *, *, #66209, .T. ) ;
#57607 = EDGE_CURVE ( 'NONE', #26148, #50878, #24675, .T. ) ;
#57608 = CARTESIAN_POINT ( 'NONE',  ( 19.72487221294570858, 21.86607318730131411, 6.500000000000000888 ) ) ;
#57609 = CARTESIAN_POINT ( 'NONE',  ( -3.628035180575734486, -3.629434796165400989, 3.750000000000000888 ) ) ;
#57611 = CARTESIAN_POINT ( 'NONE',  ( 0.1532563361054082862, 31.21726448433412315, 2.638427012816831674 ) ) ;
#57610 = SURFACE_STYLE_USAGE ( .BOTH. , #27111 ) ;
#57612 = CARTESIAN_POINT ( 'NONE',  ( 2.917880565312950480, 55.97041550158063217, -12.26659068614894821 ) ) ;
#57613 = LINE ( 'NONE', #17674, #97785 ) ;
#57614 = ORIENTED_EDGE ( 'NONE', *, *, #67640, .T. ) ;
#57615 = CARTESIAN_POINT ( 'NONE',  ( -7.313705784284687539, 0.3640475087720989045, 13.09617149020739113 ) ) ;
#57616 = CARTESIAN_POINT ( 'NONE',  ( 0.1532563361054100626, 30.80059781766744820, -2.638427012816831230 ) ) ;
#57617 = FILL_AREA_STYLE ('',( #49141 ) ) ;
#57618 = CARTESIAN_POINT ( 'NONE',  ( 10.00000000000000178, 0.3736346699304200492, 12.81628187352647608 ) ) ;
#57620 = EDGE_CURVE ( 'NONE', #57586, #67582, #47151, .T. ) ;
#57619 = CARTESIAN_POINT ( 'NONE',  ( 0.5774900079438590739, 67.64701867748817676, -5.440088680355550821 ) ) ;
#57621 = PRESENTATION_STYLE_ASSIGNMENT (( #57130 ) ) ;
#57622 = CARTESIAN_POINT ( 'NONE',  ( 17.20831665107776587, 4.133931151000785675, -7.208316651077762316 ) ) ;
#57623 = CARTESIAN_POINT ( 'NONE',  ( 19.84674366389459266, 63.71726448433412315, -2.638427012816827677 ) ) ;
#57624 = CARTESIAN_POINT ( 'NONE',  ( 0.000000000000000000, 35.00000000000000000, 0.000000000000000000 ) ) ;
#57625 = CIRCLE ( 'NONE', #65612, 0.2500000000000002220 ) ;
#57626 = EDGE_LOOP ( 'NONE', ( #39202, #48613, #77510, #3735 ) ) ;
#57627 = CARTESIAN_POINT ( 'NONE',  ( 10.00000000000000000, 6.813685344154838397, -10.88017736071110342 ) ) ;
#57628 = CARTESIAN_POINT ( 'NONE',  ( -4.164238869374099927, 2.012082168247300906, 3.795296366450308767 ) ) ;
#57629 = CARTESIAN_POINT ( 'NONE',  ( 14.92337183194729988, 14.34226448433411782, -8.527530157486177487 ) ) ;
#57630 = CARTESIAN_POINT ( 'NONE',  ( 2.035157376598824452, 38.68868534415483396, 7.964842623401179544 ) ) ;
#57631 = TOROIDAL_SURFACE ( 'NONE', #48069, 0.5000000000000000000, 0.2500000000000000000 ) ;
#57633 = DIRECTION ( 'NONE',  ( 1.000000000000000000, -0.000000000000000000, -0.000000000000000000 ) ) ;
#57632 = CARTESIAN_POINT ( 'NONE',  ( 10.00000000000000000, 32.87363466993042493, -12.81628187352647608 ) ) ;
#57634 = DIRECTION ( 'NONE',  ( 0.000000000000000000, 1.000000000000000000, -0.000000000000000000 ) ) ;
#57636 = CIRCLE ( 'NONE', #92761, 0.2500000000000002220 ) ;
#57635 = DIRECTION ( 'NONE',  ( 0.8070303256584298035, -0.5905099943842175847, 0.000000000000000000 ) ) ;
#57637 = CYLINDRICAL_SURFACE ( 'NONE', #21698, 0.2500000000000002220 ) ;
#57638 = CARTESIAN_POINT ( 'NONE',  ( -2.816281873526473856, -0.6680319967362464695, 3.434112377981055619 ) ) ;
#57639 = CARTESIAN_POINT ( 'NONE',  ( 7.361572987183169658, 19.96726448433411960, -9.846743663894592657 ) ) ;
#57640 = CARTESIAN_POINT ( 'NONE',  ( -10.88017736071110342, -21.93631465584515894, 3.903127820947815962E-15 ) ) ;
#57641 = CARTESIAN_POINT ( 'NONE',  ( 10.00000000000000178, 20.37363466993042138, 12.81628187352647608 ) ) ;
#57642 = CARTESIAN_POINT ( 'NONE',  ( -10.91892017000252046, -97.58704351930606435, -3.999999999999996891 ) ) ;
#57643 = CARTESIAN_POINT ( 'NONE',  ( 4.559911319644449179, 32.23035201082150536, -9.422509992056141925 ) ) ;
#57644 = DIRECTION ( 'NONE',  ( 1.000000000000000000, 0.000000000000000000, 0.000000000000000000 ) ) ;
#57645 = CARTESIAN_POINT ( 'NONE',  ( -2.266590686148945544, 47.22041550158063927, 7.082119434687048631 ) ) ;
#57646 = FILL_AREA_STYLE_COLOUR ( '', #44923 ) ;
#57647 = CARTESIAN_POINT ( 'NONE',  ( 2.791683348922240793, 46.63393115100077324, 7.208316651077764092 ) ) ;
#57648 = CARTESIAN_POINT ( 'NONE',  ( 0.6178305044545818747, 38.49863466993042493, -9.382169495545419124 ) ) ;
#57649 = CARTESIAN_POINT ( 'NONE',  ( 15.44008868035555793, 31.39701867748817676, -9.422509992056140149 ) ) ;
#57650 = CARTESIAN_POINT ( 'NONE',  ( 5.076628168052703671, 46.84226448433412315, 8.527530157486179263 ) ) ;
#57651 = CARTESIAN_POINT ( 'NONE',  ( 4.559911319644449179, 52.23035201082151247, -9.422509992056141925 ) ) ;
#57652 = CARTESIAN_POINT ( 'NONE',  ( 21.09922568453594849, 6.206968003263753531, 6.408140936763242479 ) ) ;
#57653 = CARTESIAN_POINT ( 'NONE',  ( -2.266590686148945544, 32.22041550158063927, 7.082119434687048631 ) ) ;
#57654 = CARTESIAN_POINT ( 'NONE',  ( -14.43100913236846061, 15.00000000000000000, -1.412789942453363423 ) ) ;
#57655 = CARTESIAN_POINT ( 'NONE',  ( 17.20831665107776587, 19.13393115100078035, -7.208316651077762316 ) ) ;
#57656 = CARTESIAN_POINT ( 'NONE',  ( 19.38216949554541557, 62.24863466993041072, -9.382169495545420901 ) ) ;
#57657 = CARTESIAN_POINT ( 'NONE',  ( 5.076628168052704559, 65.17559781766745175, -8.527530157486179263 ) ) ;
#57658 = ORIENTED_EDGE ( 'NONE', *, *, #91312, .T. ) ;
#57659 = SURFACE_STYLE_FILL_AREA ( #33189 ) ;
#57660 = CARTESIAN_POINT ( 'NONE',  ( 12.91533473730992121, 14.52201867748817143, 10.88017736071110164 ) ) ;
#57662 = CARTESIAN_POINT ( 'NONE',  ( 17.75000000000000355, 73.00000000000001421, 6.250000000000000000 ) ) ;
#57661 = CARTESIAN_POINT ( 'NONE',  ( -0.3689425029237898834, 31.17874883491396787, -10.36894250292378850 ) ) ;
#57663 = CARTESIAN_POINT ( 'NONE',  ( 7.084665262690076126, 67.02201867748817676, -10.88017736071110164 ) ) ;
#57664 = CARTESIAN_POINT ( 'NONE',  ( 12.63842701281683922, 54.55059781766745175, -9.846743663894590881 ) ) ;
#57665 = CARTESIAN_POINT ( 'NONE',  ( 12.91533473730993009, 31.60535201082150891, -10.88017736071109987 ) ) ;
#57666 = DIRECTION ( 'NONE',  ( 0.000000000000000000, 0.000000000000000000, -1.000000000000000000 ) ) ;
#57667 = CARTESIAN_POINT ( 'NONE',  ( 2.913501739333757889, 3.989000423594319145E-16, -14.20427779279535230 ) ) ;
#57668 = VECTOR ( 'NONE', #83357, 1000.000000000000000 ) ;
#57669 = VECTOR ( 'NONE', #75847, 1000.000000000000000 ) ;
#57670 = EDGE_CURVE ( 'NONE', #2401, #22706, #94134, .T. ) ;
#57671 = ORIENTED_EDGE ( 'NONE', *, *, #37323, .T. ) ;
#57672 = CARTESIAN_POINT ( 'NONE',  ( 6.683977931330074895, -73.15273079441168136, 2.500000000000000000 ) ) ;
#57673 = CARTESIAN_POINT ( 'NONE',  ( 5.076628168052703671, 51.84226448433412315, 8.527530157486179263 ) ) ;
#57674 = ORIENTED_EDGE ( 'NONE', *, *, #78891, .T. ) ;
#57675 = EDGE_LOOP ( 'NONE', ( #21011, #78755, #86959, #66320 ) ) ;
#57676 = AXIS2_PLACEMENT_3D ( 'NONE', #80530, #18550, #56546 ) ;
#57677 = CARTESIAN_POINT ( 'NONE',  ( -4.164238869374098151, 11.59541550158063217, -3.795296366450310543 ) ) ;
#57678 = CARTESIAN_POINT ( 'NONE',  ( 22.26659068614895176, 4.720415501580633943, -7.082119434687042414 ) ) ;
#57679 = CARTESIAN_POINT ( 'NONE',  ( 10.00000000000000178, 49.31368534415484106, 10.88017736071110342 ) ) ;
#57680 = CARTESIAN_POINT ( 'NONE',  ( -0.3689425029237881626, 52.42874883491396076, 10.36894250292379027 ) ) ;
#57681 = CARTESIAN_POINT ( 'NONE',  ( 17.20831665107776587, 52.88393115100078035, 7.208316651077764980 ) ) ;
#57682 = CARTESIAN_POINT ( 'NONE',  ( 0.1532563361054082862, 31.21726448433412315, 2.638427012816831674 ) ) ;
#57684 = CARTESIAN_POINT ( 'NONE',  ( 22.81628187352648496, 11.83196800326375531, -3.434112377981050290 ) ) ;
#57683 = CARTESIAN_POINT ( 'NONE',  ( -0.8801773607110991993, 32.85535201082151247, -2.915334737309923874 ) ) ;
#57685 = CARTESIAN_POINT ( 'NONE',  ( 24.16423886937410614, 4.512082168247300906, -3.795296366450302550 ) ) ;
#57686 = EDGE_CURVE ( 'NONE', #57201, #97596, #86158, .T. ) ;
#57687 = CARTESIAN_POINT ( 'NONE',  ( 17.08211943468705130, 53.47041550158063217, 12.26659068614894998 ) ) ;
#57688 = CARTESIAN_POINT ( 'NONE',  ( 20.88017736071110875, 5.772018677488170546, -2.915334737309920765 ) ) ;
#57689 = CARTESIAN_POINT ( 'NONE',  ( 6.382347221874423937, 0.5000000000000004441, -13.57444820018227638 ) ) ;
#57690 = DIRECTION ( 'NONE',  ( 0.000000000000000000, 0.000000000000000000, 1.000000000000000000 ) ) ;
#57691 = CARTESIAN_POINT ( 'NONE',  ( -4.923371831947302546, -34.82440218233254114, -8.527530157486173934 ) ) ;
#57692 = EDGE_LOOP ( 'NONE', ( #95198, #80568, #57742, #96501 ) ) ;
#57693 = ORIENTED_EDGE ( 'NONE', *, *, #13609, .T. ) ;
#57694 = CARTESIAN_POINT ( 'NONE',  ( 14.92337183194729633, 22.67559781766745175, 8.527530157486181039 ) ) ;
#57695 = ORIENTED_EDGE ( 'NONE', *, *, #34928, .F. ) ;
#57696 = CARTESIAN_POINT ( 'NONE',  ( 2.917880565312948704, 27.63708216824730357, 12.26659068614894643 ) ) ;
#57697 = CARTESIAN_POINT ( 'NONE',  ( 12.63842701281683922, 39.55059781766744464, -9.846743663894590881 ) ) ;
#57698 = CARTESIAN_POINT ( 'NONE',  ( -0.8801773607111009756, 63.06368534415484106, 1.068504757029289695E-15 ) ) ;
#57699 = FACE_OUTER_BOUND ( 'NONE', #84625, .T. ) ;
#57700 = CARTESIAN_POINT ( 'NONE',  ( 10.00000000000000000, 51.81368534415484106, -10.88017736071110342 ) ) ;
#57701 = EDGE_CURVE ( 'NONE', #44176, #1795, #58636, .T. ) ;
#57702 = CARTESIAN_POINT ( 'NONE',  ( 10.00000000000000000, 62.87363466993042493, -12.81628187352647608 ) ) ;
#57703 = CARTESIAN_POINT ( 'NONE',  ( 3.434112377981060948, 10.58196800326375353, 12.81628187352647430 ) ) ;
#57704 = ORIENTED_EDGE ( 'NONE', *, *, #89986, .F. ) ;
#57705 = CARTESIAN_POINT ( 'NONE',  ( 20.36894250292379738, 14.92874883491396432, -10.36894250292379027 ) ) ;
#57706 = ADVANCED_FACE ( 'NONE', ( #9666 ), #4249, .F. ) ;
#57707 = VERTEX_POINT ( 'NONE', #95110 ) ;
#57708 = CARTESIAN_POINT ( 'NONE',  ( 3.591859063236761518, 49.95696800326375353, 11.09922568453594849 ) ) ;
#57709 = CARTESIAN_POINT ( 'NONE',  ( -0.8801773607111009756, 18.06368534415484106, 1.068504757029289695E-15 ) ) ;
#57710 = CARTESIAN_POINT ( 'NONE',  ( 10.00000000000000178, 17.25893115100078745, 9.846743663894594434 ) ) ;
#57711 = CARTESIAN_POINT ( 'NONE',  ( 4.559911319644449179, 17.23035201082150536, -9.422509992056141925 ) ) ;
#57712 = CARTESIAN_POINT ( 'NONE',  ( 0.6178305044545838731, 49.74863466993041072, 9.382169495545420901 ) ) ;
#57713 = CARTESIAN_POINT ( 'NONE',  ( -4.000000000000000000, 10.00000000000000000, -2.500000000000000000 ) ) ;
#57714 = CARTESIAN_POINT ( 'NONE',  ( 2.791683348922237240, 25.38393115100078390, -7.208316651077763204 ) ) ;
#57715 = CARTESIAN_POINT ( 'NONE',  ( -12.83294900548073336, 14.49999999999999112, 7.766300266068329350 ) ) ;
#57716 = DIRECTION ( 'NONE',  ( 0.000000000000000000, 1.000000000000000000, 0.000000000000000000 ) ) ;
#57717 = CARTESIAN_POINT ( 'NONE',  ( 15.44008868035555260, 64.73035201082151957, 9.422509992056143702 ) ) ;
#57718 = CARTESIAN_POINT ( 'NONE',  ( 19.72487221294570858, 7.802231764288317883, -6.499999999999999112 ) ) ;
#57719 = CARTESIAN_POINT ( 'NONE',  ( -0.2418659066527654722, 45.11633188102327807, 6.114288769123054301 ) ) ;
#57720 = CARTESIAN_POINT ( 'NONE',  ( 5.076628168052704559, 20.17559781766745175, -8.527530157486179263 ) ) ;
#57721 = CARTESIAN_POINT ( 'NONE',  ( -1.099225684535947600, 19.54030133659708568, 6.408140936763237150 ) ) ;
#57722 = CARTESIAN_POINT ( 'NONE',  ( 3.420591144908545100, 0.5000000000000004441, -14.60477854057955938 ) ) ;
#57723 = CARTESIAN_POINT ( 'NONE',  ( 17.20831665107776587, 44.13393115100078745, -7.208316651077762316 ) ) ;
#57724 = CARTESIAN_POINT ( 'NONE',  ( -14.99847009497944583, 0.5000000000000004441, 0.2142307401079343032 ) ) ;
#57725 = CARTESIAN_POINT ( 'NONE',  ( 10.00000000000000000, 15.55374883491396787, -14.16423886937410082 ) ) ;
#57726 = CARTESIAN_POINT ( 'NONE',  ( 17.20831665107776587, 37.88393115100078745, 7.208316651077764980 ) ) ;
#57727 = CARTESIAN_POINT ( 'NONE',  ( 6.565887622018943937, 30.16530133659708568, 12.81628187352647430 ) ) ;
#57729 = CARTESIAN_POINT ( 'NONE',  ( -14.02068044289371684, 0.5000000000000004441, -5.331089937175857330 ) ) ;
#57728 = DIRECTION ( 'NONE',  ( 0.000000000000000000, 0.000000000000000000, 1.000000000000000000 ) ) ;
#57730 = CARTESIAN_POINT ( 'NONE',  ( 2.035157376598822676, 62.43868534415483396, -7.964842623401177768 ) ) ;
#57731 = CARTESIAN_POINT ( 'NONE',  ( 13.43411237798105340, 0.5819680032637533085, 12.81628187352647963 ) ) ;
#57732 = DIRECTION ( 'NONE',  ( -0.5901017155109078427, -0.8073289077885689169, 0.000000000000000000 ) ) ;
#57733 = CARTESIAN_POINT ( 'NONE',  ( 12.63842701281683922, 34.55059781766745886, -9.846743663894590881 ) ) ;
#57735 = EDGE_CURVE ( 'NONE', #81929, #86010, #72118, .T. ) ;
#57734 = CARTESIAN_POINT ( 'NONE',  ( 15.44008868035555793, 21.39701867748817321, -9.422509992056140149 ) ) ;
#57736 = CARTESIAN_POINT ( 'NONE',  ( 3.591859063236763294, 33.29030133659708213, -11.09922568453595026 ) ) ;
#57737 = CARTESIAN_POINT ( 'NONE',  ( 1.472469842513823179, 30.59226448433411960, -4.923371831947296329 ) ) ;
#57738 =( BOUNDED_CURVE ( )  B_SPLINE_CURVE ( 2, ( #18276, #48265, #94257, #25784, #80740, #78778, #10284, #88232, #12235 ),
 .UNSPECIFIED., .F., .F. ) 
 B_SPLINE_CURVE_WITH_KNOTS ( ( 3, 2, 2, 2, 3 ),
 ( 0.2962860886497511448, 0.2976190476190476164, 0.3035714285714285476, 0.3095238095238095344, 0.3108567684931059505 ),
 .UNSPECIFIED. ) 
 CURVE ( )  GEOMETRIC_REPRESENTATION_ITEM ( )  RATIONAL_B_SPLINE_CURVE ( ( 0.9881565478350728959, 0.9923695281211487584, 1.000000000000000000, 0.9659258262890683122, 1.000000000000000000, 0.9659258262890683122, 1.000000000000000000, 0.9923695281211490915, 0.9881565478350733400 ) ) 
 REPRESENTATION_ITEM ( '' )  );
#57739 = CARTESIAN_POINT ( 'NONE',  ( -228.9177352951725481, -142.1062388753802566, -59.32363299443191096 ) ) ;
#57740 = CARTESIAN_POINT ( 'NONE',  ( -5.204170427930421283E-15, 6.671802177851543725, -11.25000000000000178 ) ) ;
#57741 = CARTESIAN_POINT ( 'NONE',  ( 17.96484262340118221, 36.18868534415484106, -7.964842623401177768 ) ) ;
#57742 = ORIENTED_EDGE ( 'NONE', *, *, #85590, .T. ) ;
#57743 = CARTESIAN_POINT ( 'NONE',  ( -11.25000000000000000, 5.326366962315977283, 3.014428414850140570 ) ) ;
#57744 = CARTESIAN_POINT ( 'NONE',  ( 20.88017736071110164, 5.355352010821502695, 2.915334737309930979 ) ) ;
#57746 = CARTESIAN_POINT ( 'NONE',  ( 20.88017736071110875, 25.77201867748816966, -2.915334737309920765 ) ) ;
#57745 = CARTESIAN_POINT ( 'NONE',  ( 18.52753015748617571, 53.09226448433412315, 4.923371831947298993 ) ) ;
#57747 = CARTESIAN_POINT ( 'NONE',  ( 15.00000000000000000, 77.07179676972447169, 6.250000000000000000 ) ) ;
#57748 = CARTESIAN_POINT ( 'NONE',  ( -0.8801773607111009756, 53.06368534415484106, 1.068504757029289695E-15 ) ) ;
#57749 = B_SPLINE_CURVE_WITH_KNOTS ( 'NONE', 3,
 ( #84985, #8983, #1517, #31962 ),
 .UNSPECIFIED., .F., .F.,
 ( 4, 4 ),
 ( 0.000000000000000000, 0.001036303429213010323 ),
 .UNSPECIFIED. ) ;
#57751 = CARTESIAN_POINT ( 'NONE',  ( -0.000000000000000000, 75.99261571001677851, -6.807497417685388186 ) ) ;
#57750 = CARTESIAN_POINT ( 'NONE',  ( 17.96484262340118221, 26.18868534415483396, -7.964842623401177768 ) ) ;
#57752 = CARTESIAN_POINT ( 'NONE',  ( 18.52753015748617571, 3.092264484334118269, 4.923371831947298993 ) ) ;
#57753 = DIRECTION ( 'NONE',  ( -0.000000000000000000, -0.000000000000000000, -1.000000000000000000 ) ) ;
#57754 = CARTESIAN_POINT ( 'NONE',  ( 0.1532563361054100626, 55.80059781766745175, -2.638427012816831230 ) ) ;
#57756 = CARTESIAN_POINT ( 'NONE',  ( 6.910419567532135154, -84.29192550413311835, 3.750000000000001776 ) ) ;
#57755 = CARTESIAN_POINT ( 'NONE',  ( 24.16423886937410614, 54.51208216824730357, -3.795296366450302550 ) ) ;
#57757 = DIRECTION ( 'NONE',  ( -0.000000000000000000, -1.000000000000000000, -0.000000000000000000 ) ) ;
#57758 = CARTESIAN_POINT ( 'NONE',  ( -4.164238869374099039, 6.803748834913967869, 8.674139862899312516E-16 ) ) ;
#57759 = CARTESIAN_POINT ( 'NONE',  ( 6.204703633549690345, 40.76208216824731778, -14.16423886937410259 ) ) ;
#57760 = PRESENTATION_LAYER_ASSIGNMENT (  '', '', ( #59333 ) ) ;
#57761 = CARTESIAN_POINT ( 'NONE',  ( -1.099225684535947600, 4.540301336597087456, 6.408140936763237150 ) ) ;
#57762 = CARTESIAN_POINT ( 'NONE',  ( -8.399999999999998579, 98.49999999999998579, -8.525133428036873795 ) ) ;
#57763 = ORIENTED_EDGE ( 'NONE', *, *, #9021, .F. ) ;
#57764 = CARTESIAN_POINT ( 'NONE',  ( -4.164238869374098151, 66.59541550158060375, -3.795296366450310543 ) ) ;
#57765 = CARTESIAN_POINT ( 'NONE',  ( 1.472469842513823179, 40.59226448433411605, -4.923371831947296329 ) ) ;
#57766 = CARTESIAN_POINT ( 'NONE',  ( -3.750000000000000000, 10.00000000000000000, 2.750000000000000000 ) ) ;
#57767 = CARTESIAN_POINT ( 'NONE',  ( 17.96484262340118221, 59.93868534415484106, 7.964842623401181321 ) ) ;
#57768 = EDGE_CURVE ( 'NONE', #25488, #30081, #64602, .T. ) ;
#57769 = AXIS2_PLACEMENT_3D ( 'NONE', #54374, #7429, #61384 ) ;
#57770 = CARTESIAN_POINT ( 'NONE',  ( -1.099225684535947600, 59.54030133659708923, 6.408140936763237150 ) ) ;
#57771 = CARTESIAN_POINT ( 'NONE',  ( 21.09922568453594849, 31.20696800326375353, 6.408140936763242479 ) ) ;
#57772 = CARTESIAN_POINT ( 'NONE',  ( 19.84674366389459266, 33.30059781766744464, 2.638427012816836559 ) ) ;
#57773 = VERTEX_POINT ( 'NONE', #94631 ) ;
#57774 = CARTESIAN_POINT ( 'NONE',  ( 9.879999999999988347, 26.99999999999999645, 2.900000000000000355 ) ) ;
#57775 = CARTESIAN_POINT ( 'NONE',  ( -4.164238869374098151, 61.59541550158063217, -3.795296366450310543 ) ) ;
#57776 = CARTESIAN_POINT ( 'NONE',  ( 10.00000000000000000, 11.81368534415483751, -10.88017736071110342 ) ) ;
#57777 = CARTESIAN_POINT ( 'NONE',  ( 10.00000000000000000, 45.55374883491397497, -14.16423886937410082 ) ) ;
#57778 = CARTESIAN_POINT ( 'NONE',  ( -0.8801773607111009756, 33.06368534415484106, 1.068504757029289695E-15 ) ) ;
#57779 = CARTESIAN_POINT ( 'NONE',  ( 12.91533473730993009, 66.60535201082150536, -10.88017736071109987 ) ) ;
#57780 = CARTESIAN_POINT ( 'NONE',  ( -0.7375392941515958034, 14.49999999999999112, -14.98185688723478215 ) ) ;
#57781 = CARTESIAN_POINT ( 'NONE',  ( 12.00809552683952752, 0.5000000000000004441, 8.989195838243626113 ) ) ;
#57782 = CARTESIAN_POINT ( 'NONE',  ( 0.1532563361054100626, 15.80059781766745353, -2.638427012816831230 ) ) ;
#57783 = DIRECTION ( 'NONE',  ( 0.000000000000000000, 0.000000000000000000, 1.000000000000000000 ) ) ;
#57784 = CARTESIAN_POINT ( 'NONE',  ( 19.84674366389459266, 3.717264484334118713, -2.638427012816827677 ) ) ;
#57785 = CARTESIAN_POINT ( 'NONE',  ( 0.9082943533636183009, 15.00000000000000000, 14.47152380945585648 ) ) ;
#57786 = CARTESIAN_POINT ( 'NONE',  ( 19.84674366389459266, 43.71726448433410894, -2.638427012816827677 ) ) ;
#57787 = CARTESIAN_POINT ( 'NONE',  ( 1.472469842513823179, 61.42559781766745175, 4.923371831947296329 ) ) ;
#57788 = CARTESIAN_POINT ( 'NONE',  ( 17.96484262340118221, 26.18868534415483396, -7.964842623401177768 ) ) ;
#57789 = ADVANCED_FACE ( 'NONE', ( #80114 ), #57067, .T. ) ;
#57790 = ORIENTED_EDGE ( 'NONE', *, *, #24810, .T. ) ;
#57791 = CARTESIAN_POINT ( 'NONE',  ( -2.816281873526473856, 49.12363466993042493, 9.499525473075851096E-16 ) ) ;
#57792 = DIRECTION ( 'NONE',  ( 0.000000000000000000, 1.000000000000000000, 0.000000000000000000 ) ) ;
#57793 = CARTESIAN_POINT ( 'NONE',  ( -0.8801773607110991993, 62.85535201082150536, -2.915334737309923874 ) ) ;
#57794 = CARTESIAN_POINT ( 'NONE',  ( 18.52753015748618282, 23.92559781766745530, -4.923371831947291888 ) ) ;
#57796 = CARTESIAN_POINT ( 'NONE',  ( 2.791683348922240793, 21.63393115100078745, 7.208316651077764092 ) ) ;
#57795 = CARTESIAN_POINT ( 'NONE',  ( 6.204703633549690345, 52.84541550158062506, 14.16423886937410082 ) ) ;
#57798 = ADVANCED_FACE ( 'NONE', ( #35095 ), #34602, .F. ) ;
#57797 = DIRECTION ( 'NONE',  ( 0.5547001962252290364, 0.8320502943378437211, 0.000000000000000000 ) ) ;
#57799 = EDGE_CURVE ( 'NONE', #41402, #4498, #72603, .T. ) ;
#57800 = CARTESIAN_POINT ( 'NONE',  ( 1.472469842513823179, 61.42559781766745175, 4.923371831947296329 ) ) ;
#57801 = CARTESIAN_POINT ( 'NONE',  ( 6.204703633549690345, 27.84541550158063217, 14.16423886937410082 ) ) ;
#57802 = CARTESIAN_POINT ( 'NONE',  ( 2.791683348922237240, 45.38393115100079456, -7.208316651077763204 ) ) ;
#57803 = CARTESIAN_POINT ( 'NONE',  ( 4.999999999999999112, 11.50000000000000000, -6.000000000000000000 ) ) ;
#57804 = CARTESIAN_POINT ( 'NONE',  ( 0.5774900079438607392, 23.48035201082150536, 5.440088680355550821 ) ) ;
#57805 = CARTESIAN_POINT ( 'NONE',  ( 19.42250999205614193, 65.14701867748817676, 5.440088680355555262 ) ) ;
#57806 = ORIENTED_EDGE ( 'NONE', *, *, #94151, .F. ) ;
#57807 = CARTESIAN_POINT ( 'NONE',  ( -1.099225684535947600, 44.54030133659708923, 6.408140936763237150 ) ) ;
#57808 = ORIENTED_EDGE ( 'NONE', *, *, #51184, .F. ) ;
#57809 = CARTESIAN_POINT ( 'NONE',  ( 0.5774900079438590739, 52.64701867748817676, -5.440088680355550821 ) ) ;
#57810 = ORIENTED_EDGE ( 'NONE', *, *, #86392, .T. ) ;
#57811 =( NAMED_UNIT ( * ) SI_UNIT ( $, .STERADIAN. ) SOLID_ANGLE_UNIT ( ) );
#57812 = LINE ( 'NONE', #97828, #32849 ) ;
#57813 = ORIENTED_EDGE ( 'NONE', *, *, #92675, .F. ) ;
#57814 = CARTESIAN_POINT ( 'NONE',  ( 12.91533473730992121, 59.52201867748816966, 10.88017736071110164 ) ) ;
#57815 = CARTESIAN_POINT ( 'NONE',  ( 15.44008868035555260, 14.73035201082150536, 9.422509992056143702 ) ) ;
#57816 = TOROIDAL_SURFACE ( 'NONE', #62592, 14.49999999999999822, 0.5000000000000000000 ) ;
#57817 = CARTESIAN_POINT ( 'NONE',  ( 18.04007052943773104, 9.002578601053489393, -5.767676674365834977 ) ) ;
#57818 = FILL_AREA_STYLE_COLOUR ( '', #8947 ) ;
#57819 = CARTESIAN_POINT ( 'NONE',  ( 10.00000000000000000, 6.813685344154838397, -10.88017736071110342 ) ) ;
#57820 = CARTESIAN_POINT ( 'NONE',  ( 5.076628168052704559, 25.17559781766745175, -8.527530157486179263 ) ) ;
#57821 = CARTESIAN_POINT ( 'NONE',  ( -4.164238869374099927, 17.01208216824730357, 3.795296366450308767 ) ) ;
#57822 = CARTESIAN_POINT ( 'NONE',  ( 7.084665262690076126, 17.02201867748817676, -10.88017736071110164 ) ) ;
#57823 = CARTESIAN_POINT ( 'NONE',  ( 0.1532563361054100626, 60.80059781766744464, -2.638427012816831230 ) ) ;
#57824 = ORIENTED_EDGE ( 'NONE', *, *, #90094, .T. ) ;
#57825 = ADVANCED_FACE ( 'NONE', ( #65096 ), #15134, .T. ) ;
#57826 = CARTESIAN_POINT ( 'NONE',  ( 14.92337183194729988, 64.34226448433412315, -8.527530157486177487 ) ) ;
#57827 = VERTEX_POINT ( 'NONE', #84705 ) ;
#57828 = CARTESIAN_POINT ( 'NONE',  ( 20.88017736071110164, 50.35535201082151247, 2.915334737309930979 ) ) ;
#57829 = LINE ( 'NONE', #51321, #86558 ) ;
#57830 = CARTESIAN_POINT ( 'NONE',  ( 13.43411237798106583, 42.66530133659707502, -12.81628187352647252 ) ) ;
#57831 = LINE ( 'NONE', #34334, #11191 ) ;
#57832 = CARTESIAN_POINT ( 'NONE',  ( 19.42250999205614548, 60.98035201082151247, -5.440088680355545492 ) ) ;
#57833 = CARTESIAN_POINT ( 'NONE',  ( 7.084665262690076126, 22.02201867748817321, -10.88017736071110164 ) ) ;
#57834 = AXIS2_PLACEMENT_3D ( 'NONE', #44695, #6213, #60189 ) ;
#57835 = CARTESIAN_POINT ( 'NONE',  ( 13.43411237798105340, 35.58196800326375353, 12.81628187352647963 ) ) ;
#57836 = CARTESIAN_POINT ( 'NONE',  ( -0.8801773607110991993, 27.85535201082150181, -2.915334737309923874 ) ) ;
#57837 = LINE ( 'NONE', #51334, #57880 ) ;
#57838 = CARTESIAN_POINT ( 'NONE',  ( -2.816281873526473856, 44.33196800326375353, 3.434112377981055619 ) ) ;
#57839 = CARTESIAN_POINT ( 'NONE',  ( 10.00000000000000178, 34.31368534415484106, 10.88017736071110342 ) ) ;
#57840 = CARTESIAN_POINT ( 'NONE',  ( 7.361572987183170547, 52.05059781766745175, 9.846743663894590881 ) ) ;
#57841 = ORIENTED_EDGE ( 'NONE', *, *, #42717, .F. ) ;
#57843 = FACE_OUTER_BOUND ( 'NONE', #62978, .T. ) ;
#57842 = CIRCLE ( 'NONE', #76993, 2.000000000000000000 ) ;
#57844 = CARTESIAN_POINT ( 'NONE',  ( 14.92337183194729988, 64.34226448433412315, -8.527530157486177487 ) ) ;
#57846 = CARTESIAN_POINT ( 'NONE',  ( 19.84674366389459266, 48.71726448433413026, -2.638427012816827677 ) ) ;
#57845 = DIRECTION ( 'NONE',  ( 0.000000000000000000, 0.000000000000000000, -1.000000000000000000 ) ) ;
#57847 = CARTESIAN_POINT ( 'NONE',  ( 4.559911319644449179, 28.89701867748817321, 9.422509992056141925 ) ) ;
#57848 = DIRECTION ( 'NONE',  ( 1.000000000000000000, 0.000000000000000000, 0.000000000000000000 ) ) ;
#57849 = CARTESIAN_POINT ( 'NONE',  ( 10.00000000000000178, 42.25893115100078745, 9.846743663894594434 ) ) ;
#57850 = CARTESIAN_POINT ( 'NONE',  ( 19.72487221294570858, 51.86607318730076344, 6.500000000000000888 ) ) ;
#57851 = FACE_OUTER_BOUND ( 'NONE', #45660, .T. ) ;
#57852 = CARTESIAN_POINT ( 'NONE',  ( 5.076628168052703671, 36.84226448433412315, 8.527530157486179263 ) ) ;
#57853 = CARTESIAN_POINT ( 'NONE',  ( 2.791683348922240793, 1.633931151000784565, 7.208316651077764092 ) ) ;
#57855 = ORIENTED_EDGE ( 'NONE', *, *, #75342, .T. ) ;
#57854 = CARTESIAN_POINT ( 'NONE',  ( 14.92337183194729633, 62.67559781766745886, 8.527530157486181039 ) ) ;
#57856 = FILL_AREA_STYLE ('',( #44332 ) ) ;
#57857 = LINE ( 'NONE', #12851, #32639 ) ;
#57858 = CARTESIAN_POINT ( 'NONE',  ( -2.816281873526473856, 39.33196800326374643, 3.434112377981055619 ) ) ;
#57859 = CARTESIAN_POINT ( 'NONE',  ( 17.20831665107776587, 39.13393115100079456, -7.208316651077762316 ) ) ;
#57860 = FACE_OUTER_BOUND ( 'NONE', #11400, .T. ) ;
#57861 = CARTESIAN_POINT ( 'NONE',  ( 6.204703633549690345, 55.76208216824730357, -14.16423886937410259 ) ) ;
#57862 = CARTESIAN_POINT ( 'NONE',  ( 14.92337183194729633, 32.67559781766745175, 8.527530157486181039 ) ) ;
#57863 = LINE ( 'NONE', #86896, #63179 ) ;
#57864 = CARTESIAN_POINT ( 'NONE',  ( 24.16423886937410614, 59.30374883491397497, 8.672049930838204340E-16 ) ) ;
#57865 = CARTESIAN_POINT ( 'NONE',  ( 12.58848565468357883, 15.00000000000000888, -7.447709424579856297 ) ) ;
#57866 = CARTESIAN_POINT ( 'NONE',  ( 19.42250999205614548, 25.98035201082150891, -5.440088680355545492 ) ) ;
#57867 = AXIS2_PLACEMENT_3D ( 'NONE', #6456, #95496, #57486 ) ;
#57868 = CARTESIAN_POINT ( 'NONE',  ( -2.266590686148945544, 41.38708216824729647, -7.082119434687050408 ) ) ;
#57870 = LINE ( 'NONE', #96393, #35097 ) ;
#57869 = CARTESIAN_POINT ( 'NONE',  ( 6.204703633549690345, 55.76208216824730357, -14.16423886937410259 ) ) ;
#57871 = CARTESIAN_POINT ( 'NONE',  ( 1.472469842513823179, 15.59226448433411960, -4.923371831947296329 ) ) ;
#57873 = CARTESIAN_POINT ( 'NONE',  ( 2.791683348922237240, 65.38393115100078035, -7.208316651077763204 ) ) ;
#57872 = CARTESIAN_POINT ( 'NONE',  ( 6.935134328181136176, -80.57830137131841752, 2.500000000002415401 ) ) ;
#57874 = CARTESIAN_POINT ( 'NONE',  ( 12.91533473730992121, 54.52201867748816255, 10.88017736071110164 ) ) ;
#57875 = DIRECTION ( 'NONE',  ( -1.257402221000611116E-16, 1.000000000000000000, 0.000000000000000000 ) ) ;
#57876 = CARTESIAN_POINT ( 'NONE',  ( 1.472469842513823179, 50.59226448433411605, -4.923371831947296329 ) ) ;
#57877 = LINE ( 'NONE', #58363, #58703 ) ;
#57878 = CARTESIAN_POINT ( 'NONE',  ( 5.076628168052704559, 60.17559781766745175, -8.527530157486179263 ) ) ;
#57879 = CARTESIAN_POINT ( 'NONE',  ( 2.917880565312948704, 2.637082168247300906, 12.26659068614894643 ) ) ;
#57880 = VECTOR ( 'NONE', #43818, 1000.000000000000000 ) ;
#57881 = VERTEX_POINT ( 'NONE', #39213 ) ;
#57882 = CARTESIAN_POINT ( 'NONE',  ( -4.164238869374099039, 31.80374883491396432, 8.674139862899312516E-16 ) ) ;
#57884 = CARTESIAN_POINT ( 'NONE',  ( 2.603489959281601873, 25.43575266056827289, -6.500000000000015987 ) ) ;
#57883 = CARTESIAN_POINT ( 'NONE',  ( -3.271890209819572792, -0.8418601081564157651, -2.499999999999999112 ) ) ;
#57885 = CARTESIAN_POINT ( 'NONE',  ( 19.42250999205614548, 15.98035201082150714, -5.440088680355545492 ) ) ;
#57886 = CARTESIAN_POINT ( 'NONE',  ( 21.09922568453594849, 36.20696800326375353, 6.408140936763242479 ) ) ;
#57887 = CARTESIAN_POINT ( 'NONE',  ( -7.108715748588991801, 14.95077488074853456, -12.92719074505376575 ) ) ;
#57888 = CARTESIAN_POINT ( 'NONE',  ( 2.791683348922240793, 6.633931151000785675, 7.208316651077764092 ) ) ;
#57889 = DIRECTION ( 'NONE',  ( -0.000000000000000000, -1.000000000000000000, -0.000000000000000000 ) ) ;
#57890 = ORIENTED_EDGE ( 'NONE', *, *, #51700, .F. ) ;
#57891 = CARTESIAN_POINT ( 'NONE',  ( 5.170525679121678486, -13.81869365337359845, -4.000000000000000000 ) ) ;
#57892 = CARTESIAN_POINT ( 'NONE',  ( 24.16423886937410614, 29.51208216824729647, -3.795296366450302550 ) ) ;
#57893 = SURFACE_STYLE_FILL_AREA ( #13392 ) ;
#57894 = CARTESIAN_POINT ( 'NONE',  ( 10.00000000000000178, 4.313685344154837509, 10.88017736071110342 ) ) ;
#57895 = CARTESIAN_POINT ( 'NONE',  ( 0.000000000000000000, 0.5000000000000004441, 0.000000000000000000 ) ) ;
#57896 = CARTESIAN_POINT ( 'NONE',  ( 12.50534872682732690, 4.484280952698287085E-16, -7.339363270777523596 ) ) ;
#57897 = CARTESIAN_POINT ( 'NONE',  ( 15.44008868035555793, 46.39701867748817676, -9.422509992056140149 ) ) ;
#57898 = CARTESIAN_POINT ( 'NONE',  ( 2.035157376598822676, 47.43868534415484817, -7.964842623401177768 ) ) ;
#57899 = CARTESIAN_POINT ( 'NONE',  ( 16.40814093676324603, 12.45696800326375353, -11.09922568453594671 ) ) ;
#57900 = SURFACE_SIDE_STYLE ('',( #93947 ) ) ;
#57901 = CARTESIAN_POINT ( 'NONE',  ( 2.271632352219104423, 1.405976953357037207, 6.499999999999993783 ) ) ;
#57902 = CARTESIAN_POINT ( 'NONE',  ( 17.20831665107776587, 12.88393115100078390, 7.208316651077764980 ) ) ;
#57903 = EDGE_CURVE ( 'NONE', #63872, #77456, #22049, .T. ) ;
#57904 = SURFACE_SIDE_STYLE ('',( #96430 ) ) ;
#57905 = CARTESIAN_POINT ( 'NONE',  ( 7.084665262690076126, 49.10535201082149825, 10.88017736071109987 ) ) ;
#57906 = AXIS2_PLACEMENT_3D ( 'NONE', #33143, #18652, #57126 ) ;
#57907 = EDGE_CURVE ( 'NONE', #19780, #10063, #35553, .T. ) ;
#57908 = CARTESIAN_POINT ( 'NONE',  ( 10.00000000000000000, 7.873634669930421381, -12.81628187352647608 ) ) ;
#57909 = CARTESIAN_POINT ( 'NONE',  ( 0.5774900079438607392, 63.48035201082149825, 5.440088680355550821 ) ) ;
#57910 = EDGE_CURVE ( 'NONE', #89108, #39417, #249, .T. ) ;
#57911 = CARTESIAN_POINT ( 'NONE',  ( 12.63842701281683034, 22.46726448433411605, 9.846743663894596210 ) ) ;
#57912 = CARTESIAN_POINT ( 'NONE',  ( 22.81628187352648496, 46.83196800326376064, -3.434112377981050290 ) ) ;
#57913 = STYLED_ITEM ( 'NONE', ( #92657 ), #24988 ) ;
#57914 = CARTESIAN_POINT ( 'NONE',  ( 5.076628168052703671, 1.842264484334118047, 8.527530157486179263 ) ) ;
#57915 = EDGE_LOOP ( 'NONE', ( #1674, #21288, #51453, #19795 ) ) ;
#57916 = DIRECTION ( 'NONE',  ( 0.000000000000000000, 1.000000000000000000, -0.000000000000000000 ) ) ;
#57917 = CARTESIAN_POINT ( 'NONE',  ( -14.88232117145532385, 0.5000000000000004441, 1.875237731503040628 ) ) ;
#57918 = CARTESIAN_POINT ( 'NONE',  ( 12.91533473730992121, 19.52201867748816611, 10.88017736071110164 ) ) ;
#57920 = CARTESIAN_POINT ( 'NONE',  ( 22.26659068614895176, 24.72041550158063572, -7.082119434687042414 ) ) ;
#57919 = CARTESIAN_POINT ( 'NONE',  ( -2.816281873526473856, 59.33196800326374643, 3.434112377981055619 ) ) ;
#57921 = CARTESIAN_POINT ( 'NONE',  ( 5.076628168052704559, 25.17559781766745175, -8.527530157486179263 ) ) ;
#57922 = CARTESIAN_POINT ( 'NONE',  ( 7.084665262690076126, 24.10535201082150181, 10.88017736071109987 ) ) ;
#57923 = CARTESIAN_POINT ( 'NONE',  ( -0.8801773607111008646, 8.272018677488171434, 2.915334737309923430 ) ) ;
#57924 = ORIENTED_EDGE ( 'NONE', *, *, #84904, .F. ) ;
#57925 = AXIS2_PLACEMENT_3D ( 'NONE', #33767, #26779, #10317 ) ;
#57926 = CARTESIAN_POINT ( 'NONE',  ( 20.88017736071110875, 10.77201867748817143, -2.915334737309920765 ) ) ;
#57927 = CARTESIAN_POINT ( 'NONE',  ( -0.8801773607111008646, 38.27201867748816255, 2.915334737309923430 ) ) ;
#57929 = CARTESIAN_POINT ( 'NONE',  ( 17.96484262340118221, 31.18868534415483751, -7.964842623401177768 ) ) ;
#57928 = CARTESIAN_POINT ( 'NONE',  ( -5.148594389986093312, 15.00000000000000711, -13.69051944078651317 ) ) ;
#57930 = ORIENTED_EDGE ( 'NONE', *, *, #71994, .T. ) ;
#57931 = CARTESIAN_POINT ( 'NONE',  ( 19.84674366389459266, 63.30059781766745886, 2.638427012816836559 ) ) ;
#57932 = CARTESIAN_POINT ( 'NONE',  ( -0.8801773607111009756, 28.06368534415484106, 1.068504757029289695E-15 ) ) ;
#57933 = CARTESIAN_POINT ( 'NONE',  ( 4.471658927061713307, -3.629165645961075715, 3.750000000000000000 ) ) ;
#57934 = CARTESIAN_POINT ( 'NONE',  ( 12.50534872682727716, 15.00000000000000000, 7.339363270777608861 ) ) ;
#57935 = CARTESIAN_POINT ( 'NONE',  ( 6.565887622018943937, 65.16530133659709634, 12.81628187352647430 ) ) ;
#57936 = CARTESIAN_POINT ( 'NONE',  ( -0.2418659066527783508, 4.260286857231743163, -6.114288769123032985 ) ) ;
#57937 = CARTESIAN_POINT ( 'NONE',  ( 20.36894250292379738, 29.92874883491396432, -10.36894250292379027 ) ) ;
#57938 = CARTESIAN_POINT ( 'NONE',  ( 17.96484262340118221, 46.18868534415484106, -7.964842623401177768 ) ) ;
#57939 = CARTESIAN_POINT ( 'NONE',  ( 17.96484262340118221, 29.93868534415484106, 7.964842623401181321 ) ) ;
#57940 = CARTESIAN_POINT ( 'NONE',  ( 18.52753015748618282, 63.92559781766745886, -4.923371831947291888 ) ) ;
#57941 = LINE ( 'NONE', #65938, #41320 ) ;
#57942 = CARTESIAN_POINT ( 'NONE',  ( 1.472469842513823179, 50.59226448433411605, -4.923371831947296329 ) ) ;
#57943 = EDGE_CURVE ( 'NONE', #25434, #85493, #94617, .T. ) ;
#57944 = CARTESIAN_POINT ( 'NONE',  ( 19.72487221294570858, 0.000000000000000000, -6.500000000000000888 ) ) ;
#57945 = CARTESIAN_POINT ( 'NONE',  ( 2.791683348922237240, 25.38393115100078390, -7.208316651077763204 ) ) ;
#57946 = CARTESIAN_POINT ( 'NONE',  ( -3.434112377981047626, -29.83469866340290721, 12.81628187352647963 ) ) ;
#57947 = CARTESIAN_POINT ( 'NONE',  ( 10.00000000000000000, 16.81368534415483751, -10.88017736071110342 ) ) ;
#57948 = CARTESIAN_POINT ( 'NONE',  ( 17.20831665107776587, 24.13393115100078035, -7.208316651077762316 ) ) ;
#57949 = CARTESIAN_POINT ( 'NONE',  ( 6.565887622018943937, 8.081968003263751754, -12.81628187352647608 ) ) ;
#57950 = CARTESIAN_POINT ( 'NONE',  ( 20.88017736071110875, 55.77201867748816966, -2.915334737309920765 ) ) ;
#57952 = CARTESIAN_POINT ( 'NONE',  ( -2.816281873526471635, 63.91530133659708923, -3.434112377981056508 ) ) ;
#57951 = CARTESIAN_POINT ( 'NONE',  ( 17.96484262340118221, 24.93868534415484461, 7.964842623401181321 ) ) ;
#57953 = CARTESIAN_POINT ( 'NONE',  ( 24.16423886937410614, 34.30374883491396787, 8.672049930838204340E-16 ) ) ;
#57954 = CIRCLE ( 'NONE', #29266, 15.00000000000000000 ) ;
#57955 = EDGE_CURVE ( 'NONE', #34693, #16030, #31193, .T. ) ;
#57956 = AXIS2_PLACEMENT_3D ( 'NONE', #83312, #31279, #46781 ) ;
#57957 = LINE ( 'NONE', #44924, #69047 ) ;
#57958 = ORIENTED_EDGE ( 'NONE', *, *, #83876, .F. ) ;
#57959 = CARTESIAN_POINT ( 'NONE',  ( -1.099225684535947600, -1.293031996736246469, -6.408140936763238038 ) ) ;
#57960 = LINE ( 'NONE', #87483, #58515 ) ;
#57961 = CARTESIAN_POINT ( 'NONE',  ( 19.42250999205614193, 30.14701867748817321, 5.440088680355555262 ) ) ;
#57962 = CARTESIAN_POINT ( 'NONE',  ( 17.20831665107776587, 59.13393115100078745, -7.208316651077762316 ) ) ;
#57963 = ORIENTED_EDGE ( 'NONE', *, *, #73178, .F. ) ;
#57964 = CARTESIAN_POINT ( 'NONE',  ( 14.92337183194729633, 12.67559781766745353, 8.527530157486181039 ) ) ;
#57965 = CARTESIAN_POINT ( 'NONE',  ( 12.63842701281683922, 14.55059781766744997, -9.846743663894590881 ) ) ;
#57966 = CARTESIAN_POINT ( 'NONE',  ( 1.472469842513823179, 16.42559781766745175, 4.923371831947296329 ) ) ;
#57967 = CARTESIAN_POINT ( 'NONE',  ( 0.1532563361054083140, 6.008931151000784787, 1.131784320476157264E-15 ) ) ;
#57968 = CARTESIAN_POINT ( 'NONE',  ( -4.181050312905175481, -2.964615315390050201E-16, 14.01631781289601442 ) ) ;
#57969 = CARTESIAN_POINT ( 'NONE',  ( -3.377759596007864129, -3.629459927034941025, 2.500000000000000888 ) ) ;
#57971 = CARTESIAN_POINT ( 'NONE',  ( 66.76470751278411342, 44.49999999999998579, 9.500000000000000000 ) ) ;
#57970 = CARTESIAN_POINT ( 'NONE',  ( 10.00000000000000000, 4.758931151000784787, -9.846743663894594434 ) ) ;
#57972 = CARTESIAN_POINT ( 'NONE',  ( 2.791683348922240793, 1.633931151000784565, 7.208316651077764092 ) ) ;
#57974 = ORIENTED_EDGE ( 'NONE', *, *, #29023, .T. ) ;
#57973 = CARTESIAN_POINT ( 'NONE',  ( 12.63842701281683922, 14.55059781766744997, -9.846743663894590881 ) ) ;
#57975 = CARTESIAN_POINT ( 'NONE',  ( 5.930053198192435815, -28.64714083316723503, 4.000000000000000000 ) ) ;
#57976 = CARTESIAN_POINT ( 'NONE',  ( 19.84674366389459266, 63.71726448433412315, -2.638427012816827677 ) ) ;
#57977 = ORIENTED_EDGE ( 'NONE', *, *, #53534, .F. ) ;
#57978 = ORIENTED_EDGE ( 'NONE', *, *, #57997, .T. ) ;
#57979 = CARTESIAN_POINT ( 'NONE',  ( 6.204703633549690345, 25.76208216824730712, -14.16423886937410259 ) ) ;
#57980 = DIRECTION ( 'NONE',  ( 0.9981347984218670311, 0.000000000000000000, -0.06104853953485662316 ) ) ;
#57981 = VECTOR ( 'NONE', #74620, 1000.000000000000000 ) ;
#57982 = CARTESIAN_POINT ( 'NONE',  ( 2.917880565312950480, 20.97041550158063217, -12.26659068614894821 ) ) ;
#57983 = CARTESIAN_POINT ( 'NONE',  ( -0.3689425029237898834, 36.17874883491396787, -10.36894250292378850 ) ) ;
#57984 = EDGE_CURVE ( 'NONE', #56421, #75686, #15240, .T. ) ;
#57985 = DIRECTION ( 'NONE',  ( 1.000000000000000000, 0.000000000000000000, 0.000000000000000000 ) ) ;
#57986 = CARTESIAN_POINT ( 'NONE',  ( 13.79529636645030344, 18.26208216824730002, 14.16423886937410614 ) ) ;
#57987 = CARTESIAN_POINT ( 'NONE',  ( 17.96484262340118221, 34.93868534415482685, 7.964842623401181321 ) ) ;
#57988 = CARTESIAN_POINT ( 'NONE',  ( 6.878063601867475008, -66.29791949882819324, -2.750000000000000000 ) ) ;
#57990 = VECTOR ( 'NONE', #61790, 1000.000000000000114 ) ;
#57989 = CARTESIAN_POINT ( 'NONE',  ( 7.361572987183169658, 9.967264484334119601, -9.846743663894592657 ) ) ;
#57992 = CARTESIAN_POINT ( 'NONE',  ( 18.52753015748618282, 33.92559781766745886, -4.923371831947291888 ) ) ;
#57991 = CARTESIAN_POINT ( 'NONE',  ( 4.559911319644449179, 58.89701867748817676, 9.422509992056141925 ) ) ;
#57993 = ORIENTED_EDGE ( 'NONE', *, *, #78931, .T. ) ;
#57994 = CARTESIAN_POINT ( 'NONE',  ( 15.44008868035555793, 16.39701867748817321, -9.422509992056140149 ) ) ;
#57995 = CARTESIAN_POINT ( 'NONE',  ( 6.565887622018943937, 43.08196800326374643, -12.81628187352647608 ) ) ;
#57996 = CARTESIAN_POINT ( 'NONE',  ( 18.52753015748618282, 53.92559781766745175, -4.923371831947291888 ) ) ;
#57997 = EDGE_CURVE ( 'NONE', #81607, #9509, #37249, .T. ) ;
#57998 = CARTESIAN_POINT ( 'NONE',  ( 19.38216949554541557, 32.24863466993041783, -9.382169495545420901 ) ) ;
#57999 = CARTESIAN_POINT ( 'NONE',  ( -5.204170427930421283E-15, -29.44625116508602858, -14.16423886937410082 ) ) ;
#58000 = CARTESIAN_POINT ( 'NONE',  ( 2.791683348922237240, 40.38393115100078035, -7.208316651077763204 ) ) ;
#58001 = CARTESIAN_POINT ( 'NONE',  ( -2.266590686148945544, 22.22041550158063572, 7.082119434687048631 ) ) ;
#58002 = ORIENTED_EDGE ( 'NONE', *, *, #98245, .F. ) ;
#58003 = CARTESIAN_POINT ( 'NONE',  ( 19.42250999205614193, 55.14701867748817676, 5.440088680355555262 ) ) ;
#58004 = CARTESIAN_POINT ( 'NONE',  ( 7.084665262690076126, 49.10535201082149825, 10.88017736071109987 ) ) ;
#58005 = CARTESIAN_POINT ( 'NONE',  ( 2.917880565312950480, 50.97041550158064638, -12.26659068614894821 ) ) ;
#58006 = CARTESIAN_POINT ( 'NONE',  ( 12.63842701281683034, 57.46726448433411605, 9.846743663894596210 ) ) ;
#58007 = CARTESIAN_POINT ( 'NONE',  ( 14.09394518620607428, 15.00000000000000000, 3.407449058785458451 ) ) ;
#58008 = CARTESIAN_POINT ( 'NONE',  ( 20.88017736071110164, 35.35535201082150536, 2.915334737309930979 ) ) ;
#58009 = CARTESIAN_POINT ( 'NONE',  ( -6.761335002693183327, 0.2301500669213601691, 13.32315948060032973 ) ) ;
#58010 = CARTESIAN_POINT ( 'NONE',  ( 17.20831665107776587, 59.13393115100078745, -7.208316651077762316 ) ) ;
#58011 = CARTESIAN_POINT ( 'NONE',  ( -2.915334737309917656, 9.105352010821512465, 10.88017736071110164 ) ) ;
#58012 = CARTESIAN_POINT ( 'NONE',  ( 12.91533473730993009, 6.605352010821504471, -10.88017736071109987 ) ) ;
#58013 = CARTESIAN_POINT ( 'NONE',  ( 17.96484262340118221, 66.18868534415483396, -7.964842623401177768 ) ) ;
#58014 = ORIENTED_EDGE ( 'NONE', *, *, #35702, .F. ) ;
#58015 = AXIS2_PLACEMENT_3D ( 'NONE', #39716, #25213, #94665 ) ;
#58016 = CARTESIAN_POINT ( 'NONE',  ( 17.96484262340118221, 9.938685344154837509, 7.964842623401181321 ) ) ;
#58017 = CARTESIAN_POINT ( 'NONE',  ( 14.99999999999998046, 79.82179676972448590, 6.500000000000000888 ) ) ;
#58018 = CARTESIAN_POINT ( 'NONE',  ( 7.084665262690076126, 62.02201867748816966, -10.88017736071110164 ) ) ;
#58020 = CARTESIAN_POINT ( 'NONE',  ( 17.96484262340118221, 66.18868534415483396, -7.964842623401177768 ) ) ;
#58019 = AXIS2_PLACEMENT_3D ( 'NONE', #5491, #6453, #81954 ) ;
#58021 = CARTESIAN_POINT ( 'NONE',  ( 17.90558034491733963, 78.11737700066652224, -4.059948642090408732 ) ) ;
#58022 = EDGE_CURVE ( 'NONE', #89795, #9875, #80267, .T. ) ;
#58023 = CARTESIAN_POINT ( 'NONE',  ( 14.92337183194729988, 34.34226448433411605, -8.527530157486177487 ) ) ;
#58024 = CARTESIAN_POINT ( 'NONE',  ( 4.559911319644449179, 27.23035201082150536, -9.422509992056141925 ) ) ;
#58025 = EDGE_CURVE ( 'NONE', #19716, #70499, #67738, .T. ) ;
#58026 = CARTESIAN_POINT ( 'NONE',  ( 21.09922568453595559, 2.040301336597086568, -6.408140936763230044 ) ) ;
#58028 = CARTESIAN_POINT ( 'NONE',  ( 3.969999999999999751, 10.00000000000000000, 2.750000000000000000 ) ) ;
#58027 = CARTESIAN_POINT ( 'NONE',  ( 7.084665262690076126, 29.10535201082150181, 10.88017736071109987 ) ) ;
#58029 = PRESENTATION_STYLE_ASSIGNMENT (( #4565 ) ) ;
#58030 = CARTESIAN_POINT ( 'NONE',  ( 19.38216949554541202, 40.99863466993042493, 9.382169495545424454 ) ) ;
#58031 = ORIENTED_EDGE ( 'NONE', *, *, #11000, .T. ) ;
#58032 = CARTESIAN_POINT ( 'NONE',  ( 10.00000000000000178, 70.00000000000000000, 0.000000000000000000 ) ) ;
#58034 = CARTESIAN_POINT ( 'NONE',  ( -13.21236992757665973, 0.000000000000000000, -5.338143956176898186 ) ) ;
#58033 = CARTESIAN_POINT ( 'NONE',  ( -2.816281873526471635, 13.91530133659708746, -3.434112377981056508 ) ) ;
#58035 = LINE ( 'NONE', #36542, #16424 ) ;
#58036 = CARTESIAN_POINT ( 'NONE',  ( 12.91533473730993009, 21.60535201082150536, -10.88017736071109987 ) ) ;
#58037 = CARTESIAN_POINT ( 'NONE',  ( 6.204703633549690345, 62.84541550158063927, 14.16423886937410082 ) ) ;
#58038 = CARTESIAN_POINT ( 'NONE',  ( 0.1532563361054082862, 56.21726448433411605, 2.638427012816831674 ) ) ;
#58039 = CARTESIAN_POINT ( 'NONE',  ( 2.791683348922237240, 5.383931151000785675, -7.208316651077763204 ) ) ;
#58040 = CARTESIAN_POINT ( 'NONE',  ( 17.96484262340118221, 66.18868534415483396, -7.964842623401177768 ) ) ;
#58041 = CARTESIAN_POINT ( 'NONE',  ( -12.00809552683965187, 15.00000000000000000, 8.989195838243462688 ) ) ;
#58042 = CARTESIAN_POINT ( 'NONE',  ( 6.204703633549690345, 30.76208216824730357, -14.16423886937410259 ) ) ;
#58043 = CARTESIAN_POINT ( 'NONE',  ( 12.34086200392826882, 15.00000000000000000, -7.124999999999971578 ) ) ;
#58044 = CARTESIAN_POINT ( 'NONE',  ( -3.772435416985459256, -6.430908609848360769, -4.000000000000000000 ) ) ;
#58045 = ORIENTED_EDGE ( 'NONE', *, *, #69562, .F. ) ;
#58046 = EDGE_LOOP ( 'NONE', ( #26240, #56385, #62973, #69389, #12921, #94720 ) ) ;
#58047 = CARTESIAN_POINT ( 'NONE',  ( 6.204703633549690345, 67.84541550158060375, 14.16423886937410082 ) ) ;
#58048 = CARTESIAN_POINT ( 'NONE',  ( 20.36894250292379382, 43.67874883491397497, 10.36894250292379205 ) ) ;
#58049 = CARTESIAN_POINT ( 'NONE',  ( 2.791683348922240793, 31.63393115100078745, 7.208316651077764092 ) ) ;
#58050 = DIRECTION ( 'NONE',  ( 1.000000000000000000, -1.355252715606880851E-17, 0.000000000000000000 ) ) ;
#58052 = PRESENTATION_STYLE_ASSIGNMENT (( #20063 ) ) ;
#58051 = CIRCLE ( 'NONE', #97989, 0.2500000000000002220 ) ;
#58053 = PRESENTATION_STYLE_ASSIGNMENT (( #12565 ) ) ;
#58054 = CARTESIAN_POINT ( 'NONE',  ( 13.79529636645031943, 40.34541550158063217, -14.16423886937409904 ) ) ;
#58055 = CARTESIAN_POINT ( 'NONE',  ( 6.879999999999995453, 43.00000000000000000, -4.250000000000000000 ) ) ;
#58056 = CARTESIAN_POINT ( 'NONE',  ( 19.84674366389459621, 3.508931151000785231, 7.409399052514197653E-17 ) ) ;
#58057 = B_SPLINE_CURVE_WITH_KNOTS ( 'NONE', 3,
 ( #64647, #65147, #95667, #27152, #57161, #57654 ),
 .UNSPECIFIED., .F., .F.,
 ( 4, 2, 4 ),
 ( 3.409110551333730758E-05, 0.0004400426677351795672, 0.0008459942299570218267 ),
 .UNSPECIFIED. ) ;
#58058 = EDGE_CURVE ( 'NONE', #77859, #587, #2861, .T. ) ;
#58059 = B_SPLINE_CURVE_WITH_KNOTS ( 'NONE', 3,
 ( #56787, #47807, #56311, #94786, #78308, #49773 ),
 .UNSPECIFIED., .F., .F.,
 ( 4, 2, 4 ),
 ( 3.409110551494646011E-05, 0.0004400426677367911795, 0.0008459942299586358785 ),
 .UNSPECIFIED. ) ;
#58060 = CYLINDRICAL_SURFACE ( 'NONE', #3525, 15.00000000000000000 ) ;
#58061 = CARTESIAN_POINT ( 'NONE',  ( -9.846743663894590881, 6.217264484334116936, 2.638427012816840111 ) ) ;
#58062 = ORIENTED_EDGE ( 'NONE', *, *, #43226, .F. ) ;
#58063 = EDGE_LOOP ( 'NONE', ( #39134, #70918, #58958, #40637 ) ) ;
#58064 = SURFACE_STYLE_FILL_AREA ( #57088 ) ;
#58065 = EDGE_LOOP ( 'NONE', ( #92486, #35786 ) ) ;
#58066 = CARTESIAN_POINT ( 'NONE',  ( 13.79529636645031943, 10.34541550158063394, -14.16423886937409904 ) ) ;
#58068 = CARTESIAN_POINT ( 'NONE',  ( 10.00000000000000000, 21.81368534415484106, -10.88017736071110342 ) ) ;
#58067 = CARTESIAN_POINT ( 'NONE',  ( 12.91533473730993009, 21.60535201082150536, -10.88017736071109987 ) ) ;
#58070 = CARTESIAN_POINT ( 'NONE',  ( -2.816281873526473856, 14.12363466993041961, 9.499525473075851096E-16 ) ) ;
#58069 = CARTESIAN_POINT ( 'NONE',  ( 17.20831665107776587, 52.88393115100078035, 7.208316651077764980 ) ) ;
#58071 = PRESENTATION_STYLE_ASSIGNMENT (( #96094 ) ) ;
#58072 = CARTESIAN_POINT ( 'NONE',  ( 19.38216949554541557, 12.24863466993041961, -9.382169495545420901 ) ) ;
#58073 = ORIENTED_EDGE ( 'NONE', *, *, #84035, .T. ) ;
#58074 = CARTESIAN_POINT ( 'NONE',  ( 7.361572987183170547, 37.05059781766744464, 9.846743663894590881 ) ) ;
#58075 = CARTESIAN_POINT ( 'NONE',  ( 6.204703633549690345, 57.84541550158063927, 14.16423886937410082 ) ) ;
#58076 = ORIENTED_EDGE ( 'NONE', *, *, #21238, .F. ) ;
#58077 = CARTESIAN_POINT ( 'NONE',  ( 2.035157376598822676, 2.438685344154838397, -7.964842623401177768 ) ) ;
#58078 = ORIENTED_EDGE ( 'NONE', *, *, #4848, .T. ) ;
#58079 = CARTESIAN_POINT ( 'NONE',  ( 2.035157376598822676, 52.43868534415483396, -7.964842623401177768 ) ) ;
#58080 = CARTESIAN_POINT ( 'NONE',  ( 4.559911319644449179, 38.89701867748817676, 9.422509992056141925 ) ) ;
#58081 = CARTESIAN_POINT ( 'NONE',  ( -0.8801773607110991993, 47.85535201082150536, -2.915334737309923874 ) ) ;
#58082 = CARTESIAN_POINT ( 'NONE',  ( 20.10421743870886147, 5.607361737662019507, -6.337391062633416006 ) ) ;
#58083 = CARTESIAN_POINT ( 'NONE',  ( 17.96484262340118221, 34.93868534415482685, 7.964842623401181321 ) ) ;
#58084 = CARTESIAN_POINT ( 'NONE',  ( -0.1503990784575279516, 53.10158574516643171, 6.262539305110076171 ) ) ;
#58086 = ORIENTED_EDGE ( 'NONE', *, *, #61373, .F. ) ;
#58085 = FILL_AREA_STYLE_COLOUR ( '', #84049 ) ;
#58087 = CARTESIAN_POINT ( 'NONE',  ( 2.791683348922237240, 30.38393115100078390, -7.208316651077763204 ) ) ;
#58088 = VERTEX_POINT ( 'NONE', #83719 ) ;
#58089 = CARTESIAN_POINT ( 'NONE',  ( 19.84674366389459266, 63.30059781766745886, 2.638427012816836559 ) ) ;
#58090 = CARTESIAN_POINT ( 'NONE',  ( 6.599999999999995204, -97.00000000000000000, 3.750000000000000000 ) ) ;
#58091 = CARTESIAN_POINT ( 'NONE',  ( -3.990799379706100325, -9.967613007074422882, 2.750000000000000000 ) ) ;
#58092 = ORIENTED_EDGE ( 'NONE', *, *, #34526, .F. ) ;
#58093 = CARTESIAN_POINT ( 'NONE',  ( -3.750000000000000888, 1.019547802438465212, 3.750000000000000000 ) ) ;
#58094 = CARTESIAN_POINT ( 'NONE',  ( 5.076628168052704559, 65.17559781766745175, -8.527530157486179263 ) ) ;
#58095 = CARTESIAN_POINT ( 'NONE',  ( 24.16423886937410614, 54.51208216824730357, -3.795296366450302550 ) ) ;
#58096 = CARTESIAN_POINT ( 'NONE',  ( 18.28836319691949797, 64.34492782695771496, 6.499999999999917399 ) ) ;
#58097 = CYLINDRICAL_SURFACE ( 'NONE', #60750, 15.00000000000000000 ) ;
#58098 = CARTESIAN_POINT ( 'NONE',  ( 1.472469842513823179, 36.42559781766745175, 4.923371831947296329 ) ) ;
#58099 = SURFACE_STYLE_FILL_AREA ( #57617 ) ;
#58100 = CARTESIAN_POINT ( 'NONE',  ( -2.816281873526473856, 4.123634669930420493, 9.499525473075851096E-16 ) ) ;
#58101 = CARTESIAN_POINT ( 'NONE',  ( 2.791683348922240793, 6.633931151000785675, 7.208316651077764092 ) ) ;
#58102 = EDGE_CURVE ( 'NONE', #40543, #26337, #58704, .T. ) ;
#58103 = CARTESIAN_POINT ( 'NONE',  ( -0.1503990784575323369, 4.248846992468888750, -6.262539305110070842 ) ) ;
#58104 = CARTESIAN_POINT ( 'NONE',  ( 10.00000000000000000, 4.758931151000784787, -9.846743663894594434 ) ) ;
#58105 = CARTESIAN_POINT ( 'NONE',  ( 19.84674366389459621, 58.50893115100078745, 7.409399052514197653E-17 ) ) ;
#58106 = CARTESIAN_POINT ( 'NONE',  ( 18.72515096720568195, 21.07228050351032422, -6.500000000000018652 ) ) ;
#58107 = ORIENTED_EDGE ( 'NONE', *, *, #48492, .T. ) ;
#58108 = CARTESIAN_POINT ( 'NONE',  ( 2.035157376598824452, 8.688685344154839285, 7.964842623401179544 ) ) ;
#58109 = CARTESIAN_POINT ( 'NONE',  ( -0.3689425029237898834, 1.178748834913967869, -10.36894250292378850 ) ) ;
#58110 = CARTESIAN_POINT ( 'NONE',  ( 14.92337183194729988, 9.342264484334119601, -8.527530157486177487 ) ) ;
#58111 = CARTESIAN_POINT ( 'NONE',  ( 20.88017736071110519, 50.56368534415484106, 2.639326808657452039E-16 ) ) ;
#58113 = FACE_OUTER_BOUND ( 'NONE', #9186, .T. ) ;
#58112 = CARTESIAN_POINT ( 'NONE',  ( 10.00000000000000178, 25.37363466993041783, 12.81628187352647608 ) ) ;
#58114 = CARTESIAN_POINT ( 'NONE',  ( 7.084665262690076126, 4.105352010821503583, 10.88017736071109987 ) ) ;
#58115 = PRESENTATION_LAYER_ASSIGNMENT (  '', '', ( #32584 ) ) ;
#58116 = CARTESIAN_POINT ( 'NONE',  ( 0.000000000000000000, 15.00000000000000000, 0.000000000000000000 ) ) ;
#58117 = CARTESIAN_POINT ( 'NONE',  ( 19.38216949554541202, 5.998634669930420493, 9.382169495545424454 ) ) ;
#58118 = CARTESIAN_POINT ( 'NONE',  ( 0.1532563361054083140, 61.00893115100078745, 1.131784320476157264E-15 ) ) ;
#58119 = CARTESIAN_POINT ( 'NONE',  ( 5.076628168052703671, 16.84226448433411960, 8.527530157486179263 ) ) ;
#58120 = CARTESIAN_POINT ( 'NONE',  ( -9.422509992056136596, -26.51964798917849109, 5.440088680355559703 ) ) ;
#58121 = CARTESIAN_POINT ( 'NONE',  ( 22.81628187352647785, 16.62363466993042138, 6.195893100308588602E-16 ) ) ;
#58122 = CARTESIAN_POINT ( 'NONE',  ( -11.26382985233585643, -93.42670896123698299, -3.750000000000000000 ) ) ;
#58123 = CARTESIAN_POINT ( 'NONE',  ( 20.88017736071110164, 25.35535201082150891, 2.915334737309930979 ) ) ;
#58124 = DIRECTION ( 'NONE',  ( -0.000000000000000000, -1.000000000000000000, -0.000000000000000000 ) ) ;
#58125 = CARTESIAN_POINT ( 'NONE',  ( 17.08211943468705130, 48.47041550158063927, 12.26659068614894998 ) ) ;
#58126 = CARTESIAN_POINT ( 'NONE',  ( 1.881645754503766366, 15.00000000000000533, 14.50406564081098182 ) ) ;
#58127 = CARTESIAN_POINT ( 'NONE',  ( 4.559911319644449179, 33.89701867748817676, 9.422509992056141925 ) ) ;
#58128 = B_SPLINE_CURVE_WITH_KNOTS ( 'NONE', 3,
 ( #2645, #80578, #65553, #33099, #42579, #35055 ),
 .UNSPECIFIED., .F., .F.,
 ( 4, 2, 4 ),
 ( 0.0002800170536516742212, 0.0006862224498868413260, 0.001092427846122008593 ),
 .UNSPECIFIED. ) ;
#58129 = CARTESIAN_POINT ( 'NONE',  ( 14.92337183194729633, 47.67559781766745175, 8.527530157486181039 ) ) ;
#58130 = EDGE_CURVE ( 'NONE', #2137, #14813, #62673, .T. ) ;
#58131 = CARTESIAN_POINT ( 'NONE',  ( 10.00000000000000178, 49.31368534415484106, 10.88017736071110342 ) ) ;
#58132 = CARTESIAN_POINT ( 'NONE',  ( 22.26659068614894466, 28.88708216824730357, 7.082119434687054849 ) ) ;
#58133 = CARTESIAN_POINT ( 'NONE',  ( -8.209432707284749497, 14.49999999999999112, -12.55409154915501269 ) ) ;
#58134 = UNCERTAINTY_MEASURE_WITH_UNIT (LENGTH_MEASURE( 1.000000000000000082E-05 ), #61346, 'distance_accuracy_value', 'NONE');
#58135 = EDGE_CURVE ( 'NONE', #28589, #56516, #87478, .T. ) ;
#58136 = CARTESIAN_POINT ( 'NONE',  ( 12.63842701281683922, 34.55059781766745886, -9.846743663894590881 ) ) ;
#58137 = CARTESIAN_POINT ( 'NONE',  ( 10.00000000000000000, 62.87363466993042493, -12.81628187352647608 ) ) ;
#58138 = CARTESIAN_POINT ( 'NONE',  ( 18.52753015748618282, 63.92559781766745886, -4.923371831947291888 ) ) ;
#58139 = ORIENTED_EDGE ( 'NONE', *, *, #12731, .F. ) ;
#58140 = CARTESIAN_POINT ( 'NONE',  ( 20.88017736071110519, 25.56368534415483751, 2.639326808657452039E-16 ) ) ;
#58141 = CARTESIAN_POINT ( 'NONE',  ( 17.74999999999999645, 91.00000000000000000, -8.000000000000000000 ) ) ;
#58142 = CARTESIAN_POINT ( 'NONE',  ( 4.380000000000000782, -0.01592157648205478476, 2.750000000000000000 ) ) ;
#58143 = CARTESIAN_POINT ( 'NONE',  ( 15.44008868035555260, 9.730352010821505360, 9.422509992056143702 ) ) ;
#58144 = CARTESIAN_POINT ( 'NONE',  ( 10.00000000000000000, 66.81368534415484817, -10.88017736071110342 ) ) ;
#58145 = CARTESIAN_POINT ( 'NONE',  ( 20.36894250292379382, 28.67874883491396787, 10.36894250292379205 ) ) ;
#58146 = CARTESIAN_POINT ( 'NONE',  ( 14.92337183194729633, 7.675597817667451750, 8.527530157486181039 ) ) ;
#58147 = FACE_OUTER_BOUND ( 'NONE', #72758, .T. ) ;
#58148 = CARTESIAN_POINT ( 'NONE',  ( 15.44008868035555260, 29.73035201082150891, 9.422509992056143702 ) ) ;
#58149 = CARTESIAN_POINT ( 'NONE',  ( 19.39235739573468820, 64.87576471608601025, 6.499999999999992895 ) ) ;
#58150 = CARTESIAN_POINT ( 'NONE',  ( 4.879999999999994564, 43.00000000000000711, 4.250000000000000000 ) ) ;
#58151 = ORIENTED_EDGE ( 'NONE', *, *, #96432, .T. ) ;
#58152 = CARTESIAN_POINT ( 'NONE',  ( 7.993154516100952733, 14.95077488074853811, 12.39982181464619160 ) ) ;
#58153 = CARTESIAN_POINT ( 'NONE',  ( 17.20831665107776587, 39.13393115100079456, -7.208316651077762316 ) ) ;
#58154 = VERTEX_POINT ( 'NONE', #55170 ) ;
#58155 = ORIENTED_EDGE ( 'NONE', *, *, #56673, .T. ) ;
#58156 = DIRECTION ( 'NONE',  ( 0.000000000000000000, 0.000000000000000000, 1.000000000000000000 ) ) ;
#58157 = CARTESIAN_POINT ( 'NONE',  ( 22.26659068614894466, 3.887082168247300906, 7.082119434687054849 ) ) ;
#58158 = CARTESIAN_POINT ( 'NONE',  ( -2.266590686148945544, 11.38708216824730179, -7.082119434687050408 ) ) ;
#58159 = CARTESIAN_POINT ( 'NONE',  ( 15.44008868035555260, 44.73035201082151247, 9.422509992056143702 ) ) ;
#58160 = CARTESIAN_POINT ( 'NONE',  ( 17.08211943468705840, 50.13708216824730357, -12.26659068614894466 ) ) ;
#58161 = CARTESIAN_POINT ( 'NONE',  ( 21.09922568453594849, 6.206968003263753531, 6.408140936763242479 ) ) ;
#58162 = CARTESIAN_POINT ( 'NONE',  ( 0.1532563361054083140, 36.00893115100078745, 1.131784320476157264E-15 ) ) ;
#58163 = CARTESIAN_POINT ( 'NONE',  ( -10.82635109531846673, -96.00292546281325201, 4.000000000000000000 ) ) ;
#58165 = CARTESIAN_POINT ( 'NONE',  ( 22.81628187352647785, 11.62363466993042138, 6.195893100308588602E-16 ) ) ;
#58164 = CARTESIAN_POINT ( 'NONE',  ( 12.91533473730993009, 36.60535201082151247, -10.88017736071109987 ) ) ;
#58166 = CARTESIAN_POINT ( 'NONE',  ( 6.204703633549690345, 2.845415501580634388, 14.16423886937410082 ) ) ;
#58167 = CARTESIAN_POINT ( 'NONE',  ( 2.917880565312950480, 55.97041550158063217, -12.26659068614894821 ) ) ;
#58168 = CARTESIAN_POINT ( 'NONE',  ( 4.559911319644449179, 22.23035201082150536, -9.422509992056141925 ) ) ;
#58169 = CARTESIAN_POINT ( 'NONE',  ( 18.52753015748618282, 38.92559781766745175, -4.923371831947291888 ) ) ;
#58170 = CARTESIAN_POINT ( 'NONE',  ( 12.34086200392821908, -0.03417435944610275333, 7.125000000000058620 ) ) ;
#58171 = CARTESIAN_POINT ( 'NONE',  ( 9.846743663894590881, -31.69940218233254825, 2.638427012816828565 ) ) ;
#58172 = ORIENTED_EDGE ( 'NONE', *, *, #40812, .T. ) ;
#58173 = CYLINDRICAL_SURFACE ( 'NONE', #44346, 15.00000000000000000 ) ;
#58174 = ORIENTED_EDGE ( 'NONE', *, *, #44993, .F. ) ;
#58175 = ORIENTED_EDGE ( 'NONE', *, *, #70147, .T. ) ;
#58176 = CARTESIAN_POINT ( 'NONE',  ( -2.266590686148945544, 46.38708216824730357, -7.082119434687050408 ) ) ;
#58177 = CARTESIAN_POINT ( 'NONE',  ( 2.791683348922240793, 51.63393115100078745, 7.208316651077764092 ) ) ;
#58178 = CARTESIAN_POINT ( 'NONE',  ( 17.96484262340118221, 61.18868534415482685, -7.964842623401177768 ) ) ;
#58179 = EDGE_CURVE ( 'NONE', #91322, #83574, #48141, .T. ) ;
#58180 = DIRECTION ( 'NONE',  ( 3.907985046680551022E-14, 0.000000000000000000, 1.000000000000000000 ) ) ;
#58181 = CARTESIAN_POINT ( 'NONE',  ( 0.5774900079438590739, 57.64701867748817676, -5.440088680355550821 ) ) ;
#58182 = VECTOR ( 'NONE', #42987, 1000.000000000000227 ) ;
#58183 = CARTESIAN_POINT ( 'NONE',  ( -12.81628187352647608, 9.123634669930428487, 3.903127820947815962E-15 ) ) ;
#58184 = ORIENTED_EDGE ( 'NONE', *, *, #54750, .F. ) ;
#58185 = CARTESIAN_POINT ( 'NONE',  ( 22.26659068614895176, 14.72041550158063572, -7.082119434687042414 ) ) ;
#58186 = COLOUR_RGB ( '', 0.31764706, 0.68627451, 0.89019608) ;
#58187 = CARTESIAN_POINT ( 'NONE',  ( 13.43411237798105340, 30.58196800326374998, 12.81628187352647963 ) ) ;
#58188 = ORIENTED_EDGE ( 'NONE', *, *, #17199, .T. ) ;
#58189 = CARTESIAN_POINT ( 'NONE',  ( 21.09922568453594849, 51.20696800326375353, 6.408140936763242479 ) ) ;
#58190 = CARTESIAN_POINT ( 'NONE',  ( 2.791683348922237240, 40.38393115100078035, -7.208316651077763204 ) ) ;
#58191 = CARTESIAN_POINT ( 'NONE',  ( 20.88017736071110875, 10.77201867748817143, -2.915334737309920765 ) ) ;
#58192 = VECTOR ( 'NONE', #40300, 1000.000000000000000 ) ;
#58193 = CARTESIAN_POINT ( 'NONE',  ( 16.40814093676323893, 55.79030133659708923, 11.09922568453595026 ) ) ;
#58194 = CARTESIAN_POINT ( 'NONE',  ( -46.07360246527855452, 103.8701977390177120, -6.036219926076625164 ) ) ;
#58195 = CARTESIAN_POINT ( 'NONE',  ( 19.84674366389459266, 38.71726448433412315, -2.638427012816827677 ) ) ;
#58196 = CARTESIAN_POINT ( 'NONE',  ( 0.9082943533637206635, 15.00000000000000000, -14.47152380945584760 ) ) ;
#58197 = COLOUR_RGB ( '', 0.40784314, 0.44705882, 0.49803922) ;
#58198 = CARTESIAN_POINT ( 'NONE',  ( -45.94000000000000483, 93.00000000000000000, -8.999999999999998224 ) ) ;
#58199 = CARTESIAN_POINT ( 'NONE',  ( 1.780824192092498315, 14.63595249122789177, -14.89391369643514373 ) ) ;
#58200 = CARTESIAN_POINT ( 'NONE',  ( 0.1532563361054082862, 21.21726448433412315, 2.638427012816831674 ) ) ;
#58201 = CARTESIAN_POINT ( 'NONE',  ( 6.565887622018943937, 20.16530133659708213, 12.81628187352647430 ) ) ;
#58202 = EDGE_LOOP ( 'NONE', ( #12435, #94337, #35692, #29907, #66489, #79934 ) ) ;
#58203 = CARTESIAN_POINT ( 'NONE',  ( 10.00000000000000000, 59.75893115100078745, -9.846743663894594434 ) ) ;
#58204 = CARTESIAN_POINT ( 'NONE',  ( -14.99847009497945294, 0.3640475087720990155, 0.2142307401079311391 ) ) ;
#58205 = CARTESIAN_POINT ( 'NONE',  ( 6.204703633549690345, 22.84541550158062861, 14.16423886937410082 ) ) ;
#58206 = CARTESIAN_POINT ( 'NONE',  ( 2.791683348922240793, 31.63393115100078745, 7.208316651077764092 ) ) ;
#58207 = CARTESIAN_POINT ( 'NONE',  ( 16.40814093676323893, 40.79030133659708923, 11.09922568453595026 ) ) ;
#58209 = DIRECTION ( 'NONE',  ( -0.000000000000000000, 0.000000000000000000, 1.000000000000000000 ) ) ;
#58208 = CARTESIAN_POINT ( 'NONE',  ( -6.000000000000000000, 78.07179676972447169, 6.500000000000000888 ) ) ;
#58210 = CARTESIAN_POINT ( 'NONE',  ( 12.91533473730992121, 59.52201867748816966, 10.88017736071110164 ) ) ;
#58211 = CARTESIAN_POINT ( 'NONE',  ( -1.099225684535947600, 13.70696800326375353, -6.408140936763238038 ) ) ;
#58212 = DIRECTION ( 'NONE',  ( -1.000000000000000000, 0.000000000000000000, 0.000000000000000000 ) ) ;
#58213 = PRESENTATION_LAYER_ASSIGNMENT (  '', '', ( #75801 ) ) ;
#58214 = CARTESIAN_POINT ( 'NONE',  ( 0.1532563361054100626, 40.80059781766745886, -2.638427012816831230 ) ) ;
#58215 = CARTESIAN_POINT ( 'NONE',  ( 7.084665262690076126, 44.10535201082151247, 10.88017736071109987 ) ) ;
#58216 = EDGE_CURVE ( 'NONE', #66682, #12912, #48164, .T. ) ;
#58217 = CARTESIAN_POINT ( 'NONE',  ( 10.00000000000000000, 42.87363466993042493, -12.81628187352647608 ) ) ;
#58218 = CARTESIAN_POINT ( 'NONE',  ( 17.20831665107776587, 37.88393115100078745, 7.208316651077764980 ) ) ;
#58219 = CARTESIAN_POINT ( 'NONE',  ( -13.07907619356937268, 14.76984992095085758, 7.222187741820579099 ) ) ;
#58220 = CARTESIAN_POINT ( 'NONE',  ( 2.035157376598822676, 32.43868534415483396, -7.964842623401177768 ) ) ;
#58221 = CARTESIAN_POINT ( 'NONE',  ( 14.49440716394873618, 4.800686736885023475E-16, -0.4026921475166205244 ) ) ;
#58222 = CARTESIAN_POINT ( 'NONE',  ( 19.42250999205614193, 20.14701867748817321, 5.440088680355555262 ) ) ;
#58224 = CARTESIAN_POINT ( 'NONE',  ( 7.084665262690076126, 24.10535201082150181, 10.88017736071109987 ) ) ;
#58223 = CARTESIAN_POINT ( 'NONE',  ( 19.84674366389459621, 53.50893115100078745, 7.409399052514197653E-17 ) ) ;
#58225 = DIRECTION ( 'NONE',  ( 6.938893903907222067E-15, 0.000000000000000000, -1.000000000000000000 ) ) ;
#58226 = B_SPLINE_CURVE_WITH_KNOTS ( 'NONE', 3,
 ( #30940, #61438, #84455, #15954, #55925, #56418 ),
 .UNSPECIFIED., .F., .F.,
 ( 4, 2, 4 ),
 ( 7.805926233243723174E-18, 0.0002626113303185862824, 0.0005252226606371647585 ),
 .UNSPECIFIED. ) ;
#58227 = CARTESIAN_POINT ( 'NONE',  ( 12.91533473730992121, 59.52201867748816966, 10.88017736071110164 ) ) ;
#58229 = CARTESIAN_POINT ( 'NONE',  ( -2.168404344971008868E-15, 78.76925905125540339, -9.369910658262430303 ) ) ;
#58228 = CARTESIAN_POINT ( 'NONE',  ( 2.035157376598822676, 22.43868534415483396, -7.964842623401177768 ) ) ;
#58230 =( NAMED_UNIT ( * ) PLANE_ANGLE_UNIT ( ) SI_UNIT ( $, .RADIAN. ) );
#58231 = CARTESIAN_POINT ( 'NONE',  ( 7.361572987183169658, 29.96726448433411960, -9.846743663894592657 ) ) ;
#58232 = CARTESIAN_POINT ( 'NONE',  ( 70.68973184038034674, 41.77083333333331439, 9.500000000000000000 ) ) ;
#58233 = CARTESIAN_POINT ( 'NONE',  ( 7.082119434687054849, 3.470415501580635720, 12.26659068614894288 ) ) ;
#58234 = CARTESIAN_POINT ( 'NONE',  ( 1.472469842513823179, 50.59226448433411605, -4.923371831947296329 ) ) ;
#58236 = CARTESIAN_POINT ( 'NONE',  ( 4.471369574522381818, -3.620508344108031018, 3.750000000000000444 ) ) ;
#58235 = CARTESIAN_POINT ( 'NONE',  ( 17.08211943468705840, 50.13708216824730357, -12.26659068614894466 ) ) ;
#58237 = SURFACE_STYLE_FILL_AREA ( #4286 ) ;
#58238 = CARTESIAN_POINT ( 'NONE',  ( 13.79529636645031943, 5.345415501580634832, -14.16423886937409904 ) ) ;
#58239 = CARTESIAN_POINT ( 'NONE',  ( 6.204703633549690345, 35.76208216824729647, -14.16423886937410259 ) ) ;
#58240 = CARTESIAN_POINT ( 'NONE',  ( 6.565887622018943937, 5.165301336597086568, 12.81628187352647430 ) ) ;
#58241 = FACE_OUTER_BOUND ( 'NONE', #66154, .T. ) ;
#58242 = VERTEX_POINT ( 'NONE', #96528 ) ;
#58243 = EDGE_CURVE ( 'NONE', #86107, #13092, #71181, .T. ) ;
#58244 = PRESENTATION_LAYER_ASSIGNMENT (  '', '', ( #5542 ) ) ;
#58245 = CARTESIAN_POINT ( 'NONE',  ( -0.8801773607111009756, 13.06368534415483929, 1.068504757029289695E-15 ) ) ;
#58246 = CARTESIAN_POINT ( 'NONE',  ( 5.076628168052703671, 36.84226448433412315, 8.527530157486179263 ) ) ;
#58247 = CARTESIAN_POINT ( 'NONE',  ( -11.88867004768947488, 90.28252147127371074, -6.948627224671861669 ) ) ;
#58248 = CARTESIAN_POINT ( 'NONE',  ( 12.91533473730992121, 54.52201867748816255, 10.88017736071110164 ) ) ;
#58249 = DIRECTION ( 'NONE',  ( -2.569960705150826877E-16, 1.000000000000000000, 0.000000000000000000 ) ) ;
#58250 = CIRCLE ( 'NONE', #27936, 0.5000000000000004441 ) ;
#58251 = CARTESIAN_POINT ( 'NONE',  ( 10.00000000000000000, -0.2410688489992152128, -9.846743663894594434 ) ) ;
#58252 = CARTESIAN_POINT ( 'NONE',  ( 3.591859063236763294, 23.29030133659708568, -11.09922568453595026 ) ) ;
#58253 = CARTESIAN_POINT ( 'NONE',  ( 14.92337183194729988, 29.34226448433411960, -8.527530157486177487 ) ) ;
#58255 = EDGE_LOOP ( 'NONE', ( #69729, #18622, #61899, #77251, #31218, #87524, #22966, #23136, #78499, #30741, #75128, #38189, #34172, #30676, #88927, #65780, #46534, #34015, #67511, #50432, #93404, #25500, #28162, #45590, #54033, #35457, #95351, #31658, #96720, #88484, #84747, #83142, #68856, #63125, #91236, #28564, #95998, #51319, #4584, #28391, #79378, #89698, #5749, #15794, #19753, #95403, #88577, #27688, #11788, #17709, #25411, #21201, #33087, #44534, #89956, #12849, #59149, #33714, #29650, #38093, #49586, #70530, #22210, #68837, #77328, #71536, #57963, #79514, #44486, #20561, #82875, #82490, #23800, #33588, #8386, #18915, #89311, #5402, #22355, #31383, #89163, #26603, #63823, #18953, #90655, #22793, #48359, #55369, #81680, #67661, #8571, #42034, #33288, #3218, #35205, #84645, #42232, #57806, #37934, #82070, #27770, #49330, #18843, #47438, #73313, #12499, #6580, #76653, #17447, #50513, #43188, #27598, #38902, #91579, #28805, #21103, #30493, #47263, #34691, #91522, #5092, #87987, #61916, #78754, #25394, #19635, #51236, #98691, #53042, #38649, #39628, #1294, #9906, #18800, #8046, #1744, #67072, #37574, #65062, #58464, #82601, #45538, #56718, #55538, #15941, #46707, #10144, #34174, #14823, #69418, #30220, #37765, #30616, #20251, #22639, #70610, #88698, #46755, #11689, #33220, #89865, #75990, #72825, #5484, #95571, #9263, #44840, #98283, #72484, #33700, #61411, #57890, #40641, #47147, #55047, #61765, #27430, #16789, #21039, #29919, #59332, #69411, #56500, #58615, #21791, #73200, #96054, #5375, #90134, #94638, #57085, #7088, #80941, #23791, #3639, #15769, #94944, #60617, #12722, #67099, #67215, #36158, #75096, #12928, #28061, #9492, #16189, #20824, #52558, #74164, #83804, #33911, #66086, #68598, #97825, #53029, #48832, #23638, #38110, #18014, #42311, #54036, #572, #36951, #89689, #90517, #18895, #70773, #23037, #83195, #91492, #907, #49940, #68658, #36327, #74284, #6919, #9236, #92388, #7802, #86815, #95939, #43575, #1400, #73909, #13603, #50096, #22994, #78036, #25632, #28188, #87815, #4739, #71051, #40027, #21946, #25994, #60290, #43594, #52862, #17858, #44142, #44976, #32258, #27307, #56254, #68176, #68345, #19498, #32357 ) ) ;
#58254 = EDGE_CURVE ( 'NONE', #19349, #3216, #58499, .T. ) ;
#58256 = DIRECTION ( 'NONE',  ( 0.000000000000000000, 0.000000000000000000, 1.000000000000000000 ) ) ;
#58257 = LINE ( 'NONE', #35272, #38077 ) ;
#58258 = CARTESIAN_POINT ( 'NONE',  ( 24.16423886937410614, 64.51208216824728936, -3.795296366450302550 ) ) ;
#58259 = CARTESIAN_POINT ( 'NONE',  ( 15.44008868035555793, 11.39701867748817143, -9.422509992056140149 ) ) ;
#58260 = CARTESIAN_POINT ( 'NONE',  ( 10.00000000000000178, 43.05374883491397497, 14.16423886937410082 ) ) ;
#58261 = CARTESIAN_POINT ( 'NONE',  ( 4.559911319644449179, 37.23035201082150536, -9.422509992056141925 ) ) ;
#58262 = CARTESIAN_POINT ( 'NONE',  ( -0.8801773607111008646, 58.27201867748816966, 2.915334737309923430 ) ) ;
#58263 = CARTESIAN_POINT ( 'NONE',  ( -0.8217048220028323469, 14.95037104780827342, -14.73031263976448457 ) ) ;
#58264 = CARTESIAN_POINT ( 'NONE',  ( 21.92686044187657046, 40.16212336850779963, 4.562052436263912550E-16 ) ) ;
#58265 = CARTESIAN_POINT ( 'NONE',  ( 10.00000000000000178, 22.25893115100078745, 9.846743663894594434 ) ) ;
#58266 = DIRECTION ( 'NONE',  ( 1.000000000000000000, 0.000000000000000000, 0.000000000000000000 ) ) ;
#58267 = CARTESIAN_POINT ( 'NONE',  ( 18.52753015748618282, 8.925597817667451750, -4.923371831947291888 ) ) ;
#58268 = DIRECTION ( 'NONE',  ( 0.000000000000000000, 0.000000000000000000, 1.000000000000000000 ) ) ;
#58269 = CARTESIAN_POINT ( 'NONE',  ( 19.84674366389459621, 33.50893115100078745, 7.409399052514197653E-17 ) ) ;
#58270 = CARTESIAN_POINT ( 'NONE',  ( 5.076628168052703671, 56.84226448433412315, 8.527530157486179263 ) ) ;
#58271 = CARTESIAN_POINT ( 'NONE',  ( 20.88017736071110164, 30.35535201082151247, 2.915334737309930979 ) ) ;
#58272 = EDGE_LOOP ( 'NONE', ( #14322, #82505, #11572, #43612 ) ) ;
#58273 = CARTESIAN_POINT ( 'NONE',  ( 3.591859063236761518, 44.95696800326376064, 11.09922568453594849 ) ) ;
#58274 = CIRCLE ( 'NONE', #4063, 0.5000000000000073275 ) ;
#58275 = LINE ( 'NONE', #88793, #74772 ) ;
#58276 = CARTESIAN_POINT ( 'NONE',  ( 19.42250999205614548, 65.98035201082151957, -5.440088680355545492 ) ) ;
#58277 = CARTESIAN_POINT ( 'NONE',  ( 3.591859063236763294, 38.29030133659708923, -11.09922568453595026 ) ) ;
#58279 = CARTESIAN_POINT ( 'NONE',  ( 5.076628168052704559, 40.17559781766745175, -8.527530157486179263 ) ) ;
#58278 = CARTESIAN_POINT ( 'NONE',  ( 6.204703633549690345, 55.76208216824730357, -14.16423886937410259 ) ) ;
#58280 = DIRECTION ( 'NONE',  ( 0.000000000000000000, 0.000000000000000000, 1.000000000000000000 ) ) ;
#58281 = CARTESIAN_POINT ( 'NONE',  ( 17.20831665107776587, 59.13393115100078745, -7.208316651077762316 ) ) ;
#58282 = CARTESIAN_POINT ( 'NONE',  ( 6.204703633549690345, 35.76208216824729647, -14.16423886937410259 ) ) ;
#58283 = CARTESIAN_POINT ( 'NONE',  ( 2.791683348922240793, 46.63393115100077324, 7.208316651077764092 ) ) ;
#58284 = CARTESIAN_POINT ( 'NONE',  ( 18.17829156368507881, 9.167925641218957367, 6.499999999999990230 ) ) ;
#58285 = CARTESIAN_POINT ( 'NONE',  ( 15.44008868035555793, 36.39701867748816966, -9.422509992056140149 ) ) ;
#58286 = CARTESIAN_POINT ( 'NONE',  ( 12.91533473730993009, 61.60535201082150536, -10.88017736071109987 ) ) ;
#58287 = SURFACE_SIDE_STYLE ('',( #28789 ) ) ;
#58288 = ORIENTED_EDGE ( 'NONE', *, *, #48173, .F. ) ;
#58289 = CARTESIAN_POINT ( 'NONE',  ( -2.816281873526473856, 39.12363466993041783, 9.499525473075851096E-16 ) ) ;
#58290 = ORIENTED_EDGE ( 'NONE', *, *, #73141, .F. ) ;
#58291 = CARTESIAN_POINT ( 'NONE',  ( 2.035157376598824452, 68.68868534415484817, 7.964842623401179544 ) ) ;
#58292 = ORIENTED_EDGE ( 'NONE', *, *, #456, .T. ) ;
#58293 = AXIS2_PLACEMENT_3D ( 'NONE', #53325, #44831, #23840 ) ;
#58294 = CARTESIAN_POINT ( 'NONE',  ( 17.08211943468705130, 8.470415501580635720, 12.26659068614894998 ) ) ;
#58295 = CARTESIAN_POINT ( 'NONE',  ( 14.92337183194729988, 9.342264484334119601, -8.527530157486177487 ) ) ;
#58296 = EDGE_CURVE ( 'NONE', #77048, #46169, #10833, .T. ) ;
#58297 = DIRECTION ( 'NONE',  ( 0.000000000000000000, 0.000000000000000000, 1.000000000000000000 ) ) ;
#58298 = ORIENTED_EDGE ( 'NONE', *, *, #84241, .F. ) ;
#58299 = LINE ( 'NONE', #81315, #73254 ) ;
#58300 = CARTESIAN_POINT ( 'NONE',  ( 10.00000000000000178, 9.313685344154839285, 10.88017736071110342 ) ) ;
#58301 = CARTESIAN_POINT ( 'NONE',  ( 19.10478245763058069, 61.02576239577081907, -5.990408912944218400 ) ) ;
#58302 = CARTESIAN_POINT ( 'NONE',  ( 10.00000000000000000, 15.55374883491396787, -14.16423886937410082 ) ) ;
#58303 = CARTESIAN_POINT ( 'NONE',  ( 12.91533473730992121, 24.52201867748816966, 10.88017736071110164 ) ) ;
#58304 = CARTESIAN_POINT ( 'NONE',  ( 17.20831665107776587, 64.13393115100079456, -7.208316651077762316 ) ) ;
#58305 = VERTEX_POINT ( 'NONE', #19526 ) ;
#58306 = ADVANCED_FACE ( 'NONE', ( #12023 ), #43013, .T. ) ;
#58307 = CARTESIAN_POINT ( 'NONE',  ( 14.92337183194729988, 59.34226448433412315, -8.527530157486177487 ) ) ;
#58308 = ORIENTED_EDGE ( 'NONE', *, *, #42353, .F. ) ;
#58309 = CARTESIAN_POINT ( 'NONE',  ( 20.88017736071110875, 65.77201867748817676, -2.915334737309920765 ) ) ;
#58310 = CARTESIAN_POINT ( 'NONE',  ( 0.000000000000000000, 0.5000000000000004441, 0.000000000000000000 ) ) ;
#58311 = CARTESIAN_POINT ( 'NONE',  ( 16.40814093676324603, 37.45696800326376064, -11.09922568453594671 ) ) ;
#58313 = FACE_OUTER_BOUND ( 'NONE', #7059, .T. ) ;
#58312 = CARTESIAN_POINT ( 'NONE',  ( 15.44008868035555793, 11.39701867748817143, -9.422509992056140149 ) ) ;
#58314 = CARTESIAN_POINT ( 'NONE',  ( 7.361572987183169658, -0.03273551566588185635, -9.846743663894592657 ) ) ;
#58315 = CARTESIAN_POINT ( 'NONE',  ( 4.559911319644449179, 17.23035201082150536, -9.422509992056141925 ) ) ;
#58316 = B_SPLINE_CURVE_WITH_KNOTS ( 'NONE', 3,
 ( #79711, #33696, #88682, #88186, #64195, #11210 ),
 .UNSPECIFIED., .F., .F.,
 ( 4, 2, 4 ),
 ( 3.409110551496207940E-05, 0.0004400426677367885232, 0.0008459942299586149534 ),
 .UNSPECIFIED. ) ;
#58317 = VERTEX_POINT ( 'NONE', #73496 ) ;
#58318 = CARTESIAN_POINT ( 'NONE',  ( 18.52753015748617571, 33.09226448433411605, 4.923371831947298993 ) ) ;
#58319 = CARTESIAN_POINT ( 'NONE',  ( 10.00000000000000178, 60.37363466993041783, 12.81628187352647608 ) ) ;
#58320 = CARTESIAN_POINT ( 'NONE',  ( 17.96484262340118221, 29.93868534415484106, 7.964842623401181321 ) ) ;
#58321 = CARTESIAN_POINT ( 'NONE',  ( -46.94000000000001194, 101.1610691152390586, -7.882642855603069876 ) ) ;
#58322 = PRESENTATION_LAYER_ASSIGNMENT (  '', '', ( #32780 ) ) ;
#58323 = CARTESIAN_POINT ( 'NONE',  ( 13.43411237798105340, 40.58196800326375353, 12.81628187352647963 ) ) ;
#58324 = CARTESIAN_POINT ( 'NONE',  ( 7.084665262690076126, 54.10535201082151247, 10.88017736071109987 ) ) ;
#58325 = CARTESIAN_POINT ( 'NONE',  ( 1.472469842513823179, 50.59226448433411605, -4.923371831947296329 ) ) ;
#58326 = EDGE_LOOP ( 'NONE', ( #39045, #88165, #15258, #83005, #2882, #63028 ) ) ;
#58327 = DIRECTION ( 'NONE',  ( -1.000000000000000000, 0.000000000000000000, 0.000000000000000000 ) ) ;
#58328 = CARTESIAN_POINT ( 'NONE',  ( 10.00000000000000000, 9.758931151000785675, -9.846743663894594434 ) ) ;
#58329 = CARTESIAN_POINT ( 'NONE',  ( 22.81628187352647785, 11.41530133659708390, 3.434112377981063169 ) ) ;
#58331 = CARTESIAN_POINT ( 'NONE',  ( 2.791683348922240793, 46.63393115100077324, 7.208316651077764092 ) ) ;
#58330 = DIRECTION ( 'NONE',  ( -0.000000000000000000, -1.000000000000000000, -0.000000000000000000 ) ) ;
#58332 = CARTESIAN_POINT ( 'NONE',  ( 10.00000000000000000, 26.81368534415484106, -10.88017736071110342 ) ) ;
#58333 = CARTESIAN_POINT ( 'NONE',  ( 17.20831665107776587, 44.13393115100078745, -7.208316651077762316 ) ) ;
#58334 = LINE ( 'NONE', #11869, #85850 ) ;
#58335 = CARTESIAN_POINT ( 'NONE',  ( 7.361572987183170547, 7.050597817667451750, 9.846743663894590881 ) ) ;
#58336 = EDGE_CURVE ( 'NONE', #79224, #18387, #10188, .T. ) ;
#58338 = ORIENTED_EDGE ( 'NONE', *, *, #38681, .F. ) ;
#58337 = CARTESIAN_POINT ( 'NONE',  ( 17.20831665107776587, 57.88393115100078745, 7.208316651077764980 ) ) ;
#58339 = LINE ( 'NONE', #13351, #83827 ) ;
#58340 = CARTESIAN_POINT ( 'NONE',  ( 13.43411237798106583, 42.66530133659707502, -12.81628187352647252 ) ) ;
#58341 = CARTESIAN_POINT ( 'NONE',  ( 1.472469842513823179, 36.42559781766745175, 4.923371831947296329 ) ) ;
#58342 = CARTESIAN_POINT ( 'NONE',  ( -0.1049300847420783084, 12.21697413083879091, -6.336235997365740502 ) ) ;
#58344 = EDGE_CURVE ( 'NONE', #58154, #42121, #55683, .T. ) ;
#58343 = CARTESIAN_POINT ( 'NONE',  ( -4.164238869374099927, 62.01208216824728936, 3.795296366450308767 ) ) ;
#58345 = CARTESIAN_POINT ( 'NONE',  ( 0.1532563361054082862, 31.21726448433412315, 2.638427012816831674 ) ) ;
#58346 = CARTESIAN_POINT ( 'NONE',  ( -1.926860441876563801, 39.89664270246083788, 3.195792623639529761 ) ) ;
#58347 = CARTESIAN_POINT ( 'NONE',  ( -0.3689425029237881626, 57.42874883491397497, 10.36894250292379027 ) ) ;
#58348 = CARTESIAN_POINT ( 'NONE',  ( 4.879999999999991900, 76.07179676972444327, -6.250000000000000000 ) ) ;
#58349 = CARTESIAN_POINT ( 'NONE',  ( 17.96484262340118221, 19.93868534415484106, 7.964842623401181321 ) ) ;
#58350 = CARTESIAN_POINT ( 'NONE',  ( -0.3689425029237898834, 41.17874883491397497, -10.36894250292378850 ) ) ;
#58352 = CARTESIAN_POINT ( 'NONE',  ( 4.862001128006775197, 15.00000000000000000, -13.66056166602457367 ) ) ;
#58351 = CARTESIAN_POINT ( 'NONE',  ( 10.00000000000000178, 48.05374883491396787, 14.16423886937410082 ) ) ;
#58353 = CARTESIAN_POINT ( 'NONE',  ( -8.000000000000000000, 80.99999999999994316, 2.900000000000001243 ) ) ;
#58354 = CARTESIAN_POINT ( 'NONE',  ( 7.361572987183170547, 7.050597817667451750, 9.846743663894590881 ) ) ;
#58355 = ADVANCED_FACE ( 'NONE', ( #27508 ), #88510, .F. ) ;
#58356 = CARTESIAN_POINT ( 'NONE',  ( 2.791683348922240793, 66.63393115100079456, 7.208316651077764092 ) ) ;
#58357 = CARTESIAN_POINT ( 'NONE',  ( 18.06765999051784632, 13.99127512925448791, 6.500000000000019540 ) ) ;
#58358 = ORIENTED_EDGE ( 'NONE', *, *, #23608, .T. ) ;
#58359 = CARTESIAN_POINT ( 'NONE',  ( 15.44008868035555260, 54.73035201082150536, 9.422509992056143702 ) ) ;
#58360 = MECHANICAL_DESIGN_GEOMETRIC_PRESENTATION_REPRESENTATION (  '', ( #75938 ), #69666 ) ;
#58361 = DIRECTION ( 'NONE',  ( -0.000000000000000000, -1.000000000000000000, -0.000000000000000000 ) ) ;
#58362 = CARTESIAN_POINT ( 'NONE',  ( 12.63842701281683034, 52.46726448433413026, 9.846743663894596210 ) ) ;
#58363 = CARTESIAN_POINT ( 'NONE',  ( -1.983216688680738082, 15.00000000000000000, -14.11131997956740491 ) ) ;
#58364 = FILL_AREA_STYLE ('',( #95401 ) ) ;
#58365 = ORIENTED_EDGE ( 'NONE', *, *, #9438, .F. ) ;
#58366 = AXIS2_PLACEMENT_3D ( 'NONE', #11811, #66282, #58280 ) ;
#58367 = CARTESIAN_POINT ( 'NONE',  ( -0.3689425029237898834, 46.17874883491397497, -10.36894250292378850 ) ) ;
#58368 = CARTESIAN_POINT ( 'NONE',  ( -14.36343418943208761, 14.95077488074853456, -3.367173657400845510 ) ) ;
#58370 = CARTESIAN_POINT ( 'NONE',  ( -2.120353041430445895, 3.806229657360874111E-16, -14.34413130794948543 ) ) ;
#58369 = CARTESIAN_POINT ( 'NONE',  ( 24.35999999999999233, 44.49999999999997868, -9.500000000000000000 ) ) ;
#58371 = CARTESIAN_POINT ( 'NONE',  ( 0.5774900079438607392, 18.48035201082150536, 5.440088680355550821 ) ) ;
#58372 = CARTESIAN_POINT ( 'NONE',  ( 0.6178305044545818747, 43.49863466993042493, -9.382169495545419124 ) ) ;
#58373 = CARTESIAN_POINT ( 'NONE',  ( -11.92686044187656691, 9.479976035794177136, -3.195792623639521324 ) ) ;
#58374 = CARTESIAN_POINT ( 'NONE',  ( 0.6178305044545838731, 24.74863466993042493, 9.382169495545420901 ) ) ;
#58375 = CARTESIAN_POINT ( 'NONE',  ( 22.81628187352647785, 56.41530133659708213, 3.434112377981063169 ) ) ;
#58377 = EDGE_CURVE ( 'NONE', #23275, #24577, #45472, .T. ) ;
#58376 = VERTEX_POINT ( 'NONE', #34508 ) ;
#58378 = CARTESIAN_POINT ( 'NONE',  ( 6.829574850505124139, -88.00372650098208283, -4.000000000000000000 ) ) ;
#58379 = CARTESIAN_POINT ( 'NONE',  ( -8.900000000000002132, 80.99999999999994316, -2.900000000000000355 ) ) ;
#58380 = CARTESIAN_POINT ( 'NONE',  ( 13.79529636645031943, 25.34541550158063572, -14.16423886937409904 ) ) ;
#58381 = CARTESIAN_POINT ( 'NONE',  ( -4.164238869374098151, 1.595415501580634388, -3.795296366450310543 ) ) ;
#58382 = CARTESIAN_POINT ( 'NONE',  ( 9.876730923139298568, 15.00000000000000000, -11.28938378619063165 ) ) ;
#58383 = CARTESIAN_POINT ( 'NONE',  ( -0.8801773607111008646, 23.27201867748817676, 2.915334737309923430 ) ) ;
#58384 = CARTESIAN_POINT ( 'NONE',  ( 11.35178980618974087, 0.5000000000000004441, -9.804941009311923139 ) ) ;
#58385 = CARTESIAN_POINT ( 'NONE',  ( -13.64884605730320644, -0.03417435944610275333, 8.341846182955681144 ) ) ;
#58386 = CARTESIAN_POINT ( 'NONE',  ( 15.44008868035555260, 39.73035201082150536, 9.422509992056143702 ) ) ;
#58387 = CARTESIAN_POINT ( 'NONE',  ( 4.559911319644449179, 53.89701867748817676, 9.422509992056141925 ) ) ;
#58388 = CARTESIAN_POINT ( 'NONE',  ( 13.43411237798106583, 12.66530133659708746, -12.81628187352647252 ) ) ;
#58389 = CARTESIAN_POINT ( 'NONE',  ( -2.815433093577223378, 0.5000000000000004441, 14.73340885523747978 ) ) ;
#58390 = DIRECTION ( 'NONE',  ( 0.000000000000000000, -1.000000000000000000, 0.000000000000000000 ) ) ;
#58391 = CARTESIAN_POINT ( 'NONE',  ( 14.92337183194729633, 27.67559781766745530, 8.527530157486181039 ) ) ;
#58392 = CARTESIAN_POINT ( 'NONE',  ( -22.44000000000001194, 93.50000000000000000, 9.500000000000000000 ) ) ;
#58393 = CARTESIAN_POINT ( 'NONE',  ( 7.084665262690076126, 44.10535201082151247, 10.88017736071109987 ) ) ;
#58394 = STYLED_ITEM ( 'NONE', ( #13046 ), #35948 ) ;
#58395 = AXIS2_PLACEMENT_3D ( 'NONE', #58803, #89310, #52298 ) ;
#58396 = CARTESIAN_POINT ( 'NONE',  ( -2.816281873526473856, 9.331968003263753531, 3.434112377981055619 ) ) ;
#58397 =( NAMED_UNIT ( * ) SI_UNIT ( $, .STERADIAN. ) SOLID_ANGLE_UNIT ( ) );
#58398 = CIRCLE ( 'NONE', #88740, 0.1000000000000001166 ) ;
#58399 = CARTESIAN_POINT ( 'NONE',  ( 7.361572987183169658, 24.96726448433412315, -9.846743663894592657 ) ) ;
#58400 = CARTESIAN_POINT ( 'NONE',  ( 13.43411237798106583, 42.66530133659707502, -12.81628187352647252 ) ) ;
#58401 = CARTESIAN_POINT ( 'NONE',  ( 2.791683348922237240, 10.38393115100078390, -7.208316651077763204 ) ) ;
#58402 = VERTEX_POINT ( 'NONE', #75482 ) ;
#58403 = CARTESIAN_POINT ( 'NONE',  ( -7.750000000000000000, 40.99999999999999289, -4.250000000000000000 ) ) ;
#58404 = CARTESIAN_POINT ( 'NONE',  ( 0.1532563361054100626, 35.80059781766745175, -2.638427012816831230 ) ) ;
#58405 = CARTESIAN_POINT ( 'NONE',  ( 19.42250999205614193, 25.14701867748817321, 5.440088680355555262 ) ) ;
#58407 = CARTESIAN_POINT ( 'NONE',  ( -2.266590686148945544, 36.38708216824730357, -7.082119434687050408 ) ) ;
#58406 = CARTESIAN_POINT ( 'NONE',  ( 7.361080431567760485, -0.6440110890646428832, 2.900000000000000355 ) ) ;
#58408 = CARTESIAN_POINT ( 'NONE',  ( 17.20831665107776587, 27.88393115100078390, 7.208316651077764980 ) ) ;
#58409 = CARTESIAN_POINT ( 'NONE',  ( 2.035157376598824452, 18.68868534415484106, 7.964842623401179544 ) ) ;
#58410 = CARTESIAN_POINT ( 'NONE',  ( 4.559911319644449179, 3.897018677488171434, 9.422509992056141925 ) ) ;
#58411 = VERTEX_POINT ( 'NONE', #44487 ) ;
#58412 = CARTESIAN_POINT ( 'NONE',  ( 2.035157376598822676, 7.438685344154837509, -7.964842623401177768 ) ) ;
#58413 = EDGE_CURVE ( 'NONE', #56516, #55254, #7636, .T. ) ;
#58414 = CARTESIAN_POINT ( 'NONE',  ( 7.084665262690076126, 29.10535201082150181, 10.88017736071109987 ) ) ;
#58416 = CARTESIAN_POINT ( 'NONE',  ( 0.5774900079438590739, 42.64701867748816966, -5.440088680355550821 ) ) ;
#58415 = CARTESIAN_POINT ( 'NONE',  ( -12.11353679309427278, 14.95037110518055989, -8.421373815019801867 ) ) ;
#58417 = ORIENTED_EDGE ( 'NONE', *, *, #94697, .F. ) ;
#58418 = CARTESIAN_POINT ( 'NONE',  ( 21.92686044187656691, 27.18830936912750573, 4.562052436263911564E-16 ) ) ;
#58419 = CARTESIAN_POINT ( 'NONE',  ( 15.44008868035555793, 36.39701867748816966, -9.422509992056140149 ) ) ;
#58420 = CARTESIAN_POINT ( 'NONE',  ( 1.472469842513823179, 66.42559781766745175, 4.923371831947296329 ) ) ;
#58421 = CIRCLE ( 'NONE', #83995, 2.750000000000000888 ) ;
#58422 = DIRECTION ( 'NONE',  ( -0.000000000000000000, -1.000000000000000000, -0.000000000000000000 ) ) ;
#58423 = CARTESIAN_POINT ( 'NONE',  ( -2.816281873526471635, 63.91530133659708923, -3.434112377981056508 ) ) ;
#58424 = DIRECTION ( 'NONE',  ( 1.257568779154408793E-17, 1.000000000000000000, -0.000000000000000000 ) ) ;
#58425 = CARTESIAN_POINT ( 'NONE',  ( 2.917880565312948704, 27.63708216824730357, 12.26659068614894643 ) ) ;
#58426 = CARTESIAN_POINT ( 'NONE',  ( -0.8801773607111008646, 48.27201867748816966, 2.915334737309923430 ) ) ;
#58427 = CARTESIAN_POINT ( 'NONE',  ( 19.42250999205614193, 25.14701867748817321, 5.440088680355555262 ) ) ;
#58428 = CARTESIAN_POINT ( 'NONE',  ( 19.84674366389459621, 63.50893115100078745, 7.409399052514197653E-17 ) ) ;
#58429 = B_SPLINE_CURVE_WITH_KNOTS ( 'NONE', 3,
 ( #70548, #54539, #94030, #2076 ),
 .UNSPECIFIED., .F., .F.,
 ( 4, 4 ),
 ( 0.000000000000000000, 0.002562518741975564930 ),
 .UNSPECIFIED. ) ;
#58430 = FACE_OUTER_BOUND ( 'NONE', #64998, .T. ) ;
#58431 = CARTESIAN_POINT ( 'NONE',  ( 2.791683348922237240, 55.38393115100078745, -7.208316651077763204 ) ) ;
#58432 = VERTEX_POINT ( 'NONE', #75974 ) ;
#58433 = CARTESIAN_POINT ( 'NONE',  ( 1.472469842513823179, 15.59226448433411960, -4.923371831947296329 ) ) ;
#58434 = CARTESIAN_POINT ( 'NONE',  ( 9.382169495545419124, -19.00136533006957507, 9.382169495545417348 ) ) ;
#58435 = CARTESIAN_POINT ( 'NONE',  ( 12.91533473730992121, 19.52201867748816611, 10.88017736071110164 ) ) ;
#58436 = CARTESIAN_POINT ( 'NONE',  ( 18.52753015748617571, 28.09226448433411960, 4.923371831947298993 ) ) ;
#58437 = CARTESIAN_POINT ( 'NONE',  ( 0.6178305044545818747, 8.498634669930421381, -9.382169495545419124 ) ) ;
#58439 = CARTESIAN_POINT ( 'NONE',  ( 20.88017736071110875, 50.77201867748817676, -2.915334737309920765 ) ) ;
#58438 = CARTESIAN_POINT ( 'NONE',  ( 12.91533473730992121, 54.52201867748816255, 10.88017736071110164 ) ) ;
#58441 = CARTESIAN_POINT ( 'NONE',  ( 6.565887622018943937, 58.08196800326376064, -12.81628187352647608 ) ) ;
#58440 = CARTESIAN_POINT ( 'NONE',  ( 17.96484262340118221, 34.93868534415482685, 7.964842623401181321 ) ) ;
#58442 = CARTESIAN_POINT ( 'NONE',  ( -2.266590686148945544, 46.38708216824730357, -7.082119434687050408 ) ) ;
#58443 = VECTOR ( 'NONE', #76601, 1000.000000000000000 ) ;
#58444 = AXIS2_PLACEMENT_3D ( 'NONE', #47674, #24199, #17683 ) ;
#58445 = DIRECTION ( 'NONE',  ( 0.000000000000000000, 0.000000000000000000, -1.000000000000000000 ) ) ;
#58446 = ORIENTED_EDGE ( 'NONE', *, *, #84746, .F. ) ;
#58447 = CARTESIAN_POINT ( 'NONE',  ( -2.816281873526473856, -0.6680319967362464695, 3.434112377981055619 ) ) ;
#58448 = CARTESIAN_POINT ( 'NONE',  ( 17.96484262340118221, 11.18868534415483929, -7.964842623401177768 ) ) ;
#58449 = CARTESIAN_POINT ( 'NONE',  ( 19.42250999205614548, 40.98035201082150536, -5.440088680355545492 ) ) ;
#58450 = CARTESIAN_POINT ( 'NONE',  ( 19.84674366389459266, 63.71726448433412315, -2.638427012816827677 ) ) ;
#58451 = ORIENTED_EDGE ( 'NONE', *, *, #19126, .F. ) ;
#58452 = CARTESIAN_POINT ( 'NONE',  ( 18.52753015748617571, 13.09226448433411960, 4.923371831947298993 ) ) ;
#58453 = CARTESIAN_POINT ( 'NONE',  ( 19.84674366389459266, 8.717264484334116048, -2.638427012816827677 ) ) ;
#58454 = CARTESIAN_POINT ( 'NONE',  ( 10.00000000000000178, 27.25893115100078390, 9.846743663894594434 ) ) ;
#58455 = EDGE_CURVE ( 'NONE', #79695, #78202, #14506, .T. ) ;
#58456 = CARTESIAN_POINT ( 'NONE',  ( 7.361572987183169658, 9.967264484334119601, -9.846743663894592657 ) ) ;
#58457 = CARTESIAN_POINT ( 'NONE',  ( -4.096035146093626622, 4.358906096699807873E-16, 13.90943910019256258 ) ) ;
#58458 = CARTESIAN_POINT ( 'NONE',  ( 18.17884179759847285, 63.66688879859523809, -6.500000000000002665 ) ) ;
#58460 = DIRECTION ( 'NONE',  ( 0.9942165912674658657, -0.1073935270325955399, 0.000000000000000000 ) ) ;
#58459 = CARTESIAN_POINT ( 'NONE',  ( 2.791683348922240793, 6.633931151000785675, 7.208316651077764092 ) ) ;
#58461 = CARTESIAN_POINT ( 'NONE',  ( 0.1532563361054082862, 6.217264484334118713, 2.638427012816831674 ) ) ;
#58462 = MECHANICAL_DESIGN_GEOMETRIC_PRESENTATION_REPRESENTATION (  '', ( #20144 ), #80821 ) ;
#58464 = ORIENTED_EDGE ( 'NONE', *, *, #73127, .F. ) ;
#58463 = CARTESIAN_POINT ( 'NONE',  ( 12.63842701281683922, 24.55059781766745175, -9.846743663894590881 ) ) ;
#58465 = ADVANCED_FACE ( 'NONE', ( #67495 ), #56012, .T. ) ;
#58466 = EDGE_CURVE ( 'NONE', #16129, #85150, #23129, .T. ) ;
#58467 = CARTESIAN_POINT ( 'NONE',  ( 7.160365893312770069, -84.29711206764774545, 3.999999999999999112 ) ) ;
#58468 = CARTESIAN_POINT ( 'NONE',  ( 19.84674366389459621, 63.50893115100078745, 7.409399052514197653E-17 ) ) ;
#58469 = ORIENTED_EDGE ( 'NONE', *, *, #25141, .T. ) ;
#58470 =( NAMED_UNIT ( * ) PLANE_ANGLE_UNIT ( ) SI_UNIT ( $, .RADIAN. ) );
#58471 = EDGE_CURVE ( 'NONE', #69763, #94718, #30104, .T. ) ;
#58472 = AXIS2_PLACEMENT_3D ( 'NONE', #10153, #55651, #63620 ) ;
#58474 = EDGE_CURVE ( 'NONE', #31975, #88480, #92587, .T. ) ;
#58473 = CARTESIAN_POINT ( 'NONE',  ( 13.79529636645030344, 13.26208216824729824, 14.16423886937410614 ) ) ;
#58475 = UNCERTAINTY_MEASURE_WITH_UNIT (LENGTH_MEASURE( 1.000000000000000082E-05 ), #23083, 'distance_accuracy_value', 'NONE');
#58476 = DIRECTION ( 'NONE',  ( 0.000000000000000000, 0.000000000000000000, 1.000000000000000000 ) ) ;
#58477 = CARTESIAN_POINT ( 'NONE',  ( 13.79529636645030344, 18.26208216824730002, 14.16423886937410614 ) ) ;
#58478 = CARTESIAN_POINT ( 'NONE',  ( 2.917880565312948704, 42.63708216824729647, 12.26659068614894643 ) ) ;
#58479 = CARTESIAN_POINT ( 'NONE',  ( 24.16423886937410614, 9.512082168247301794, -3.795296366450302550 ) ) ;
#58480 = CARTESIAN_POINT ( 'NONE',  ( -0.8801773607111008646, 38.27201867748816255, 2.915334737309923430 ) ) ;
#58481 = CARTESIAN_POINT ( 'NONE',  ( 11.12471383767373467, 2.500000000000004885, 1.674288514525068328 ) ) ;
#58482 = EDGE_LOOP ( 'NONE', ( #44945, #1640, #42495, #44363, #70047, #18253, #81742, #97400, #67574, #88190, #69746, #2237, #46068, #74282, #86865, #63156, #38743, #51076, #35463, #41203 ) ) ;
#58483 = CARTESIAN_POINT ( 'NONE',  ( 1.472469842513823179, 21.42559781766745175, 4.923371831947296329 ) ) ;
#58485 = CARTESIAN_POINT ( 'NONE',  ( 19.84674366389459266, 33.71726448433410894, -2.638427012816827677 ) ) ;
#58484 = CARTESIAN_POINT ( 'NONE',  ( 0.5774900079438590739, 57.64701867748817676, -5.440088680355550821 ) ) ;
#58486 = EDGE_CURVE ( 'NONE', #29308, #62057, #85059, .T. ) ;
#58487 = CARTESIAN_POINT ( 'NONE',  ( 4.559911319644449179, 7.230352010821505360, -9.422509992056141925 ) ) ;
#58488 = CARTESIAN_POINT ( 'NONE',  ( -1.099225684535947600, 64.54030133659709634, 6.408140936763237150 ) ) ;
#58489 = CARTESIAN_POINT ( 'NONE',  ( 5.076628168052703671, 56.84226448433412315, 8.527530157486179263 ) ) ;
#58490 = DIRECTION ( 'NONE',  ( -1.000000000000000000, 0.000000000000000000, 0.000000000000000000 ) ) ;
#58492 = CARTESIAN_POINT ( 'NONE',  ( 6.565887622018943937, 38.08196800326376064, -12.81628187352647608 ) ) ;
#58491 = MECHANICAL_DESIGN_GEOMETRIC_PRESENTATION_REPRESENTATION (  '', ( #2659 ), #1070 ) ;
#58493 = CARTESIAN_POINT ( 'NONE',  ( -12.26659068614894110, -22.77958449841936073, 7.082119434687058401 ) ) ;
#58494 = MECHANICAL_DESIGN_GEOMETRIC_PRESENTATION_REPRESENTATION (  '', ( #9044 ), #64904 ) ;
#58495 = CARTESIAN_POINT ( 'NONE',  ( 0.5774900079438590739, 47.64701867748817676, -5.440088680355550821 ) ) ;
#58496 = CARTESIAN_POINT ( 'NONE',  ( 17.20831665107776587, 37.88393115100078745, 7.208316651077764980 ) ) ;
#58497 = CARTESIAN_POINT ( 'NONE',  ( 20.36894250292379738, 29.92874883491396432, -10.36894250292379027 ) ) ;
#58498 = ORIENTED_EDGE ( 'NONE', *, *, #4609, .T. ) ;
#58499 = LINE ( 'NONE', #50514, #65110 ) ;
#58500 = CARTESIAN_POINT ( 'NONE',  ( 0.5774900079438590739, 52.64701867748817676, -5.440088680355550821 ) ) ;
#58501 = CARTESIAN_POINT ( 'NONE',  ( -0.8801773607111009756, 63.06368534415484106, 1.068504757029289695E-15 ) ) ;
#58502 = CARTESIAN_POINT ( 'NONE',  ( 6.204703633549690345, 50.76208216824730357, -14.16423886937410259 ) ) ;
#58503 = CARTESIAN_POINT ( 'NONE',  ( 0.1532563361054082862, 66.21726448433413736, 2.638427012816831674 ) ) ;
#58504 = CARTESIAN_POINT ( 'NONE',  ( 22.81628187352647785, 61.41530133659709634, 3.434112377981063169 ) ) ;
#58505 = CARTESIAN_POINT ( 'NONE',  ( 4.559911319644449179, 38.89701867748817676, 9.422509992056141925 ) ) ;
#58506 = EDGE_CURVE ( 'NONE', #72124, #30282, #46116, .T. ) ;
#58507 = DIRECTION ( 'NONE',  ( 0.000000000000000000, -1.000000000000000000, 0.000000000000000000 ) ) ;
#58508 = CARTESIAN_POINT ( 'NONE',  ( 2.791683348922237240, 60.38393115100078745, -7.208316651077763204 ) ) ;
#58509 = CARTESIAN_POINT ( 'NONE',  ( 2.915334737309928315, 14.52201867748817499, 10.88017736071109987 ) ) ;
#58510 = FILL_AREA_STYLE ('',( #41574 ) ) ;
#58511 = CARTESIAN_POINT ( 'NONE',  ( 4.559911319644449179, 7.230352010821505360, -9.422509992056141925 ) ) ;
#58512 = CARTESIAN_POINT ( 'NONE',  ( 7.285838599102620089E-14, 21.00000000000003197, 3.000000000000000000 ) ) ;
#58513 = ORIENTED_EDGE ( 'NONE', *, *, #43080, .F. ) ;
#58514 = B_SPLINE_CURVE_WITH_KNOTS ( 'NONE', 3,
 ( #42146, #57615, #88113, #50117, #12121, #42623 ),
 .UNSPECIFIED., .F., .F.,
 ( 4, 2, 4 ),
 ( 3.409110551495909784E-05, 0.0004400426677367837527, 0.0008459942299586083398 ),
 .UNSPECIFIED. ) ;
#58515 = VECTOR ( 'NONE', #10998, 999.9999999999998863 ) ;
#58516 = CARTESIAN_POINT ( 'NONE',  ( 0.000000000000000000, 0.5000000000000004441, 0.000000000000000000 ) ) ;
#58517 = CARTESIAN_POINT ( 'NONE',  ( 0.5774900079438590739, 67.64701867748817676, -5.440088680355550821 ) ) ;
#58518 = CARTESIAN_POINT ( 'NONE',  ( 19.42250999205614193, 65.14701867748817676, 5.440088680355555262 ) ) ;
#58519 = DIRECTION ( 'NONE',  ( 0.000000000000000000, 0.000000000000000000, 1.000000000000000000 ) ) ;
#58520 = CARTESIAN_POINT ( 'NONE',  ( 19.84674366389459266, 28.71726448433411960, -2.638427012816827677 ) ) ;
#58521 = CARTESIAN_POINT ( 'NONE',  ( -0.8801773607111008646, 23.27201867748817676, 2.915334737309923430 ) ) ;
#58522 = CARTESIAN_POINT ( 'NONE',  ( 19.38216949554541202, 5.998634669930420493, 9.382169495545424454 ) ) ;
#58524 = LINE ( 'NONE', #51526, #57570 ) ;
#58523 = CARTESIAN_POINT ( 'NONE',  ( 12.91533473730993009, 31.60535201082150891, -10.88017736071109987 ) ) ;
#58525 = CARTESIAN_POINT ( 'NONE',  ( -2.816281873526473856, 34.33196800326376064, 3.434112377981055619 ) ) ;
#58526 = ORIENTED_EDGE ( 'NONE', *, *, #93150, .F. ) ;
#58527 = CARTESIAN_POINT ( 'NONE',  ( 7.084665262690076126, 67.02201867748817676, -10.88017736071110164 ) ) ;
#58529 = CARTESIAN_POINT ( 'NONE',  ( 9.402796353261051010, 0.5000000000000004441, 11.68706210897763320 ) ) ;
#58528 = CARTESIAN_POINT ( 'NONE',  ( 0.6178305044545818747, 23.49863466993041783, -9.382169495545419124 ) ) ;
#58530 = CARTESIAN_POINT ( 'NONE',  ( 10.00000000000000000, -0.2410688489992152128, -9.846743663894594434 ) ) ;
#58531 = CARTESIAN_POINT ( 'NONE',  ( 7.084665262690076126, 34.10535201082151247, 10.88017736071109987 ) ) ;
#58532 = LINE ( 'NONE', #22041, #59575 ) ;
#58533 = CARTESIAN_POINT ( 'NONE',  ( 2.917880565312950480, 60.97041550158063927, -12.26659068614894821 ) ) ;
#58534 = CARTESIAN_POINT ( 'NONE',  ( 14.92337183194729988, 49.34226448433411605, -8.527530157486177487 ) ) ;
#58535 = CARTESIAN_POINT ( 'NONE',  ( 0.5774900079438607392, 68.48035201082150536, 5.440088680355550821 ) ) ;
#58536 = CARTESIAN_POINT ( 'NONE',  ( -0.8801773607110991993, 57.85535201082149825, -2.915334737309923874 ) ) ;
#58537 = CARTESIAN_POINT ( 'NONE',  ( 0.1143410931637199451, 5.216910754863025801, 6.480892540919842126 ) ) ;
#58538 = CARTESIAN_POINT ( 'NONE',  ( 24.16423886937409904, 24.09541550158063927, 3.795296366450317205 ) ) ;
#58539 = VECTOR ( 'NONE', #47300, 1000.000000000000114 ) ;
#58540 = VECTOR ( 'NONE', #20757, 1000.000000000000000 ) ;
#58541 = CARTESIAN_POINT ( 'NONE',  ( -15.08495336817617982, 15.00000000000000000, 5.321802168063332950 ) ) ;
#58542 = CARTESIAN_POINT ( 'NONE',  ( -3.500000000000000888, 1.019547802438454109, -4.000000000000000000 ) ) ;
#58543 = ORIENTED_EDGE ( 'NONE', *, *, #45261, .T. ) ;
#58544 = CARTESIAN_POINT ( 'NONE',  ( -4.164238869374098151, 56.59541550158063927, -3.795296366450310543 ) ) ;
#58545 = CARTESIAN_POINT ( 'NONE',  ( 6.204703633549690345, 45.76208216824729647, -14.16423886937410259 ) ) ;
#58546 = CARTESIAN_POINT ( 'NONE',  ( 19.84674366389459266, 28.71726448433411960, -2.638427012816827677 ) ) ;
#58547 = CARTESIAN_POINT ( 'NONE',  ( 13.43411237798106583, 27.66530133659708568, -12.81628187352647252 ) ) ;
#58548 = FACE_OUTER_BOUND ( 'NONE', #80773, .T. ) ;
#58549 = CARTESIAN_POINT ( 'NONE',  ( 7.084665262690076126, 14.10535201082150358, 10.88017736071109987 ) ) ;
#58550 = CARTESIAN_POINT ( 'NONE',  ( 2.917880565312948704, 52.63708216824730357, 12.26659068614894643 ) ) ;
#58551 = CIRCLE ( 'NONE', #50567, 0.09999999999999982514 ) ;
#58552 = CARTESIAN_POINT ( 'NONE',  ( 5.076628168052703671, 31.84226448433412315, 8.527530157486179263 ) ) ;
#58553 = CARTESIAN_POINT ( 'NONE',  ( 1.274849032794305170, 12.55509018479935968, -6.499999999999995559 ) ) ;
#58554 = CARTESIAN_POINT ( 'NONE',  ( 0.1532563361054100626, 10.80059781766745175, -2.638427012816831230 ) ) ;
#58555 = CARTESIAN_POINT ( 'NONE',  ( 17.62281668512001431, 58.28593319516822646, 6.500000000000010658 ) ) ;
#58556 = CARTESIAN_POINT ( 'NONE',  ( 8.527530157486175710, 3.925597817667457523, -4.923371831947298993 ) ) ;
#58557 = ORIENTED_EDGE ( 'NONE', *, *, #46970, .F. ) ;
#58558 = ORIENTED_EDGE ( 'NONE', *, *, #43941, .T. ) ;
#58559 = FILL_AREA_STYLE_COLOUR ( '', #66915 ) ;
#58560 = ORIENTED_EDGE ( 'NONE', *, *, #72663, .T. ) ;
#58561 = PRESENTATION_LAYER_ASSIGNMENT (  '', '', ( #36227 ) ) ;
#58562 = CARTESIAN_POINT ( 'NONE',  ( 22.26659068614895176, 14.72041550158063572, -7.082119434687042414 ) ) ;
#58564 = CARTESIAN_POINT ( 'NONE',  ( 15.44008868035555260, 29.73035201082150891, 9.422509992056143702 ) ) ;
#58563 = CARTESIAN_POINT ( 'NONE',  ( 7.084665262690076126, 17.02201867748817676, -10.88017736071110164 ) ) ;
#58566 = CARTESIAN_POINT ( 'NONE',  ( -1.099225684535947600, 18.70696800326375353, -6.408140936763238038 ) ) ;
#58565 = CARTESIAN_POINT ( 'NONE',  ( 19.84674366389459621, 43.50893115100078745, 7.409399052514197653E-17 ) ) ;
#58567 = CARTESIAN_POINT ( 'NONE',  ( 10.00000000000000000, 10.55374883491396787, -14.16423886937410082 ) ) ;
#58568 = ADVANCED_FACE ( 'NONE', ( #1123 ), #31585, .T. ) ;
#58569 = LINE ( 'NONE', #88080, #20752 ) ;
#58570 = PRESENTATION_LAYER_ASSIGNMENT (  '', '', ( #5910 ) ) ;
#58571 = AXIS2_PLACEMENT_3D ( 'NONE', #6530, #44025, #20050 ) ;
#58572 = AXIS2_PLACEMENT_3D ( 'NONE', #88503, #20006, #58490 ) ;
#58573 = CARTESIAN_POINT ( 'NONE',  ( 16.40814093676324603, 27.45696800326375708, -11.09922568453594671 ) ) ;
#58574 = ORIENTED_EDGE ( 'NONE', *, *, #95864, .T. ) ;
#58575 = CARTESIAN_POINT ( 'NONE',  ( 14.92337183194729633, 27.67559781766745530, 8.527530157486181039 ) ) ;
#58576 = CARTESIAN_POINT ( 'NONE',  ( -4.164238869374098151, 56.59541550158063927, -3.795296366450310543 ) ) ;
#58577 = ORIENTED_EDGE ( 'NONE', *, *, #98768, .F. ) ;
#58578 = CARTESIAN_POINT ( 'NONE',  ( 2.917880565312950480, 65.97041550158063217, -12.26659068614894821 ) ) ;
#58579 = ORIENTED_EDGE ( 'NONE', *, *, #23968, .F. ) ;
#58580 = CARTESIAN_POINT ( 'NONE',  ( 4.559911319644449179, 52.23035201082151247, -9.422509992056141925 ) ) ;
#58581 = CARTESIAN_POINT ( 'NONE',  ( 4.559911319644449179, 43.89701867748816966, 9.422509992056141925 ) ) ;
#58582 = CARTESIAN_POINT ( 'NONE',  ( 4.559911319644449179, 52.23035201082151247, -9.422509992056141925 ) ) ;
#58583 = PRESENTATION_STYLE_ASSIGNMENT (( #88092 ) ) ;
#58584 = CARTESIAN_POINT ( 'NONE',  ( 15.44008868035555260, 34.73035201082151247, 9.422509992056143702 ) ) ;
#58585 = LINE ( 'NONE', #43583, #1207 ) ;
#58587 = ORIENTED_EDGE ( 'NONE', *, *, #79124, .T. ) ;
#58586 = CARTESIAN_POINT ( 'NONE',  ( 10.17177286909463341, 14.76984972048479783, 10.94336654633689321 ) ) ;
#58588 = EDGE_CURVE ( 'NONE', #45519, #12193, #48063, .T. ) ;
#58589 = CARTESIAN_POINT ( 'NONE',  ( 18.52753015748617571, 33.09226448433411605, 4.923371831947298993 ) ) ;
#58590 = ORIENTED_EDGE ( 'NONE', *, *, #93242, .F. ) ;
#58591 = CARTESIAN_POINT ( 'NONE',  ( 19.84674366389459266, 58.71726448433411605, -2.638427012816827677 ) ) ;
#58593 = EDGE_CURVE ( 'NONE', #37579, #15233, #9093, .T. ) ;
#58592 = CARTESIAN_POINT ( 'NONE',  ( -0.1503990784575260087, 24.24884699246888786, -6.262539305110081500 ) ) ;
#58594 = AXIS2_PLACEMENT_3D ( 'NONE', #91680, #23198, #8666 ) ;
#58595 = B_SPLINE_CURVE_WITH_KNOTS ( 'NONE', 3,
 ( #72412, #96427, #50406, #27410, #87425, #57901, #89397 ),
 .UNSPECIFIED., .F., .F.,
 ( 4, 3, 4 ),
 ( 1.748223473168675632E-18, 0.001126965689051421778, 0.002254079279539391613 ),
 .UNSPECIFIED. ) ;
#58596 = CARTESIAN_POINT ( 'NONE',  ( 24.16423886937410614, 4.303748834913967869, 8.672049930838204340E-16 ) ) ;
#58597 = ORIENTED_EDGE ( 'NONE', *, *, #33525, .F. ) ;
#58598 = DIRECTION ( 'NONE',  ( 4.510281037539694028E-14, 1.000000000000000000, -0.000000000000000000 ) ) ;
#58599 = CARTESIAN_POINT ( 'NONE',  ( 1.046131998949896280, 25.73810908735718428, 6.499999999999989342 ) ) ;
#58600 = CARTESIAN_POINT ( 'NONE',  ( 20.36894250292379738, 64.92874883491397497, -10.36894250292379027 ) ) ;
#58601 = FACE_OUTER_BOUND ( 'NONE', #1057, .T. ) ;
#58602 = VERTEX_POINT ( 'NONE', #78577 ) ;
#58603 =( BOUNDED_CURVE ( )  B_SPLINE_CURVE ( 2, ( #70322, #48287, #40313, #41312, #16821, #9811, #94277, #1837, #10306 ),
 .UNSPECIFIED., .F., .F. ) 
 B_SPLINE_CURVE_WITH_KNOTS ( ( 3, 2, 2, 2, 3 ),
 ( 0.6544266512259456769, 0.6547619047619047672, 0.6607142857142858094, 0.6666666666666667407, 0.6670019202026259419 ),
 .UNSPECIFIED. ) 
 CURVE ( )  GEOMETRIC_REPRESENTATION_ITEM ( )  RATIONAL_B_SPLINE_CURVE ( ( 0.9963778908391764944, 0.9980808541467923733, 1.000000000000000000, 0.9659258262890683122, 1.000000000000000000, 0.9659258262890683122, 1.000000000000000000, 0.9980808541467917072, 0.9963778908391753841 ) ) 
 REPRESENTATION_ITEM ( '' )  );
#58604 = DIRECTION ( 'NONE',  ( 0.000000000000000000, 0.000000000000000000, 1.000000000000000000 ) ) ;
#58605 = CARTESIAN_POINT ( 'NONE',  ( 2.791683348922240793, 36.63393115100078035, 7.208316651077764092 ) ) ;
#58606 = CARTESIAN_POINT ( 'NONE',  ( -13.16740645155975464, 14.95077488074853811, 6.653232860246455438 ) ) ;
#58607 = CARTESIAN_POINT ( 'NONE',  ( 21.09922568453594849, 6.206968003263753531, 6.408140936763242479 ) ) ;
#58608 = CARTESIAN_POINT ( 'NONE',  ( 19.84674366389459266, 13.71726448433411782, -2.638427012816827677 ) ) ;
#58609 = CARTESIAN_POINT ( 'NONE',  ( 2.603489959281588995, 40.43575266056827644, -6.500000000000003553 ) ) ;
#58610 = CARTESIAN_POINT ( 'NONE',  ( 19.84674366389459266, 3.300597817667451750, 2.638427012816836559 ) ) ;
#58611 = CARTESIAN_POINT ( 'NONE',  ( 22.81628187352647785, 6.415301336597088344, 3.434112377981063169 ) ) ;
#58612 = DIRECTION ( 'NONE',  ( 1.000000000000000000, 2.641710877122040890E-15, 0.000000000000000000 ) ) ;
#58613 = B_SPLINE_CURVE_WITH_KNOTS ( 'NONE', 3,
 ( #67623, #29593, #13622, #44103, #74613, #44611 ),
 .UNSPECIFIED., .F., .F.,
 ( 4, 2, 4 ),
 ( 0.0002800760588436753545, 0.0006862820326555788431, 0.001092488006467482332 ),
 .UNSPECIFIED. ) ;
#58614 = VECTOR ( 'NONE', #10163, 1000.000000000000000 ) ;
#58615 = ORIENTED_EDGE ( 'NONE', *, *, #42360, .F. ) ;
#58616 = CARTESIAN_POINT ( 'NONE',  ( 19.42250999205614193, 10.14701867748816966, 5.440088680355555262 ) ) ;
#58617 = CARTESIAN_POINT ( 'NONE',  ( 24.16423886937410614, 4.512082168247300906, -3.795296366450302550 ) ) ;
#58618 = CARTESIAN_POINT ( 'NONE',  ( 14.92337183194729633, 22.67559781766745175, 8.527530157486181039 ) ) ;
#58619 = CARTESIAN_POINT ( 'NONE',  ( 17.96484262340118221, 56.18868534415484817, -7.964842623401177768 ) ) ;
#58621 = PRESENTATION_STYLE_ASSIGNMENT (( #75104 ) ) ;
#58620 = CARTESIAN_POINT ( 'NONE',  ( 0.6178305044545838731, 24.74863466993042493, 9.382169495545420901 ) ) ;
#58622 = CARTESIAN_POINT ( 'NONE',  ( 15.44008868035555793, 6.397018677488170546, -9.422509992056140149 ) ) ;
#58623 = ADVANCED_FACE ( 'NONE', ( #77578 ), #79565, .T. ) ;
#58624 = DIRECTION ( 'NONE',  ( -1.000000000000000000, 0.000000000000000000, 0.000000000000000000 ) ) ;
#58625 = SURFACE_SIDE_STYLE ('',( #95648 ) ) ;
#58626 = PRESENTATION_LAYER_ASSIGNMENT (  '', '', ( #28301 ) ) ;
#58627 = CARTESIAN_POINT ( 'NONE',  ( 3.591859063236761518, 4.956968003263753531, 11.09922568453594849 ) ) ;
#58628 = CARTESIAN_POINT ( 'NONE',  ( 21.09922568453594849, 1.206968003263753531, 6.408140936763242479 ) ) ;
#58629 = CARTESIAN_POINT ( 'NONE',  ( 0.1532563361054082862, 16.21726448433411960, 2.638427012816831674 ) ) ;
#58630 = CARTESIAN_POINT ( 'NONE',  ( -7.964842623401179544, -27.56131465584515894, -7.964842623401174215 ) ) ;
#58631 = CARTESIAN_POINT ( 'NONE',  ( 10.00000000000000178, 25.37363466993041783, 12.81628187352647608 ) ) ;
#58632 = CARTESIAN_POINT ( 'NONE',  ( -11.48880622960838593, -88.23206844530358239, -3.999999999998199218 ) ) ;
#58634 = CARTESIAN_POINT ( 'NONE',  ( 11.10136736363526744, 14.95077488074853811, 9.716261771424980154 ) ) ;
#58633 = CARTESIAN_POINT ( 'NONE',  ( 20.88017736071110875, 25.77201867748816966, -2.915334737309920765 ) ) ;
#58635 = CARTESIAN_POINT ( 'NONE',  ( 13.79529636645031943, 50.34541550158064638, -14.16423886937409904 ) ) ;
#58636 = CIRCLE ( 'NONE', #74623, 0.5000000000000004441 ) ;
#58637 = CARTESIAN_POINT ( 'NONE',  ( 1.796787675079194013, 14.76984984742152385, 14.83218748772992690 ) ) ;
#58638 = AXIS2_PLACEMENT_3D ( 'NONE', #26326, #42323, #4336 ) ;
#58639 = CARTESIAN_POINT ( 'NONE',  ( 12.91533473730993009, 26.60535201082150536, -10.88017736071109987 ) ) ;
#58640 = CARTESIAN_POINT ( 'NONE',  ( 1.472469842513823179, 45.59226448433412315, -4.923371831947296329 ) ) ;
#58641 = CARTESIAN_POINT ( 'NONE',  ( 12.91533473730993009, 51.60535201082149825, -10.88017736071109987 ) ) ;
#58642 = CARTESIAN_POINT ( 'NONE',  ( 22.26659068614894466, 33.88708216824730357, 7.082119434687054849 ) ) ;
#58643 = LINE ( 'NONE', #88151, #13636 ) ;
#58644 = CARTESIAN_POINT ( 'NONE',  ( 19.84674366389459621, 33.50893115100078745, 7.409399052514197653E-17 ) ) ;
#58645 = CARTESIAN_POINT ( 'NONE',  ( -1.099225684535947600, 59.54030133659708923, 6.408140936763237150 ) ) ;
#58646 = CARTESIAN_POINT ( 'NONE',  ( 7.361572987183170547, 62.05059781766745886, 9.846743663894590881 ) ) ;
#58647 = ORIENTED_EDGE ( 'NONE', *, *, #1082, .T. ) ;
#58648 = CARTESIAN_POINT ( 'NONE',  ( 19.42250999205614193, 25.14701867748817321, 5.440088680355555262 ) ) ;
#58649 = CARTESIAN_POINT ( 'NONE',  ( 0.5774900079438590739, 12.64701867748817321, -5.440088680355550821 ) ) ;
#58650 = CARTESIAN_POINT ( 'NONE',  ( 5.076628168052703671, 1.842264484334118047, 8.527530157486179263 ) ) ;
#58651 = CARTESIAN_POINT ( 'NONE',  ( -4.164238869374099039, 21.80374883491396787, 8.674139862899312516E-16 ) ) ;
#58652 = CARTESIAN_POINT ( 'NONE',  ( 0.1532563361054100626, 10.80059781766745175, -2.638427012816831230 ) ) ;
#58653 = CARTESIAN_POINT ( 'NONE',  ( 17.20831665107776587, 57.88393115100078745, 7.208316651077764980 ) ) ;
#58654 = CARTESIAN_POINT ( 'NONE',  ( -0.8801773607110991993, 37.85535201082151247, -2.915334737309923874 ) ) ;
#58655 = DIRECTION ( 'NONE',  ( 1.000000000000000000, 0.000000000000000000, 0.000000000000000000 ) ) ;
#58656 = CARTESIAN_POINT ( 'NONE',  ( -45.94000000000001194, 103.9981609152045650, -5.961202730336927047 ) ) ;
#58657 = ORIENTED_EDGE ( 'NONE', *, *, #51744, .T. ) ;
#58658 = DIRECTION ( 'NONE',  ( -0.9970872288863208421, -0.07626964003977952655, 0.000000000000000000 ) ) ;
#58659 = CARTESIAN_POINT ( 'NONE',  ( 12.63842701281683922, 44.55059781766745175, -9.846743663894590881 ) ) ;
#58660 = VERTEX_POINT ( 'NONE', #79059 ) ;
#58661 = VERTEX_POINT ( 'NONE', #85591 ) ;
#58662 = CARTESIAN_POINT ( 'NONE',  ( -0.8801773607111009756, 63.06368534415484106, 1.068504757029289695E-15 ) ) ;
#58663 = CARTESIAN_POINT ( 'NONE',  ( -0.3689425029237881626, 27.42874883491397142, 10.36894250292379027 ) ) ;
#58664 = CARTESIAN_POINT ( 'NONE',  ( 22.26659068614894466, 13.88708216824730179, 7.082119434687054849 ) ) ;
#58665 = CARTESIAN_POINT ( 'NONE',  ( 15.44008868035555793, 66.39701867748817676, -9.422509992056140149 ) ) ;
#58666 = CARTESIAN_POINT ( 'NONE',  ( 2.917880565312950480, 55.97041550158063217, -12.26659068614894821 ) ) ;
#58667 = CARTESIAN_POINT ( 'NONE',  ( 17.20831665107776587, 64.13393115100079456, -7.208316651077762316 ) ) ;
#58668 = CARTESIAN_POINT ( 'NONE',  ( 1.472469842513823179, 31.42559781766745530, 4.923371831947296329 ) ) ;
#58669 = CARTESIAN_POINT ( 'NONE',  ( -10.91898769931337299, -97.58648078756493760, 4.000000000000000000 ) ) ;
#58671 = CARTESIAN_POINT ( 'NONE',  ( 13.43411237798106583, 2.665301336597086568, -12.81628187352647252 ) ) ;
#58670 = CARTESIAN_POINT ( 'NONE',  ( 17.96484262340118221, 29.93868534415484106, 7.964842623401181321 ) ) ;
#58672 = CARTESIAN_POINT ( 'NONE',  ( 20.36894250292379382, 18.67874883491397142, 10.36894250292379205 ) ) ;
#58673 = B_SPLINE_CURVE_WITH_KNOTS ( 'NONE', 3,
 ( #1725, #17702, #32179, #92695, #78685, #40192, #93182, #85694, #70699, #32677 ),
 .UNSPECIFIED., .F., .F.,
 ( 4, 3, 3, 4 ),
 ( 0.000000000000000000, 0.0006253016069560883442, 0.001250604074564952515, 0.002501455912506551308 ),
 .UNSPECIFIED. ) ;
#58674 = CARTESIAN_POINT ( 'NONE',  ( -4.164238869374099927, 47.01208216824729647, 3.795296366450308767 ) ) ;
#58675 = PRESENTATION_LAYER_ASSIGNMENT (  '', '', ( #21941 ) ) ;
#58676 = CARTESIAN_POINT ( 'NONE',  ( 19.42250999205614193, 20.14701867748817321, 5.440088680355555262 ) ) ;
#58677 = CARTESIAN_POINT ( 'NONE',  ( -0.2538888227782572504, 0.000000000000000000, 6.092555545977056397 ) ) ;
#58678 = CARTESIAN_POINT ( 'NONE',  ( 4.629999999999991900, 76.07179676972444327, -4.000000000000000000 ) ) ;
#58679 = CARTESIAN_POINT ( 'NONE',  ( -0.8801773607111009756, 43.06368534415484106, 1.068504757029289695E-15 ) ) ;
#58680 = CARTESIAN_POINT ( 'NONE',  ( 9.846743663894590881, -31.28273551566587685, -2.638427012816833894 ) ) ;
#58681 = ORIENTED_EDGE ( 'NONE', *, *, #33608, .T. ) ;
#58682 = VERTEX_POINT ( 'NONE', #18081 ) ;
#58683 = ORIENTED_EDGE ( 'NONE', *, *, #98365, .T. ) ;
#58684 = CARTESIAN_POINT ( 'NONE',  ( -4.164238869374099927, 42.01208216824728936, 3.795296366450308767 ) ) ;
#58685 = CARTESIAN_POINT ( 'NONE',  ( 17.20831665107776587, 49.13393115100078745, -7.208316651077762316 ) ) ;
#58686 = CARTESIAN_POINT ( 'NONE',  ( 0.5774900079438590739, 57.64701867748817676, -5.440088680355550821 ) ) ;
#58687 = EDGE_CURVE ( 'NONE', #13062, #88822, #38036, .T. ) ;
#58688 = CARTESIAN_POINT ( 'NONE',  ( -9.159723438033054776, -0.03417435944610275333, -10.91613331444555079 ) ) ;
#58689 = AXIS2_PLACEMENT_3D ( 'NONE', #41116, #36050, #68041 ) ;
#58690 = CARTESIAN_POINT ( 'NONE',  ( 0.5774900079438607392, 53.48035201082151247, 5.440088680355550821 ) ) ;
#58691 = CARTESIAN_POINT ( 'NONE',  ( 9.382169495545415572, 2.248634669930418273, -9.382169495545422677 ) ) ;
#58692 = ORIENTED_EDGE ( 'NONE', *, *, #16297, .T. ) ;
#58693 = CARTESIAN_POINT ( 'NONE',  ( -0.3689425029237881626, 17.42874883491397142, 10.36894250292379027 ) ) ;
#58694 = CARTESIAN_POINT ( 'NONE',  ( 16.40814093676323893, 25.79030133659708923, 11.09922568453595026 ) ) ;
#58695 = ORIENTED_EDGE ( 'NONE', *, *, #69650, .T. ) ;
#58696 = CARTESIAN_POINT ( 'NONE',  ( -2.816281873526471635, 38.91530133659708213, -3.434112377981056508 ) ) ;
#58697 = CIRCLE ( 'NONE', #15617, 1.999999999999996669 ) ;
#58698 = CARTESIAN_POINT ( 'NONE',  ( 19.84674366389459266, 33.30059781766744464, 2.638427012816836559 ) ) ;
#58699 = CARTESIAN_POINT ( 'NONE',  ( 4.559911319644449179, 13.89701867748817143, 9.422509992056141925 ) ) ;
#58700 = CARTESIAN_POINT ( 'NONE',  ( 22.81628187352647785, 51.41530133659708923, 3.434112377981063169 ) ) ;
#58701 = DIRECTION ( 'NONE',  ( 0.7808688094430307203, -0.6246950475544238435, 0.000000000000000000 ) ) ;
#58702 = CARTESIAN_POINT ( 'NONE',  ( 17.20831665107776587, 44.13393115100078745, -7.208316651077762316 ) ) ;
#58703 = VECTOR ( 'NONE', #88882, 1000.000000000000114 ) ;
#58704 = CIRCLE ( 'NONE', #7701, 14.49999999999999822 ) ;
#58705 = TOROIDAL_SURFACE ( 'NONE', #28379, 0.5000000000000000000, 0.2500000000000000000 ) ;
#58706 = CARTESIAN_POINT ( 'NONE',  ( -12.83294900548069961, 14.63595249122789177, 7.766300266068285829 ) ) ;
#58707 = EDGE_CURVE ( 'NONE', #87189, #39787, #95542, .T. ) ;
#58708 = CARTESIAN_POINT ( 'NONE',  ( 0.1922240491738519130, 3.188781737317406328, 6.500000000000000888 ) ) ;
#58709 = CARTESIAN_POINT ( 'NONE',  ( 10.14667048435135577, 15.00000000000000000, 10.35833375027046976 ) ) ;
#58710 = FACE_OUTER_BOUND ( 'NONE', #51168, .T. ) ;
#58711 = CARTESIAN_POINT ( 'NONE',  ( -0.1049300847420783223, 17.21697413083878914, -6.336235997365740502 ) ) ;
#58712 = CARTESIAN_POINT ( 'NONE',  ( 5.076628168052703671, 21.84226448433411960, 8.527530157486179263 ) ) ;
#58713 = EDGE_CURVE ( 'NONE', #189, #77019, #78082, .T. ) ;
#58714 = CARTESIAN_POINT ( 'NONE',  ( -1.099225684535947600, 18.70696800326375353, -6.408140936763238038 ) ) ;
#58715 = CARTESIAN_POINT ( 'NONE',  ( 8.606322355891288467, 3.856550154308941175E-16, 11.66967075398812703 ) ) ;
#58716 = ORIENTED_EDGE ( 'NONE', *, *, #9371, .F. ) ;
#58717 = CARTESIAN_POINT ( 'NONE',  ( -14.74963345907815793, 0.04922511925147218109, 0.3072669459659669866 ) ) ;
#58718 = CARTESIAN_POINT ( 'NONE',  ( -4.164238869374099927, 22.01208216824730357, 3.795296366450308767 ) ) ;
#58719 = CARTESIAN_POINT ( 'NONE',  ( 7.361572987183170547, 52.05059781766745175, 9.846743663894590881 ) ) ;
#58720 = CARTESIAN_POINT ( 'NONE',  ( 21.09922568453595559, 47.04030133659708923, -6.408140936763230044 ) ) ;
#58722 = CARTESIAN_POINT ( 'NONE',  ( 3.969999999999999751, 36.75000000000000000, 3.750000000000000000 ) ) ;
#58721 = CARTESIAN_POINT ( 'NONE',  ( 20.15039907845753220, 37.62777174578614847, -6.262539305110077947 ) ) ;
#58723 = CARTESIAN_POINT ( 'NONE',  ( 17.96484262340118221, 66.18868534415483396, -7.964842623401177768 ) ) ;
#58724 = CARTESIAN_POINT ( 'NONE',  ( -13.21236992757665973, 15.00000000000000000, -5.338143956176898186 ) ) ;
#58725 = CARTESIAN_POINT ( 'NONE',  ( 7.361572987183169658, 34.96726448433411605, -9.846743663894592657 ) ) ;
#58726 = CARTESIAN_POINT ( 'NONE',  ( -0.8801773607111008646, 38.27201867748816255, 2.915334737309923430 ) ) ;
#58727 = CARTESIAN_POINT ( 'NONE',  ( 19.38216949554541557, 42.24863466993041783, -9.382169495545420901 ) ) ;
#58728 = CARTESIAN_POINT ( 'NONE',  ( 18.52753015748617571, 33.09226448433411605, 4.923371831947298993 ) ) ;
#58729 = SHAPE_REPRESENTATION_RELATIONSHIP ( 'NONE' , 'NONE' ,  #57512, #32234 ) ;
#58730 = CARTESIAN_POINT ( 'NONE',  ( 8.880000000000022098, 80.32179676972448590, 4.000000000000000000 ) ) ;
#58731 = CARTESIAN_POINT ( 'NONE',  ( 19.42250999205614193, 50.14701867748817676, 5.440088680355555262 ) ) ;
#58732 = ORIENTED_EDGE ( 'NONE', *, *, #37027, .F. ) ;
#58733 = CARTESIAN_POINT ( 'NONE',  ( 7.084665262690076126, 69.10535201082151957, 10.88017736071109987 ) ) ;
#58734 = CARTESIAN_POINT ( 'NONE',  ( -0.8801773607110991993, 12.85535201082150358, -2.915334737309923874 ) ) ;
#58736 = CARTESIAN_POINT ( 'NONE',  ( 0.5774900079438590739, 47.64701867748817676, -5.440088680355550821 ) ) ;
#58735 = CARTESIAN_POINT ( 'NONE',  ( 12.63842701281683034, 62.46726448433410894, 9.846743663894596210 ) ) ;
#58737 = DIRECTION ( 'NONE',  ( 0.000000000000000000, 1.000000000000000000, 0.000000000000000000 ) ) ;
#58738 = CARTESIAN_POINT ( 'NONE',  ( -0.8801773607111009756, 63.06368534415484106, 1.068504757029289695E-15 ) ) ;
#58740 = CARTESIAN_POINT ( 'NONE',  ( 0.000000000000000000, 0.5000000000000004441, 0.000000000000000000 ) ) ;
#58739 = CARTESIAN_POINT ( 'NONE',  ( 15.44008868035555793, 21.39701867748817321, -9.422509992056140149 ) ) ;
#58741 = CARTESIAN_POINT ( 'NONE',  ( 10.00000000000000178, 2.258931151000784787, 9.846743663894594434 ) ) ;
#58742 = CARTESIAN_POINT ( 'NONE',  ( 0.1532563361054082862, 31.21726448433412315, 2.638427012816831674 ) ) ;
#58743 = CYLINDRICAL_SURFACE ( 'NONE', #66465, 1.500000000000001332 ) ;
#58744 = CARTESIAN_POINT ( 'NONE',  ( 12.26659068614894466, 4.720415501580636608, -7.082119434687053960 ) ) ;
#58745 = CARTESIAN_POINT ( 'NONE',  ( 19.84674366389459621, 53.50893115100078745, 7.409399052514197653E-17 ) ) ;
#58747 =( NAMED_UNIT ( * ) SI_UNIT ( $, .STERADIAN. ) SOLID_ANGLE_UNIT ( ) );
#58746 = CARTESIAN_POINT ( 'NONE',  ( 10.00000000000000000, 50.55374883491396787, -14.16423886937410082 ) ) ;
#58748 = CARTESIAN_POINT ( 'NONE',  ( 56.78206182523731371, 44.99999999999999289, 0.000000000000000000 ) ) ;
#58749 = CARTESIAN_POINT ( 'NONE',  ( -4.164238869374098151, 11.59541550158063217, -3.795296366450310543 ) ) ;
#58750 = CARTESIAN_POINT ( 'NONE',  ( 2.917880565312948704, 32.63708216824730357, 12.26659068614894643 ) ) ;
#58751 = CIRCLE ( 'NONE', #44331, 7.250000000000002665 ) ;
#58752 = CARTESIAN_POINT ( 'NONE',  ( 3.591859063236763294, 3.290301336597087012, -11.09922568453595026 ) ) ;
#58753 = EDGE_LOOP ( 'NONE', ( #22933, #79842, #22688, #86863, #69169, #96072, #20674, #91355, #59857, #7077, #16147, #45289 ) ) ;
#58754 = CARTESIAN_POINT ( 'NONE',  ( 20.88017736071110164, 20.35535201082150891, 2.915334737309930979 ) ) ;
#58755 = CARTESIAN_POINT ( 'NONE',  ( 5.076628168052704559, 50.17559781766745886, -8.527530157486179263 ) ) ;
#58757 = CARTESIAN_POINT ( 'NONE',  ( -13.86076281203281901, 90.90669854496248092, -7.842019570309373577 ) ) ;
#58756 = CARTESIAN_POINT ( 'NONE',  ( 6.204703633549690345, 0.7620821682473009062, -14.16423886937410259 ) ) ;
#58758 = CARTESIAN_POINT ( 'NONE',  ( 11.12471383767373467, 2.500000000000004885, 1.674288514525068328 ) ) ;
#58759 = CARTESIAN_POINT ( 'NONE',  ( 2.888614318722341867, 6.013933925505530435E-16, 14.33855829812825888 ) ) ;
#58760 = CARTESIAN_POINT ( 'NONE',  ( -2.816281873526473856, 19.12363466993042138, 9.499525473075851096E-16 ) ) ;
#58761 = CARTESIAN_POINT ( 'NONE',  ( 14.92337183194729633, 27.67559781766745530, 8.527530157486181039 ) ) ;
#58762 = ORIENTED_EDGE ( 'NONE', *, *, #61114, .T. ) ;
#58763 = CARTESIAN_POINT ( 'NONE',  ( 5.076628168052703671, 1.842264484334118047, 8.527530157486179263 ) ) ;
#58764 = DIRECTION ( 'NONE',  ( -0.7716245833877148907, 0.000000000000000000, -0.6360782202777701677 ) ) ;
#58765 = CARTESIAN_POINT ( 'NONE',  ( 15.44008868035555793, 6.397018677488171434, -9.422509992056140149 ) ) ;
#58766 = CARTESIAN_POINT ( 'NONE',  ( 2.035157376598824452, 13.68868534415483751, 7.964842623401179544 ) ) ;
#58767 = CARTESIAN_POINT ( 'NONE',  ( -4.164238869374098151, 41.59541550158061796, -3.795296366450310543 ) ) ;
#58768 = CARTESIAN_POINT ( 'NONE',  ( 4.559911319644449179, 47.23035201082150536, -9.422509992056141925 ) ) ;
#58769 = VECTOR ( 'NONE', #86160, 1000.000000000000000 ) ;
#58770 = CARTESIAN_POINT ( 'NONE',  ( 17.96484262340118221, 61.18868534415482685, -7.964842623401177768 ) ) ;
#58771 = CARTESIAN_POINT ( 'NONE',  ( 11.81378540890930751, -0.03417435944610275333, 7.968498874458199488 ) ) ;
#58772 = CARTESIAN_POINT ( 'NONE',  ( 18.18329248733323311, 17.60290668512020318, 6.499999999999984901 ) ) ;
#58773 = CARTESIAN_POINT ( 'NONE',  ( 7.361572987183169658, 24.96726448433412315, -9.846743663894592657 ) ) ;
#58774 = CARTESIAN_POINT ( 'NONE',  ( -0.6999999999999975131, 99.99999999999998579, 8.000000000000000000 ) ) ;
#58775 = CARTESIAN_POINT ( 'NONE',  ( 10.00000000000000178, 7.258931151000785675, 9.846743663894594434 ) ) ;
#58776 = CARTESIAN_POINT ( 'NONE',  ( 2.791683348922240793, 31.63393115100078745, 7.208316651077764092 ) ) ;
#58777 = CARTESIAN_POINT ( 'NONE',  ( -2.816281873526471635, -1.084698663402913210, -3.434112377981056508 ) ) ;
#58778 = CARTESIAN_POINT ( 'NONE',  ( 19.42250999205614548, 35.98035201082151247, -5.440088680355545492 ) ) ;
#58779 = COLOUR_RGB ( '', 0.09019608, 0.27058824, 0.51372549) ;
#58780 = AXIS2_PLACEMENT_3D ( 'NONE', #84033, #30519, #46514 ) ;
#58781 = VERTEX_POINT ( 'NONE', #26073 ) ;
#58782 = CARTESIAN_POINT ( 'NONE',  ( 0.6178305044545838731, 54.74863466993042493, 9.382169495545420901 ) ) ;
#58783 = CARTESIAN_POINT ( 'NONE',  ( 1.472469842513823179, 1.425597817667451528, 4.923371831947296329 ) ) ;
#58784 = CARTESIAN_POINT ( 'NONE',  ( 19.38216949554541557, 37.24863466993041783, -9.382169495545420901 ) ) ;
#58786 = CARTESIAN_POINT ( 'NONE',  ( 10.00000000000000178, 32.25893115100078745, 9.846743663894594434 ) ) ;
#58785 = CARTESIAN_POINT ( 'NONE',  ( 10.00000000000000000, 60.55374883491397497, -14.16423886937410082 ) ) ;
#58787 = CARTESIAN_POINT ( 'NONE',  ( 1.046131998950050157, 50.73810908735727310, 6.499999999999992006 ) ) ;
#58788 = DIRECTION ( 'NONE',  ( 0.000000000000000000, 0.000000000000000000, -1.000000000000000000 ) ) ;
#58789 = CARTESIAN_POINT ( 'NONE',  ( 17.08211943468705130, 48.47041550158063927, 12.26659068614894998 ) ) ;
#58790 = CARTESIAN_POINT ( 'NONE',  ( 1.472469842513823179, 41.42559781766745886, 4.923371831947296329 ) ) ;
#58791 = LINE ( 'NONE', #95822, #33086 ) ;
#58792 = CARTESIAN_POINT ( 'NONE',  ( 10.00000000000000000, 36.81368534415484106, -10.88017736071110342 ) ) ;
#58793 = CARTESIAN_POINT ( 'NONE',  ( -0.8801773607111008646, 63.27201867748817676, 2.915334737309923430 ) ) ;
#58794 = CARTESIAN_POINT ( 'NONE',  ( 0.000000000000000000, 15.00000000000000000, 0.000000000000000000 ) ) ;
#58795 = ORIENTED_EDGE ( 'NONE', *, *, #85590, .F. ) ;
#58796 = CARTESIAN_POINT ( 'NONE',  ( -1.099225684535947600, 48.70696800326375353, -6.408140936763238038 ) ) ;
#58797 = ORIENTED_EDGE ( 'NONE', *, *, #68556, .T. ) ;
#58798 = CARTESIAN_POINT ( 'NONE',  ( 20.88017736071110875, 65.77201867748817676, -2.915334737309920765 ) ) ;
#58799 = EDGE_LOOP ( 'NONE', ( #63695, #79616, #97863, #20327, #40110 ) ) ;
#58800 = CARTESIAN_POINT ( 'NONE',  ( -2.266590686148945544, 6.387082168247300906, -7.082119434687050408 ) ) ;
#58801 = CARTESIAN_POINT ( 'NONE',  ( 10.00000000000000178, 12.25893115100078568, 9.846743663894594434 ) ) ;
#58802 = EDGE_CURVE ( 'NONE', #55250, #36305, #66200, .T. ) ;
#58803 = CARTESIAN_POINT ( 'NONE',  ( 0.000000000000000000, 0.5000000000000004441, 0.000000000000000000 ) ) ;
#58804 = ORIENTED_EDGE ( 'NONE', *, *, #19990, .T. ) ;
#58805 = CARTESIAN_POINT ( 'NONE',  ( 12.91533473730993009, 16.60535201082150891, -10.88017736071109987 ) ) ;
#58806 = CARTESIAN_POINT ( 'NONE',  ( 19.10478245763055227, 60.10160829253886305, 5.990408912944262809 ) ) ;
#58807 = CARTESIAN_POINT ( 'NONE',  ( -0.3689425029237881626, 22.42874883491397142, 10.36894250292379027 ) ) ;
#58808 = EDGE_LOOP ( 'NONE', ( #50778, #70708, #45714, #80 ) ) ;
#58809 = CARTESIAN_POINT ( 'NONE',  ( 0.5774900079438590739, 27.64701867748817676, -5.440088680355550821 ) ) ;
#58810 = CARTESIAN_POINT ( 'NONE',  ( 7.361572987183169658, 54.96726448433413026, -9.846743663894592657 ) ) ;
#58811 = ORIENTED_EDGE ( 'NONE', *, *, #11731, .F. ) ;
#58812 = CARTESIAN_POINT ( 'NONE',  ( 17.20831665107776587, 57.88393115100078745, 7.208316651077764980 ) ) ;
#58813 = ORIENTED_EDGE ( 'NONE', *, *, #39658, .F. ) ;
#58814 = CARTESIAN_POINT ( 'NONE',  ( 4.559911319644449179, 62.23035201082150536, -9.422509992056141925 ) ) ;
#58815 = CARTESIAN_POINT ( 'NONE',  ( 10.00000000000000178, 62.25893115100078745, 9.846743663894594434 ) ) ;
#58816 = CARTESIAN_POINT ( 'NONE',  ( -1.099225684535947600, 34.54030133659708923, 6.408140936763237150 ) ) ;
#58817 = DIRECTION ( 'NONE',  ( -5.818595309480553908E-17, -1.000000000000000000, -0.000000000000000000 ) ) ;
#58818 = CARTESIAN_POINT ( 'NONE',  ( 1.472469842513823179, 6.425597817667451750, 4.923371831947296329 ) ) ;
#58819 = CARTESIAN_POINT ( 'NONE',  ( 2.035157376598824452, 23.68868534415484461, 7.964842623401179544 ) ) ;
#58820 = ORIENTED_EDGE ( 'NONE', *, *, #64585, .T. ) ;
#58821 = ADVANCED_FACE ( 'NONE', ( #33063 ), #4551, .T. ) ;
#58822 = CARTESIAN_POINT ( 'NONE',  ( 22.81628187352648496, 56.83196800326374643, -3.434112377981050290 ) ) ;
#58823 = CARTESIAN_POINT ( 'NONE',  ( 2.035157376598824452, 38.68868534415483396, 7.964842623401179544 ) ) ;
#58824 = LINE ( 'NONE', #67323, #77029 ) ;
#58825 = CARTESIAN_POINT ( 'NONE',  ( 19.38216949554541202, 35.99863466993041072, 9.382169495545424454 ) ) ;
#58826 = CARTESIAN_POINT ( 'NONE',  ( 4.559911319644449179, 52.23035201082151247, -9.422509992056141925 ) ) ;
#58827 = CARTESIAN_POINT ( 'NONE',  ( 12.63842701281683922, 59.55059781766744464, -9.846743663894590881 ) ) ;
#58828 = ORIENTED_EDGE ( 'NONE', *, *, #58455, .F. ) ;
#58829 = LINE ( 'NONE', #68324, #91055 ) ;
#58830 = B_SPLINE_CURVE_WITH_KNOTS ( 'NONE', 3,
 ( #23452, #92414, #15935, #47398, #68451, #23938 ),
 .UNSPECIFIED., .F., .F.,
 ( 4, 2, 4 ),
 ( 0.000000000000000000, 0.0002565770811491003721, 0.0005131541622982007441 ),
 .UNSPECIFIED. ) ;
#58831 = CARTESIAN_POINT ( 'NONE',  ( 12.63842701281683034, 17.46726448433411250, 9.846743663894596210 ) ) ;
#58832 = CARTESIAN_POINT ( 'NONE',  ( 19.38216949554541557, 2.248634669930420049, -9.382169495545420901 ) ) ;
#58834 = CARTESIAN_POINT ( 'NONE',  ( 5.054308323419867577, 70.51564955044841554, -5.000000000000000000 ) ) ;
#58833 = DIRECTION ( 'NONE',  ( -0.000000000000000000, -1.000000000000000000, -0.000000000000000000 ) ) ;
#58835 = CARTESIAN_POINT ( 'NONE',  ( -0.8801773607110991993, 22.85535201082150181, -2.915334737309923874 ) ) ;
#58836 = CARTESIAN_POINT ( 'NONE',  ( 0.1532563361054100626, 55.80059781766745175, -2.638427012816831230 ) ) ;
#58837 = CARTESIAN_POINT ( 'NONE',  ( -10.27090289957542169, 15.00000000000000711, 10.41235154178098199 ) ) ;
#58838 = CARTESIAN_POINT ( 'NONE',  ( -45.94000000000001194, 99.99999999999998579, -9.500000000000000000 ) ) ;
#58840 = CARTESIAN_POINT ( 'NONE',  ( 19.84674366389459621, 3.508931151000785231, 7.409399052514197653E-17 ) ) ;
#58839 = PRESENTATION_LAYER_ASSIGNMENT (  '', '', ( #2998 ) ) ;
#58841 = CARTESIAN_POINT ( 'NONE',  ( 7.361572987183169658, -0.03273551566588185635, -9.846743663894592657 ) ) ;
#58843 = VERTEX_POINT ( 'NONE', #87057 ) ;
#58842 = CARTESIAN_POINT ( 'NONE',  ( 21.09922568453595559, 2.040301336597086568, -6.408140936763230044 ) ) ;
#58844 = VECTOR ( 'NONE', #44419, 1000.000000000000000 ) ;
#58845 = CARTESIAN_POINT ( 'NONE',  ( 7.003840667633619788, 15.00000000000000888, 12.84073839985658161 ) ) ;
#58846 = CARTESIAN_POINT ( 'NONE',  ( -2.816281873526471635, 38.91530133659708213, -3.434112377981056508 ) ) ;
#58847 = CARTESIAN_POINT ( 'NONE',  ( 1.472469842513823179, 35.59226448433412315, -4.923371831947296329 ) ) ;
#58848 = CARTESIAN_POINT ( 'NONE',  ( -8.000343251535921851, 84.06932101904432386, -3.750000000000000000 ) ) ;
#58849 = CARTESIAN_POINT ( 'NONE',  ( 24.16423886937410614, 64.51208216824728936, -3.795296366450302550 ) ) ;
#58850 = CARTESIAN_POINT ( 'NONE',  ( 5.076628168052704559, 35.17559781766745175, -8.527530157486179263 ) ) ;
#58851 = PLANE ( 'NONE',  #76046 ) ;
#58852 = CARTESIAN_POINT ( 'NONE',  ( 15.44008868035555260, 9.730352010821505360, 9.422509992056143702 ) ) ;
#58853 = CARTESIAN_POINT ( 'NONE',  ( -11.12340613366069419, 89.95527085539235657, -6.571742733942876669 ) ) ;
#58854 = CARTESIAN_POINT ( 'NONE',  ( -0.8801773607110991993, 17.85535201082150536, -2.915334737309923874 ) ) ;
#58855 = CARTESIAN_POINT ( 'NONE',  ( 17.08211943468705130, 53.47041550158063217, 12.26659068614894998 ) ) ;
#58857 = CARTESIAN_POINT ( 'NONE',  ( -10.91036564011048426, 0.2301503799940542716, 10.20716212663429801 ) ) ;
#58856 = CARTESIAN_POINT ( 'NONE',  ( 24.16423886937410614, 54.30374883491396787, 8.672049930838204340E-16 ) ) ;
#58858 = PRESENTATION_STYLE_ASSIGNMENT (( #94400 ) ) ;
#58859 = EDGE_CURVE ( 'NONE', #4978, #79846, #81506, .T. ) ;
#58860 = CIRCLE ( 'NONE', #8001, 14.49999999999999822 ) ;
#58861 = CARTESIAN_POINT ( 'NONE',  ( 12.63842701281683034, 12.46726448433411782, 9.846743663894596210 ) ) ;
#58862 = CARTESIAN_POINT ( 'NONE',  ( 17.20831665107776587, 64.13393115100079456, -7.208316651077762316 ) ) ;
#58863 = VERTEX_POINT ( 'NONE', #14965 ) ;
#58864 = CARTESIAN_POINT ( 'NONE',  ( 0.5774900079438590739, 47.64701867748817676, -5.440088680355550821 ) ) ;
#58865 = CARTESIAN_POINT ( 'NONE',  ( 0.2751277870542967463, 70.00000000000000000, -6.000000000000000000 ) ) ;
#58866 = ADVANCED_FACE ( 'NONE', ( #52933 ), #75937, .T. ) ;
#58867 = CARTESIAN_POINT ( 'NONE',  ( 7.361572987183169658, 54.96726448433413026, -9.846743663894592657 ) ) ;
#58868 = CARTESIAN_POINT ( 'NONE',  ( 0.000000000000000000, -97.00000000000000000, -3.750000000000000000 ) ) ;
#58869 = CARTESIAN_POINT ( 'NONE',  ( -8.000000000000000000, 80.07179676972448590, -4.250000000000000000 ) ) ;
#58870 = CARTESIAN_POINT ( 'NONE',  ( 13.34343830728404079, 0.5000000000000004441, -6.852200678592596184 ) ) ;
#58871 = ORIENTED_EDGE ( 'NONE', *, *, #75055, .F. ) ;
#58872 = CARTESIAN_POINT ( 'NONE',  ( 1.472469842513823179, 16.42559781766745175, 4.923371831947296329 ) ) ;
#58873 = LINE ( 'NONE', #86069, #49594 ) ;
#58874 = ORIENTED_EDGE ( 'NONE', *, *, #33056, .F. ) ;
#58875 = CARTESIAN_POINT ( 'NONE',  ( 17.08211943468705840, 35.13708216824730357, -12.26659068614894466 ) ) ;
#58876 = CARTESIAN_POINT ( 'NONE',  ( 0.1532563361054083140, 1.008931151000784787, 1.131784320476157264E-15 ) ) ;
#58878 = DIRECTION ( 'NONE',  ( -0.8320502943378437211, 0.5547001962252290364, 0.000000000000000000 ) ) ;
#58877 = CARTESIAN_POINT ( 'NONE',  ( -7.124975165242272368, -78.82169502743931844, -2.750000000000000000 ) ) ;
#58879 = CARTESIAN_POINT ( 'NONE',  ( -0.8801773607110991993, 32.85535201082151247, -2.915334737309923874 ) ) ;
#58880 = CARTESIAN_POINT ( 'NONE',  ( -2.816281873526471635, 38.91530133659708213, -3.434112377981056508 ) ) ;
#58881 = CARTESIAN_POINT ( 'NONE',  ( -0.8801773607111008646, 3.272018677488171434, 2.915334737309923430 ) ) ;
#58882 = CARTESIAN_POINT ( 'NONE',  ( 10.00000000000000178, 35.37363466993042493, 12.81628187352647608 ) ) ;
#58883 = FACE_OUTER_BOUND ( 'NONE', #12511, .T. ) ;
#58884 = EDGE_LOOP ( 'NONE', ( #65869, #50821, #49605 ) ) ;
#58885 = CARTESIAN_POINT ( 'NONE',  ( -2.962741594152892510, 15.00000000000000000, -13.93860331045676837 ) ) ;
#58886 = EDGE_CURVE ( 'NONE', #38526, #3732, #2843, .T. ) ;
#58887 = CARTESIAN_POINT ( 'NONE',  ( -8.922167142635604620, 75.09950301435408448, -3.000000000000000000 ) ) ;
#58888 = CARTESIAN_POINT ( 'NONE',  ( -4.164238869374098151, 31.59541550158063927, -3.795296366450310543 ) ) ;
#58889 = CARTESIAN_POINT ( 'NONE',  ( -4.164238869374098151, 6.595415501580634832, -3.795296366450310543 ) ) ;
#58890 = CARTESIAN_POINT ( 'NONE',  ( 4.559911319644449179, 12.23035201082150536, -9.422509992056141925 ) ) ;
#58891 = CARTESIAN_POINT ( 'NONE',  ( 20.88017736071110519, 20.56368534415484106, 2.639326808657452039E-16 ) ) ;
#58892 = CARTESIAN_POINT ( 'NONE',  ( 0.2751277870542911952, 53.21833443783938122, 6.499999999999992006 ) ) ;
#58893 = VECTOR ( 'NONE', #79188, 1000.000000000000114 ) ;
#58894 = CARTESIAN_POINT ( 'NONE',  ( 2.815433093577122126, 15.00000000000000000, -14.73340885523749932 ) ) ;
#58895 = CARTESIAN_POINT ( 'NONE',  ( 15.44008868035555260, 59.73035201082151247, 9.422509992056143702 ) ) ;
#58896 = CARTESIAN_POINT ( 'NONE',  ( 19.42250999205614193, 45.14701867748817676, 5.440088680355555262 ) ) ;
#58897 = CARTESIAN_POINT ( 'NONE',  ( -2.816281873526473856, 14.12363466993041961, 9.499525473075851096E-16 ) ) ;
#58898 = DIRECTION ( 'NONE',  ( 0.000000000000000000, 0.000000000000000000, -1.000000000000000000 ) ) ;
#58899 = CARTESIAN_POINT ( 'NONE',  ( -10.00000000000000000, 82.00000000000000000, 9.500000000000000000 ) ) ;
#58900 = CARTESIAN_POINT ( 'NONE',  ( 7.361572987183170547, 22.05059781766745530, 9.846743663894590881 ) ) ;
#58901 = CARTESIAN_POINT ( 'NONE',  ( 0.5600000000000083800, 105.0000000000000000, 5.000000000000000000 ) ) ;
#58902 = CARTESIAN_POINT ( 'NONE',  ( 20.88017736071110164, 45.35535201082149115, 2.915334737309930979 ) ) ;
#58903 = CARTESIAN_POINT ( 'NONE',  ( -1.099225684535947600, 4.540301336597087456, 6.408140936763237150 ) ) ;
#58904 =( NAMED_UNIT ( * ) PLANE_ANGLE_UNIT ( ) SI_UNIT ( $, .RADIAN. ) );
#58905 = CARTESIAN_POINT ( 'NONE',  ( 19.84674366389459266, 23.30059781766745530, 2.638427012816836559 ) ) ;
#58906 = CARTESIAN_POINT ( 'NONE',  ( -2.816281873526473856, 54.33196800326376064, 3.434112377981055619 ) ) ;
#58907 = CARTESIAN_POINT ( 'NONE',  ( 5.076628168052704559, 20.17559781766745175, -8.527530157486179263 ) ) ;
#58908 = ORIENTED_EDGE ( 'NONE', *, *, #13929, .F. ) ;
#58909 = CARTESIAN_POINT ( 'NONE',  ( 2.917880565312950480, 10.97041550158063572, -12.26659068614894821 ) ) ;
#58910 = DIRECTION ( 'NONE',  ( 0.000000000000000000, 1.000000000000000000, 0.000000000000000000 ) ) ;
#58911 = CARTESIAN_POINT ( 'NONE',  ( 7.084665262690076126, 24.10535201082150181, 10.88017736071109987 ) ) ;
#58912 = CARTESIAN_POINT ( 'NONE',  ( 22.26659068614895176, 34.72041550158063927, -7.082119434687042414 ) ) ;
#58913 = CARTESIAN_POINT ( 'NONE',  ( 5.076628168052704559, 30.17559781766745175, -8.527530157486179263 ) ) ;
#58914 = CIRCLE ( 'NONE', #39795, 14.49999999999999822 ) ;
#58915 = CARTESIAN_POINT ( 'NONE',  ( 17.96484262340118221, 16.18868534415483396, -7.964842623401177768 ) ) ;
#58916 = CARTESIAN_POINT ( 'NONE',  ( 10.00000000000000178, 4.313685344154837509, 10.88017736071110342 ) ) ;
#58917 = ORIENTED_EDGE ( 'NONE', *, *, #32045, .T. ) ;
#58918 = CARTESIAN_POINT ( 'NONE',  ( 19.42250999205614193, 20.14701867748817321, 5.440088680355555262 ) ) ;
#58919 = CARTESIAN_POINT ( 'NONE',  ( 16.40814093676324603, 52.45696800326375353, -11.09922568453594671 ) ) ;
#58920 = EDGE_CURVE ( 'NONE', #31636, #87937, #58830, .T. ) ;
#58921 = CARTESIAN_POINT ( 'NONE',  ( -0.8801773607111008646, 33.27201867748817676, 2.915334737309923430 ) ) ;
#58923 = CARTESIAN_POINT ( 'NONE',  ( 2.035157376598822676, 37.43868534415484106, -7.964842623401177768 ) ) ;
#58922 = CARTESIAN_POINT ( 'NONE',  ( -13.78891971893199830, 0.5000000000000004441, -5.904717858191724567 ) ) ;
#58924 = ORIENTED_EDGE ( 'NONE', *, *, #76910, .F. ) ;
#58925 = CARTESIAN_POINT ( 'NONE',  ( 10.00000000000000000, 54.75893115100078745, -9.846743663894594434 ) ) ;
#58926 = CARTESIAN_POINT ( 'NONE',  ( 19.42250999205614193, 35.14701867748816966, 5.440088680355555262 ) ) ;
#58927 = CARTESIAN_POINT ( 'NONE',  ( 5.076628168052704559, 65.17559781766745175, -8.527530157486179263 ) ) ;
#58928 = PRESENTATION_STYLE_ASSIGNMENT (( #81919 ) ) ;
#58929 = CARTESIAN_POINT ( 'NONE',  ( 3.591859063236761518, 64.95696800326376774, 11.09922568453594849 ) ) ;
#58930 = CARTESIAN_POINT ( 'NONE',  ( 19.72487221294570858, 70.00000000000000000, 6.000000000000000000 ) ) ;
#58931 = CARTESIAN_POINT ( 'NONE',  ( 24.16423886937410614, 39.51208216824731068, -3.795296366450302550 ) ) ;
#58932 = CARTESIAN_POINT ( 'NONE',  ( 0.5774900079438590739, 57.64701867748817676, -5.440088680355550821 ) ) ;
#58933 = ADVANCED_FACE ( 'NONE', ( #98972 ), #8429, .T. ) ;
#58934 = CARTESIAN_POINT ( 'NONE',  ( 18.72515096720579209, 51.07228050351030646, -6.499999999999869438 ) ) ;
#58935 = CARTESIAN_POINT ( 'NONE',  ( -3.799999999999998934, 1.639999999999999014, 0.000000000000000000 ) ) ;
#58936 = CARTESIAN_POINT ( 'NONE',  ( 18.52753015748617571, 53.09226448433412315, 4.923371831947298993 ) ) ;
#58937 = CARTESIAN_POINT ( 'NONE',  ( 14.92337183194729988, 4.342264484334117824, -8.527530157486177487 ) ) ;
#58938 = CARTESIAN_POINT ( 'NONE',  ( 19.84674366389459266, 23.71726448433412315, -2.638427012816827677 ) ) ;
#58939 = VERTEX_POINT ( 'NONE', #90929 ) ;
#58940 = CARTESIAN_POINT ( 'NONE',  ( 0.1532563361054082862, 16.21726448433411960, 2.638427012816831674 ) ) ;
#58941 = CARTESIAN_POINT ( 'NONE',  ( 12.81628187352647608, -13.37636533006957684, -2.602085213965210642E-15 ) ) ;
#58942 = CARTESIAN_POINT ( 'NONE',  ( 7.084665262690076126, 32.02201867748816966, -10.88017736071110164 ) ) ;
#58943 = CARTESIAN_POINT ( 'NONE',  ( 19.84674366389459621, 18.50893115100078745, 7.409399052514197653E-17 ) ) ;
#58944 = CARTESIAN_POINT ( 'NONE',  ( 3.591859063236761518, 9.956968003263753531, 11.09922568453594849 ) ) ;
#58945 = CARTESIAN_POINT ( 'NONE',  ( -0.8801773607111008646, 58.27201867748816966, 2.915334737309923430 ) ) ;
#58947 = CARTESIAN_POINT ( 'NONE',  ( -2.816281873526473856, 54.12363466993041783, 9.499525473075851096E-16 ) ) ;
#58946 = CARTESIAN_POINT ( 'NONE',  ( 4.559911319644449179, 28.89701867748817321, 9.422509992056141925 ) ) ;
#58948 = CARTESIAN_POINT ( 'NONE',  ( 10.00000000000000000, 50.55374883491396787, -14.16423886937410082 ) ) ;
#58949 = CIRCLE ( 'NONE', #26970, 0.2500000000000002220 ) ;
#58950 = EDGE_CURVE ( 'NONE', #59946, #74297, #83247, .T. ) ;
#58951 = CARTESIAN_POINT ( 'NONE',  ( 10.00000000000000178, 65.37363466993042493, 12.81628187352647608 ) ) ;
#58952 = ORIENTED_EDGE ( 'NONE', *, *, #62755, .T. ) ;
#58953 = CARTESIAN_POINT ( 'NONE',  ( 2.791683348922240793, 66.63393115100079456, 7.208316651077764092 ) ) ;
#58954 = CARTESIAN_POINT ( 'NONE',  ( 15.44008868035555793, 6.397018677488170546, -9.422509992056140149 ) ) ;
#58955 = CARTESIAN_POINT ( 'NONE',  ( 17.96484262340118221, 51.18868534415483396, -7.964842623401177768 ) ) ;
#58957 = EDGE_CURVE ( 'NONE', #1795, #57881, #16922, .T. ) ;
#58956 = CARTESIAN_POINT ( 'NONE',  ( 14.92337183194729988, 64.34226448433412315, -8.527530157486177487 ) ) ;
#58958 = ORIENTED_EDGE ( 'NONE', *, *, #15600, .T. ) ;
#58960 = CARTESIAN_POINT ( 'NONE',  ( -3.999999999999999112, 78.07179676972445748, 6.250000000000000000 ) ) ;
#58959 = CARTESIAN_POINT ( 'NONE',  ( 19.84674366389459266, 18.71726448433411960, -2.638427012816827677 ) ) ;
#58961 = CARTESIAN_POINT ( 'NONE',  ( 11.92686044187656336, 6.979976035794169142, 3.195792623639526653 ) ) ;
#58962 = AXIS2_PLACEMENT_3D ( 'NONE', #37152, #38143, #60121 ) ;
#58963 = CARTESIAN_POINT ( 'NONE',  ( -0.8801773607111008646, 58.27201867748816966, 2.915334737309923430 ) ) ;
#58964 = CARTESIAN_POINT ( 'NONE',  ( 0.1532563361054100626, 35.80059781766745175, -2.638427012816831230 ) ) ;
#58965 = CARTESIAN_POINT ( 'NONE',  ( 19.84674366389459621, 18.50893115100078745, 7.409399052514197653E-17 ) ) ;
#58966 = CARTESIAN_POINT ( 'NONE',  ( 7.361572987183170547, 12.05059781766744997, 9.846743663894590881 ) ) ;
#58967 = CARTESIAN_POINT ( 'NONE',  ( 17.39651004071841456, 64.08210964143329136, -6.500000000000001776 ) ) ;
#58969 = CARTESIAN_POINT ( 'NONE',  ( -39.29878048780484789, 31.43902439024384776, -8.000000000000000000 ) ) ;
#58968 = CARTESIAN_POINT ( 'NONE',  ( 7.084665262690076126, 64.10535201082150536, 10.88017736071109987 ) ) ;
#58971 = ORIENTED_EDGE ( 'NONE', *, *, #40889, .F. ) ;
#58970 = CARTESIAN_POINT ( 'NONE',  ( 2.791683348922240793, 31.63393115100078745, 7.208316651077764092 ) ) ;
#58972 = LINE ( 'NONE', #73968, #88530 ) ;
#58973 = CARTESIAN_POINT ( 'NONE',  ( 7.361572987183170547, 62.05059781766745886, 9.846743663894590881 ) ) ;
#58974 = CARTESIAN_POINT ( 'NONE',  ( 0.4195498155886339120, 0.5000000000000038858, 9.500000000000000000 ) ) ;
#58975 = CARTESIAN_POINT ( 'NONE',  ( -4.164238869374099039, 16.80374883491396787, 8.674139862899312516E-16 ) ) ;
#58976 = CARTESIAN_POINT ( 'NONE',  ( 11.59608414876342408, 0.2306972965111887541, 9.421724210956368140 ) ) ;
#58977 = CARTESIAN_POINT ( 'NONE',  ( 2.917880565312950480, 15.97041550158063217, -12.26659068614894821 ) ) ;
#58978 = CARTESIAN_POINT ( 'NONE',  ( 13.79529636645031943, 50.34541550158064638, -14.16423886937409904 ) ) ;
#58979 = CARTESIAN_POINT ( 'NONE',  ( -4.164238869374099927, 2.012082168247300906, 3.795296366450308767 ) ) ;
#58980 = CARTESIAN_POINT ( 'NONE',  ( 20.36894250292379738, 14.92874883491396432, -10.36894250292379027 ) ) ;
#58981 = CARTESIAN_POINT ( 'NONE',  ( -0.8801773607111008646, 53.27201867748816966, 2.915334737309923430 ) ) ;
#58982 = CYLINDRICAL_SURFACE ( 'NONE', #35583, 3.940000000000000835 ) ;
#58983 = EDGE_LOOP ( 'NONE', ( #2839, #69135, #756, #64094 ) ) ;
#58984 = CARTESIAN_POINT ( 'NONE',  ( 0.1532563361054100626, 25.80059781766744820, -2.638427012816831230 ) ) ;
#58986 = CARTESIAN_POINT ( 'NONE',  ( 18.52753015748618282, 28.92559781766745175, -4.923371831947291888 ) ) ;
#58985 = CARTESIAN_POINT ( 'NONE',  ( 15.44008868035555793, 66.39701867748817676, -9.422509992056140149 ) ) ;
#58987 = CARTESIAN_POINT ( 'NONE',  ( 2.035157376598822676, 12.43868534415483751, -7.964842623401177768 ) ) ;
#58988 = CARTESIAN_POINT ( 'NONE',  ( 10.00000000000000178, 55.37363466993042493, 12.81628187352647608 ) ) ;
#58989 = CARTESIAN_POINT ( 'NONE',  ( 14.92337183194729633, 52.67559781766745175, 8.527530157486181039 ) ) ;
#58990 = CARTESIAN_POINT ( 'NONE',  ( 18.00000000000000000, 77.34875458013688387, 4.131905931794615405 ) ) ;
#58991 = EDGE_CURVE ( 'NONE', #73794, #25822, #36453, .T. ) ;
#58992 = CARTESIAN_POINT ( 'NONE',  ( 14.92337183194729633, 27.67559781766745530, 8.527530157486181039 ) ) ;
#58993 = CARTESIAN_POINT ( 'NONE',  ( 3.591859063236761518, 44.95696800326376064, 11.09922568453594849 ) ) ;
#58994 = CARTESIAN_POINT ( 'NONE',  ( 14.16423886937410082, -20.48791783175269643, -3.795296366450314096 ) ) ;
#58995 = CARTESIAN_POINT ( 'NONE',  ( 10.00000000000000178, 39.31368534415484106, 10.88017736071110342 ) ) ;
#58996 = CARTESIAN_POINT ( 'NONE',  ( 18.52753015748618282, 38.92559781766745175, -4.923371831947291888 ) ) ;
#58997 = CARTESIAN_POINT ( 'NONE',  ( 10.00000000000000000, 20.55374883491396787, -14.16423886937410082 ) ) ;
#58998 = VERTEX_POINT ( 'NONE', #29931 ) ;
#58999 = CARTESIAN_POINT ( 'NONE',  ( 17.08211943468705130, 3.470415501580634388, 12.26659068614894998 ) ) ;
#59000 = CARTESIAN_POINT ( 'NONE',  ( 19.42250999205614548, 50.98035201082151247, -5.440088680355545492 ) ) ;
#59001 = CARTESIAN_POINT ( 'NONE',  ( 19.42250999205614193, 65.14701867748817676, 5.440088680355555262 ) ) ;
#59002 = CARTESIAN_POINT ( 'NONE',  ( 24.16423886937410614, 49.51208216824730357, -3.795296366450302550 ) ) ;
#59003 = CARTESIAN_POINT ( 'NONE',  ( 10.00000000000000178, 62.25893115100078745, 9.846743663894594434 ) ) ;
#59004 = DIRECTION ( 'NONE',  ( 0.000000000000000000, -1.000000000000000000, 0.000000000000000000 ) ) ;
#59005 = CARTESIAN_POINT ( 'NONE',  ( 4.559911319644449179, 53.89701867748817676, 9.422509992056141925 ) ) ;
#59006 = CARTESIAN_POINT ( 'NONE',  ( -3.521020805652876007, -6.414291667507516337, -2.500000000000000000 ) ) ;
#59007 = CARTESIAN_POINT ( 'NONE',  ( -1.099225684535947600, 24.54030133659708923, 6.408140936763237150 ) ) ;
#59008 = CARTESIAN_POINT ( 'NONE',  ( 13.43411237798106583, 2.665301336597086568, -12.81628187352647252 ) ) ;
#59009 = CARTESIAN_POINT ( 'NONE',  ( -10.88017736071110164, 27.85535201082149470, -2.915334737309917212 ) ) ;
#59010 = CARTESIAN_POINT ( 'NONE',  ( 7.084665262690076126, 19.10535201082150181, 10.88017736071109987 ) ) ;
#59011 = CARTESIAN_POINT ( 'NONE',  ( 17.96484262340118221, 11.18868534415484106, -7.964842623401177768 ) ) ;
#59012 = VERTEX_POINT ( 'NONE', #53929 ) ;
#59013 =( GEOMETRIC_REPRESENTATION_CONTEXT ( 3 ) GLOBAL_UNCERTAINTY_ASSIGNED_CONTEXT ( ( #82127 ) ) GLOBAL_UNIT_ASSIGNED_CONTEXT ( ( #2504, #63933, #94447 ) ) REPRESENTATION_CONTEXT ( 'NONE', 'WORKASPACE' ) );
#59014 = DIRECTION ( 'NONE',  ( 8.673617379884027583E-16, 1.000000000000000000, 0.000000000000000000 ) ) ;
#59015 = CARTESIAN_POINT ( 'NONE',  ( 1.472469842513823179, 15.59226448433411960, -4.923371831947296329 ) ) ;
#59016 = CARTESIAN_POINT ( 'NONE',  ( 14.92337183194729633, 37.67559781766745175, 8.527530157486181039 ) ) ;
#59017 = CARTESIAN_POINT ( 'NONE',  ( 15.44008868035555793, 41.39701867748817676, -9.422509992056140149 ) ) ;
#59018 = CARTESIAN_POINT ( 'NONE',  ( -1.099225684535947600, 13.70696800326375353, -6.408140936763238038 ) ) ;
#59020 = CARTESIAN_POINT ( 'NONE',  ( 4.219999999999999751, 9.750000000000000000, -4.000000000000000000 ) ) ;
#59019 = CARTESIAN_POINT ( 'NONE',  ( 20.88017736071110519, 30.56368534415484106, 2.639326808657452039E-16 ) ) ;
#59021 = EDGE_CURVE ( 'NONE', #68558, #76972, #52436, .T. ) ;
#59022 = CARTESIAN_POINT ( 'NONE',  ( -13.82192141328803991, 15.00000000000000000, -4.382292601468865456 ) ) ;
#59023 = CARTESIAN_POINT ( 'NONE',  ( 21.09922568453595559, 57.04030133659708923, -6.408140936763230044 ) ) ;
#59024 = ORIENTED_EDGE ( 'NONE', *, *, #13155, .T. ) ;
#59025 = CARTESIAN_POINT ( 'NONE',  ( 12.91533473730992121, 64.52201867748817676, 10.88017736071110164 ) ) ;
#59027 = CARTESIAN_POINT ( 'NONE',  ( 20.36894250292379382, 3.678748834913967869, 10.36894250292379205 ) ) ;
#59026 = CARTESIAN_POINT ( 'NONE',  ( 6.565887622018943937, 28.08196800326375353, -12.81628187352647608 ) ) ;
#59028 = CARTESIAN_POINT ( 'NONE',  ( 5.076628168052703671, 1.842264484334118047, 8.527530157486179263 ) ) ;
#59029 = CARTESIAN_POINT ( 'NONE',  ( 4.559911319644449179, 42.23035201082151247, -9.422509992056141925 ) ) ;
#59030 = CARTESIAN_POINT ( 'NONE',  ( 12.63842701281683034, 62.46726448433410894, 9.846743663894596210 ) ) ;
#59031 = CARTESIAN_POINT ( 'NONE',  ( 14.92337183194729988, 59.34226448433412315, -8.527530157486177487 ) ) ;
#59032 = AXIS2_PLACEMENT_3D ( 'NONE', #6855, #14868, #32294 ) ;
#59033 = CARTESIAN_POINT ( 'NONE',  ( 1.472469842513823179, 15.59226448433411960, -4.923371831947296329 ) ) ;
#59034 = CARTESIAN_POINT ( 'NONE',  ( 0.5774900079438590739, 57.64701867748817676, -5.440088680355550821 ) ) ;
#59035 = DIRECTION ( 'NONE',  ( -0.9996573249755572599, 0.000000000000000000, -0.02617694830787627158 ) ) ;
#59036 = CARTESIAN_POINT ( 'NONE',  ( 17.08211943468705130, 23.47041550158063572, 12.26659068614894998 ) ) ;
#59037 = CARTESIAN_POINT ( 'NONE',  ( 12.11353679309438824, 0.04962889481942911463, -8.421373815019629561 ) ) ;
#59038 = CARTESIAN_POINT ( 'NONE',  ( 11.40652922194187369, -69.23660773168047911, -3.749999999999999556 ) ) ;
#59039 = VERTEX_POINT ( 'NONE', #84437 ) ;
#59040 = VERTEX_POINT ( 'NONE', #7947 ) ;
#59041 = CARTESIAN_POINT ( 'NONE',  ( -4.164238869374099927, 62.01208216824728936, 3.795296366450308767 ) ) ;
#59042 = CARTESIAN_POINT ( 'NONE',  ( 10.00000000000000178, 63.05374883491396076, 14.16423886937410082 ) ) ;
#59043 = CARTESIAN_POINT ( 'NONE',  ( 5.076628168052704559, 30.17559781766745175, -8.527530157486179263 ) ) ;
#59044 = CARTESIAN_POINT ( 'NONE',  ( 10.00000000000000178, 30.37363466993042138, 12.81628187352647608 ) ) ;
#59045 = FILL_AREA_STYLE_COLOUR ( '', #47558 ) ;
#59046 = DIRECTION ( 'NONE',  ( -0.4617486132350285266, 0.000000000000000000, -0.8870108331782246003 ) ) ;
#59047 = CARTESIAN_POINT ( 'NONE',  ( 10.00000000000000178, 9.313685344154839285, 10.88017736071110342 ) ) ;
#59048 = CARTESIAN_POINT ( 'NONE',  ( 10.00000000000000178, 53.05374883491396787, 14.16423886937410082 ) ) ;
#59049 = ADVANCED_FACE ( 'NONE', ( #59274 ), #25327, .T. ) ;
#59050 = EDGE_CURVE ( 'NONE', #21240, #15967, #1355, .T. ) ;
#59051 = CARTESIAN_POINT ( 'NONE',  ( 2.791683348922237240, 30.38393115100078390, -7.208316651077763204 ) ) ;
#59052 = DIRECTION ( 'NONE',  ( 0.9975640502598257520, -0.06975647374410356982, 0.000000000000000000 ) ) ;
#59053 = CARTESIAN_POINT ( 'NONE',  ( 1.472469842513823179, 5.592264484334118713, -4.923371831947296329 ) ) ;
#59054 = CARTESIAN_POINT ( 'NONE',  ( 18.52753015748617571, 3.092264484334118269, 4.923371831947298993 ) ) ;
#59055 = CARTESIAN_POINT ( 'NONE',  ( 4.923371831947301658, 22.67559781766745175, 8.527530157486175710 ) ) ;
#59056 = VERTEX_POINT ( 'NONE', #20799 ) ;
#59057 = ORIENTED_EDGE ( 'NONE', *, *, #18789, .F. ) ;
#59058 = DIRECTION ( 'NONE',  ( 0.000000000000000000, 1.000000000000000000, 0.000000000000000000 ) ) ;
#59059 = VERTEX_POINT ( 'NONE', #36287 ) ;
#59061 = CARTESIAN_POINT ( 'NONE',  ( -0.8801773607110991993, 27.85535201082150181, -2.915334737309923874 ) ) ;
#59060 = CARTESIAN_POINT ( 'NONE',  ( -0.8801773607111008646, 18.27201867748817321, 2.915334737309923430 ) ) ;
#59063 = CARTESIAN_POINT ( 'NONE',  ( 16.40814093676323893, 20.79030133659708923, 11.09922568453595026 ) ) ;
#59062 = CARTESIAN_POINT ( 'NONE',  ( 1.472469842513823179, 66.42559781766745175, 4.923371831947296329 ) ) ;
#59064 = CARTESIAN_POINT ( 'NONE',  ( 16.40814093676324603, 32.45696800326375353, -11.09922568453594671 ) ) ;
#59065 = EDGE_LOOP ( 'NONE', ( #42584, #33015, #61264, #19820 ) ) ;
#59066 = CARTESIAN_POINT ( 'NONE',  ( 14.92337183194729633, 32.67559781766745175, 8.527530157486181039 ) ) ;
#59067 = CARTESIAN_POINT ( 'NONE',  ( -2.266590686148945544, 67.22041550158063217, 7.082119434687048631 ) ) ;
#59068 = ORIENTED_EDGE ( 'NONE', *, *, #57378, .F. ) ;
#59069 = ADVANCED_FACE ( 'NONE', ( #66276 ), #89773, .T. ) ;
#59070 = CARTESIAN_POINT ( 'NONE',  ( -4.164238869374099039, 66.80374883491396076, 8.674139862899312516E-16 ) ) ;
#59071 = EDGE_LOOP ( 'NONE', ( #96612, #29364, #38099, #76891 ) ) ;
#59072 = CARTESIAN_POINT ( 'NONE',  ( 12.91533473730992121, 49.52201867748817676, 10.88017736071110164 ) ) ;
#59073 = CARTESIAN_POINT ( 'NONE',  ( 4.559911319644449179, 53.89701867748817676, 9.422509992056141925 ) ) ;
#59074 = CARTESIAN_POINT ( 'NONE',  ( 20.88017736071110875, 55.77201867748816966, -2.915334737309920765 ) ) ;
#59075 = CARTESIAN_POINT ( 'NONE',  ( 20.88017736071110164, 35.35535201082150536, 2.915334737309930979 ) ) ;
#59076 = CARTESIAN_POINT ( 'NONE',  ( -46.94000000000000483, 101.3580217190346389, 7.614242055636530893 ) ) ;
#59077 = CIRCLE ( 'NONE', #6408, 0.5000000000000004441 ) ;
#59079 = VERTEX_POINT ( 'NONE', #65782 ) ;
#59078 = CARTESIAN_POINT ( 'NONE',  ( -45.94000000000000483, 92.00000000000000000, 5.000000000000000000 ) ) ;
#59080 = CARTESIAN_POINT ( 'NONE',  ( 1.472469842513823179, 30.59226448433411960, -4.923371831947296329 ) ) ;
#59081 = ORIENTED_EDGE ( 'NONE', *, *, #20098, .F. ) ;
#59082 = CARTESIAN_POINT ( 'NONE',  ( 17.20831665107776587, 59.13393115100078745, -7.208316651077762316 ) ) ;
#59083 = CARTESIAN_POINT ( 'NONE',  ( 14.26295192185811445, 14.95077488074852035, -3.770186020345025479 ) ) ;
#59084 = CARTESIAN_POINT ( 'NONE',  ( 6.204703633549690345, 10.76208216824729824, -14.16423886937410259 ) ) ;
#59085 = ORIENTED_EDGE ( 'NONE', *, *, #79251, .T. ) ;
#59086 = FACE_OUTER_BOUND ( 'NONE', #21701, .T. ) ;
#59087 = CARTESIAN_POINT ( 'NONE',  ( -5.069388085562224866, -24.96207786480668744, 3.750000000000001332 ) ) ;
#59088 = DIRECTION ( 'NONE',  ( 0.000000000000000000, 0.000000000000000000, -1.000000000000000000 ) ) ;
#59089 = CARTESIAN_POINT ( 'NONE',  ( 24.16423886937410614, 59.51208216824728936, -3.795296366450302550 ) ) ;
#59090 = DIRECTION ( 'NONE',  ( 0.000000000000000000, 1.000000000000000000, 0.000000000000000000 ) ) ;
#59091 = ORIENTED_EDGE ( 'NONE', *, *, #13652, .F. ) ;
#59092 = FACE_OUTER_BOUND ( 'NONE', #53480, .T. ) ;
#59093 = CARTESIAN_POINT ( 'NONE',  ( 0.1532563361054100626, 40.80059781766745886, -2.638427012816831230 ) ) ;
#59094 = CARTESIAN_POINT ( 'NONE',  ( 8.880000000000000782, -7.313785530894214126, 3.750000000000000000 ) ) ;
#59095 = CARTESIAN_POINT ( 'NONE',  ( 21.09922568453594849, 21.20696800326375353, 6.408140936763242479 ) ) ;
#59096 = CARTESIAN_POINT ( 'NONE',  ( 10.00000000000000000, 9.758931151000785675, -9.846743663894594434 ) ) ;
#59097 = CARTESIAN_POINT ( 'NONE',  ( 10.00000000000000178, 70.00000000000000000, 0.000000000000000000 ) ) ;
#59098 = CARTESIAN_POINT ( 'NONE',  ( 0.1532563361054082862, 6.217264484334118713, 2.638427012816831674 ) ) ;
#59099 = CARTESIAN_POINT ( 'NONE',  ( -1.099225684535947600, 8.706968003263753531, -6.408140936763238038 ) ) ;
#59100 = CARTESIAN_POINT ( 'NONE',  ( -8.399999999999998579, 98.49999999999998579, 8.000000000000000000 ) ) ;
#59101 = ORIENTED_EDGE ( 'NONE', *, *, #89741, .T. ) ;
#59102 = CARTESIAN_POINT ( 'NONE',  ( 20.88017736071110519, 10.56368534415483929, 2.639326808657452039E-16 ) ) ;
#59103 = CARTESIAN_POINT ( 'NONE',  ( 22.26659068614894466, 8.887082168247300018, 7.082119434687054849 ) ) ;
#59104 = CARTESIAN_POINT ( 'NONE',  ( 1.472469842513823179, 30.59226448433411960, -4.923371831947296329 ) ) ;
#59105 = CARTESIAN_POINT ( 'NONE',  ( 7.084665262690076126, 59.10535201082150536, 10.88017736071109987 ) ) ;
#59106 = CARTESIAN_POINT ( 'NONE',  ( -1.099225684535947600, 24.54030133659708923, 6.408140936763237150 ) ) ;
#59107 = CARTESIAN_POINT ( 'NONE',  ( 19.42250999205614193, 20.14701867748817321, 5.440088680355555262 ) ) ;
#59108 = DIRECTION ( 'NONE',  ( 0.000000000000000000, 0.000000000000000000, 1.000000000000000000 ) ) ;
#59109 = CARTESIAN_POINT ( 'NONE',  ( -10.98829462902744858, 46.98606209026556968, -2.899999999999999467 ) ) ;
#59110 = CARTESIAN_POINT ( 'NONE',  ( 21.09922568453595559, 2.040301336597086568, -6.408140936763230044 ) ) ;
#59111 = CARTESIAN_POINT ( 'NONE',  ( 0.1532563361054082862, 61.21726448433412315, 2.638427012816831674 ) ) ;
#59112 = CARTESIAN_POINT ( 'NONE',  ( 10.00000000000000178, 17.25893115100078745, 9.846743663894594434 ) ) ;
#59113 = CARTESIAN_POINT ( 'NONE',  ( 3.469446951953614189E-15, -5.686314655845153609, 10.88017736071110342 ) ) ;
#59114 = CARTESIAN_POINT ( 'NONE',  ( -2.816281873526471635, 33.91530133659708213, -3.434112377981056508 ) ) ;
#59115 = CARTESIAN_POINT ( 'NONE',  ( -10.91892017065343445, -97.58704351937099375, -3.750000000000000000 ) ) ;
#59117 = CARTESIAN_POINT ( 'NONE',  ( 14.94699059465107105, 14.49999999999999112, 1.259949270174897329 ) ) ;
#59116 = CARTESIAN_POINT ( 'NONE',  ( 10.00000000000000178, 39.31368534415484106, 10.88017736071110342 ) ) ;
#59118 = EDGE_CURVE ( 'NONE', #87452, #24464, #12299, .T. ) ;
#59119 = CARTESIAN_POINT ( 'NONE',  ( -45.94000000000000483, 92.00000000000000000, 9.000000000000000000 ) ) ;
#59120 = CARTESIAN_POINT ( 'NONE',  ( 20.88017736071110164, 25.35535201082150891, 2.915334737309930979 ) ) ;
#59121 = MECHANICAL_DESIGN_GEOMETRIC_PRESENTATION_REPRESENTATION (  '', ( #76691 ), #83117 ) ;
#59122 = CARTESIAN_POINT ( 'NONE',  ( 4.559911319644449179, 32.23035201082150536, -9.422509992056141925 ) ) ;
#59123 = CARTESIAN_POINT ( 'NONE',  ( 7.361572987183169658, 44.96726448433412315, -9.846743663894592657 ) ) ;
#59124 = CARTESIAN_POINT ( 'NONE',  ( 4.559911319644449179, 58.89701867748817676, 9.422509992056141925 ) ) ;
#59125 = CARTESIAN_POINT ( 'NONE',  ( -4.164238869374099927, 32.01208216824730357, 3.795296366450308767 ) ) ;
#59126 = UNCERTAINTY_MEASURE_WITH_UNIT (LENGTH_MEASURE( 1.000000000000000082E-05 ), #65581, 'distance_accuracy_value', 'NONE');
#59127 = CARTESIAN_POINT ( 'NONE',  ( 12.63842701281683034, 42.46726448433412315, 9.846743663894596210 ) ) ;
#59128 = CIRCLE ( 'NONE', #14480, 0.5000000000000004441 ) ;
#59129 = CARTESIAN_POINT ( 'NONE',  ( 19.84674366389459621, 63.50893115100078745, 7.409399052514197653E-17 ) ) ;
#59130 = ORIENTED_EDGE ( 'NONE', *, *, #6639, .T. ) ;
#59131 = CARTESIAN_POINT ( 'NONE',  ( 10.00000000000000178, 24.31368534415484106, 10.88017736071110342 ) ) ;
#59132 = CARTESIAN_POINT ( 'NONE',  ( 0.000000000000000000, 0.5000000000000004441, 0.000000000000000000 ) ) ;
#59133 = VECTOR ( 'NONE', #8009, 1000.000000000000114 ) ;
#59134 = CARTESIAN_POINT ( 'NONE',  ( 20.88017736071110519, 10.56368534415483929, 2.639326808657452039E-16 ) ) ;
#59135 = CARTESIAN_POINT ( 'NONE',  ( 10.00000000000000000, -0.2410688489992152128, -9.846743663894594434 ) ) ;
#59136 = CARTESIAN_POINT ( 'NONE',  ( 13.79529636645030344, 28.26208216824729647, 14.16423886937410614 ) ) ;
#59137 = CARTESIAN_POINT ( 'NONE',  ( 17.20831665107776587, 17.88393115100078745, 7.208316651077764980 ) ) ;
#59138 = CARTESIAN_POINT ( 'NONE',  ( 17.20831665107776587, 64.13393115100079456, -7.208316651077762316 ) ) ;
#59139 = CARTESIAN_POINT ( 'NONE',  ( 4.559911319644449179, 43.89701867748816966, 9.422509992056141925 ) ) ;
#59140 = CARTESIAN_POINT ( 'NONE',  ( 9.010802615329073006, 14.76984942314351734, -11.91753657575854675 ) ) ;
#59141 = CARTESIAN_POINT ( 'NONE',  ( 3.640395162852214650, 89.00000000000000000, 9.500000000000000000 ) ) ;
#59142 = ADVANCED_FACE ( 'NONE', ( #64787 ), #73781, .F. ) ;
#59143 = CIRCLE ( 'NONE', #16055, 0.7500000000000006661 ) ;
#59144 = ORIENTED_EDGE ( 'NONE', *, *, #4887, .T. ) ;
#59145 = CARTESIAN_POINT ( 'NONE',  ( -13.77612262535527954, 90.93158326518027934, 7.883772450803742338 ) ) ;
#59146 = CARTESIAN_POINT ( 'NONE',  ( 2.791683348922240793, 51.63393115100078745, 7.208316651077764092 ) ) ;
#59148 = VERTEX_POINT ( 'NONE', #73291 ) ;
#59147 = ADVANCED_FACE ( 'NONE', ( #41834 ), #57205, .T. ) ;
#59149 = ORIENTED_EDGE ( 'NONE', *, *, #65020, .T. ) ;
#59150 = DIRECTION ( 'NONE',  ( 0.000000000000000000, 1.000000000000000000, 0.000000000000000000 ) ) ;
#59151 = CARTESIAN_POINT ( 'NONE',  ( -4.164238869374099927, 17.01208216824730357, 3.795296366450308767 ) ) ;
#59152 = CARTESIAN_POINT ( 'NONE',  ( -2.266590686148945544, 22.22041550158063572, 7.082119434687048631 ) ) ;
#59153 = CARTESIAN_POINT ( 'NONE',  ( 0.5774900079438607392, 53.48035201082151247, 5.440088680355550821 ) ) ;
#59154 = CARTESIAN_POINT ( 'NONE',  ( 24.16423886937410614, 54.30374883491396787, 8.672049930838204340E-16 ) ) ;
#59155 = CARTESIAN_POINT ( 'NONE',  ( 22.81628187352647785, 1.623634669930420271, 6.195893100308588602E-16 ) ) ;
#59156 = CARTESIAN_POINT ( 'NONE',  ( 18.52753015748618282, 48.92559781766745886, -4.923371831947291888 ) ) ;
#59157 = CARTESIAN_POINT ( 'NONE',  ( -11.26393249254987516, -93.42496533367179268, 3.999999999999998224 ) ) ;
#59159 = CARTESIAN_POINT ( 'NONE',  ( 3.591859063236761518, 4.956968003263753531, 11.09922568453594849 ) ) ;
#59158 = CARTESIAN_POINT ( 'NONE',  ( -0.8801773607111008646, 48.27201867748816966, 2.915334737309923430 ) ) ;
#59160 = CARTESIAN_POINT ( 'NONE',  ( 10.00000000000000000, 20.55374883491396787, -14.16423886937410082 ) ) ;
#59161 = CARTESIAN_POINT ( 'NONE',  ( 13.79529636645031943, 55.34541550158062506, -14.16423886937409904 ) ) ;
#59162 = EDGE_CURVE ( 'NONE', #32363, #7251, #65286, .T. ) ;
#59163 = CARTESIAN_POINT ( 'NONE',  ( 20.88017736071110519, 20.56368534415484106, 2.639326808657452039E-16 ) ) ;
#59164 = CARTESIAN_POINT ( 'NONE',  ( 9.997910040112605756, 4.102332422533249404E-16, -10.50199004140717562 ) ) ;
#59165 = CARTESIAN_POINT ( 'NONE',  ( -0.8801773607111008646, 48.27201867748816966, 2.915334737309923430 ) ) ;
#59166 = CIRCLE ( 'NONE', #19271, 14.49999999999999822 ) ;
#59167 = CARTESIAN_POINT ( 'NONE',  ( -2.638427012816824124, -17.94940218233254825, 9.846743663894596210 ) ) ;
#59168 = ORIENTED_EDGE ( 'NONE', *, *, #36189, .T. ) ;
#59169 = CARTESIAN_POINT ( 'NONE',  ( -3.750000000000000000, 36.75000000000000000, -4.000000000000000000 ) ) ;
#59170 = VERTEX_POINT ( 'NONE', #87794 ) ;
#59171 = ORIENTED_EDGE ( 'NONE', *, *, #87068, .T. ) ;
#59172 = AXIS2_PLACEMENT_3D ( 'NONE', #23113, #31076, #92085 ) ;
#59173 = CARTESIAN_POINT ( 'NONE',  ( -0.3689425029237898834, 41.17874883491397497, -10.36894250292378850 ) ) ;
#59174 = CARTESIAN_POINT ( 'NONE',  ( 19.84674366389459266, 48.30059781766745175, 2.638427012816836559 ) ) ;
#59175 = CARTESIAN_POINT ( 'NONE',  ( 20.15039907845753575, 50.60158574516642460, -6.262539305110073506 ) ) ;
#59176 = DIRECTION ( 'NONE',  ( 0.000000000000000000, 0.000000000000000000, -1.000000000000000000 ) ) ;
#59177 = CARTESIAN_POINT ( 'NONE',  ( -0.8801773607111008646, 53.27201867748816966, 2.915334737309923430 ) ) ;
#59178 = AXIS2_PLACEMENT_3D ( 'NONE', #58208, #88725, #43223 ) ;
#59179 = CARTESIAN_POINT ( 'NONE',  ( 22.81628187352647785, 56.62363466993042493, 6.195893100308588602E-16 ) ) ;
#59180 = CARTESIAN_POINT ( 'NONE',  ( 12.81628187352647608, 11.62363466993042493, -2.602085213965210642E-15 ) ) ;
#59181 = EDGE_LOOP ( 'NONE', ( #31521, #32286, #79515, #73688 ) ) ;
#59182 = CARTESIAN_POINT ( 'NONE',  ( 10.00000000000000178, 38.05374883491396787, 14.16423886937410082 ) ) ;
#59183 = EDGE_CURVE ( 'NONE', #23479, #88687, #80306, .T. ) ;
#59184 = CARTESIAN_POINT ( 'NONE',  ( -1.099225684535947600, 18.70696800326375353, -6.408140936763238038 ) ) ;
#59185 = EDGE_LOOP ( 'NONE', ( #15728, #5595, #31623, #94507 ) ) ;
#59186 = CARTESIAN_POINT ( 'NONE',  ( 22.81628187352648496, 41.83196800326375353, -3.434112377981050290 ) ) ;
#59187 = CARTESIAN_POINT ( 'NONE',  ( 5.076628168052703671, 31.84226448433412315, 8.527530157486179263 ) ) ;
#59188 = CARTESIAN_POINT ( 'NONE',  ( -0.8801773607111008646, 13.27201867748817143, 2.915334737309923430 ) ) ;
#59189 = CARTESIAN_POINT ( 'NONE',  ( 13.43411237798106583, 57.66530133659708923, -12.81628187352647252 ) ) ;
#59190 = CARTESIAN_POINT ( 'NONE',  ( 12.14357320772536575, 54.02013147999952736, -3.000000000000000000 ) ) ;
#59191 = CARTESIAN_POINT ( 'NONE',  ( 18.52753015748617571, 43.09226448433412315, 4.923371831947298993 ) ) ;
#59192 = EDGE_CURVE ( 'NONE', #29547, #89183, #13287, .T. ) ;
#59193 =( BOUNDED_CURVE ( )  B_SPLINE_CURVE ( 2, ( #59175, #61151, #45165, #29656, #14191, #75669, #13189, #53163, #68182 ),
 .UNSPECIFIED., .F., .F. ) 
 B_SPLINE_CURVE_WITH_KNOTS ( ( 3, 2, 2, 2, 3 ),
 ( 0.2615695083688028277, 0.2619047619047619735, 0.2678571428571429047, 0.2738095238095238360, 0.2741447773454829817 ),
 .UNSPECIFIED. ) 
 CURVE ( )  GEOMETRIC_REPRESENTATION_ITEM ( )  RATIONAL_B_SPLINE_CURVE ( ( 0.9963778908391760503, 0.9980808541467920403, 1.000000000000000000, 0.9659258262890682012, 1.000000000000000000, 0.9659258262890682012, 1.000000000000000000, 0.9980808541467920403, 0.9963778908391759392 ) ) 
 REPRESENTATION_ITEM ( '' )  );
#59194 = CARTESIAN_POINT ( 'NONE',  ( 10.19513985507825637, 0.5000000000000004441, 11.00268709613223983 ) ) ;
#59195 = CARTESIAN_POINT ( 'NONE',  ( 18.95386800104996539, 18.23810908735726599, -6.499999999999990230 ) ) ;
#59196 = CARTESIAN_POINT ( 'NONE',  ( 4.879999999999991900, 76.07179676972444327, 6.250000000000000000 ) ) ;
#59197 = DIRECTION ( 'NONE',  ( 0.000000000000000000, 1.000000000000000000, 0.000000000000000000 ) ) ;
#59198 = CARTESIAN_POINT ( 'NONE',  ( 0.2751277870542910842, 67.28217586085239077, -6.499999999999992006 ) ) ;
#59199 = CARTESIAN_POINT ( 'NONE',  ( 1.472469842513823179, 11.42559781766745175, 4.923371831947296329 ) ) ;
#59200 = CARTESIAN_POINT ( 'NONE',  ( 22.81628187352647785, 21.62363466993041783, 6.195893100308588602E-16 ) ) ;
#59201 = STYLED_ITEM ( 'NONE', ( #2120 ), #46296 ) ;
#59202 = CARTESIAN_POINT ( 'NONE',  ( 9.779999999999988702, 27.00436609429084811, -3.000000000000000000 ) ) ;
#59203 = ORIENTED_EDGE ( 'NONE', *, *, #52387, .F. ) ;
#59204 = CARTESIAN_POINT ( 'NONE',  ( 7.361572987183170547, 52.05059781766745175, 9.846743663894590881 ) ) ;
#59205 = LINE ( 'NONE', #51222, #45858 ) ;
#59206 = CARTESIAN_POINT ( 'NONE',  ( 6.204703633549690345, 25.76208216824730712, -14.16423886937410259 ) ) ;
#59207 = CARTESIAN_POINT ( 'NONE',  ( 0.1532563361054100626, 45.80059781766745886, -2.638427012816831230 ) ) ;
#59208 = CARTESIAN_POINT ( 'NONE',  ( 16.40814093676323893, 50.79030133659708923, 11.09922568453595026 ) ) ;
#59209 = DIRECTION ( 'NONE',  ( 0.000000000000000000, 0.000000000000000000, 1.000000000000000000 ) ) ;
#59210 = CARTESIAN_POINT ( 'NONE',  ( 0.1532563361054083140, 11.00893115100078568, 1.131784320476157264E-15 ) ) ;
#59211 = CARTESIAN_POINT ( 'NONE',  ( 21.92686044187657046, 47.39664270246085209, -3.195792623639524432 ) ) ;
#59212 = CARTESIAN_POINT ( 'NONE',  ( 0.1532563361054083140, 46.00893115100079456, 1.131784320476157264E-15 ) ) ;
#59213 = CARTESIAN_POINT ( 'NONE',  ( 20.88017736071110875, 45.77201867748816966, -2.915334737309920765 ) ) ;
#59214 = CARTESIAN_POINT ( 'NONE',  ( 10.00000000000000000, 34.75893115100078745, -9.846743663894594434 ) ) ;
#59215 = APPLICATION_PROTOCOL_DEFINITION ( 'draft international standard', 'automotive_design', 1998, #42329 ) ;
#59216 = CARTESIAN_POINT ( 'NONE',  ( 0.7375392941518293943, 0.5000000000000004441, -14.98185688723470932 ) ) ;
#59217 = B_SPLINE_CURVE_WITH_KNOTS ( 'NONE', 3,
 ( #18774, #27234, #63752, #72243, #25299, #19250 ),
 .UNSPECIFIED., .F., .F.,
 ( 4, 2, 4 ),
 ( 3.409110551496116460E-05, 0.0004400426677367864632, 0.0008459942299586117008 ),
 .UNSPECIFIED. ) ;
#59218 = CARTESIAN_POINT ( 'NONE',  ( 7.084665262690076126, 42.02201867748816966, -10.88017736071110164 ) ) ;
#59219 = EDGE_LOOP ( 'NONE', ( #95355, #50616, #63425, #31395 ) ) ;
#59220 = CARTESIAN_POINT ( 'NONE',  ( -5.624999999999996447, 5.951366962315985276, 9.742785792574938597 ) ) ;
#59221 = CARTESIAN_POINT ( 'NONE',  ( 12.91533473730992121, 14.52201867748817143, 10.88017736071110164 ) ) ;
#59223 = CARTESIAN_POINT ( 'NONE',  ( 12.91533473730992121, 39.52201867748817676, 10.88017736071110164 ) ) ;
#59222 = CARTESIAN_POINT ( 'NONE',  ( 2.791683348922240793, 56.63393115100078035, 7.208316651077764092 ) ) ;
#59224 = DIRECTION ( 'NONE',  ( -0.8320502943378437211, 0.5547001962252290364, 0.000000000000000000 ) ) ;
#59225 = CARTESIAN_POINT ( 'NONE',  ( 12.91533473730993009, 56.60535201082151247, -10.88017736071109987 ) ) ;
#59227 = DIRECTION ( 'NONE',  ( 0.000000000000000000, 1.000000000000000000, 0.000000000000000000 ) ) ;
#59226 = CARTESIAN_POINT ( 'NONE',  ( 17.96484262340118221, 19.93868534415484106, 7.964842623401181321 ) ) ;
#59228 = CARTESIAN_POINT ( 'NONE',  ( 2.791683348922237240, 0.3839311510007847872, -7.208316651077763204 ) ) ;
#59229 = EDGE_CURVE ( 'NONE', #61453, #26206, #19797, .T. ) ;
#59230 = CARTESIAN_POINT ( 'NONE',  ( 10.00000000000000000, 19.75893115100078390, -9.846743663894594434 ) ) ;
#59231 = SURFACE_SIDE_STYLE ('',( #64751 ) ) ;
#59232 = CARTESIAN_POINT ( 'NONE',  ( 14.16423886937410437, 9.095415501580637496, 3.795296366450304770 ) ) ;
#59233 = CARTESIAN_POINT ( 'NONE',  ( 1.472469842513823179, 51.42559781766745886, 4.923371831947296329 ) ) ;
#59234 = CARTESIAN_POINT ( 'NONE',  ( 22.26659068614894466, 63.88708216824730357, 7.082119434687054849 ) ) ;
#59235 = VECTOR ( 'NONE', #10312, 1000.000000000000114 ) ;
#59237 = TOROIDAL_SURFACE ( 'NONE', #24156, 0.7500000000000008882, 0.2500000000000000000 ) ;
#59236 = CARTESIAN_POINT ( 'NONE',  ( 14.97687855664614531, 14.49999999999999112, -0.8325315005900779664 ) ) ;
#59238 = EDGE_CURVE ( 'NONE', #9538, #54489, #58275, .T. ) ;
#59239 = CARTESIAN_POINT ( 'NONE',  ( 6.204703633549690345, 10.76208216824729824, -14.16423886937410259 ) ) ;
#59240 = CARTESIAN_POINT ( 'NONE',  ( -0.3689425029237898834, 46.17874883491397497, -10.36894250292378850 ) ) ;
#59241 = CARTESIAN_POINT ( 'NONE',  ( 22.81628187352647785, 6.415301336597088344, 3.434112377981063169 ) ) ;
#59242 = PRESENTATION_LAYER_ASSIGNMENT (  '', '', ( #30484 ) ) ;
#59243 = EDGE_LOOP ( 'NONE', ( #49195, #42222, #45579, #19601, #90963, #20220 ) ) ;
#59244 = CARTESIAN_POINT ( 'NONE',  ( 10.00000000000000000, 16.81368534415483751, -10.88017736071110342 ) ) ;
#59245 = CARTESIAN_POINT ( 'NONE',  ( 2.791683348922237240, 45.38393115100079456, -7.208316651077763204 ) ) ;
#59247 = DIRECTION ( 'NONE',  ( 0.000000000000000000, 1.000000000000000000, 0.000000000000000000 ) ) ;
#59246 = SURFACE_STYLE_FILL_AREA ( #51760 ) ;
#59248 = PRESENTATION_STYLE_ASSIGNMENT (( #28756 ) ) ;
#59249 = DIRECTION ( 'NONE',  ( -0.000000000000000000, 1.000000000000000000, 0.000000000000000000 ) ) ;
#59250 = CARTESIAN_POINT ( 'NONE',  ( 6.565887622018943937, 18.08196800326375708, -12.81628187352647608 ) ) ;
#59251 = CARTESIAN_POINT ( 'NONE',  ( 12.63842701281683922, 24.55059781766745175, -9.846743663894590881 ) ) ;
#59252 = ORIENTED_EDGE ( 'NONE', *, *, #73729, .T. ) ;
#59253 = CARTESIAN_POINT ( 'NONE',  ( 18.52753015748618282, 8.925597817667451750, -4.923371831947291888 ) ) ;
#59254 = CARTESIAN_POINT ( 'NONE',  ( 17.84635730667656617, 3.637910973973187190, 6.500000000000000888 ) ) ;
#59255 = CARTESIAN_POINT ( 'NONE',  ( -46.82017113615791004, 100.6079546444643569, -9.324761308090124601 ) ) ;
#59256 = CARTESIAN_POINT ( 'NONE',  ( 0.5774900079438590739, 7.647018677488171434, -5.440088680355550821 ) ) ;
#59257 = CARTESIAN_POINT ( 'NONE',  ( -4.164238869374099039, 36.80374883491396787, 8.674139862899312516E-16 ) ) ;
#59258 = CARTESIAN_POINT ( 'NONE',  ( 7.084665262690076126, 42.02201867748816966, -10.88017736071110164 ) ) ;
#59259 = CARTESIAN_POINT ( 'NONE',  ( -0.8801773607110991993, 62.85535201082150536, -2.915334737309923874 ) ) ;
#59260 = DIRECTION ( 'NONE',  ( 1.000000000000000000, 0.000000000000000000, 0.000000000000000000 ) ) ;
#59261 = CARTESIAN_POINT ( 'NONE',  ( 1.472469842513823179, 25.59226448433412315, -4.923371831947296329 ) ) ;
#59262 = FACE_OUTER_BOUND ( 'NONE', #53317, .T. ) ;
#59263 = CARTESIAN_POINT ( 'NONE',  ( 14.92337183194729633, 2.675597817667451750, 8.527530157486181039 ) ) ;
#59264 = CARTESIAN_POINT ( 'NONE',  ( -1.419660342300774092, -7.341591041528218084E-16, 2.710667984842351608 ) ) ;
#59265 = CARTESIAN_POINT ( 'NONE',  ( 1.472469842513823179, 36.42559781766745175, 4.923371831947296329 ) ) ;
#59266 = CARTESIAN_POINT ( 'NONE',  ( 12.63842701281683922, 64.55059781766745175, -9.846743663894590881 ) ) ;
#59267 = AXIS2_PLACEMENT_3D ( 'NONE', #4261, #64727, #79264 ) ;
#59268 = CARTESIAN_POINT ( 'NONE',  ( 15.44008868035555260, 29.73035201082150891, 9.422509992056143702 ) ) ;
#59269 = UNCERTAINTY_MEASURE_WITH_UNIT (LENGTH_MEASURE( 1.000000000000000082E-05 ), #28776, 'distance_accuracy_value', 'NONE');
#59270 = VECTOR ( 'NONE', #53982, 1000.000000000000114 ) ;
#59271 = EDGE_CURVE ( 'NONE', #55464, #88425, #38104, .T. ) ;
#59272 = EDGE_LOOP ( 'NONE', ( #18319, #30144, #2285, #15687, #92626, #37219 ) ) ;
#59273 = CARTESIAN_POINT ( 'NONE',  ( 13.43411237798106583, 62.66530133659708923, -12.81628187352647252 ) ) ;
#59274 = FACE_OUTER_BOUND ( 'NONE', #66174, .T. ) ;
#59275 = CARTESIAN_POINT ( 'NONE',  ( 10.00000000000000178, 12.25893115100078568, 9.846743663894594434 ) ) ;
#59276 = CARTESIAN_POINT ( 'NONE',  ( 0.6178305044545818747, 43.49863466993042493, -9.382169495545419124 ) ) ;
#59278 = CARTESIAN_POINT ( 'NONE',  ( 0.1532563361054082862, 31.21726448433412315, 2.638427012816831674 ) ) ;
#59277 = CARTESIAN_POINT ( 'NONE',  ( 10.00000000000000000, 1.813685344154838175, -10.88017736071110342 ) ) ;
#59279 = PLANE ( 'NONE',  #31262 ) ;
#59280 = CARTESIAN_POINT ( 'NONE',  ( 6.204703633549690345, 20.76208216824730357, -14.16423886937410259 ) ) ;
#59281 = EDGE_CURVE ( 'NONE', #63243, #15746, #90260, .T. ) ;
#59282 = CARTESIAN_POINT ( 'NONE',  ( 6.204703633549690345, 42.84541550158063217, 14.16423886937410082 ) ) ;
#59283 = CARTESIAN_POINT ( 'NONE',  ( 14.92337183194729988, 49.34226448433411605, -8.527530157486177487 ) ) ;
#59284 = AXIS2_PLACEMENT_3D ( 'NONE', #4069, #81521, #80050 ) ;
#59285 = SURFACE_SIDE_STYLE ('',( #21300 ) ) ;
#59286 = CARTESIAN_POINT ( 'NONE',  ( 7.084665262690076126, 44.10535201082151247, 10.88017736071109987 ) ) ;
#59287 = B_SPLINE_CURVE_WITH_KNOTS ( 'NONE', 3,
 ( #28481, #51979, #58976, #51476, #83948, #13986 ),
 .UNSPECIFIED., .F., .F.,
 ( 4, 2, 4 ),
 ( 3.409110551496083934E-05, 0.0004400426677367859753, 0.0008459942299586110503 ),
 .UNSPECIFIED. ) ;
#59288 = CARTESIAN_POINT ( 'NONE',  ( 7.084665262690076126, 69.10535201082151957, 10.88017736071109987 ) ) ;
#59289 = DIRECTION ( 'NONE',  ( 1.000000000000000000, 0.000000000000000000, 0.000000000000000000 ) ) ;
#59290 = EDGE_LOOP ( 'NONE', ( #9872, #39355, #42486, #15384 ) ) ;
#59291 = CARTESIAN_POINT ( 'NONE',  ( -1.099225684535947600, 59.54030133659708923, 6.408140936763237150 ) ) ;
#59292 = VECTOR ( 'NONE', #50674, 1000.000000000000000 ) ;
#59293 = CARTESIAN_POINT ( 'NONE',  ( -0.8801773607111009756, 63.06368534415484106, 1.068504757029289695E-15 ) ) ;
#59294 = ORIENTED_EDGE ( 'NONE', *, *, #73617, .T. ) ;
#59295 = CARTESIAN_POINT ( 'NONE',  ( 13.79529636645030344, 3.262082168247301350, 14.16423886937410614 ) ) ;
#59296 = CARTESIAN_POINT ( 'NONE',  ( 2.791683348922237240, 5.383931151000785675, -7.208316651077763204 ) ) ;
#59297 = DIRECTION ( 'NONE',  ( -0.7445673648800779088, 0.6675473310227050261, 0.000000000000000000 ) ) ;
#59298 = VERTEX_POINT ( 'NONE', #29271 ) ;
#59299 = CARTESIAN_POINT ( 'NONE',  ( 15.44008868035555260, 19.73035201082150536, 9.422509992056143702 ) ) ;
#59300 = EDGE_CURVE ( 'NONE', #84680, #70377, #51783, .T. ) ;
#59301 = ORIENTED_EDGE ( 'NONE', *, *, #42395, .F. ) ;
#59302 = CARTESIAN_POINT ( 'NONE',  ( 4.559911319644449179, 27.23035201082150536, -9.422509992056141925 ) ) ;
#59303 = CARTESIAN_POINT ( 'NONE',  ( 1.472469842513823179, 65.59226448433412315, -4.923371831947296329 ) ) ;
#59304 = ORIENTED_EDGE ( 'NONE', *, *, #55011, .T. ) ;
#59305 = CARTESIAN_POINT ( 'NONE',  ( 1.472469842513823179, 61.42559781766745175, 4.923371831947296329 ) ) ;
#59306 = ORIENTED_EDGE ( 'NONE', *, *, #22299, .F. ) ;
#59307 = CARTESIAN_POINT ( 'NONE',  ( 7.361572987183169658, -0.03273551566588185635, -9.846743663894592657 ) ) ;
#59308 = CARTESIAN_POINT ( 'NONE',  ( 17.20831665107776587, 62.88393115100078745, 7.208316651077764980 ) ) ;
#59309 = CARTESIAN_POINT ( 'NONE',  ( -1.099225684535947600, 33.70696800326375353, -6.408140936763238038 ) ) ;
#59311 =( LENGTH_UNIT ( ) NAMED_UNIT ( * ) SI_UNIT ( .MILLI., .METRE. ) );
#59310 = CARTESIAN_POINT ( 'NONE',  ( -0.8801773607110991993, 22.85535201082150181, -2.915334737309923874 ) ) ;
#59312 = CARTESIAN_POINT ( 'NONE',  ( 14.92337183194729633, 2.675597817667451750, 8.527530157486181039 ) ) ;
#59313 = CARTESIAN_POINT ( 'NONE',  ( 20.88017736071110875, 20.77201867748816611, -2.915334737309920765 ) ) ;
#59314 = ORIENTED_EDGE ( 'NONE', *, *, #94367, .T. ) ;
#59315 = CARTESIAN_POINT ( 'NONE',  ( 22.81628187352647785, 51.62363466993042493, 6.195893100308588602E-16 ) ) ;
#59316 = CARTESIAN_POINT ( 'NONE',  ( 4.559911319644449179, 48.89701867748817676, 9.422509992056141925 ) ) ;
#59317 = CARTESIAN_POINT ( 'NONE',  ( 14.49154782523117291, 14.95037109980596135, 2.766288502469715471 ) ) ;
#59318 = CARTESIAN_POINT ( 'NONE',  ( 21.09922568453594849, 51.20696800326375353, 6.408140936763242479 ) ) ;
#59319 = CARTESIAN_POINT ( 'NONE',  ( -0.8801773607111009756, 48.06368534415484817, 1.068504757029289695E-15 ) ) ;
#59320 = CARTESIAN_POINT ( 'NONE',  ( 10.00000000000000178, 62.25893115100078745, 9.846743663894594434 ) ) ;
#59321 = CYLINDRICAL_SURFACE ( 'NONE', #40302, 19.99999999999999645 ) ;
#59322 = CARTESIAN_POINT ( 'NONE',  ( 17.20831665107776587, 24.13393115100078035, -7.208316651077762316 ) ) ;
#59323 = CARTESIAN_POINT ( 'NONE',  ( 13.43411237798106583, 7.665301336597086568, -12.81628187352647252 ) ) ;
#59325 = CARTESIAN_POINT ( 'NONE',  ( 18.52753015748618282, 58.92559781766745886, -4.923371831947291888 ) ) ;
#59324 = CARTESIAN_POINT ( 'NONE',  ( 6.000000000000000000, 60.50000000000000711, 6.500000000000000888 ) ) ;
#59326 = CARTESIAN_POINT ( 'NONE',  ( 0.5774900079438590739, 27.64701867748817676, -5.440088680355550821 ) ) ;
#59327 = CARTESIAN_POINT ( 'NONE',  ( 19.84674366389459266, 48.71726448433413026, -2.638427012816827677 ) ) ;
#59328 = FILL_AREA_STYLE_COLOUR ( '', #846 ) ;
#59329 = CARTESIAN_POINT ( 'NONE',  ( 1.472469842513823179, 6.425597817667451750, 4.923371831947296329 ) ) ;
#59330 = CARTESIAN_POINT ( 'NONE',  ( 17.39651004071842166, 27.93575266056828355, 6.499999999999998224 ) ) ;
#59332 = ORIENTED_EDGE ( 'NONE', *, *, #53785, .F. ) ;
#59331 = CARTESIAN_POINT ( 'NONE',  ( 6.565887622018943937, 8.081968003263751754, -12.81628187352647608 ) ) ;
#59333 = STYLED_ITEM ( 'NONE', ( #3472 ), #63985 ) ;
#59334 = CARTESIAN_POINT ( 'NONE',  ( 9.240973841163533820, 15.00000000000000000, 11.17382667070378943 ) ) ;
#59335 = DIRECTION ( 'NONE',  ( 0.000000000000000000, 0.000000000000000000, 1.000000000000000000 ) ) ;
#59336 = CARTESIAN_POINT ( 'NONE',  ( -2.816281873526473856, 44.12363466993042493, 9.499525473075851096E-16 ) ) ;
#59337 = CARTESIAN_POINT ( 'NONE',  ( 2.791683348922240793, 31.63393115100078745, 7.208316651077764092 ) ) ;
#59338 = DIRECTION ( 'NONE',  ( -0.000000000000000000, -1.000000000000000000, -0.000000000000000000 ) ) ;
#59339 = CARTESIAN_POINT ( 'NONE',  ( 2.035157376598822676, 12.43868534415483751, -7.964842623401177768 ) ) ;
#59340 = CARTESIAN_POINT ( 'NONE',  ( 10.00000000000000178, 27.25893115100078390, 9.846743663894594434 ) ) ;
#59341 = TOROIDAL_SURFACE ( 'NONE', #97714, 14.49999999999999822, 0.5000000000000000000 ) ;
#59342 = CARTESIAN_POINT ( 'NONE',  ( 11.81378540890936080, -0.03417435944610275333, -7.968498874458115999 ) ) ;
#59343 = CARTESIAN_POINT ( 'NONE',  ( 7.084665262690076126, 4.105352010821503583, 10.88017736071109987 ) ) ;
#59344 = CARTESIAN_POINT ( 'NONE',  ( -12.94148294176549108, 90.75484370785780186, -7.596443435273322997 ) ) ;
#59345 = CARTESIAN_POINT ( 'NONE',  ( 12.91533473730993009, 16.60535201082150891, -10.88017736071109987 ) ) ;
#59346 = CARTESIAN_POINT ( 'NONE',  ( -4.164238869374098151, 51.59541550158063217, -3.795296366450310543 ) ) ;
#59348 = CARTESIAN_POINT ( 'NONE',  ( -1.354709868695410657, 15.00000000000000000, -14.93870011653153362 ) ) ;
#59347 = CARTESIAN_POINT ( 'NONE',  ( 24.16423886937409904, 49.09541550158063217, 3.795296366450317205 ) ) ;
#59349 = AXIS2_PLACEMENT_3D ( 'NONE', #76069, #7598, #38094 ) ;
#59350 = CARTESIAN_POINT ( 'NONE',  ( 19.84674366389459266, 8.300597817667451750, 2.638427012816836559 ) ) ;
#59351 = CARTESIAN_POINT ( 'NONE',  ( 16.40814093676323893, 5.790301336597087456, 11.09922568453595026 ) ) ;
#59352 = B_SPLINE_CURVE_WITH_KNOTS ( 'NONE', 3,
 ( #89182, #36182, #51687, #7170, #43676, #82666 ),
 .UNSPECIFIED., .F., .F.,
 ( 4, 2, 4 ),
 ( 0.0002800005319459029376, 0.0006862057665691747351, 0.001092411001192446695 ),
 .UNSPECIFIED. ) ;
#59353 = VERTEX_POINT ( 'NONE', #21793 ) ;
#59354 = CYLINDRICAL_SURFACE ( 'NONE', #86460, 0.5000000000000004441 ) ;
#59355 = ADVANCED_FACE ( 'NONE', ( #38761 ), #85991, .T. ) ;
#59356 = CARTESIAN_POINT ( 'NONE',  ( 10.00000000000000000, 59.75893115100078745, -9.846743663894594434 ) ) ;
#59357 = CARTESIAN_POINT ( 'NONE',  ( -46.90022492818602018, 100.5602504341072319, -9.231048971334091746 ) ) ;
#59358 = CARTESIAN_POINT ( 'NONE',  ( 18.52753015748618282, 63.92559781766745886, -4.923371831947291888 ) ) ;
#59359 = CARTESIAN_POINT ( 'NONE',  ( 14.61046065509106029, 15.00000000000000533, 0.6655452423543793961 ) ) ;
#59360 = CARTESIAN_POINT ( 'NONE',  ( 14.92337183194729988, 19.34226448433411960, -8.527530157486177487 ) ) ;
#59361 = CARTESIAN_POINT ( 'NONE',  ( 0.000000000000000000, 14.49999999999999822, 0.000000000000000000 ) ) ;
#59362 = CARTESIAN_POINT ( 'NONE',  ( -0.3689425029237898834, 36.17874883491396787, -10.36894250292378850 ) ) ;
#59363 = B_SPLINE_SURFACE_WITH_KNOTS ( 'NONE', 3, 1, ( 
 ( #47222, #86224 ),
 ( #62717, #54721 ),
 ( #41232, #93217 ),
 ( #54237, #92733 ),
 ( #69749, #8739 ) ),
 .UNSPECIFIED., .F., .F., .F.,
 ( 4, 1, 4 ),
 ( 2, 2 ),
 ( 0.000000000000000000, 0.4679165934955020201, 1.000000000000000000 ),
 ( 0.000000000000000000, 1.000000000000000000 ),
 .UNSPECIFIED. ) ;
#59364 = CARTESIAN_POINT ( 'NONE',  ( 12.63842701281683922, 4.550597817667451750, -9.846743663894590881 ) ) ;
#59366 = SURFACE_STYLE_FILL_AREA ( #4424 ) ;
#59365 = CARTESIAN_POINT ( 'NONE',  ( 1.152268111383477178, 1.024801820426059406E-17, -6.000000000000281553 ) ) ;
#59367 = CARTESIAN_POINT ( 'NONE',  ( -0.8801773607111009756, 28.06368534415484106, 1.068504757029289695E-15 ) ) ;
#59368 = CARTESIAN_POINT ( 'NONE',  ( 0.6178305044545838731, 39.74863466993041072, 9.382169495545420901 ) ) ;
#59369 = CARTESIAN_POINT ( 'NONE',  ( 7.084665262690076126, 9.105352010821503583, 10.88017736071109987 ) ) ;
#59370 = CARTESIAN_POINT ( 'NONE',  ( 22.81628187352647785, 41.62363466993042493, 6.195893100308588602E-16 ) ) ;
#59371 = CARTESIAN_POINT ( 'NONE',  ( 3.591859063236761518, 59.95696800326375353, 11.09922568453594849 ) ) ;
#59372 = ORIENTED_EDGE ( 'NONE', *, *, #65266, .F. ) ;
#59373 = CARTESIAN_POINT ( 'NONE',  ( 1.932340009482149679, 11.49127512925448080, -6.499999999999995559 ) ) ;
#59374 = CARTESIAN_POINT ( 'NONE',  ( 22.26659068614895176, 34.72041550158063927, -7.082119434687042414 ) ) ;
#59375 = CARTESIAN_POINT ( 'NONE',  ( 20.88017736071110164, 5.355352010821502695, 2.915334737309930979 ) ) ;
#59376 = CARTESIAN_POINT ( 'NONE',  ( 12.91533473730992121, 24.52201867748816966, 10.88017736071110164 ) ) ;
#59377 = DIRECTION ( 'NONE',  ( -0.07626964003977962370, 0.9970872288863209532, 0.000000000000000000 ) ) ;
#59378 = CARTESIAN_POINT ( 'NONE',  ( 27.50000000000000355, 35.99999999999997158, -10.00000000000000000 ) ) ;
#59379 = CARTESIAN_POINT ( 'NONE',  ( 20.88017736071110164, 50.35535201082151247, 2.915334737309930979 ) ) ;
#59380 = CARTESIAN_POINT ( 'NONE',  ( -0.8801773607111008646, 48.27201867748816966, 2.915334737309923430 ) ) ;
#59381 = CARTESIAN_POINT ( 'NONE',  ( 3.591859063236761518, 14.95696800326375531, 11.09922568453594849 ) ) ;
#59382 = CARTESIAN_POINT ( 'NONE',  ( 0.000000000000000000, 0.000000000000000000, 14.25000000000000000 ) ) ;
#59383 = CARTESIAN_POINT ( 'NONE',  ( -7.860426697680325425, -0.03417435944610275333, -13.93165778241942832 ) ) ;
#59384 = CARTESIAN_POINT ( 'NONE',  ( 12.63842701281683034, 27.46726448433411250, 9.846743663894596210 ) ) ;
#59385 = CARTESIAN_POINT ( 'NONE',  ( -0.8801773607111008646, 63.27201867748817676, 2.915334737309923430 ) ) ;
#59386 = B_SPLINE_CURVE_WITH_KNOTS ( 'NONE', 3,
 ( #86960, #48959, #79469, #10967, #71958, #11926 ),
 .UNSPECIFIED., .F., .F.,
 ( 4, 2, 4 ),
 ( 0.0002800020636817269993, 0.0006862073132860365288, 0.001092412562890346167 ),
 .UNSPECIFIED. ) ;
#59387 = CIRCLE ( 'NONE', #14738, 0.5000000000000004441 ) ;
#59388 = EDGE_CURVE ( 'NONE', #28267, #4086, #76745, .T. ) ;
#59389 = CARTESIAN_POINT ( 'NONE',  ( 0.6178305044545838731, 14.74863466993041783, 9.382169495545420901 ) ) ;
#59390 = CARTESIAN_POINT ( 'NONE',  ( 19.42250999205614193, 10.14701867748816966, 5.440088680355555262 ) ) ;
#59391 = CARTESIAN_POINT ( 'NONE',  ( 5.076628168052703671, 36.84226448433412315, 8.527530157486179263 ) ) ;
#59392 = CARTESIAN_POINT ( 'NONE',  ( 16.40814093676324603, 52.45696800326375353, -11.09922568453594671 ) ) ;
#59393 = CARTESIAN_POINT ( 'NONE',  ( 12.63842701281683034, 22.46726448433411605, 9.846743663894596210 ) ) ;
#59394 = EDGE_CURVE ( 'NONE', #19380, #56358, #44764, .T. ) ;
#59395 = CARTESIAN_POINT ( 'NONE',  ( 10.00000000000000000, 10.55374883491396787, -14.16423886937410082 ) ) ;
#59396 = CARTESIAN_POINT ( 'NONE',  ( 2.603489959281614308, 36.58210964143329136, 6.500000000000031086 ) ) ;
#59397 = CARTESIAN_POINT ( 'NONE',  ( -0.8801773607111008646, 18.27201867748817321, 2.915334737309923430 ) ) ;
#59399 = CARTESIAN_POINT ( 'NONE',  ( -2.266590686148945544, 32.22041550158063927, 7.082119434687048631 ) ) ;
#59398 = LINE ( 'NONE', #29883, #8951 ) ;
#59400 = CARTESIAN_POINT ( 'NONE',  ( 19.84674366389459266, 38.71726448433412315, -2.638427012816827677 ) ) ;
#59401 = CARTESIAN_POINT ( 'NONE',  ( 10.00000000000000178, 24.31368534415484106, 10.88017736071110342 ) ) ;
#59402 = CARTESIAN_POINT ( 'NONE',  ( -0.8801773607111009756, 13.06368534415483929, 1.068504757029289695E-15 ) ) ;
#59403 = VERTEX_POINT ( 'NONE', #83269 ) ;
#59404 = CARTESIAN_POINT ( 'NONE',  ( 7.084665262690076126, 29.10535201082150181, 10.88017736071109987 ) ) ;
#59405 = CARTESIAN_POINT ( 'NONE',  ( 0.6178305044545818747, 48.49863466993042493, -9.382169495545419124 ) ) ;
#59406 = CARTESIAN_POINT ( 'NONE',  ( -0.8801773607110991993, 32.85535201082151247, -2.915334737309923874 ) ) ;
#59407 = ORIENTED_EDGE ( 'NONE', *, *, #36355, .T. ) ;
#59408 = CARTESIAN_POINT ( 'NONE',  ( 1.472469842513823179, 51.42559781766745886, 4.923371831947296329 ) ) ;
#59409 = CARTESIAN_POINT ( 'NONE',  ( 17.96484262340118221, 36.18868534415484106, -7.964842623401177768 ) ) ;
#59410 = CARTESIAN_POINT ( 'NONE',  ( 19.84674366389459266, 63.71726448433412315, -2.638427012816827677 ) ) ;
#59411 =( NAMED_UNIT ( * ) SI_UNIT ( $, .STERADIAN. ) SOLID_ANGLE_UNIT ( ) );
#59412 = CARTESIAN_POINT ( 'NONE',  ( 21.09922568453594849, 61.20696800326376064, 6.408140936763242479 ) ) ;
#59413 = FACE_OUTER_BOUND ( 'NONE', #47045, .T. ) ;
#59414 = CARTESIAN_POINT ( 'NONE',  ( 2.917880565312950480, 50.97041550158064638, -12.26659068614894821 ) ) ;
#59415 = CARTESIAN_POINT ( 'NONE',  ( -0.8801773607111008646, 58.27201867748816966, 2.915334737309923430 ) ) ;
#59416 = DIRECTION ( 'NONE',  ( 0.9970872288863208421, 0.07626964003977952655, -0.000000000000000000 ) ) ;
#59417 = DIRECTION ( 'NONE',  ( 0.000000000000000000, 0.000000000000000000, 1.000000000000000000 ) ) ;
#59418 = CARTESIAN_POINT ( 'NONE',  ( 19.84674366389459621, 63.50893115100078745, 7.409399052514197653E-17 ) ) ;
#59419 = AXIS2_PLACEMENT_3D ( 'NONE', #26147, #96128, #55665 ) ;
#59420 = DIRECTION ( 'NONE',  ( 0.000000000000000000, 1.000000000000000000, 0.000000000000000000 ) ) ;
#59421 = CARTESIAN_POINT ( 'NONE',  ( 17.20831665107776587, 14.13393115100078568, -7.208316651077762316 ) ) ;
#59422 = ORIENTED_EDGE ( 'NONE', *, *, #7131, .F. ) ;
#59423 = VECTOR ( 'NONE', #86604, 1000.000000000000000 ) ;
#59424 = CARTESIAN_POINT ( 'NONE',  ( 5.076628168052704559, 15.17559781766745175, -8.527530157486179263 ) ) ;
#59425 = CARTESIAN_POINT ( 'NONE',  ( 3.469446951953614189E-15, -19.62636533006957507, 12.81628187352647608 ) ) ;
#59426 = EDGE_CURVE ( 'NONE', #79199, #73080, #31235, .T. ) ;
#59427 = CARTESIAN_POINT ( 'NONE',  ( 12.91533473730992121, 29.52201867748817321, 10.88017736071110164 ) ) ;
#59428 = CARTESIAN_POINT ( 'NONE',  ( 18.52753015748618282, 23.92559781766745530, -4.923371831947291888 ) ) ;
#59430 = CARTESIAN_POINT ( 'NONE',  ( 7.084665262690076126, 62.02201867748816966, -10.88017736071110164 ) ) ;
#59429 = CARTESIAN_POINT ( 'NONE',  ( 12.91533473730993009, 56.60535201082151247, -10.88017736071109987 ) ) ;
#59432 = CARTESIAN_POINT ( 'NONE',  ( 16.40814093676324603, 57.45696800326375353, -11.09922568453594671 ) ) ;
#59431 = CARTESIAN_POINT ( 'NONE',  ( -0.8801773607111008646, 33.27201867748817676, 2.915334737309923430 ) ) ;
#59433 = CARTESIAN_POINT ( 'NONE',  ( 2.917880565312950480, 45.97041550158063927, -12.26659068614894821 ) ) ;
#59434 = EDGE_CURVE ( 'NONE', #10785, #11195, #29756, .T. ) ;
#59435 = CIRCLE ( 'NONE', #37115, 1.000000000000000888 ) ;
#59436 = CYLINDRICAL_SURFACE ( 'NONE', #67466, 0.2500000000000002220 ) ;
#59437 = ORIENTED_EDGE ( 'NONE', *, *, #46885, .T. ) ;
#59438 = CARTESIAN_POINT ( 'NONE',  ( -2.816281873526471635, -1.084698663402913210, -3.434112377981056508 ) ) ;
#59439 = CARTESIAN_POINT ( 'NONE',  ( 7.084665262690076126, 4.105352010821503583, 10.88017736071109987 ) ) ;
#59440 = CARTESIAN_POINT ( 'NONE',  ( 17.96484262340118221, 49.93868534415484106, 7.964842623401181321 ) ) ;
#59441 = DIRECTION ( 'NONE',  ( -1.000000000000000000, 0.000000000000000000, 0.000000000000000000 ) ) ;
#59442 = ORIENTED_EDGE ( 'NONE', *, *, #93485, .T. ) ;
#59443 = CARTESIAN_POINT ( 'NONE',  ( 1.472469842513823179, 20.59226448433411960, -4.923371831947296329 ) ) ;
#59444 = CARTESIAN_POINT ( 'NONE',  ( 15.44008868035555260, 59.73035201082151247, 9.422509992056143702 ) ) ;
#59445 = CARTESIAN_POINT ( 'NONE',  ( 12.63842701281683034, 37.46726448433411605, 9.846743663894596210 ) ) ;
#59446 = CARTESIAN_POINT ( 'NONE',  ( 19.84674366389459266, 28.30059781766745886, 2.638427012816836559 ) ) ;
#59447 = CARTESIAN_POINT ( 'NONE',  ( 0.1532563361054083140, 16.00893115100078390, 1.131784320476157264E-15 ) ) ;
#59449 = CARTESIAN_POINT ( 'NONE',  ( 10.00000000000000178, 40.37363466993042493, 12.81628187352647608 ) ) ;
#59448 = CARTESIAN_POINT ( 'NONE',  ( 9.075906804202286793, 15.00000000000000000, -13.17214151599837990 ) ) ;
#59451 = DIRECTION ( 'NONE',  ( -0.9636304532086211738, 0.000000000000000000, -0.2672383760782636175 ) ) ;
#59450 = CARTESIAN_POINT ( 'NONE',  ( 7.084665262690076126, 69.10535201082151957, 10.88017736071109987 ) ) ;
#59452 = B_SPLINE_CURVE_WITH_KNOTS ( 'NONE', 3,
 ( #75586, #36098, #21110, #82093, #97625, #13604 ),
 .UNSPECIFIED., .F., .F.,
 ( 4, 2, 4 ),
 ( 3.409110551415738455E-05, 0.0004400426677360065966, 0.0008459942299578557950 ),
 .UNSPECIFIED. ) ;
#59453 = CARTESIAN_POINT ( 'NONE',  ( 10.34946471146702152, -32.01331896740364158, 3.750000000000000000 ) ) ;
#59455 = ORIENTED_EDGE ( 'NONE', *, *, #48537, .T. ) ;
#59454 = CARTESIAN_POINT ( 'NONE',  ( 12.63842701281683034, 32.46726448433412315, 9.846743663894596210 ) ) ;
#59456 = CARTESIAN_POINT ( 'NONE',  ( 19.38216949554541557, 57.24863466993042493, -9.382169495545420901 ) ) ;
#59457 = VECTOR ( 'NONE', #33358, 1000.000000000000000 ) ;
#59458 = CARTESIAN_POINT ( 'NONE',  ( 7.184033521041855330, -73.16344059793534882, 4.000000000000000888 ) ) ;
#59459 = CARTESIAN_POINT ( 'NONE',  ( 6.565887622018943937, -1.918031996736246692, -12.81628187352647608 ) ) ;
#59460 = CARTESIAN_POINT ( 'NONE',  ( 20.88017736071110519, 10.56368534415483751, 2.639326808657452039E-16 ) ) ;
#59461 = CARTESIAN_POINT ( 'NONE',  ( -0.3689425029237881626, 37.42874883491396787, 10.36894250292379027 ) ) ;
#59462 = UNCERTAINTY_MEASURE_WITH_UNIT (LENGTH_MEASURE( 1.000000000000000082E-05 ), #69104, 'distance_accuracy_value', 'NONE');
#59463 = CARTESIAN_POINT ( 'NONE',  ( 3.000000000000000444, 23.03999999999999915, 3.673940397442059868E-16 ) ) ;
#59464 = CARTESIAN_POINT ( 'NONE',  ( -4.164238869374099927, 37.01208216824731068, 3.795296366450308767 ) ) ;
#59465 = CARTESIAN_POINT ( 'NONE',  ( 24.16423886937409904, 44.09541550158063927, 3.795296366450317205 ) ) ;
#59466 = CARTESIAN_POINT ( 'NONE',  ( 13.79529636645031943, 10.34541550158063394, -14.16423886937409904 ) ) ;
#59468 = DIRECTION ( 'NONE',  ( -1.000000000000000000, 0.000000000000000000, -0.000000000000000000 ) ) ;
#59467 = CARTESIAN_POINT ( 'NONE',  ( 22.26659068614894466, 8.887082168247300018, 7.082119434687054849 ) ) ;
#59469 = CARTESIAN_POINT ( 'NONE',  ( 7.084665262690076126, 44.10535201082151247, 10.88017736071109987 ) ) ;
#59470 = DIRECTION ( 'NONE',  ( -0.000000000000000000, -0.000000000000000000, -1.000000000000000000 ) ) ;
#59471 = EDGE_LOOP ( 'NONE', ( #61883, #24177, #63996, #18250 ) ) ;
#59472 = CARTESIAN_POINT ( 'NONE',  ( 5.076628168052704559, 35.17559781766745175, -8.527530157486179263 ) ) ;
#59474 = CARTESIAN_POINT ( 'NONE',  ( 7.361572987183169658, 24.96726448433412315, -9.846743663894592657 ) ) ;
#59473 = DIRECTION ( 'NONE',  ( 1.000000000000000000, 2.799047438454523236E-16, -0.000000000000000000 ) ) ;
#59475 = CARTESIAN_POINT ( 'NONE',  ( 15.44008868035555260, 9.730352010821505360, 9.422509992056143702 ) ) ;
#59476 = CARTESIAN_POINT ( 'NONE',  ( 0.6178305044545818747, 58.49863466993042493, -9.382169495545419124 ) ) ;
#59477 = CARTESIAN_POINT ( 'NONE',  ( 1.472469842513823179, 51.42559781766745886, 4.923371831947296329 ) ) ;
#59478 = EDGE_CURVE ( 'NONE', #49035, #43285, #87039, .T. ) ;
#59479 = CARTESIAN_POINT ( 'NONE',  ( 18.52753015748618282, 28.92559781766745175, -4.923371831947291888 ) ) ;
#59480 = CARTESIAN_POINT ( 'NONE',  ( 10.00000000000000178, 45.37363466993041783, 12.81628187352647608 ) ) ;
#59481 = CARTESIAN_POINT ( 'NONE',  ( 12.26659068614894821, -16.11291783175269643, 7.082119434687044190 ) ) ;
#59482 = CIRCLE ( 'NONE', #16390, 14.49999999999999822 ) ;
#59483 = CARTESIAN_POINT ( 'NONE',  ( 20.88017736071110519, 40.56368534415484106, 2.639326808657452039E-16 ) ) ;
#59484 = CARTESIAN_POINT ( 'NONE',  ( 1.472469842513823179, 35.59226448433412315, -4.923371831947296329 ) ) ;
#59485 = CARTESIAN_POINT ( 'NONE',  ( 13.79529636645031943, 25.34541550158063572, -14.16423886937409904 ) ) ;
#59486 = ORIENTED_EDGE ( 'NONE', *, *, #57620, .F. ) ;
#59487 = CARTESIAN_POINT ( 'NONE',  ( 2.917880565312950480, 0.9704155015806342766, -12.26659068614894821 ) ) ;
#59488 = B_SPLINE_CURVE_WITH_KNOTS ( 'NONE', 3,
 ( #44429, #6939, #37446, #67937 ),
 .UNSPECIFIED., .F., .F.,
 ( 4, 4 ),
 ( 3.418109631315660599E-17, 0.002392975128318455130 ),
 .UNSPECIFIED. ) ;
#59489 = CARTESIAN_POINT ( 'NONE',  ( 12.91533473730993009, 61.60535201082150536, -10.88017736071109987 ) ) ;
#59490 = CARTESIAN_POINT ( 'NONE',  ( 15.44008868035555260, 64.73035201082151957, 9.422509992056143702 ) ) ;
#59492 = VECTOR ( 'NONE', #78268, 1000.000000000000000 ) ;
#59491 = CARTESIAN_POINT ( 'NONE',  ( 17.08211943468705130, 63.47041550158063927, 12.26659068614894998 ) ) ;
#59493 = CARTESIAN_POINT ( 'NONE',  ( 1.472469842513823179, 66.42559781766745175, 4.923371831947296329 ) ) ;
#59494 = AXIS2_PLACEMENT_3D ( 'NONE', #28846, #13365, #36364 ) ;
#59495 = CARTESIAN_POINT ( 'NONE',  ( 4.380000000000002558, 1.019547802438462547, 2.750000000000000000 ) ) ;
#59496 = CARTESIAN_POINT ( 'NONE',  ( 10.00000000000000178, 54.31368534415484106, 10.88017736071110342 ) ) ;
#59497 = AXIS2_PLACEMENT_3D ( 'NONE', #9003, #17013, #47491 ) ;
#59498 = FACE_OUTER_BOUND ( 'NONE', #46518, .T. ) ;
#59499 = CARTESIAN_POINT ( 'NONE',  ( -9.422509992056136596, 23.48035201082151957, 5.440088680355559703 ) ) ;
#59500 = CARTESIAN_POINT ( 'NONE',  ( 0.5774900079438607392, 18.48035201082150536, 5.440088680355550821 ) ) ;
#59502 = CIRCLE ( 'NONE', #29163, 0.2500000000000034972 ) ;
#59501 = CARTESIAN_POINT ( 'NONE',  ( 20.88017736071110519, 5.563685344154838397, 2.639326808657452039E-16 ) ) ;
#59503 = CARTESIAN_POINT ( 'NONE',  ( 18.52753015748617571, 48.09226448433412315, 4.923371831947298993 ) ) ;
#59504 = CARTESIAN_POINT ( 'NONE',  ( 16.40814093676323893, 55.79030133659708923, 11.09922568453595026 ) ) ;
#59505 = DIRECTION ( 'NONE',  ( -0.000000000000000000, -1.000000000000000000, -0.000000000000000000 ) ) ;
#59506 = ORIENTED_EDGE ( 'NONE', *, *, #84593, .T. ) ;
#59507 = CARTESIAN_POINT ( 'NONE',  ( 20.88017736071110519, 20.56368534415484106, 2.639326808657452039E-16 ) ) ;
#59508 = CARTESIAN_POINT ( 'NONE',  ( -2.816281873526473856, -0.6680319967362464695, 3.434112377981055619 ) ) ;
#59509 = DIRECTION ( 'NONE',  ( -0.000000000000000000, -0.000000000000000000, -1.000000000000000000 ) ) ;
#59510 = CIRCLE ( 'NONE', #11397, 0.2499999999999998890 ) ;
#59511 = CARTESIAN_POINT ( 'NONE',  ( 14.92337183194729633, 12.67559781766745353, 8.527530157486181039 ) ) ;
#59512 = ADVANCED_FACE ( 'NONE', ( #75269 ), #13784, .F. ) ;
#59513 = CARTESIAN_POINT ( 'NONE',  ( 12.63842701281683034, 47.46726448433412315, 9.846743663894596210 ) ) ;
#59514 = CARTESIAN_POINT ( 'NONE',  ( 0.5774900079438590739, 32.64701867748816966, -5.440088680355550821 ) ) ;
#59515 = CARTESIAN_POINT ( 'NONE',  ( -2.816281873526473856, 4.331968003263754419, 3.434112377981055619 ) ) ;
#59517 = CARTESIAN_POINT ( 'NONE',  ( -8.900000000000002132, 80.99999999999994316, 2.900000000000001243 ) ) ;
#59516 = CARTESIAN_POINT ( 'NONE',  ( -0.8801773607110991993, 52.85535201082151247, -2.915334737309923874 ) ) ;
#59518 = FACE_OUTER_BOUND ( 'NONE', #41867, .T. ) ;
#59519 = CARTESIAN_POINT ( 'NONE',  ( 19.38216949554541557, 52.24863466993041072, -9.382169495545420901 ) ) ;
#59520 = ORIENTED_EDGE ( 'NONE', *, *, #76323, .F. ) ;
#59521 = CARTESIAN_POINT ( 'NONE',  ( 5.419894505350532299, 14.49999999999999112, 13.98659156302467466 ) ) ;
#59522 = ADVANCED_FACE ( 'NONE', ( #44270 ), #30743, .F. ) ;
#59523 = CARTESIAN_POINT ( 'NONE',  ( 6.565887622018943937, 33.08196800326374643, -12.81628187352647608 ) ) ;
#59524 = DIRECTION ( 'NONE',  ( -1.000000000000000000, 2.081668171172166620E-14, 0.000000000000000000 ) ) ;
#59525 = CARTESIAN_POINT ( 'NONE',  ( 10.00000000000000178, 44.31368534415484106, 10.88017736071110342 ) ) ;
#59526 = DIRECTION ( 'NONE',  ( 0.000000000000000000, 0.000000000000000000, 1.000000000000000000 ) ) ;
#59527 = CARTESIAN_POINT ( 'NONE',  ( 12.63842701281683034, 47.46726448433412315, 9.846743663894596210 ) ) ;
#59528 = CARTESIAN_POINT ( 'NONE',  ( 2.791683348922240793, 21.63393115100078745, 7.208316651077764092 ) ) ;
#59529 = CARTESIAN_POINT ( 'NONE',  ( 0.1532563361054082862, 11.21726448433411605, 2.638427012816831674 ) ) ;
#59530 = CARTESIAN_POINT ( 'NONE',  ( 22.26659068614894466, 38.88708216824731068, 7.082119434687054849 ) ) ;
#59531 = DIRECTION ( 'NONE',  ( 1.000000000000000000, 0.000000000000000000, 0.000000000000000000 ) ) ;
#59532 = CARTESIAN_POINT ( 'NONE',  ( 11.04741838685800204, -95.58930130597927644, -3.750000000000000000 ) ) ;
#59533 = DIRECTION ( 'NONE',  ( -0.3826834323650877834, 0.000000000000000000, 0.9238795325112876267 ) ) ;
#59534 = ORIENTED_EDGE ( 'NONE', *, *, #84794, .T. ) ;
#59535 = VERTEX_POINT ( 'NONE', #98801 ) ;
#59536 = AXIS2_PLACEMENT_3D ( 'NONE', #30668, #29195, #54160 ) ;
#59537 = CARTESIAN_POINT ( 'NONE',  ( 17.08211943468705840, 65.13708216824730357, -12.26659068614894466 ) ) ;
#59538 = CARTESIAN_POINT ( 'NONE',  ( 17.08211943468705130, 63.47041550158063927, 12.26659068614894998 ) ) ;
#59539 = CARTESIAN_POINT ( 'NONE',  ( 17.20831665107776587, 34.13393115100078745, -7.208316651077762316 ) ) ;
#59540 = CARTESIAN_POINT ( 'NONE',  ( 3.591859063236763294, 23.29030133659708568, -11.09922568453595026 ) ) ;
#59541 = DIRECTION ( 'NONE',  ( -1.000000000000000000, -2.799047438454523236E-16, 0.000000000000000000 ) ) ;
#59543 = CARTESIAN_POINT ( 'NONE',  ( -2.266590686148945544, 12.22041550158063394, 7.082119434687048631 ) ) ;
#59542 = DIRECTION ( 'NONE',  ( 0.6246950475544238435, 0.7808688094430307203, 0.000000000000000000 ) ) ;
#59544 = CARTESIAN_POINT ( 'NONE',  ( 15.44008868035555260, 9.730352010821505360, 9.422509992056143702 ) ) ;
#59545 = CARTESIAN_POINT ( 'NONE',  ( 17.08211943468705840, 55.13708216824731068, -12.26659068614894466 ) ) ;
#59546 = CARTESIAN_POINT ( 'NONE',  ( 2.791683348922240793, 26.63393115100078745, 7.208316651077764092 ) ) ;
#59547 = CARTESIAN_POINT ( 'NONE',  ( -0.1079698255113996641, 0.1351729006312037407, 6.323366879845591981 ) ) ;
#59548 = CARTESIAN_POINT ( 'NONE',  ( 18.52753015748617571, 8.092264484334117824, 4.923371831947298993 ) ) ;
#59549 = DIRECTION ( 'NONE',  ( 0.000000000000000000, 0.000000000000000000, -1.000000000000000000 ) ) ;
#59550 = CARTESIAN_POINT ( 'NONE',  ( 3.469446951953614189E-15, 12.25893115100078923, 9.846743663894594434 ) ) ;
#59551 = ORIENTED_EDGE ( 'NONE', *, *, #65380, .T. ) ;
#59552 = VERTEX_POINT ( 'NONE', #37783 ) ;
#59553 = CARTESIAN_POINT ( 'NONE',  ( 1.114591949025028450, 15.00000000000000000, -14.45709807627964416 ) ) ;
#59554 = ORIENTED_EDGE ( 'NONE', *, *, #18074, .T. ) ;
#59555 = CARTESIAN_POINT ( 'NONE',  ( 18.52753015748617571, 48.09226448433412315, 4.923371831947298993 ) ) ;
#59556 = CARTESIAN_POINT ( 'NONE',  ( 20.88017736071110164, 25.35535201082150891, 2.915334737309930979 ) ) ;
#59558 = CARTESIAN_POINT ( 'NONE',  ( 0.6178305044545818747, 18.49863466993041428, -9.382169495545419124 ) ) ;
#59557 = CARTESIAN_POINT ( 'NONE',  ( 17.20831665107776587, 62.88393115100078745, 7.208316651077764980 ) ) ;
#59559 =( NAMED_UNIT ( * ) PLANE_ANGLE_UNIT ( ) SI_UNIT ( $, .RADIAN. ) );
#59560 = EDGE_CURVE ( 'NONE', #63305, #19716, #33227, .T. ) ;
#59561 = AXIS2_PLACEMENT_3D ( 'NONE', #53872, #39850, #69863 ) ;
#59562 = AXIS2_PLACEMENT_3D ( 'NONE', #54066, #70072, #40059 ) ;
#59563 = CARTESIAN_POINT ( 'NONE',  ( -2.816281873526471635, 28.91530133659708213, -3.434112377981056508 ) ) ;
#59564 = ORIENTED_EDGE ( 'NONE', *, *, #86071, .T. ) ;
#59565 = AXIS2_PLACEMENT_3D ( 'NONE', #61182, #90691, #82205 ) ;
#59566 = CARTESIAN_POINT ( 'NONE',  ( 10.00000000000000178, 32.25893115100078745, 9.846743663894594434 ) ) ;
#59567 = AXIS2_PLACEMENT_3D ( 'NONE', #85826, #63785, #93315 ) ;
#59568 = CARTESIAN_POINT ( 'NONE',  ( 12.91533473730993009, 11.60535201082150714, -10.88017736071109987 ) ) ;
#59569 = PRESENTATION_LAYER_ASSIGNMENT (  '', '', ( #27654 ) ) ;
#59570 = CARTESIAN_POINT ( 'NONE',  ( -0.8801773607110991993, 7.855352010821506248, -2.915334737309923874 ) ) ;
#59571 = EDGE_LOOP ( 'NONE', ( #1594, #7618, #79497, #30540 ) ) ;
#59572 = CARTESIAN_POINT ( 'NONE',  ( 12.91533473730993009, 46.60535201082150536, -10.88017736071109987 ) ) ;
#59573 = CARTESIAN_POINT ( 'NONE',  ( 15.44008868035555260, 64.73035201082151957, 9.422509992056143702 ) ) ;
#59574 = CARTESIAN_POINT ( 'NONE',  ( 10.00000000000000178, 69.31368534415484817, 10.88017736071110342 ) ) ;
#59575 = VECTOR ( 'NONE', #60510, 1000.000000000000000 ) ;
#59576 = CARTESIAN_POINT ( 'NONE',  ( -0.8801773607111008646, 48.27201867748816966, 2.915334737309923430 ) ) ;
#59577 = DIRECTION ( 'NONE',  ( -1.000000000000000000, 0.000000000000000000, 0.000000000000000000 ) ) ;
#59578 = CARTESIAN_POINT ( 'NONE',  ( -15.61289147378506748, -0.03417435944610275333, -3.480663193108890496 ) ) ;
#59579 = CARTESIAN_POINT ( 'NONE',  ( 5.076628168052703671, 31.84226448433412315, 8.527530157486179263 ) ) ;
#59580 = ORIENTED_EDGE ( 'NONE', *, *, #29117, .T. ) ;
#59581 = CARTESIAN_POINT ( 'NONE',  ( 18.52753015748617571, 58.09226448433411605, 4.923371831947298993 ) ) ;
#59582 = DIRECTION ( 'NONE',  ( 0.000000000000000000, 1.000000000000000000, 0.000000000000000000 ) ) ;
#59583 = CARTESIAN_POINT ( 'NONE',  ( 24.16423886937410614, 9.303748834913967869, 8.672049930838204340E-16 ) ) ;
#59584 = CARTESIAN_POINT ( 'NONE',  ( 12.00809552683959325, 14.49999999999999112, 8.989195838243645653 ) ) ;
#59585 = FACE_OUTER_BOUND ( 'NONE', #25724, .T. ) ;
#59586 = CARTESIAN_POINT ( 'NONE',  ( 1.821158202401655934, 26.16688879859530914, 6.499999999999960920 ) ) ;
#59587 = CARTESIAN_POINT ( 'NONE',  ( 19.42250999205614193, 5.147018677488171434, 5.440088680355555262 ) ) ;
#59588 = CARTESIAN_POINT ( 'NONE',  ( 5.076628168052704559, 50.17559781766745886, -8.527530157486179263 ) ) ;
#59589 = CARTESIAN_POINT ( 'NONE',  ( -3.927832320392065313, -0.03417435944610275333, -13.69797916712109398 ) ) ;
#59591 = TOROIDAL_SURFACE ( 'NONE', #64364, 11.15000000000026326, 0.2500000000000000000 ) ;
#59590 = CARTESIAN_POINT ( 'NONE',  ( 16.40814093676323893, 20.79030133659708923, 11.09922568453595026 ) ) ;
#59592 = CARTESIAN_POINT ( 'NONE',  ( 10.00000000000000178, 12.25893115100078568, 9.846743663894594434 ) ) ;
#59593 = CARTESIAN_POINT ( 'NONE',  ( 2.603489959281581889, 30.43575266056827999, -6.499999999999995559 ) ) ;
#59594 = ADVANCED_FACE ( 'NONE', ( #90763 ), #2924, .T. ) ;
#59595 = CARTESIAN_POINT ( 'NONE',  ( 6.565887622018943937, 5.165301336597086568, 12.81628187352647430 ) ) ;
#59596 = DIRECTION ( 'NONE',  ( 0.000000000000000000, 1.000000000000000000, 0.000000000000000000 ) ) ;
#59597 = TOROIDAL_SURFACE ( 'NONE', #81940, 14.49999999999999822, 0.5000000000000000000 ) ;
#59598 = ADVANCED_FACE ( 'NONE', ( #61250 ), #59363, .T. ) ;
#59599 = ADVANCED_FACE ( 'NONE', ( #79205 ), #25161, .T. ) ;
#59600 = VERTEX_POINT ( 'NONE', #27316 ) ;
#59601 = CARTESIAN_POINT ( 'NONE',  ( 12.91533473730992121, 4.522018677488170546, 10.88017736071110164 ) ) ;
#59602 = CARTESIAN_POINT ( 'NONE',  ( 2.917880565312948704, 17.63708216824730357, 12.26659068614894643 ) ) ;
#59603 = CARTESIAN_POINT ( 'NONE',  ( 17.20831665107776587, 32.88393115100078745, 7.208316651077764980 ) ) ;
#59604 = CARTESIAN_POINT ( 'NONE',  ( 12.91533473730993009, 61.60535201082150536, -10.88017736071109987 ) ) ;
#59606 = CARTESIAN_POINT ( 'NONE',  ( -3.530007528296587704, -1.230351260576522110, -2.750000000000000444 ) ) ;
#59605 = CARTESIAN_POINT ( 'NONE',  ( 16.40814093676324603, 37.45696800326376064, -11.09922568453594671 ) ) ;
#59607 = CARTESIAN_POINT ( 'NONE',  ( 4.559911319644449179, 17.23035201082150536, -9.422509992056141925 ) ) ;
#59608 = DIRECTION ( 'NONE',  ( -1.483861936729427615E-16, 1.000000000000000000, -0.000000000000000000 ) ) ;
#59609 = CARTESIAN_POINT ( 'NONE',  ( -16.94999999999999574, 99.99999999999998579, -8.525133428036873795 ) ) ;
#59610 = CARTESIAN_POINT ( 'NONE',  ( 0.6178305044545818747, 8.498634669930421381, -9.382169495545419124 ) ) ;
#59611 = CARTESIAN_POINT ( 'NONE',  ( 17.20831665107776587, 62.88393115100078745, 7.208316651077764980 ) ) ;
#59612 = CARTESIAN_POINT ( 'NONE',  ( 0.1532563361054083140, 26.00893115100078745, 1.131784320476157264E-15 ) ) ;
#59613 = CARTESIAN_POINT ( 'NONE',  ( 2.915334737309928315, -10.47798132251182857, 10.88017736071109987 ) ) ;
#59614 = CARTESIAN_POINT ( 'NONE',  ( 0.6178305044545838731, 29.74863466993042138, 9.382169495545420901 ) ) ;
#59615 = CARTESIAN_POINT ( 'NONE',  ( 17.62281668512003208, 23.28593319516823001, 6.499999999999993783 ) ) ;
#59617 = CARTESIAN_POINT ( 'NONE',  ( 14.97687855664607781, 0.5000000000000004441, 0.8325315005901553489 ) ) ;
#59616 = CARTESIAN_POINT ( 'NONE',  ( 2.035157376598824452, 33.68868534415484106, 7.964842623401179544 ) ) ;
#59618 = CARTESIAN_POINT ( 'NONE',  ( 19.72487221294570858, 41.86607318730076344, 6.500000000000000888 ) ) ;
#59619 = CARTESIAN_POINT ( 'NONE',  ( 20.88017736071110875, 45.77201867748816966, -2.915334737309920765 ) ) ;
#59620 = CARTESIAN_POINT ( 'NONE',  ( 7.084665262690076126, 42.02201867748816966, -10.88017736071110164 ) ) ;
#59621 = CARTESIAN_POINT ( 'NONE',  ( 0.000000000000000000, 14.49999999999999822, 0.000000000000000000 ) ) ;
#59622 = EDGE_CURVE ( 'NONE', #74673, #84748, #63351, .T. ) ;
#59623 = CARTESIAN_POINT ( 'NONE',  ( 20.88017736071110164, 50.35535201082151247, 2.915334737309930979 ) ) ;
#59624 = COLOUR_RGB ( '', 0.72549020, 0.75294118, 0.79215686) ;
#59625 = VECTOR ( 'NONE', #48629, 1000.000000000000000 ) ;
#59626 = CARTESIAN_POINT ( 'NONE',  ( 1.472469842513823179, 36.42559781766745175, 4.923371831947296329 ) ) ;
#59627 = CARTESIAN_POINT ( 'NONE',  ( 12.91533473730993009, 11.60535201082150536, -10.88017736071109987 ) ) ;
#59628 = CARTESIAN_POINT ( 'NONE',  ( 0.6178305044545838731, 9.748634669930416052, 9.382169495545420901 ) ) ;
#59629 = ORIENTED_EDGE ( 'NONE', *, *, #20467, .T. ) ;
#59630 = CARTESIAN_POINT ( 'NONE',  ( 12.91533473730992121, 29.52201867748817321, 10.88017736071110164 ) ) ;
#59631 = EDGE_CURVE ( 'NONE', #94846, #25948, #86365, .T. ) ;
#59632 = VECTOR ( 'NONE', #21491, 1000.000000000000000 ) ;
#59633 = CARTESIAN_POINT ( 'NONE',  ( 17.39651004071841456, 7.935752660568278216, 6.500000000000003553 ) ) ;
#59634 = CARTESIAN_POINT ( 'NONE',  ( 7.084665262690076126, 2.022018677488170990, -10.88017736071110164 ) ) ;
#59635 = CARTESIAN_POINT ( 'NONE',  ( 10.00000000000000000, 26.81368534415484106, -10.88017736071110342 ) ) ;
#59636 = CARTESIAN_POINT ( 'NONE',  ( -0.8801773607110991993, 67.85535201082151957, -2.915334737309923874 ) ) ;
#59637 = CARTESIAN_POINT ( 'NONE',  ( -0.3689425029237898834, 21.17874883491396432, -10.36894250292378850 ) ) ;
#59638 = CARTESIAN_POINT ( 'NONE',  ( 2.791683348922237240, 10.38393115100078390, -7.208316651077763204 ) ) ;
#59639 = CARTESIAN_POINT ( 'NONE',  ( 19.42250999205614548, 45.98035201082150536, -5.440088680355545492 ) ) ;
#59640 = CIRCLE ( 'NONE', #18618, 2.500000000000002220 ) ;
#59641 = DIRECTION ( 'NONE',  ( -0.000000000000000000, -1.000000000000000000, -0.000000000000000000 ) ) ;
#59642 = CARTESIAN_POINT ( 'NONE',  ( 17.08211943468705130, 3.470415501580634388, 12.26659068614894998 ) ) ;
#59643 = ORIENTED_EDGE ( 'NONE', *, *, #52708, .T. ) ;
#59644 = B_SPLINE_CURVE_WITH_KNOTS ( 'NONE', 3,
 ( #16314, #357, #39804, #38822, #31295, #46798 ),
 .UNSPECIFIED., .F., .F.,
 ( 4, 2, 4 ),
 ( 0.0002800047503720844394, 0.0006862100262544157739, 0.001092415302136747271 ),
 .UNSPECIFIED. ) ;
#59645 = CARTESIAN_POINT ( 'NONE',  ( 11.62719953690064933, 15.00000000000000000, -9.476720473301794456 ) ) ;
#59646 = CARTESIAN_POINT ( 'NONE',  ( 12.63842701281683922, 39.55059781766744464, -9.846743663894590881 ) ) ;
#59647 = ORIENTED_EDGE ( 'NONE', *, *, #14741, .F. ) ;
#59648 = ORIENTED_EDGE ( 'NONE', *, *, #94363, .F. ) ;
#59649 = CARTESIAN_POINT ( 'NONE',  ( 2.917880565312948704, 17.63708216824730357, 12.26659068614894643 ) ) ;
#59650 = CARTESIAN_POINT ( 'NONE',  ( -0.3689425029237881626, 22.42874883491397142, 10.36894250292379027 ) ) ;
#59651 = CARTESIAN_POINT ( 'NONE',  ( 20.88017736071110875, 65.77201867748817676, -2.915334737309920765 ) ) ;
#59652 = CARTESIAN_POINT ( 'NONE',  ( 10.00000000000000000, 65.55374883491396076, -14.16423886937410082 ) ) ;
#59653 = CARTESIAN_POINT ( 'NONE',  ( 0.1532563361054082862, 66.21726448433413736, 2.638427012816831674 ) ) ;
#59654 = CARTESIAN_POINT ( 'NONE',  ( 0.1532563361054082862, 51.21726448433412315, 2.638427012816831674 ) ) ;
#59655 = CARTESIAN_POINT ( 'NONE',  ( -3.836325488036279818, 14.49999999999999822, 14.50112432709419963 ) ) ;
#59657 = CARTESIAN_POINT ( 'NONE',  ( -2.816281873526473856, 9.123634669930421381, 9.499525473075851096E-16 ) ) ;
#59656 = CARTESIAN_POINT ( 'NONE',  ( 7.084665262690076126, 52.02201867748816255, -10.88017736071110164 ) ) ;
#59658 = CARTESIAN_POINT ( 'NONE',  ( 6.204703633549690345, 12.84541550158063572, 14.16423886937410082 ) ) ;
#59659 = CARTESIAN_POINT ( 'NONE',  ( 0.5774900079438590739, 17.64701867748817321, -5.440088680355550821 ) ) ;
#59660 = CARTESIAN_POINT ( 'NONE',  ( -0.8801773607110991993, 22.85535201082150181, -2.915334737309923874 ) ) ;
#59661 = CARTESIAN_POINT ( 'NONE',  ( 18.04007052943772038, 54.00257860105348584, -5.767676674365850076 ) ) ;
#59662 = CARTESIAN_POINT ( 'NONE',  ( 4.559911319644449179, 48.89701867748817676, 9.422509992056141925 ) ) ;
#59663 = CARTESIAN_POINT ( 'NONE',  ( 8.527530157486179263, -26.90773551566588040, 4.923371831947292776 ) ) ;
#59664 = VERTEX_POINT ( 'NONE', #92144 ) ;
#59665 = CARTESIAN_POINT ( 'NONE',  ( 9.240973841163606650, 4.560084876699663581E-16, -11.17382667070372726 ) ) ;
#59666 = ORIENTED_EDGE ( 'NONE', *, *, #93681, .T. ) ;
#59667 = ORIENTED_EDGE ( 'NONE', *, *, #92635, .T. ) ;
#59668 = DIRECTION ( 'NONE',  ( -1.000000000000000000, 0.000000000000000000, 0.000000000000000000 ) ) ;
#59670 = CARTESIAN_POINT ( 'NONE',  ( 17.96484262340118221, 11.18868534415484106, -7.964842623401177768 ) ) ;
#59669 = CARTESIAN_POINT ( 'NONE',  ( 6.204703633549690345, 47.84541550158064638, 14.16423886937410082 ) ) ;
#59672 = CARTESIAN_POINT ( 'NONE',  ( 0.1532563361054100626, 50.80059781766745175, -2.638427012816831230 ) ) ;
#59671 = CARTESIAN_POINT ( 'NONE',  ( 7.361572987183169658, 19.96726448433411960, -9.846743663894592657 ) ) ;
#59673 = CARTESIAN_POINT ( 'NONE',  ( -3.750000000000000000, 78.07179676972445748, 4.250000000000000000 ) ) ;
#59674 = DIRECTION ( 'NONE',  ( 0.5547001962252290364, 0.8320502943378437211, 0.000000000000000000 ) ) ;
#59675 = ADVANCED_FACE ( 'NONE', ( #50822 ), #27814, .F. ) ;
#59676 = CARTESIAN_POINT ( 'NONE',  ( 12.63842701281683922, 4.550597817667451750, -9.846743663894590881 ) ) ;
#59677 = CARTESIAN_POINT ( 'NONE',  ( -5.204170427930421283E-15, 22.87363466993042138, -12.81628187352647608 ) ) ;
#59678 = VERTEX_POINT ( 'NONE', #15672 ) ;
#59679 = CARTESIAN_POINT ( 'NONE',  ( -4.164238869374099039, 31.80374883491396432, 8.674139862899312516E-16 ) ) ;
#59680 = CARTESIAN_POINT ( 'NONE',  ( 22.81628187352648496, 26.83196800326374998, -3.434112377981050290 ) ) ;
#59681 = ORIENTED_EDGE ( 'NONE', *, *, #71236, .F. ) ;
#59682 = CARTESIAN_POINT ( 'NONE',  ( 22.81628187352647785, 46.41530133659708213, 3.434112377981063169 ) ) ;
#59683 = CARTESIAN_POINT ( 'NONE',  ( 1.472469842513823179, 35.59226448433412315, -4.923371831947296329 ) ) ;
#59684 = CARTESIAN_POINT ( 'NONE',  ( 20.88017736071110875, 30.77201867748816966, -2.915334737309920765 ) ) ;
#59685 = CARTESIAN_POINT ( 'NONE',  ( 21.09922568453595559, 62.04030133659709634, -6.408140936763230044 ) ) ;
#59686 = CARTESIAN_POINT ( 'NONE',  ( -29.94000000000000838, 92.00000000000000000, 9.500000000000000000 ) ) ;
#59687 = CARTESIAN_POINT ( 'NONE',  ( 12.63842701281683922, 49.55059781766744464, -9.846743663894590881 ) ) ;
#59688 = CARTESIAN_POINT ( 'NONE',  ( 1.472469842513823179, 56.42559781766745886, 4.923371831947296329 ) ) ;
#59690 = VERTEX_POINT ( 'NONE', #187 ) ;
#59689 = DIRECTION ( 'NONE',  ( 2.569960705150826877E-16, -1.000000000000000000, -0.000000000000000000 ) ) ;
#59691 = ORIENTED_EDGE ( 'NONE', *, *, #59183, .F. ) ;
#59692 = DIRECTION ( 'NONE',  ( 0.000000000000000000, 0.000000000000000000, -1.000000000000000000 ) ) ;
#59693 = VECTOR ( 'NONE', #71223, 1000.000000000000000 ) ;
#59694 = CARTESIAN_POINT ( 'NONE',  ( 8.879999999999991900, 27.04366094290857347, -2.900000000000000799 ) ) ;
#59695 = CARTESIAN_POINT ( 'NONE',  ( 7.361572987183169658, 19.96726448433411960, -9.846743663894592657 ) ) ;
#59696 = CARTESIAN_POINT ( 'NONE',  ( -1.099225684535947600, 34.54030133659708923, 6.408140936763237150 ) ) ;
#59698 = DIRECTION ( 'NONE',  ( 0.000000000000000000, 0.000000000000000000, 1.000000000000000000 ) ) ;
#59697 = AXIS2_PLACEMENT_3D ( 'NONE', #63164, #47685, #9689 ) ;
#59699 = ORIENTED_EDGE ( 'NONE', *, *, #2579, .F. ) ;
#59700 = CARTESIAN_POINT ( 'NONE',  ( 14.92337183194729988, 54.34226448433412315, -8.527530157486177487 ) ) ;
#59701 = CARTESIAN_POINT ( 'NONE',  ( -12.98685442714190508, 4.246409518909109890E-16, -6.449155920601135072 ) ) ;
#59702 = CARTESIAN_POINT ( 'NONE',  ( 7.361572987183170547, 42.05059781766745886, 9.846743663894590881 ) ) ;
#59703 = CARTESIAN_POINT ( 'NONE',  ( 10.00000000000000178, 33.05374883491396787, 14.16423886937410082 ) ) ;
#59704 = CARTESIAN_POINT ( 'NONE',  ( 10.00000000000000000, 49.75893115100078745, -9.846743663894594434 ) ) ;
#59705 = CARTESIAN_POINT ( 'NONE',  ( -1.099225684535947600, 44.54030133659708923, 6.408140936763237150 ) ) ;
#59707 = CARTESIAN_POINT ( 'NONE',  ( 9.010802615327829557, 0.2301505768537819852, 11.91753657575788772 ) ) ;
#59706 = CARTESIAN_POINT ( 'NONE',  ( 20.24186590665276597, 36.76028685723174760, 6.114288769123060518 ) ) ;
#59708 = CARTESIAN_POINT ( 'NONE',  ( 12.63842701281683034, 2.467264484334118269, 9.846743663894596210 ) ) ;
#59709 = EDGE_CURVE ( 'NONE', #66451, #22113, #38179, .T. ) ;
#59710 = CARTESIAN_POINT ( 'NONE',  ( 8.629999999999995453, 40.74999999999999289, 3.750000000000000000 ) ) ;
#59711 = CARTESIAN_POINT ( 'NONE',  ( 19.84674366389459621, 53.50893115100078745, 7.409399052514197653E-17 ) ) ;
#59712 = CARTESIAN_POINT ( 'NONE',  ( 10.00000000000000000, 46.81368534415484106, -10.88017736071110342 ) ) ;
#59713 = CARTESIAN_POINT ( 'NONE',  ( 7.361572987183170547, 42.05059781766745886, 9.846743663894590881 ) ) ;
#59714 = DIRECTION ( 'NONE',  ( 0.9762960071199331402, 0.000000000000000000, 0.2164396139381037087 ) ) ;
#59715 = EDGE_CURVE ( 'NONE', #2137, #98319, #9394, .T. ) ;
#59716 = CARTESIAN_POINT ( 'NONE',  ( 7.084665262690076126, 47.02201867748818387, -10.88017736071110164 ) ) ;
#59717 = EDGE_CURVE ( 'NONE', #39257, #52793, #63690, .T. ) ;
#59718 = ORIENTED_EDGE ( 'NONE', *, *, #31602, .F. ) ;
#59719 = CARTESIAN_POINT ( 'NONE',  ( 8.880000000000020322, 79.82179676972448590, -6.500000000000000888 ) ) ;
#59720 = CARTESIAN_POINT ( 'NONE',  ( 7.084665262690076126, 19.10535201082150181, 10.88017736071109987 ) ) ;
#59722 = CARTESIAN_POINT ( 'NONE',  ( 4.559911319644449179, 38.89701867748817676, 9.422509992056141925 ) ) ;
#59721 = CARTESIAN_POINT ( 'NONE',  ( 22.81628187352648496, 6.831968003263753531, -3.434112377981050290 ) ) ;
#59723 =( NAMED_UNIT ( * ) SI_UNIT ( $, .STERADIAN. ) SOLID_ANGLE_UNIT ( ) );
#59724 = CARTESIAN_POINT ( 'NONE',  ( 10.00000000000000000, 61.81368534415484106, -10.88017736071110342 ) ) ;
#59725 = DIRECTION ( 'NONE',  ( 0.000000000000000000, -1.000000000000000000, 0.000000000000000000 ) ) ;
#59727 = CARTESIAN_POINT ( 'NONE',  ( 8.880000000000020322, 79.82179676972448590, 6.500000000000000888 ) ) ;
#59726 = CARTESIAN_POINT ( 'NONE',  ( 4.559911319644449179, 37.23035201082150536, -9.422509992056141925 ) ) ;
#59728 = CARTESIAN_POINT ( 'NONE',  ( 19.84674366389459266, 8.717264484334116048, -2.638427012816827677 ) ) ;
#59729 = CARTESIAN_POINT ( 'NONE',  ( 5.076628168052704559, 30.17559781766745175, -8.527530157486179263 ) ) ;
#59730 = FILL_AREA_STYLE_COLOUR ( '', #5816 ) ;
#59731 = CARTESIAN_POINT ( 'NONE',  ( 3.795296366450314540, 18.26208216824730712, 14.16423886937410082 ) ) ;
#59732 = CARTESIAN_POINT ( 'NONE',  ( 19.84674366389459266, 63.30059781766745886, 2.638427012816836559 ) ) ;
#59733 = CARTESIAN_POINT ( 'NONE',  ( 13.79529636645030344, 63.26208216824730357, 14.16423886937410614 ) ) ;
#59734 = EDGE_CURVE ( 'NONE', #91147, #63974, #17406, .T. ) ;
#59735 = SURFACE_STYLE_USAGE ( .BOTH. , #23738 ) ;
#59736 = CARTESIAN_POINT ( 'NONE',  ( 2.917880565312948704, 12.63708216824730179, 12.26659068614894643 ) ) ;
#59737 = CARTESIAN_POINT ( 'NONE',  ( 13.79529636645030344, 53.26208216824730357, 14.16423886937410614 ) ) ;
#59738 = CARTESIAN_POINT ( 'NONE',  ( 7.084665262690076126, 2.022018677488170990, -10.88017736071110164 ) ) ;
#59739 = ORIENTED_EDGE ( 'NONE', *, *, #48327, .F. ) ;
#59740 = CARTESIAN_POINT ( 'NONE',  ( 19.84674366389459266, 18.30059781766745175, 2.638427012816836559 ) ) ;
#59741 = CARTESIAN_POINT ( 'NONE',  ( 0.5774900079438607392, 13.48035201082150358, 5.440088680355550821 ) ) ;
#59742 = CARTESIAN_POINT ( 'NONE',  ( 7.361572987183169658, 44.96726448433412315, -9.846743663894592657 ) ) ;
#59744 = FACE_OUTER_BOUND ( 'NONE', #52480, .T. ) ;
#59743 = LINE ( 'NONE', #13261, #64262 ) ;
#59745 = LINE ( 'NONE', #19289, #93508 ) ;
#59746 = CARTESIAN_POINT ( 'NONE',  ( -1.099225684535947600, 29.54030133659708923, 6.408140936763237150 ) ) ;
#59747 = CARTESIAN_POINT ( 'NONE',  ( 14.92337183194729988, 44.34226448433412315, -8.527530157486177487 ) ) ;
#59748 = VERTEX_POINT ( 'NONE', #682 ) ;
#59749 = CARTESIAN_POINT ( 'NONE',  ( 1.472469842513823179, 6.425597817667451750, 4.923371831947296329 ) ) ;
#59750 = EDGE_CURVE ( 'NONE', #12094, #49705, #60651, .T. ) ;
#59751 = CARTESIAN_POINT ( 'NONE',  ( 11.33987066880781036, -87.82218667481943442, -3.999999999998208100 ) ) ;
#59752 = DIRECTION ( 'NONE',  ( 0.6883545756937599069, 0.000000000000000000, -0.7253743710122820820 ) ) ;
#59753 = CARTESIAN_POINT ( 'NONE',  ( -0.8801773607111009756, 8.063685344154837509, 1.068504757029289695E-15 ) ) ;
#59754 = CARTESIAN_POINT ( 'NONE',  ( 6.204703633549690345, 40.76208216824731778, -14.16423886937410259 ) ) ;
#59755 = CARTESIAN_POINT ( 'NONE',  ( 15.44008868035555260, 59.73035201082151247, 9.422509992056143702 ) ) ;
#59756 = FACE_OUTER_BOUND ( 'NONE', #74551, .T. ) ;
#59757 = CARTESIAN_POINT ( 'NONE',  ( 5.076628168052704559, 25.17559781766745175, -8.527530157486179263 ) ) ;
#59758 =( NAMED_UNIT ( * ) SI_UNIT ( $, .STERADIAN. ) SOLID_ANGLE_UNIT ( ) );
#59759 = CARTESIAN_POINT ( 'NONE',  ( 5.076628168052703671, 1.842264484334118047, 8.527530157486179263 ) ) ;
#59760 = CARTESIAN_POINT ( 'NONE',  ( 4.856092091438321212, -3.602007608198911403E-15, -13.79590085420553081 ) ) ;
#59761 = CARTESIAN_POINT ( 'NONE',  ( 0.1532563361054100626, 40.80059781766745886, -2.638427012816831230 ) ) ;
#59762 = CARTESIAN_POINT ( 'NONE',  ( 7.084665262690076126, 34.10535201082151247, 10.88017736071109987 ) ) ;
#59763 = ORIENTED_EDGE ( 'NONE', *, *, #82293, .F. ) ;
#59764 = CARTESIAN_POINT ( 'NONE',  ( 21.09922568453594849, 61.20696800326376064, 6.408140936763242479 ) ) ;
#59765 = DIRECTION ( 'NONE',  ( 1.000000000000000000, 0.000000000000000000, 0.000000000000000000 ) ) ;
#59766 = VECTOR ( 'NONE', #89958, 1000.000000000000000 ) ;
#59767 = B_SPLINE_CURVE_WITH_KNOTS ( 'NONE', 3,
 ( #21415, #13919, #5440, #34919 ),
 .UNSPECIFIED., .F., .F.,
 ( 4, 4 ),
 ( 3.469446951953614189E-18, 0.002562518741975320334 ),
 .UNSPECIFIED. ) ;
#59768 = CARTESIAN_POINT ( 'NONE',  ( 19.84674366389459266, 13.71726448433411782, -2.638427012816827677 ) ) ;
#59769 = CARTESIAN_POINT ( 'NONE',  ( 3.591859063236761518, 49.95696800326375353, 11.09922568453594849 ) ) ;
#59771 = CARTESIAN_POINT ( 'NONE',  ( 1.472469842513823179, 40.59226448433411605, -4.923371831947296329 ) ) ;
#59770 = CARTESIAN_POINT ( 'NONE',  ( 19.42250999205614548, 10.98035201082150536, -5.440088680355545492 ) ) ;
#59772 = DIRECTION ( 'NONE',  ( 1.000000000000000000, 1.387778780781444413E-14, 0.000000000000000000 ) ) ;
#59773 = SURFACE_STYLE_FILL_AREA ( #6785 ) ;
#59774 = CARTESIAN_POINT ( 'NONE',  ( 24.16423886937409904, 49.09541550158063217, 3.795296366450317205 ) ) ;
#59775 = CARTESIAN_POINT ( 'NONE',  ( 19.84674366389459621, 63.50893115100078745, 7.409399052514197653E-17 ) ) ;
#59776 = DIRECTION ( 'NONE',  ( -1.000000000000000000, 0.000000000000000000, 0.000000000000000000 ) ) ;
#59777 = CARTESIAN_POINT ( 'NONE',  ( 19.42250999205614548, 35.98035201082151247, -5.440088680355545492 ) ) ;
#59778 = AXIS2_PLACEMENT_3D ( 'NONE', #16093, #74612, #38118 ) ;
#59779 = CARTESIAN_POINT ( 'NONE',  ( 1.472469842513823179, 6.425597817667451750, 4.923371831947296329 ) ) ;
#59780 = CARTESIAN_POINT ( 'NONE',  ( -3.586264863029322569, -2.711807932117639819, 3.999999999999596323 ) ) ;
#59781 = EDGE_LOOP ( 'NONE', ( #8829, #88385, #71706, #88169 ) ) ;
#59782 = CARTESIAN_POINT ( 'NONE',  ( 22.81628187352647785, 61.41530133659709634, 3.434112377981063169 ) ) ;
#59783 = CARTESIAN_POINT ( 'NONE',  ( 2.035157376598822676, 62.43868534415483396, -7.964842623401177768 ) ) ;
#59784 = ORIENTED_EDGE ( 'NONE', *, *, #63780, .T. ) ;
#59785 = CARTESIAN_POINT ( 'NONE',  ( 24.16423886937409904, 9.095415501580633943, 3.795296366450317205 ) ) ;
#59786 = CARTESIAN_POINT ( 'NONE',  ( 12.63842701281683034, 12.46726448433411782, 9.846743663894596210 ) ) ;
#59787 = CARTESIAN_POINT ( 'NONE',  ( 15.33206046421389601, 15.00000000000000000, 4.561284726668865197 ) ) ;
#59788 = ORIENTED_EDGE ( 'NONE', *, *, #31761, .F. ) ;
#59789 =( BOUNDED_CURVE ( )  B_SPLINE_CURVE ( 2, ( #98199, #60165, #53655, #54138, #23676, #25155, #47124, #69649, #62615 ),
 .UNSPECIFIED., .F., .T. ) 
 B_SPLINE_CURVE_WITH_KNOTS ( ( 3, 2, 2, 2, 3 ),
 ( 0.1187123655116599508, 0.1190476190476190688, 0.1250000000000000000, 0.1309523809523809312, 0.1312876344883400492 ),
 .UNSPECIFIED. ) 
 CURVE ( )  GEOMETRIC_REPRESENTATION_ITEM ( )  RATIONAL_B_SPLINE_CURVE ( ( 0.9963778908391762723, 0.9980808541467921513, 1.000000000000000000, 0.9659258262890682012, 1.000000000000000000, 0.9659258262890682012, 1.000000000000000000, 0.9980808541467922623, 0.9963778908391763833 ) ) 
 REPRESENTATION_ITEM ( '' )  );
#59790 = CARTESIAN_POINT ( 'NONE',  ( 15.44008868035555793, 26.39701867748817321, -9.422509992056140149 ) ) ;
#59791 = ORIENTED_EDGE ( 'NONE', *, *, #92673, .F. ) ;
#59792 = CARTESIAN_POINT ( 'NONE',  ( 7.084665262690076126, 34.10535201082151247, 10.88017736071109987 ) ) ;
#59793 = DIRECTION ( 'NONE',  ( -0.5547001962252291474, -0.8320502943378437211, -0.000000000000000000 ) ) ;
#59794 = ORIENTED_EDGE ( 'NONE', *, *, #18281, .F. ) ;
#59795 = VERTEX_POINT ( 'NONE', #22179 ) ;
#59796 = EDGE_CURVE ( 'NONE', #50559, #80095, #16088, .T. ) ;
#59797 = CARTESIAN_POINT ( 'NONE',  ( 20.88017736071110164, 60.35535201082151957, 2.915334737309930979 ) ) ;
#59798 = CARTESIAN_POINT ( 'NONE',  ( 5.076628168052704559, 60.17559781766745175, -8.527530157486179263 ) ) ;
#59800 = LINE ( 'NONE', #23807, #7999 ) ;
#59799 = CARTESIAN_POINT ( 'NONE',  ( 15.44008868035555260, 24.73035201082150891, 9.422509992056143702 ) ) ;
#59801 = CARTESIAN_POINT ( 'NONE',  ( 10.00000000000000178, 7.258931151000785675, 9.846743663894594434 ) ) ;
#59802 = CARTESIAN_POINT ( 'NONE',  ( 7.084665262690076126, 19.10535201082150181, 10.88017736071109987 ) ) ;
#59803 = ADVANCED_FACE ( 'NONE', ( #54131 ), #53156, .T. ) ;
#59804 = VERTEX_POINT ( 'NONE', #65806 ) ;
#59805 = CARTESIAN_POINT ( 'NONE',  ( 19.38216949554541202, 55.99863466993041072, 9.382169495545424454 ) ) ;
#59806 = CARTESIAN_POINT ( 'NONE',  ( 12.91533473730993009, 41.60535201082149825, -10.88017736071109987 ) ) ;
#59807 = CARTESIAN_POINT ( 'NONE',  ( -46.94000000000001194, 100.4376529975800025, -8.999999999986080468 ) ) ;
#59808 = CARTESIAN_POINT ( 'NONE',  ( 22.81628187352647785, 56.62363466993042493, 6.195893100308588602E-16 ) ) ;
#59809 = CARTESIAN_POINT ( 'NONE',  ( 15.44008868035555793, 41.39701867748817676, -9.422509992056140149 ) ) ;
#59810 = CARTESIAN_POINT ( 'NONE',  ( 16.40814093676323893, 0.7903013365970867898, 11.09922568453595026 ) ) ;
#59811 = DIRECTION ( 'NONE',  ( 0.000000000000000000, -1.000000000000000000, 0.000000000000000000 ) ) ;
#59812 = CARTESIAN_POINT ( 'NONE',  ( 2.791683348922237240, 15.38393115100078212, -7.208316651077763204 ) ) ;
#59814 = PRESENTATION_LAYER_ASSIGNMENT (  '', '', ( #56693 ) ) ;
#59813 = CARTESIAN_POINT ( 'NONE',  ( 13.43411237798105340, 10.58196800326375353, 12.81628187352647963 ) ) ;
#59816 = CARTESIAN_POINT ( 'NONE',  ( 19.84674366389459266, 63.71726448433412315, -2.638427012816827677 ) ) ;
#59815 = DIRECTION ( 'NONE',  ( -0.000000000000000000, -1.000000000000000000, 0.000000000000000000 ) ) ;
#59817 = CARTESIAN_POINT ( 'NONE',  ( 2.035157376598824452, 38.68868534415483396, 7.964842623401179544 ) ) ;
#59818 = CARTESIAN_POINT ( 'NONE',  ( 18.52753015748618282, 43.92559781766745175, -4.923371831947291888 ) ) ;
#59819 = FACE_OUTER_BOUND ( 'NONE', #78598, .T. ) ;
#59820 = CARTESIAN_POINT ( 'NONE',  ( 17.20831665107776587, 17.88393115100078745, 7.208316651077764980 ) ) ;
#59821 = CARTESIAN_POINT ( 'NONE',  ( 19.84674366389459266, 8.300597817667451750, 2.638427012816836559 ) ) ;
#59823 = VERTEX_POINT ( 'NONE', #45659 ) ;
#59822 = CARTESIAN_POINT ( 'NONE',  ( -1.099225684535947600, 9.540301336597087456, 6.408140936763237150 ) ) ;
#59824 = B_SPLINE_CURVE_WITH_KNOTS ( 'NONE', 3,
 ( #8396, #77369, #91395, #92380, #83411, #8880 ),
 .UNSPECIFIED., .F., .F.,
 ( 4, 2, 4 ),
 ( 0.0002800553958269931185, 0.0006862611673083514937, 0.001092466938789709869 ),
 .UNSPECIFIED. ) ;
#59825 = CARTESIAN_POINT ( 'NONE',  ( 12.63842701281683922, 59.55059781766744464, -9.846743663894590881 ) ) ;
#59826 = EDGE_CURVE ( 'NONE', #91690, #19964, #58299, .T. ) ;
#59827 = CARTESIAN_POINT ( 'NONE',  ( -1.099225684535947600, 58.70696800326375353, -6.408140936763238038 ) ) ;
#59828 = CARTESIAN_POINT ( 'NONE',  ( 2.791683348922237240, 30.38393115100078390, -7.208316651077763204 ) ) ;
#59829 = STYLED_ITEM ( 'NONE', ( #2815 ), #72777 ) ;
#59830 = CARTESIAN_POINT ( 'NONE',  ( 12.91533473730993009, 11.60535201082150714, -10.88017736071109987 ) ) ;
#59831 = CARTESIAN_POINT ( 'NONE',  ( 19.84674366389459266, 48.71726448433413026, -2.638427012816827677 ) ) ;
#59832 = AXIS2_PLACEMENT_3D ( 'NONE', #73379, #28384, #11410 ) ;
#59833 = ADVANCED_FACE ( 'NONE', ( #10615 ), #86616, .T. ) ;
#59834 = ORIENTED_EDGE ( 'NONE', *, *, #97920, .T. ) ;
#59835 = LINE ( 'NONE', #66852, #96759 ) ;
#59836 = VECTOR ( 'NONE', #28392, 1000.000000000000000 ) ;
#59837 = CARTESIAN_POINT ( 'NONE',  ( 24.16423886937410614, 64.30374883491396076, 8.672049930838204340E-16 ) ) ;
#59838 = CARTESIAN_POINT ( 'NONE',  ( 0.1532563361054083140, 6.008931151000784787, 1.131784320476157264E-15 ) ) ;
#59839 = CARTESIAN_POINT ( 'NONE',  ( 19.42250999205614193, 20.14701867748817321, 5.440088680355555262 ) ) ;
#59840 = CARTESIAN_POINT ( 'NONE',  ( 13.79529636645030344, 53.26208216824730357, 14.16423886937410614 ) ) ;
#59842 = DIRECTION ( 'NONE',  ( -0.000000000000000000, -0.000000000000000000, 1.000000000000000000 ) ) ;
#59841 = CARTESIAN_POINT ( 'NONE',  ( -4.164238869374099039, 51.80374883491396787, 8.674139862899312516E-16 ) ) ;
#59843 = CARTESIAN_POINT ( 'NONE',  ( 17.20831665107776587, 4.133931151000785675, -7.208316651077762316 ) ) ;
#59844 = AXIS2_PLACEMENT_3D ( 'NONE', #43728, #27243, #66731 ) ;
#59845 = CARTESIAN_POINT ( 'NONE',  ( 17.20831665107776587, 24.13393115100078035, -7.208316651077762316 ) ) ;
#59846 = CARTESIAN_POINT ( 'NONE',  ( -2.816281873526473856, 4.331968003263754419, 3.434112377981055619 ) ) ;
#59847 = ORIENTED_EDGE ( 'NONE', *, *, #6932, .T. ) ;
#59848 = CYLINDRICAL_SURFACE ( 'NONE', #10657, 6.999999999999995559 ) ;
#59849 = DIRECTION ( 'NONE',  ( 0.000000000000000000, 0.000000000000000000, -1.000000000000000000 ) ) ;
#59850 = CARTESIAN_POINT ( 'NONE',  ( 17.20831665107776587, 59.13393115100078745, -7.208316651077762316 ) ) ;
#59851 = DIRECTION ( 'NONE',  ( 0.000000000000000000, 0.000000000000000000, -1.000000000000000000 ) ) ;
#59852 = SPHERICAL_SURFACE ( 'NONE', #56297, 0.5000000000000000000 ) ;
#59854 = CARTESIAN_POINT ( 'NONE',  ( 10.00000000000000000, 10.55374883491396787, -14.16423886937410082 ) ) ;
#59853 =( BOUNDED_CURVE ( )  B_SPLINE_CURVE ( 2, ( #77784, #98359, #83326, #14852, #7342, #23336, #24806, #48268, #93282 ),
 .UNSPECIFIED., .F., .F. ) 
 B_SPLINE_CURVE_WITH_KNOTS ( ( 3, 2, 2, 2, 3 ),
 ( 0.5115695083688026612, 0.5119047619047618625, 0.5178571428571427937, 0.5238095238095238360, 0.5241447773454830372 ),
 .UNSPECIFIED. ) 
 CURVE ( )  GEOMETRIC_REPRESENTATION_ITEM ( )  RATIONAL_B_SPLINE_CURVE ( ( 0.9963778908391753841, 0.9980808541467917072, 1.000000000000000000, 0.9659258262890682012, 1.000000000000000000, 0.9659258262890682012, 1.000000000000000000, 0.9980808541467917072, 0.9963778908391753841 ) ) 
 REPRESENTATION_ITEM ( '' )  );
#59855 = CARTESIAN_POINT ( 'NONE',  ( 7.361572987183170547, 27.05059781766745175, 9.846743663894590881 ) ) ;
#59856 = LINE ( 'NONE', #45349, #44891 ) ;
#59857 = ORIENTED_EDGE ( 'NONE', *, *, #97438, .F. ) ;
#59858 = CARTESIAN_POINT ( 'NONE',  ( 6.204703633549690345, 35.76208216824729647, -14.16423886937410259 ) ) ;
#59859 = CARTESIAN_POINT ( 'NONE',  ( 18.52753015748618282, 3.925597817667451306, -4.923371831947291888 ) ) ;
#59861 = CARTESIAN_POINT ( 'NONE',  ( -2.189108318723541391, -3.647747387350642832E-15, -14.46085460646901666 ) ) ;
#59860 = FACE_OUTER_BOUND ( 'NONE', #51516, .T. ) ;
#59862 = CARTESIAN_POINT ( 'NONE',  ( 15.44008868035555260, 29.73035201082150891, 9.422509992056143702 ) ) ;
#59863 = CARTESIAN_POINT ( 'NONE',  ( -2.816281873526473856, 34.33196800326376064, 3.434112377981055619 ) ) ;
#59864 = CARTESIAN_POINT ( 'NONE',  ( 20.88017736071110164, 5.355352010821502695, 2.915334737309930979 ) ) ;
#59865 = CARTESIAN_POINT ( 'NONE',  ( 22.81628187352647785, 36.41530133659707502, 3.434112377981063169 ) ) ;
#59866 = CARTESIAN_POINT ( 'NONE',  ( 0.6178305044545818747, 63.49863466993043204, -9.382169495545419124 ) ) ;
#59867 = ORIENTED_EDGE ( 'NONE', *, *, #17104, .F. ) ;
#59868 = EDGE_CURVE ( 'NONE', #28932, #15789, #79623, .T. ) ;
#59869 = CARTESIAN_POINT ( 'NONE',  ( 19.80777595082613729, 35.68878173731741299, -6.500000000000036415 ) ) ;
#59870 = CARTESIAN_POINT ( 'NONE',  ( 24.16423886937410614, 44.30374883491397497, 8.672049930838204340E-16 ) ) ;
#59871 =( LENGTH_UNIT ( ) NAMED_UNIT ( * ) SI_UNIT ( .MILLI., .METRE. ) );
#59872 = CARTESIAN_POINT ( 'NONE',  ( 7.084665262690076126, 29.10535201082150181, 10.88017736071109987 ) ) ;
#59873 = DIRECTION ( 'NONE',  ( 0.000000000000000000, 0.000000000000000000, -1.000000000000000000 ) ) ;
#59874 =( NAMED_UNIT ( * ) PLANE_ANGLE_UNIT ( ) SI_UNIT ( $, .RADIAN. ) );
#59875 = CARTESIAN_POINT ( 'NONE',  ( 19.42250999205614548, 50.98035201082151247, -5.440088680355545492 ) ) ;
#59876 = DIRECTION ( 'NONE',  ( 1.000000000000000000, 0.000000000000000000, -0.000000000000000000 ) ) ;
#59877 = CARTESIAN_POINT ( 'NONE',  ( 21.09922568453594849, 26.20696800326375353, 6.408140936763242479 ) ) ;
#59878 = FACE_OUTER_BOUND ( 'NONE', #78904, .T. ) ;
#59879 = CARTESIAN_POINT ( 'NONE',  ( -5.963430220938290560, 1.828790035174478135, -10.32896413005679648 ) ) ;
#59880 = CARTESIAN_POINT ( 'NONE',  ( 12.63842701281683922, 29.55059781766745175, -9.846743663894590881 ) ) ;
#59881 = AXIS2_PLACEMENT_3D ( 'NONE', #72577, #64579, #27081 ) ;
#59882 = CARTESIAN_POINT ( 'NONE',  ( -0.8801773607110991993, 52.85535201082151247, -2.915334737309923874 ) ) ;
#59883 = CARTESIAN_POINT ( 'NONE',  ( 6.565887622018943937, 23.08196800326375708, -12.81628187352647608 ) ) ;
#59884 = CARTESIAN_POINT ( 'NONE',  ( 4.559911319644449179, 7.230352010821504471, -9.422509992056141925 ) ) ;
#59885 = CARTESIAN_POINT ( 'NONE',  ( 10.00000000000000000, 34.75893115100078745, -9.846743663894594434 ) ) ;
#59886 = CARTESIAN_POINT ( 'NONE',  ( 21.09922568453595559, 62.04030133659709634, -6.408140936763230044 ) ) ;
#59887 = CARTESIAN_POINT ( 'NONE',  ( 19.84674366389459266, 13.71726448433411782, -2.638427012816827677 ) ) ;
#59888 = CARTESIAN_POINT ( 'NONE',  ( 24.16423886937410614, 9.512082168247301794, -3.795296366450302550 ) ) ;
#59889 = CARTESIAN_POINT ( 'NONE',  ( -8.375939845167600595, -0.03417435944610275333, -11.52849216984310310 ) ) ;
#59890 = CARTESIAN_POINT ( 'NONE',  ( 12.91533473730992121, 39.52201867748817676, 10.88017736071110164 ) ) ;
#59892 = CARTESIAN_POINT ( 'NONE',  ( 24.16423886937410614, 34.51208216824731068, -3.795296366450302550 ) ) ;
#59891 = CARTESIAN_POINT ( 'NONE',  ( 2.035157376598822676, 2.438685344154837953, -7.964842623401177768 ) ) ;
#59893 = CARTESIAN_POINT ( 'NONE',  ( 17.20831665107776587, 42.88393115100077324, 7.208316651077764980 ) ) ;
#59894 = CARTESIAN_POINT ( 'NONE',  ( 4.559911319644449179, 37.23035201082150536, -9.422509992056141925 ) ) ;
#59895 = CARTESIAN_POINT ( 'NONE',  ( 0.5774900079438590739, 22.64701867748817321, -5.440088680355550821 ) ) ;
#59896 = ORIENTED_EDGE ( 'NONE', *, *, #56714, .F. ) ;
#59897 = CARTESIAN_POINT ( 'NONE',  ( 19.42250999205614193, 30.14701867748817321, 5.440088680355555262 ) ) ;
#59898 = CARTESIAN_POINT ( 'NONE',  ( 19.38216949554541557, 47.24863466993041783, -9.382169495545420901 ) ) ;
#59899 = CARTESIAN_POINT ( 'NONE',  ( 20.88017736071110875, 40.77201867748818387, -2.915334737309920765 ) ) ;
#59901 = CARTESIAN_POINT ( 'NONE',  ( 10.00000000000000178, 34.31368534415484106, 10.88017736071110342 ) ) ;
#59900 = FILL_AREA_STYLE ('',( #37921 ) ) ;
#59902 = B_SPLINE_CURVE_WITH_KNOTS ( 'NONE', 3,
 ( #77309, #8823, #33761, #10799, #2337, #55811 ),
 .UNSPECIFIED., .F., .F.,
 ( 4, 2, 4 ),
 ( 0.000000000000000000, 0.0004056965545342633298, 0.0008113931090685266596 ),
 .UNSPECIFIED. ) ;
#59903 = EDGE_LOOP ( 'NONE', ( #66210, #7189, #91590, #75779, #11456, #72609 ) ) ;
#59904 = CARTESIAN_POINT ( 'NONE',  ( 2.791683348922237240, 60.38393115100078745, -7.208316651077763204 ) ) ;
#59905 = CARTESIAN_POINT ( 'NONE',  ( 17.96484262340118221, 41.18868534415484106, -7.964842623401177768 ) ) ;
#59906 = FILL_AREA_STYLE_COLOUR ( '', #89686 ) ;
#59907 = DIRECTION ( 'NONE',  ( 0.000000000000000000, 0.000000000000000000, 1.000000000000000000 ) ) ;
#59908 = CARTESIAN_POINT ( 'NONE',  ( 13.79529636645031943, 45.34541550158062506, -14.16423886937409904 ) ) ;
#59909 = CARTESIAN_POINT ( 'NONE',  ( 4.559911319644449179, 58.89701867748817676, 9.422509992056141925 ) ) ;
#59910 = CARTESIAN_POINT ( 'NONE',  ( 20.03932841506544804, 25.62161441960502017, -6.397827110478938373 ) ) ;
#59911 = MECHANICAL_DESIGN_GEOMETRIC_PRESENTATION_REPRESENTATION (  '', ( #10389 ), #5612 ) ;
#59912 = LINE ( 'NONE', #42955, #25403 ) ;
#59913 = CARTESIAN_POINT ( 'NONE',  ( 5.076628168052703671, 66.84226448433412315, 8.527530157486179263 ) ) ;
#59914 = CARTESIAN_POINT ( 'NONE',  ( -8.000000000000000000, 80.32179676972448590, -3.750000000000000000 ) ) ;
#59915 = CARTESIAN_POINT ( 'NONE',  ( 0.1532563361054100626, 30.80059781766744820, -2.638427012816831230 ) ) ;
#59916 = VERTEX_POINT ( 'NONE', #64081 ) ;
#59917 = CARTESIAN_POINT ( 'NONE',  ( 0.1532563361054100626, 15.80059781766745353, -2.638427012816831230 ) ) ;
#59918 = CARTESIAN_POINT ( 'NONE',  ( 12.81628187352647252, -23.16803199673623936, -3.434112377981059172 ) ) ;
#59919 = CARTESIAN_POINT ( 'NONE',  ( 20.88017736071110164, 30.35535201082151247, 2.915334737309930979 ) ) ;
#59920 = CARTESIAN_POINT ( 'NONE',  ( 2.791683348922240793, 26.63393115100078745, 7.208316651077764092 ) ) ;
#59921 = CARTESIAN_POINT ( 'NONE',  ( -1.099225684535947600, 18.70696800326375353, -6.408140936763238038 ) ) ;
#59923 = CARTESIAN_POINT ( 'NONE',  ( 2.035157376598824452, 63.68868534415484106, 7.964842623401179544 ) ) ;
#59922 = DIRECTION ( 'NONE',  ( 0.000000000000000000, 1.000000000000000000, 0.000000000000000000 ) ) ;
#59925 = CARTESIAN_POINT ( 'NONE',  ( 7.084665262690076126, 2.022018677488170990, -10.88017736071110164 ) ) ;
#59924 = CARTESIAN_POINT ( 'NONE',  ( 10.00000000000000000, 36.81368534415484106, -10.88017736071110342 ) ) ;
#59926 = CARTESIAN_POINT ( 'NONE',  ( -4.164238869374099039, 41.80374883491397497, 8.674139862899312516E-16 ) ) ;
#59927 = EDGE_CURVE ( 'NONE', #6299, #64876, #42938, .T. ) ;
#59928 = COLOUR_RGB ( '', 0.40784314, 0.44705882, 0.49803922) ;
#59929 = CARTESIAN_POINT ( 'NONE',  ( -45.94000000000001194, 103.9981609152045507, 5.961202730336935041 ) ) ;
#59930 = EDGE_LOOP ( 'NONE', ( #78986, #62714, #78943, #43693 ) ) ;
#59931 = CARTESIAN_POINT ( 'NONE',  ( -2.816281873526471635, 8.915301336597083903, -3.434112377981056508 ) ) ;
#59932 = CARTESIAN_POINT ( 'NONE',  ( 10.00000000000000178, 9.313685344154839285, 10.88017736071110342 ) ) ;
#59933 = CARTESIAN_POINT ( 'NONE',  ( 0.5774900079438590739, 52.64701867748817676, -5.440088680355550821 ) ) ;
#59934 = EDGE_LOOP ( 'NONE', ( #45427, #71106, #36320, #64840 ) ) ;
#59935 = CARTESIAN_POINT ( 'NONE',  ( 0.5774900079438590739, 52.64701867748817676, -5.440088680355550821 ) ) ;
#59936 = CARTESIAN_POINT ( 'NONE',  ( 2.791683348922237240, 30.38393115100078390, -7.208316651077763204 ) ) ;
#59937 = CARTESIAN_POINT ( 'NONE',  ( 19.84674366389459621, 23.50893115100078390, 7.409399052514197653E-17 ) ) ;
#59938 = CARTESIAN_POINT ( 'NONE',  ( 10.00000000000000178, 12.25893115100078568, 9.846743663894594434 ) ) ;
#59939 = VECTOR ( 'NONE', #61809, 1000.000000000000114 ) ;
#59941 = CARTESIAN_POINT ( 'NONE',  ( 0.6178305044545838731, 39.74863466993041072, 9.382169495545420901 ) ) ;
#59940 = CARTESIAN_POINT ( 'NONE',  ( -6.606690058690507961, -50.93246948815529151, 2.750000000000000000 ) ) ;
#59943 = DIRECTION ( 'NONE',  ( 0.000000000000000000, -0.000000000000000000, -1.000000000000000000 ) ) ;
#59942 = CARTESIAN_POINT ( 'NONE',  ( 1.472469842513823179, 1.425597817667451528, 4.923371831947296329 ) ) ;
#59944 = CARTESIAN_POINT ( 'NONE',  ( 5.365133693937636394, -17.52547282955412911, -4.000000000000000888 ) ) ;
#59946 = VERTEX_POINT ( 'NONE', #48107 ) ;
#59945 = CARTESIAN_POINT ( 'NONE',  ( 19.84674366389459266, 33.71726448433410894, -2.638427012816827677 ) ) ;
#59947 = CARTESIAN_POINT ( 'NONE',  ( 13.43411237798106583, 52.66530133659708213, -12.81628187352647252 ) ) ;
#59948 = CARTESIAN_POINT ( 'NONE',  ( 7.007880867418011306, -58.32092081208355694, 4.000000000000000000 ) ) ;
#59949 = ADVANCED_FACE ( 'NONE', ( #1166 ), #17636, .F. ) ;
#59950 = CARTESIAN_POINT ( 'NONE',  ( 16.40814093676323893, 10.79030133659708923, 11.09922568453595026 ) ) ;
#59951 = CIRCLE ( 'NONE', #88711, 1.499999999999996669 ) ;
#59952 = CARTESIAN_POINT ( 'NONE',  ( 7.084665262690076126, 47.02201867748818387, -10.88017736071110164 ) ) ;
#59953 = CARTESIAN_POINT ( 'NONE',  ( 2.917880565312948704, 27.63708216824730357, 12.26659068614894643 ) ) ;
#59954 = EDGE_CURVE ( 'NONE', #1208, #70377, #95608, .T. ) ;
#59955 = LINE ( 'NONE', #59463, #80751 ) ;
#59956 = CARTESIAN_POINT ( 'NONE',  ( -0.3689425029237881626, 27.42874883491397142, 10.36894250292379027 ) ) ;
#59957 = CARTESIAN_POINT ( 'NONE',  ( 2.917880565312950480, 40.97041550158063217, -12.26659068614894821 ) ) ;
#59958 = CARTESIAN_POINT ( 'NONE',  ( -0.3689425029237898834, 6.178748834913968757, -10.36894250292378850 ) ) ;
#59960 = CARTESIAN_POINT ( 'NONE',  ( 7.084665262690076126, 69.10535201082151957, 10.88017736071109987 ) ) ;
#59959 = CARTESIAN_POINT ( 'NONE',  ( -4.164238869374099927, 12.01208216824730357, 3.795296366450308767 ) ) ;
#59961 = CARTESIAN_POINT ( 'NONE',  ( 7.084665262690076126, 52.02201867748816255, -10.88017736071110164 ) ) ;
#59962 = CARTESIAN_POINT ( 'NONE',  ( 14.82679024690670566, 0.2306972965111901697, 1.845086899513388001 ) ) ;
#59963 = CARTESIAN_POINT ( 'NONE',  ( 10.00000000000000178, 27.25893115100078390, 9.846743663894594434 ) ) ;
#59965 = CARTESIAN_POINT ( 'NONE',  ( 14.92337183194729988, 24.34226448433411960, -8.527530157486177487 ) ) ;
#59964 = CARTESIAN_POINT ( 'NONE',  ( -0.8801773607110991993, 67.85535201082151957, -2.915334737309923874 ) ) ;
#59966 = CARTESIAN_POINT ( 'NONE',  ( -0.8801773607110991993, 27.85535201082150181, -2.915334737309923874 ) ) ;
#59967 = CARTESIAN_POINT ( 'NONE',  ( 22.81628187352647785, 56.41530133659708213, 3.434112377981063169 ) ) ;
#59968 = CARTESIAN_POINT ( 'NONE',  ( 10.00000000000000178, 67.25893115100079456, 9.846743663894594434 ) ) ;
#59969 = CARTESIAN_POINT ( 'NONE',  ( 2.791683348922237240, 25.38393115100078390, -7.208316651077763204 ) ) ;
#59970 = CARTESIAN_POINT ( 'NONE',  ( 16.40814093676324603, 42.45696800326375353, -11.09922568453594671 ) ) ;
#59972 = AXIS2_PLACEMENT_3D ( 'NONE', #51546, #96569, #95570 ) ;
#59971 = CARTESIAN_POINT ( 'NONE',  ( -10.36894250292379205, -13.82125116508603035, -10.36894250292378672 ) ) ;
#59973 = CARTESIAN_POINT ( 'NONE',  ( 4.559911319644449179, 38.89701867748817676, 9.422509992056141925 ) ) ;
#59974 = CARTESIAN_POINT ( 'NONE',  ( 1.472469842513823179, 46.42559781766745175, 4.923371831947296329 ) ) ;
#59975 = AXIS2_PLACEMENT_3D ( 'NONE', #57375, #18905, #18407 ) ;
#59976 = CARTESIAN_POINT ( 'NONE',  ( 2.917880565312948704, 32.63708216824730357, 12.26659068614894643 ) ) ;
#59977 = ORIENTED_EDGE ( 'NONE', *, *, #1966, .T. ) ;
#59978 = TOROIDAL_SURFACE ( 'NONE', #64740, 2.899999999999999467, 0.1000000000000000056 ) ;
#59979 = FACE_OUTER_BOUND ( 'NONE', #22496, .T. ) ;
#59980 = CARTESIAN_POINT ( 'NONE',  ( 20.88017736071110875, 60.77201867748817676, -2.915334737309920765 ) ) ;
#59981 = CARTESIAN_POINT ( 'NONE',  ( -2.266590686148945544, 57.22041550158063217, 7.082119434687048631 ) ) ;
#59982 = CARTESIAN_POINT ( 'NONE',  ( 18.52753015748617571, 63.09226448433412315, 4.923371831947298993 ) ) ;
#59983 = CARTESIAN_POINT ( 'NONE',  ( 0.2751277870542911952, 53.21833443783938122, 6.499999999999992006 ) ) ;
#59984 = CARTESIAN_POINT ( 'NONE',  ( 15.44008868035555793, 56.39701867748817676, -9.422509992056140149 ) ) ;
#59985 = CARTESIAN_POINT ( 'NONE',  ( 1.236172813752255406, 14.95077488074853456, 14.70095156538448755 ) ) ;
#59986 = CARTESIAN_POINT ( 'NONE',  ( 13.43411237798106583, 32.66530133659708213, -12.81628187352647252 ) ) ;
#59987 = CARTESIAN_POINT ( 'NONE',  ( 9.422509992056141925, 25.14701867748816966, 5.440088680355547268 ) ) ;
#59988 = CARTESIAN_POINT ( 'NONE',  ( 0.5774900079438607392, 8.480352010821505360, 5.440088680355550821 ) ) ;
#59989 = CARTESIAN_POINT ( 'NONE',  ( 17.96484262340118221, 14.93868534415484106, 7.964842623401181321 ) ) ;
#59990 = CARTESIAN_POINT ( 'NONE',  ( 18.52753015748618282, 58.92559781766745886, -4.923371831947291888 ) ) ;
#59991 = CARTESIAN_POINT ( 'NONE',  ( 6.565887622018943937, 53.08196800326374643, -12.81628187352647608 ) ) ;
#59992 = CARTESIAN_POINT ( 'NONE',  ( -38.70923076923077133, 110.8461538461538396, -9.500000000000000000 ) ) ;
#59993 = ORIENTED_EDGE ( 'NONE', *, *, #65393, .T. ) ;
#59994 = EDGE_CURVE ( 'NONE', #60175, #56402, #77618, .T. ) ;
#59995 = CARTESIAN_POINT ( 'NONE',  ( 0.5774900079438607392, 23.48035201082150536, 5.440088680355550821 ) ) ;
#59996 = CARTESIAN_POINT ( 'NONE',  ( 13.43411237798105340, 15.58196800326374998, 12.81628187352647963 ) ) ;
#59997 = CARTESIAN_POINT ( 'NONE',  ( -14.04391541078760675, 4.104531544909319036E-16, -3.608107528143027043 ) ) ;
#59998 = CARTESIAN_POINT ( 'NONE',  ( 0.1532563361054083140, 11.00893115100078568, 1.131784320476157264E-15 ) ) ;
#59999 = VECTOR ( 'NONE', #61948, 1000.000000000000114 ) ;
#60000 = CARTESIAN_POINT ( 'NONE',  ( 10.00000000000000178, 47.25893115100078745, 9.846743663894594434 ) ) ;
#60001 = CARTESIAN_POINT ( 'NONE',  ( -0.8801773607111008646, 33.27201867748817676, 2.915334737309923430 ) ) ;
#60002 = CARTESIAN_POINT ( 'NONE',  ( 10.00000000000000178, 25.37363466993041783, 12.81628187352647608 ) ) ;
#60004 = CARTESIAN_POINT ( 'NONE',  ( 18.00000000000000000, 91.21636964435548123, 8.000000000000000000 ) ) ;
#60003 = CARTESIAN_POINT ( 'NONE',  ( 17.96484262340118221, 44.93868534415483396, 7.964842623401181321 ) ) ;
#60005 = CYLINDRICAL_SURFACE ( 'NONE', #89615, 0.5000000000000004441 ) ;
#60006 = CARTESIAN_POINT ( 'NONE',  ( 0.6178305044545818747, 58.49863466993042493, -9.382169495545419124 ) ) ;
#60007 = VERTEX_POINT ( 'NONE', #17147 ) ;
#60008 = CARTESIAN_POINT ( 'NONE',  ( 10.00000000000000000, 66.81368534415484817, -10.88017736071110342 ) ) ;
#60009 = CARTESIAN_POINT ( 'NONE',  ( -1.099225684535947600, 29.54030133659708923, 6.408140936763237150 ) ) ;
#60010 = CARTESIAN_POINT ( 'NONE',  ( 10.00000000000000000, 4.758931151000784787, -9.846743663894594434 ) ) ;
#60011 = CARTESIAN_POINT ( 'NONE',  ( -0.8801773607110991993, 37.85535201082151247, -2.915334737309923874 ) ) ;
#60012 = CARTESIAN_POINT ( 'NONE',  ( 19.72487221294571214, 2.802231764288312998, -6.500000000000001776 ) ) ;
#60013 = CARTESIAN_POINT ( 'NONE',  ( 18.00000000000000355, 77.07179676972445748, -6.250000000000000000 ) ) ;
#60014 = CARTESIAN_POINT ( 'NONE',  ( 0.1532563361054100626, 10.80059781766745175, -2.638427012816831230 ) ) ;
#60015 = CARTESIAN_POINT ( 'NONE',  ( 5.076628168052703671, 1.842264484334118047, 8.527530157486179263 ) ) ;
#60016 = CARTESIAN_POINT ( 'NONE',  ( -5.999999999999994671, 43.00000000000000000, -6.250000000000000000 ) ) ;
#60017 = CARTESIAN_POINT ( 'NONE',  ( 24.16423886937410614, 44.30374883491397497, 8.672049930838204340E-16 ) ) ;
#60018 = VECTOR ( 'NONE', #18175, 1000.000000000000114 ) ;
#60019 = CARTESIAN_POINT ( 'NONE',  ( 12.22474924877146307, 0.2301506569030462857, -8.589397507024894907 ) ) ;
#60020 = FILL_AREA_STYLE ('',( #29512 ) ) ;
#60021 = CARTESIAN_POINT ( 'NONE',  ( -6.281594481400936125, -39.81112291747236043, -4.000000000000000000 ) ) ;
#60022 = ORIENTED_EDGE ( 'NONE', *, *, #3166, .T. ) ;
#60023 = CARTESIAN_POINT ( 'NONE',  ( -2.266590686148945544, 66.38708216824730357, -7.082119434687050408 ) ) ;
#60024 = CARTESIAN_POINT ( 'NONE',  ( 10.00000000000000000, 65.55374883491396076, -14.16423886937410082 ) ) ;
#60025 = CARTESIAN_POINT ( 'NONE',  ( 12.63842701281683922, 34.55059781766745886, -9.846743663894590881 ) ) ;
#60026 = CARTESIAN_POINT ( 'NONE',  ( -2.816281873526471635, 33.91530133659708213, -3.434112377981056508 ) ) ;
#60027 =( NAMED_UNIT ( * ) PLANE_ANGLE_UNIT ( ) SI_UNIT ( $, .RADIAN. ) );
#60029 = CARTESIAN_POINT ( 'NONE',  ( 22.26659068614895176, 9.720415501580633943, -7.082119434687042414 ) ) ;
#60028 = DIRECTION ( 'NONE',  ( -0.000000000000000000, -1.000000000000000000, -0.000000000000000000 ) ) ;
#60030 = CARTESIAN_POINT ( 'NONE',  ( -0.8801773607111008646, 18.27201867748817321, 2.915334737309923430 ) ) ;
#60031 = CARTESIAN_POINT ( 'NONE',  ( 2.917880565312950480, 50.97041550158064638, -12.26659068614894821 ) ) ;
#60032 = CARTESIAN_POINT ( 'NONE',  ( 0.1532563361054082862, 31.21726448433412315, 2.638427012816831674 ) ) ;
#60033 = CARTESIAN_POINT ( 'NONE',  ( 0.9408516040111580825, 12.46693863883975872, -6.499999999999988454 ) ) ;
#60035 = B_SPLINE_CURVE_WITH_KNOTS ( 'NONE', 3,
 ( #95735, #33726, #19237, #71270, #27218, #19726 ),
 .UNSPECIFIED., .F., .F.,
 ( 4, 2, 4 ),
 ( 3.409110551494650755E-05, 0.0004400426677367923721, 0.0008459942299586381553 ),
 .UNSPECIFIED. ) ;
#60034 = CARTESIAN_POINT ( 'NONE',  ( 14.92337183194729633, 17.67559781766745175, 8.527530157486181039 ) ) ;
#60036 = CARTESIAN_POINT ( 'NONE',  ( 19.84674366389459621, 3.508931151000785231, 7.409399052514197653E-17 ) ) ;
#60037 = CARTESIAN_POINT ( 'NONE',  ( -9.846743663894594434, 11.00893115100079456, 3.469446951953614189E-15 ) ) ;
#60038 = ORIENTED_EDGE ( 'NONE', *, *, #12999, .F. ) ;
#60039 = EDGE_LOOP ( 'NONE', ( #76049, #41887, #82681, #87674 ) ) ;
#60040 = DIRECTION ( 'NONE',  ( -0.3173046564050833740, 0.000000000000000000, -0.9483236552062022096 ) ) ;
#60041 = ORIENTED_EDGE ( 'NONE', *, *, #49221, .F. ) ;
#60042 = CARTESIAN_POINT ( 'NONE',  ( 1.472469842513823179, 46.42559781766745175, 4.923371831947296329 ) ) ;
#60044 = CARTESIAN_POINT ( 'NONE',  ( 19.42250999205614548, 40.98035201082150536, -5.440088680355545492 ) ) ;
#60043 = CARTESIAN_POINT ( 'NONE',  ( 10.00000000000000000, 31.81368534415483751, -10.88017736071110342 ) ) ;
#60046 = CARTESIAN_POINT ( 'NONE',  ( 3.591859063236761518, 34.95696800326375353, 11.09922568453594849 ) ) ;
#60045 = CARTESIAN_POINT ( 'NONE',  ( 1.472469842513823179, 65.59226448433412315, -4.923371831947296329 ) ) ;
#60047 = CARTESIAN_POINT ( 'NONE',  ( 13.79529636645030344, 3.262082168247301350, 14.16423886937410614 ) ) ;
#60048 = EDGE_CURVE ( 'NONE', #41390, #68599, #3127, .T. ) ;
#60049 = CARTESIAN_POINT ( 'NONE',  ( 10.00000000000000178, 35.37363466993042493, 12.81628187352647608 ) ) ;
#60050 = ORIENTED_EDGE ( 'NONE', *, *, #40681, .T. ) ;
#60051 = CARTESIAN_POINT ( 'NONE',  ( 12.63842701281683922, 44.55059781766745175, -9.846743663894590881 ) ) ;
#60052 = CARTESIAN_POINT ( 'NONE',  ( 7.084665262690076126, 12.02201867748817321, -10.88017736071110164 ) ) ;
#60053 = ORIENTED_EDGE ( 'NONE', *, *, #31485, .F. ) ;
#60054 = CARTESIAN_POINT ( 'NONE',  ( 7.084665262690076126, 19.10535201082150181, 10.88017736071109987 ) ) ;
#60055 = EDGE_LOOP ( 'NONE', ( #87127, #86955, #45307, #62510 ) ) ;
#60056 = CARTESIAN_POINT ( 'NONE',  ( 4.559911319644449179, 43.89701867748816966, 9.422509992056141925 ) ) ;
#60057 = CARTESIAN_POINT ( 'NONE',  ( 4.559911319644449179, 52.23035201082151247, -9.422509992056141925 ) ) ;
#60058 = CARTESIAN_POINT ( 'NONE',  ( -0.8801773607110991993, 62.85535201082150536, -2.915334737309923874 ) ) ;
#60059 = B_SPLINE_CURVE_WITH_KNOTS ( 'NONE', 3,
 ( #48165, #78678, #56179, #18177, #55171, #79159 ),
 .UNSPECIFIED., .F., .F.,
 ( 4, 2, 4 ),
 ( 0.0002800225282680484967, 0.0006862279780657134631, 0.001092433427863378484 ),
 .UNSPECIFIED. ) ;
#60060 = CARTESIAN_POINT ( 'NONE',  ( 2.791683348922237240, 0.3839311510007847872, -7.208316651077763204 ) ) ;
#60061 = CARTESIAN_POINT ( 'NONE',  ( 0.5774900079438590739, 47.64701867748817676, -5.440088680355550821 ) ) ;
#60062 = DIRECTION ( 'NONE',  ( -0.000000000000000000, -1.000000000000000000, -0.000000000000000000 ) ) ;
#60063 = ORIENTED_EDGE ( 'NONE', *, *, #46970, .T. ) ;
#60064 = EDGE_CURVE ( 'NONE', #21427, #93614, #55625, .T. ) ;
#60065 = CARTESIAN_POINT ( 'NONE',  ( 5.076628168052704559, 25.17559781766745175, -8.527530157486179263 ) ) ;
#60066 = EDGE_LOOP ( 'NONE', ( #62996, #37118, #2974, #58695, #33040, #12162 ) ) ;
#60067 = CARTESIAN_POINT ( 'NONE',  ( 19.89220837332776881, 19.74062864464239198, 6.478736007405955455 ) ) ;
#60068 = ADVANCED_FACE ( 'NONE', ( #48599 ), #46631, .T. ) ;
#60069 = CARTESIAN_POINT ( 'NONE',  ( 2.917880565312950480, 0.9704155015806342766, -12.26659068614894821 ) ) ;
#60070 = ORIENTED_EDGE ( 'NONE', *, *, #70682, .T. ) ;
#60071 = CARTESIAN_POINT ( 'NONE',  ( -0.1503990784575327533, 7.222660991849186196, -6.262539305110070842 ) ) ;
#60072 = CARTESIAN_POINT ( 'NONE',  ( 0.2751277870542893633, 25.30223176428832232, 6.499999999999988454 ) ) ;
#60073 = CARTESIAN_POINT ( 'NONE',  ( 15.44008868035555793, 6.397018677488171434, -9.422509992056140149 ) ) ;
#60074 = CYLINDRICAL_SURFACE ( 'NONE', #24328, 2.000000000000001776 ) ;
#60075 = CARTESIAN_POINT ( 'NONE',  ( 11.49658347684022708, 0.04962891477616669655, -9.245857368719784475 ) ) ;
#60076 = CARTESIAN_POINT ( 'NONE',  ( 2.791683348922240793, 46.63393115100077324, 7.208316651077764092 ) ) ;
#60077 = CARTESIAN_POINT ( 'NONE',  ( 6.741983435833523330, 14.95077488074853456, -13.12218577464087232 ) ) ;
#60078 = TOROIDAL_SURFACE ( 'NONE', #29752, 14.49999999999999822, 0.5000000000000000000 ) ;
#60079 = CARTESIAN_POINT ( 'NONE',  ( 10.00000000000000000, 22.87363466993042138, -12.81628187352647608 ) ) ;
#60080 = CARTESIAN_POINT ( 'NONE',  ( 19.84674366389459621, 28.50893115100078745, 7.409399052514197653E-17 ) ) ;
#60081 = CARTESIAN_POINT ( 'NONE',  ( 0.03258911192389071787, 0.1934760744867406734, 6.401728757118932300 ) ) ;
#60082 = CARTESIAN_POINT ( 'NONE',  ( 21.09922568453594849, 6.206968003263753531, 6.408140936763242479 ) ) ;
#60083 = ORIENTED_EDGE ( 'NONE', *, *, #28521, .T. ) ;
#60084 = B_SPLINE_CURVE_WITH_KNOTS ( 'NONE', 3,
 ( #6674, #29651, #22182, #68663, #22677, #37194 ),
 .UNSPECIFIED., .F., .F.,
 ( 4, 2, 4 ),
 ( 7.874519775189146796E-18, 0.0002626113303185857945, 0.0005252226606371637827 ),
 .UNSPECIFIED. ) ;
#60085 = ORIENTED_EDGE ( 'NONE', *, *, #60523, .F. ) ;
#60086 = CARTESIAN_POINT ( 'NONE',  ( 20.88017736071110519, 25.56368534415483751, 2.639326808657452039E-16 ) ) ;
#60087 = CARTESIAN_POINT ( 'NONE',  ( 6.204703633549690345, 17.84541550158063217, 14.16423886937410082 ) ) ;
#60088 = CARTESIAN_POINT ( 'NONE',  ( 0.1532563361054082862, 21.21726448433412315, 2.638427012816831674 ) ) ;
#60089 = CARTESIAN_POINT ( 'NONE',  ( 7.084665262690076126, 52.02201867748816255, -10.88017736071110164 ) ) ;
#60091 = CARTESIAN_POINT ( 'NONE',  ( -3.990799379706100325, -9.967613007074422882, -2.750000000000000444 ) ) ;
#60090 = CARTESIAN_POINT ( 'NONE',  ( 19.38216949554541557, 42.24863466993041783, -9.382169495545420901 ) ) ;
#60092 = CARTESIAN_POINT ( 'NONE',  ( 7.084665262690076126, 14.10535201082150358, 10.88017736071109987 ) ) ;
#60093 = CARTESIAN_POINT ( 'NONE',  ( 7.264509831664694772, 14.76984904925306274, -13.05561747642790138 ) ) ;
#60094 = CARTESIAN_POINT ( 'NONE',  ( -19.64999999999999858, 92.00000000000000000, -8.000000000000000000 ) ) ;
#60095 = EDGE_CURVE ( 'NONE', #64921, #25477, #16646, .T. ) ;
#60096 = CARTESIAN_POINT ( 'NONE',  ( 22.81628187352647785, 11.62363466993042138, 6.195893100308588602E-16 ) ) ;
#60097 = CARTESIAN_POINT ( 'NONE',  ( 10.00000000000000178, 5.373634669930420493, 12.81628187352647608 ) ) ;
#60098 = CARTESIAN_POINT ( 'NONE',  ( 19.84674366389459621, 23.50893115100078390, 7.409399052514197653E-17 ) ) ;
#60099 = CARTESIAN_POINT ( 'NONE',  ( 7.964842623401177768, -13.81131465584516071, -7.964842623401181321 ) ) ;
#60100 = CARTESIAN_POINT ( 'NONE',  ( 13.43411237798106583, 32.66530133659708213, -12.81628187352647252 ) ) ;
#60101 = FILL_AREA_STYLE_COLOUR ( '', #32442 ) ;
#60103 = CARTESIAN_POINT ( 'NONE',  ( -11.22915323889586858, 0.000000000000000000, 8.773176023390528044 ) ) ;
#60102 = CARTESIAN_POINT ( 'NONE',  ( 10.00000000000000000, 41.81368534415484106, -10.88017736071110342 ) ) ;
#60104 =( GEOMETRIC_REPRESENTATION_CONTEXT ( 3 ) GLOBAL_UNCERTAINTY_ASSIGNED_CONTEXT ( ( #51146 ) ) GLOBAL_UNIT_ASSIGNED_CONTEXT ( ( #47184, #63660, #8706 ) ) REPRESENTATION_CONTEXT ( 'NONE', 'WORKASPACE' ) );
#60105 = EDGE_CURVE ( 'NONE', #4701, #69569, #70140, .T. ) ;
#60106 = DIRECTION ( 'NONE',  ( 1.000000000000000000, -5.818595309480553908E-17, 0.000000000000000000 ) ) ;
#60107 = CONICAL_SURFACE ( 'NONE', #93658, 1.249999999999987121, 1.029744258676654312 ) ;
#60108 = CARTESIAN_POINT ( 'NONE',  ( 18.39792806157249672, 29.52224192338640307, 6.499999999999997335 ) ) ;
#60109 = CARTESIAN_POINT ( 'NONE',  ( 19.42250999205614548, 45.98035201082150536, -5.440088680355545492 ) ) ;
#60110 = CARTESIAN_POINT ( 'NONE',  ( 2.035157376598822676, 42.43868534415483396, -7.964842623401177768 ) ) ;
#60111 = CARTESIAN_POINT ( 'NONE',  ( 2.791683348922240793, 61.63393115100079456, 7.208316651077764092 ) ) ;
#60112 = CARTESIAN_POINT ( 'NONE',  ( -7.313705784284448619, 0.3639312656126391099, -13.09617149020755633 ) ) ;
#60113 = VECTOR ( 'NONE', #25780, 1000.000000000000000 ) ;
#60114 = UNCERTAINTY_MEASURE_WITH_UNIT (LENGTH_MEASURE( 1.000000000000000082E-05 ), #66745, 'distance_accuracy_value', 'NONE');
#60115 = CARTESIAN_POINT ( 'NONE',  ( 5.076628168052704559, 35.17559781766745175, -8.527530157486179263 ) ) ;
#60116 = CARTESIAN_POINT ( 'NONE',  ( 20.88017736071110164, 10.35535201082150714, 2.915334737309930979 ) ) ;
#60117 = CARTESIAN_POINT ( 'NONE',  ( -2.816281873526473856, 14.33196800326375531, 3.434112377981055619 ) ) ;
#60118 = VERTEX_POINT ( 'NONE', #47118 ) ;
#60119 = CARTESIAN_POINT ( 'NONE',  ( 20.88017736071110164, 20.35535201082150891, 2.915334737309930979 ) ) ;
#60120 = EDGE_CURVE ( 'NONE', #97225, #22589, #8642, .T. ) ;
#60121 = DIRECTION ( 'NONE',  ( 0.000000000000000000, 0.000000000000000000, -1.000000000000000000 ) ) ;
#60122 = CARTESIAN_POINT ( 'NONE',  ( 15.44008868035555260, 29.73035201082150891, 9.422509992056143702 ) ) ;
#60123 = CARTESIAN_POINT ( 'NONE',  ( -0.8801773607110991993, 62.85535201082150536, -2.915334737309923874 ) ) ;
#60124 = CARTESIAN_POINT ( 'NONE',  ( 17.08211943468705840, 40.13708216824731068, -12.26659068614894466 ) ) ;
#60125 = CARTESIAN_POINT ( 'NONE',  ( 5.076628168052704559, 30.17559781766745175, -8.527530157486179263 ) ) ;
#60126 = CARTESIAN_POINT ( 'NONE',  ( 4.559911319644449179, 42.23035201082151247, -9.422509992056141925 ) ) ;
#60127 = LINE ( 'NONE', #67146, #31439 ) ;
#60128 = CARTESIAN_POINT ( 'NONE',  ( 17.08211943468705840, 5.137082168247300906, -12.26659068614894466 ) ) ;
#60130 = ORIENTED_EDGE ( 'NONE', *, *, #41929, .T. ) ;
#60129 = CIRCLE ( 'NONE', #80842, 15.00000000000000000 ) ;
#60131 = CARTESIAN_POINT ( 'NONE',  ( -8.000000000000000000, 40.99999999999999289, 4.250000000000000000 ) ) ;
#60132 = CARTESIAN_POINT ( 'NONE',  ( 17.20831665107776587, 57.88393115100078745, 7.208316651077764980 ) ) ;
#60133 = VECTOR ( 'NONE', #60441, 1000.000000000000000 ) ;
#60134 = ORIENTED_EDGE ( 'NONE', *, *, #52040, .T. ) ;
#60135 = ORIENTED_EDGE ( 'NONE', *, *, #21453, .T. ) ;
#60136 = CARTESIAN_POINT ( 'NONE',  ( -0.3689425029237898834, 16.17874883491396076, -10.36894250292378850 ) ) ;
#60138 = AXIS2_PLACEMENT_3D ( 'NONE', #28109, #74094, #52590 ) ;
#60137 = CARTESIAN_POINT ( 'NONE',  ( -4.164238869374099927, 22.01208216824730357, 3.795296366450308767 ) ) ;
#60139 = CARTESIAN_POINT ( 'NONE',  ( 12.91533473730992121, 64.52201867748817676, 10.88017736071110164 ) ) ;
#60140 = CARTESIAN_POINT ( 'NONE',  ( 20.36894250292379382, 63.67874883491396787, 10.36894250292379205 ) ) ;
#60141 = CARTESIAN_POINT ( 'NONE',  ( 3.591859063236761518, -0.04303199673624671928, 11.09922568453594849 ) ) ;
#60142 = CARTESIAN_POINT ( 'NONE',  ( 12.63842701281683922, 49.55059781766744464, -9.846743663894590881 ) ) ;
#60143 = CARTESIAN_POINT ( 'NONE',  ( -7.750000002553937506, -0.02145965645720818507, 4.000000000000000000 ) ) ;
#60145 = CARTESIAN_POINT ( 'NONE',  ( 10.00000000000000178, 25.37363466993041783, 12.81628187352647608 ) ) ;
#60144 = CARTESIAN_POINT ( 'NONE',  ( 7.084665262690076126, 49.10535201082149825, 10.88017736071109987 ) ) ;
#60146 = CARTESIAN_POINT ( 'NONE',  ( -0.3689425029237881626, 12.42874883491396609, 10.36894250292379027 ) ) ;
#60147 = CARTESIAN_POINT ( 'NONE',  ( 20.88017736071110164, 15.35535201082150358, 2.915334737309930979 ) ) ;
#60148 = CARTESIAN_POINT ( 'NONE',  ( 2.035157376598824452, 18.68868534415484106, 7.964842623401179544 ) ) ;
#60149 = DIRECTION ( 'NONE',  ( 0.000000000000000000, 0.000000000000000000, 1.000000000000000000 ) ) ;
#60150 = CARTESIAN_POINT ( 'NONE',  ( 12.91533473730993009, 56.60535201082151247, -10.88017736071109987 ) ) ;
#60151 = CARTESIAN_POINT ( 'NONE',  ( 6.565887622018943937, 48.08196800326375353, -12.81628187352647608 ) ) ;
#60152 = CARTESIAN_POINT ( 'NONE',  ( -9.846743663894594434, -23.99106884899920900, 3.469446951953614189E-15 ) ) ;
#60153 = EDGE_LOOP ( 'NONE', ( #44059, #93628, #92624, #66042, #40252, #50190 ) ) ;
#60154 = LINE ( 'NONE', #14182, #77891 ) ;
#60155 = ORIENTED_EDGE ( 'NONE', *, *, #68890, .F. ) ;
#60156 = CLOSED_SHELL ( 'NONE', ( #93070, #58821, #7689, #22643, #70810, #57032, #35211, #11973, #33558, #40082, #77779, #28482, #65095, #72720, #61971, #776, #49810, #33244, #72135, #87902, #59598, #3874, #30011, #43472, #28126, #87824, #30522, #73599, #79894, #86801, #29714, #57798, #40765, #37733, #60549, #57706, #80015, #15156, #51465, #36231, #22948, #61046, #65071, #54233, #83398, #33748, #20509, #48888, #48800, #1505, #41853, #6272, #23418, #43920, #78692, #92914, #36921, #95174, #9524, #79198, #50330, #98237, #39916, #34853, #31128, #61105, #97036, #55441, #50969, #89541, #62308, #13232, #88738, #88496, #68199, #25986, #44365, #53639, #23305, #49894, #74599, #77911, #60722, #74386, #57268, #8377, #9079, #92255, #33806, #4647, #19478, #63592, #30687, #84622, #18963, #28439, #11513, #33424, #46610, #35038, #27325, #19818, #53709, #74298, #8170, #96546, #14476, #78733, #88983, #78266, #98941, #81713, #35426, #95629, #41105, #55315, #83503, #80515, #40656, #27309, #28115, #38400, #7903, #72298, #83555, #17354, #52147, #69668, #3610, #89316, #12647, #90872, #45170, #66372, #55533, #85238, #70523, #69587, #1445, #14513, #24988, #66500, #47084, #52424, #72165, #34314, #62711, #94574, #40368, #84096, #62469, #49935, #93928, #62435, #41174, #60195, #77518, #17764, #12556, #818, #59512, #13790, #65927, #33401, #69324, #4684, #38078, #42517, #37606, #27673, #57083, #4481, #38853, #13728, #17991, #53296, #45605, #30369, #71604, #48292, #93184, #42728, #75652, #94194, #5038, #66347, #80489, #89831, #48631, #70016, #7167, #35208, #39060, #77457, #77673, #2776, #90669, #5997, #37372, #22494, #39648, #67807, #46435, #92469, #36713, #15837, #89872, #63320, #3431, #79694, #14192, #98724, #96915, #67519, #14479, #14065, #86133, #84999, #96348, #59675, #83936, #60167, #46296, #96833, #58355, #16638, #26841, #66015, #92799, #26526, #60234, #52391, #35948, #39083, #95230, #14380, #96216, #76215, #66016, #74243, #46100, #46646, #75723, #24342, #30569, #37262, #97716, #95646, #57125, #52187, #38967, #38010, #72715, #7221, #23577, #30076, #68884, #78361, #59069, #54859, #96435, #68084, #69470, #22896, #10558, #15970, #64226, #34765, #43141, #40771, #41331, #56335, #56625, #56121, #69204, #52302, #98614 ) ) ;
#60157 = DIRECTION ( 'NONE',  ( 1.000000000000000000, 0.000000000000000000, 0.000000000000000000 ) ) ;
#60158 = CARTESIAN_POINT ( 'NONE',  ( 14.92337183194729633, 32.67559781766745175, 8.527530157486181039 ) ) ;
#60159 = ORIENTED_EDGE ( 'NONE', *, *, #80382, .T. ) ;
#60160 = FACE_OUTER_BOUND ( 'NONE', #23306, .T. ) ;
#60162 = CARTESIAN_POINT ( 'NONE',  ( 7.084665262690076126, 4.105352010821503583, 10.88017736071109987 ) ) ;
#60161 = CARTESIAN_POINT ( 'NONE',  ( 6.204703633549690345, 50.76208216824730357, -14.16423886937410259 ) ) ;
#60164 = CARTESIAN_POINT ( 'NONE',  ( 1.472469842513823179, 46.42559781766745175, 4.923371831947296329 ) ) ;
#60163 = CARTESIAN_POINT ( 'NONE',  ( 0.1532563361054100626, 20.80059781766744464, -2.638427012816831230 ) ) ;
#60165 = CARTESIAN_POINT ( 'NONE',  ( 20.24186590665278018, 60.59014588040358262, -6.114288769123040090 ) ) ;
#60166 = CARTESIAN_POINT ( 'NONE',  ( -42.60666666666667624, 92.50000000000000000, -9.500000000000000000 ) ) ;
#60167 = ADVANCED_FACE ( 'NONE', ( #56120 ), #65063, .F. ) ;
#60168 = CARTESIAN_POINT ( 'NONE',  ( 10.00000000000000178, 64.31368534415483396, 10.88017736071110342 ) ) ;
#60169 = ADVANCED_FACE ( 'NONE', ( #1660 ), #6192, .T. ) ;
#60170 = CARTESIAN_POINT ( 'NONE',  ( -6.408140936763246032, 18.29030133659709279, -11.09922568453594316 ) ) ;
#60171 = MECHANICAL_DESIGN_GEOMETRIC_PRESENTATION_REPRESENTATION (  '', ( #39420 ), #64938 ) ;
#60172 = ORIENTED_EDGE ( 'NONE', *, *, #5537, .F. ) ;
#60173 = CARTESIAN_POINT ( 'NONE',  ( -2.266590686148945544, 37.22041550158063217, 7.082119434687048631 ) ) ;
#60174 = CARTESIAN_POINT ( 'NONE',  ( 13.43411237798105340, 20.58196800326374643, 12.81628187352647963 ) ) ;
#60175 = VERTEX_POINT ( 'NONE', #19584 ) ;
#60176 = CARTESIAN_POINT ( 'NONE',  ( 10.00000000000000000, 52.87363466993041783, -12.81628187352647608 ) ) ;
#60177 = CARTESIAN_POINT ( 'NONE',  ( 2.035157376598822676, 22.43868534415483396, -7.964842623401177768 ) ) ;
#60178 = CARTESIAN_POINT ( 'NONE',  ( 14.92337183194729633, 37.67559781766745175, 8.527530157486181039 ) ) ;
#60179 = CARTESIAN_POINT ( 'NONE',  ( -0.8801773607110991993, 27.85535201082150181, -2.915334737309923874 ) ) ;
#60180 = CARTESIAN_POINT ( 'NONE',  ( 3.591859063236763294, 63.29030133659708923, -11.09922568453595026 ) ) ;
#60181 = EDGE_CURVE ( 'NONE', #85753, #22949, #50082, .T. ) ;
#60182 = CARTESIAN_POINT ( 'NONE',  ( 14.04867373755350890, -0.03417435944610275333, 7.649324326489743697 ) ) ;
#60183 = CARTESIAN_POINT ( 'NONE',  ( 18.52753015748618282, 53.92559781766745175, -4.923371831947291888 ) ) ;
#60184 = CARTESIAN_POINT ( 'NONE',  ( 18.52753015748618282, 48.92559781766745886, -4.923371831947291888 ) ) ;
#60186 = PRESENTATION_LAYER_ASSIGNMENT (  '', '', ( #33060 ) ) ;
#60185 = CARTESIAN_POINT ( 'NONE',  ( -3.881785064875369784, 15.00000000000000711, 14.10213074188650140 ) ) ;
#60187 = EDGE_CURVE ( 'NONE', #33570, #73111, #22253, .T. ) ;
#60188 = CARTESIAN_POINT ( 'NONE',  ( 0.000000000000000000, 15.00000000000000000, 0.000000000000000000 ) ) ;
#60189 = DIRECTION ( 'NONE',  ( -0.3826834323650877279, 0.000000000000000000, 0.9238795325112876267 ) ) ;
#60190 = CYLINDRICAL_SURFACE ( 'NONE', #51620, 0.2500000000000002220 ) ;
#60191 = AXIS2_PLACEMENT_3D ( 'NONE', #66212, #28219, #28714 ) ;
#60192 = CARTESIAN_POINT ( 'NONE',  ( 1.274849032794278747, 57.55509018479938277, -6.499999999999960032 ) ) ;
#60193 = CARTESIAN_POINT ( 'NONE',  ( 0.1532563361054083140, 31.00893115100078390, 1.131784320476157264E-15 ) ) ;
#60194 = CARTESIAN_POINT ( 'NONE',  ( -2.816281873526473856, 34.12363466993042493, 9.499525473075851096E-16 ) ) ;
#60195 = ADVANCED_FACE ( 'NONE', ( #42108 ), #17476, .T. ) ;
#60196 = CARTESIAN_POINT ( 'NONE',  ( -4.862001128006591344, 4.779775600002961917E-16, -13.66056166602466604 ) ) ;
#60197 = VERTEX_POINT ( 'NONE', #80085 ) ;
#60198 = CARTESIAN_POINT ( 'NONE',  ( 0.1532563361054100626, 60.80059781766744464, -2.638427012816831230 ) ) ;
#60199 = CARTESIAN_POINT ( 'NONE',  ( -7.750000000000000000, 80.32179676972448590, -4.000000000000000000 ) ) ;
#60200 = CARTESIAN_POINT ( 'NONE',  ( 7.361572987183169658, 34.96726448433411605, -9.846743663894592657 ) ) ;
#60201 = CARTESIAN_POINT ( 'NONE',  ( 22.26659068614895176, 34.72041550158063927, -7.082119434687042414 ) ) ;
#60202 = CARTESIAN_POINT ( 'NONE',  ( 5.076628168052704559, 40.17559781766745175, -8.527530157486179263 ) ) ;
#60203 = CARTESIAN_POINT ( 'NONE',  ( 21.09922568453594849, 51.20696800326375353, 6.408140936763242479 ) ) ;
#60205 = CARTESIAN_POINT ( 'NONE',  ( 9.065164099344453774, 0.5000000000000004441, 11.95084933600773169 ) ) ;
#60204 = CARTESIAN_POINT ( 'NONE',  ( 66.76470751278411342, 40.99999999999997868, -9.500000000000000000 ) ) ;
#60206 = CARTESIAN_POINT ( 'NONE',  ( 19.84674366389459266, 3.717264484334118713, -2.638427012816827677 ) ) ;
#60207 = CARTESIAN_POINT ( 'NONE',  ( 13.79529636645031943, 5.345415501580634832, -14.16423886937409904 ) ) ;
#60208 = CARTESIAN_POINT ( 'NONE',  ( 12.63842701281683034, 42.46726448433412315, 9.846743663894596210 ) ) ;
#60209 = CARTESIAN_POINT ( 'NONE',  ( 17.96484262340118221, 39.93868534415484106, 7.964842623401181321 ) ) ;
#60210 = VECTOR ( 'NONE', #33022, 1000.000000000000000 ) ;
#60211 = CARTESIAN_POINT ( 'NONE',  ( 18.52753015748617571, 43.09226448433412315, 4.923371831947298993 ) ) ;
#60212 = COLOUR_RGB ( '', 0.31764706, 0.68627451, 0.89019608) ;
#60213 = ITEM_DEFINED_TRANSFORMATION ( 'NONE', 'NONE', #87031,  #27931 ) ;
#60214 = FACE_OUTER_BOUND ( 'NONE', #12177, .T. ) ;
#60215 = CARTESIAN_POINT ( 'NONE',  ( 12.91533473730993009, 51.60535201082149825, -10.88017736071109987 ) ) ;
#60216 = VERTEX_POINT ( 'NONE', #27570 ) ;
#60217 = CARTESIAN_POINT ( 'NONE',  ( 1.274849032794324932, 22.55509018479936145, -6.500000000000021316 ) ) ;
#60218 = CARTESIAN_POINT ( 'NONE',  ( 12.91533473730993009, 16.60535201082150891, -10.88017736071109987 ) ) ;
#60220 = CARTESIAN_POINT ( 'NONE',  ( 15.44008868035555793, 46.39701867748817676, -9.422509992056140149 ) ) ;
#60219 = CARTESIAN_POINT ( 'NONE',  ( 22.81628187352647785, 1.415301336597087012, 3.434112377981063169 ) ) ;
#60221 =( LENGTH_UNIT ( ) NAMED_UNIT ( * ) SI_UNIT ( .MILLI., .METRE. ) );
#60222 = DIRECTION ( 'NONE',  ( 0.000000000000000000, 0.000000000000000000, 1.000000000000000000 ) ) ;
#60223 = FACE_OUTER_BOUND ( 'NONE', #59471, .T. ) ;
#60225 = DIRECTION ( 'NONE',  ( 0.000000000000000000, 0.000000000000000000, -1.000000000000000000 ) ) ;
#60224 = CARTESIAN_POINT ( 'NONE',  ( 12.91533473730993009, 41.60535201082149825, -10.88017736071109987 ) ) ;
#60226 = CARTESIAN_POINT ( 'NONE',  ( 5.076628168052704559, 10.17559781766745175, -8.527530157486179263 ) ) ;
#60227 = CARTESIAN_POINT ( 'NONE',  ( 19.84674366389459621, 23.50893115100078390, 7.409399052514197653E-17 ) ) ;
#60228 = CARTESIAN_POINT ( 'NONE',  ( -14.16423886937409726, 22.01208216824731778, 3.795296366450320757 ) ) ;
#60229 = CARTESIAN_POINT ( 'NONE',  ( 5.076628168052704559, 60.17559781766745175, -8.527530157486179263 ) ) ;
#60231 = CARTESIAN_POINT ( 'NONE',  ( -0.1042174387088690007, 18.10736173766201418, 6.337391062633411565 ) ) ;
#60230 = CARTESIAN_POINT ( 'NONE',  ( 7.084665262690076126, 4.105352010821503583, 10.88017736071109987 ) ) ;
#60232 = CARTESIAN_POINT ( 'NONE',  ( 64.56412365047461321, 28.99999999999999645, 10.00000000000000000 ) ) ;
#60233 = CARTESIAN_POINT ( 'NONE',  ( -4.164238869374099039, 16.80374883491396787, 8.674139862899312516E-16 ) ) ;
#60234 = ADVANCED_FACE ( 'NONE', ( #5082 ), #39805, .T. ) ;
#60235 = CARTESIAN_POINT ( 'NONE',  ( 20.36894250292379382, 48.67874883491396076, 10.36894250292379205 ) ) ;
#60236 = FACE_OUTER_BOUND ( 'NONE', #61196, .T. ) ;
#60237 = VERTEX_POINT ( 'NONE', #95590 ) ;
#60238 = CARTESIAN_POINT ( 'NONE',  ( 12.63842701281683922, 19.55059781766745175, -9.846743663894590881 ) ) ;
#60239 = CARTESIAN_POINT ( 'NONE',  ( 15.44008868035555260, 14.73035201082150536, 9.422509992056143702 ) ) ;
#60240 = CARTESIAN_POINT ( 'NONE',  ( 5.076628168052704559, 55.17559781766745175, -8.527530157486179263 ) ) ;
#60242 = CARTESIAN_POINT ( 'NONE',  ( 0.000000000000000000, 15.00000000000000000, 0.000000000000000000 ) ) ;
#60241 = CARTESIAN_POINT ( 'NONE',  ( 20.36894250292379382, 8.678748834913967869, 10.36894250292379205 ) ) ;
#60243 = FACE_OUTER_BOUND ( 'NONE', #89336, .T. ) ;
#60244 = MECHANICAL_DESIGN_GEOMETRIC_PRESENTATION_REPRESENTATION (  '', ( #4300 ), #90569 ) ;
#60245 = CARTESIAN_POINT ( 'NONE',  ( 2.815433093577024426, 0.5000000000000004441, 14.73340885523751709 ) ) ;
#60246 = CARTESIAN_POINT ( 'NONE',  ( 19.38216949554541202, 35.99863466993041072, 9.382169495545424454 ) ) ;
#60247 = CARTESIAN_POINT ( 'NONE',  ( 18.52753015748617571, 38.09226448433412315, 4.923371831947298993 ) ) ;
#60248 = ORIENTED_EDGE ( 'NONE', *, *, #37166, .T. ) ;
#60249 = CARTESIAN_POINT ( 'NONE',  ( 17.20831665107776587, 7.883931151000784787, 7.208316651077764980 ) ) ;
#60250 = CARTESIAN_POINT ( 'NONE',  ( 10.93739314578613353, -97.13232482343475738, -3.999999999999775291 ) ) ;
#60251 = DIRECTION ( 'NONE',  ( -0.7253743710122820820, 0.000000000000000000, -0.6883545756937599069 ) ) ;
#60252 = CARTESIAN_POINT ( 'NONE',  ( 2.035157376598824452, 8.688685344154839285, 7.964842623401179544 ) ) ;
#60253 = CARTESIAN_POINT ( 'NONE',  ( 20.36894250292379382, 53.67874883491397497, 10.36894250292379205 ) ) ;
#60254 = CARTESIAN_POINT ( 'NONE',  ( 24.16423886937410614, 4.303748834913967869, 8.672049930838204340E-16 ) ) ;
#60255 = DIRECTION ( 'NONE',  ( 0.000000000000000000, 0.000000000000000000, 1.000000000000000000 ) ) ;
#60256 = CARTESIAN_POINT ( 'NONE',  ( 14.92337183194729633, 27.67559781766745530, 8.527530157486181039 ) ) ;
#60257 = CARTESIAN_POINT ( 'NONE',  ( 0.5774900079438590739, 12.64701867748817143, -5.440088680355550821 ) ) ;
#60258 = CARTESIAN_POINT ( 'NONE',  ( 14.92337183194729988, 39.34226448433412315, -8.527530157486177487 ) ) ;
#60259 = SURFACE_STYLE_FILL_AREA ( #22281 ) ;
#60260 = CARTESIAN_POINT ( 'NONE',  ( 7.361572987183169658, 49.96726448433410894, -9.846743663894592657 ) ) ;
#60261 = CARTESIAN_POINT ( 'NONE',  ( 20.88017736071110875, 40.77201867748818387, -2.915334737309920765 ) ) ;
#60262 = ORIENTED_EDGE ( 'NONE', *, *, #59927, .F. ) ;
#60263 = CARTESIAN_POINT ( 'NONE',  ( -1.099225684535947600, 54.54030133659708923, 6.408140936763237150 ) ) ;
#60264 = CARTESIAN_POINT ( 'NONE',  ( 17.35999999999999588, 33.99999999999997158, -9.500000000000000000 ) ) ;
#60265 = CARTESIAN_POINT ( 'NONE',  ( 18.52753015748617571, 3.092264484334118269, 4.923371831947298993 ) ) ;
#60266 = CARTESIAN_POINT ( 'NONE',  ( 19.38216949554541202, 60.99863466993042493, 9.382169495545424454 ) ) ;
#60268 = CARTESIAN_POINT ( 'NONE',  ( 18.52753015748617571, 38.09226448433412315, 4.923371831947298993 ) ) ;
#60267 = CARTESIAN_POINT ( 'NONE',  ( -0.8801773607111008646, 3.272018677488171434, 2.915334737309923430 ) ) ;
#60269 = CARTESIAN_POINT ( 'NONE',  ( 20.00000000000000711, 79.40087001978915282, 4.500000000000000888 ) ) ;
#60270 = CARTESIAN_POINT ( 'NONE',  ( -6.138934250732154041, 15.00000000000000000, 14.77128574976603481 ) ) ;
#60271 = CARTESIAN_POINT ( 'NONE',  ( 24.16423886937410614, 34.30374883491396787, 8.672049930838204340E-16 ) ) ;
#60272 = CARTESIAN_POINT ( 'NONE',  ( 24.16423886937409904, 44.09541550158063927, 3.795296366450317205 ) ) ;
#60273 = CARTESIAN_POINT ( 'NONE',  ( 2.791683348922240793, 56.63393115100078035, 7.208316651077764092 ) ) ;
#60274 = CARTESIAN_POINT ( 'NONE',  ( 6.685141491970515659, -80.57575624204726239, -2.500000000000000000 ) ) ;
#60275 = CARTESIAN_POINT ( 'NONE',  ( 2.035157376598822676, 32.43868534415483396, -7.964842623401177768 ) ) ;
#60276 = CARTESIAN_POINT ( 'NONE',  ( 12.63842701281683034, 2.467264484334118269, 9.846743663894596210 ) ) ;
#60277 = AXIS2_PLACEMENT_3D ( 'NONE', #91563, #44574, #37089 ) ;
#60278 = CARTESIAN_POINT ( 'NONE',  ( -3.500000000000000888, 1.019547802438454109, 4.000000000000000000 ) ) ;
#60279 = EDGE_LOOP ( 'NONE', ( #33815, #33509, #81844, #55972 ) ) ;
#60280 = CARTESIAN_POINT ( 'NONE',  ( 10.00000000000000000, 57.87363466993042493, -12.81628187352647608 ) ) ;
#60281 = VERTEX_POINT ( 'NONE', #46044 ) ;
#60282 = AXIS2_PLACEMENT_3D ( 'NONE', #50379, #96399, #82354 ) ;
#60283 = CARTESIAN_POINT ( 'NONE',  ( 10.00000000000000178, 69.31368534415484817, 10.88017736071110342 ) ) ;
#60284 = ORIENTED_EDGE ( 'NONE', *, *, #75787, .F. ) ;
#60285 = CARTESIAN_POINT ( 'NONE',  ( -0.3689425029237881626, 12.42874883491396609, 10.36894250292379027 ) ) ;
#60286 = CARTESIAN_POINT ( 'NONE',  ( 2.791683348922240793, 1.633931151000784565, 7.208316651077764092 ) ) ;
#60287 = CARTESIAN_POINT ( 'NONE',  ( 12.91533473730992121, 29.52201867748817321, 10.88017736071110164 ) ) ;
#60288 = CIRCLE ( 'NONE', #49081, 0.2500000000000002220 ) ;
#60289 = SURFACE_SIDE_STYLE ('',( #92272 ) ) ;
#60290 = ORIENTED_EDGE ( 'NONE', *, *, #6279, .T. ) ;
#60291 = CIRCLE ( 'NONE', #93832, 15.00000000000000000 ) ;
#60292 = EDGE_CURVE ( 'NONE', #96379, #21109, #1497, .T. ) ;
#60293 = CARTESIAN_POINT ( 'NONE',  ( 4.559911319644449179, 28.89701867748817321, 9.422509992056141925 ) ) ;
#60294 = EDGE_CURVE ( 'NONE', #47390, #3873, #21571, .T. ) ;
#60295 = EDGE_CURVE ( 'NONE', #12471, #83600, #23831, .T. ) ;
#60296 = ORIENTED_EDGE ( 'NONE', *, *, #42653, .F. ) ;
#60297 = CARTESIAN_POINT ( 'NONE',  ( 19.42250999205614548, 30.98035201082150536, -5.440088680355545492 ) ) ;
#60298 = CARTESIAN_POINT ( 'NONE',  ( 24.50000000000000000, 35.99999999999997158, 7.000000000000000888 ) ) ;
#60299 = ORIENTED_EDGE ( 'NONE', *, *, #11611, .T. ) ;
#60300 = ORIENTED_EDGE ( 'NONE', *, *, #88430, .T. ) ;
#60301 = CARTESIAN_POINT ( 'NONE',  ( 16.40814093676324603, 17.45696800326375353, -11.09922568453594671 ) ) ;
#60302 = CARTESIAN_POINT ( 'NONE',  ( -0.8801773607111009756, 68.06368534415484817, 1.068504757029289695E-15 ) ) ;
#60303 = DIRECTION ( 'NONE',  ( 0.000000000000000000, 1.000000000000000000, 0.000000000000000000 ) ) ;
#60305 = LINE ( 'NONE', #61283, #49441 ) ;
#60304 = CARTESIAN_POINT ( 'NONE',  ( 17.96484262340118221, 19.93868534415484106, 7.964842623401181321 ) ) ;
#60306 = CARTESIAN_POINT ( 'NONE',  ( 12.63842701281683922, 9.550597817667449974, -9.846743663894590881 ) ) ;
#60307 = CARTESIAN_POINT ( 'NONE',  ( 15.44008868035555260, 34.73035201082151247, 9.422509992056143702 ) ) ;
#60308 = ORIENTED_EDGE ( 'NONE', *, *, #6234, .T. ) ;
#60309 = CARTESIAN_POINT ( 'NONE',  ( 0.6178305044545818747, 48.49863466993042493, -9.382169495545419124 ) ) ;
#60310 = CARTESIAN_POINT ( 'NONE',  ( 7.084665262690076126, 47.02201867748818387, -10.88017736071110164 ) ) ;
#60311 = DIRECTION ( 'NONE',  ( 0.000000000000000000, 0.000000000000000000, 1.000000000000000000 ) ) ;
#60312 = CARTESIAN_POINT ( 'NONE',  ( -2.816281873526471635, 48.91530133659708213, -3.434112377981056508 ) ) ;
#60313 = CARTESIAN_POINT ( 'NONE',  ( 17.96484262340118221, 44.93868534415483396, 7.964842623401181321 ) ) ;
#60314 = CARTESIAN_POINT ( 'NONE',  ( 0.1532563361054083140, 66.00893115100079456, 1.131784320476157264E-15 ) ) ;
#60315 = EDGE_CURVE ( 'NONE', #43044, #57022, #90536, .T. ) ;
#60316 = CARTESIAN_POINT ( 'NONE',  ( -14.62617646268082972, 15.00000000000000000, -3.327906561567078647 ) ) ;
#60317 = CARTESIAN_POINT ( 'NONE',  ( 5.076628168052704559, 20.17559781766745175, -8.527530157486179263 ) ) ;
#60318 = CARTESIAN_POINT ( 'NONE',  ( 10.00000000000000178, 60.37363466993041783, 12.81628187352647608 ) ) ;
#60319 = CARTESIAN_POINT ( 'NONE',  ( 1.932340009482190091, 36.49127512925446837, -6.500000000000079936 ) ) ;
#60320 = CARTESIAN_POINT ( 'NONE',  ( 5.076628168052703671, 11.84226448433411960, 8.527530157486179263 ) ) ;
#60321 = CARTESIAN_POINT ( 'NONE',  ( 10.00000000000000178, 10.37363466993041961, 12.81628187352647608 ) ) ;
#60323 = CARTESIAN_POINT ( 'NONE',  ( 10.00000000000000000, 59.75893115100078745, -9.846743663894594434 ) ) ;
#60322 = CARTESIAN_POINT ( 'NONE',  ( 14.69227023463712456, 0.04922511925149390677, -1.335400878252530843 ) ) ;
#60324 = CARTESIAN_POINT ( 'NONE',  ( 4.559911319644449179, 37.23035201082150536, -9.422509992056141925 ) ) ;
#60325 = CARTESIAN_POINT ( 'NONE',  ( 19.84674366389459621, 48.50893115100078745, 7.409399052514197653E-17 ) ) ;
#60326 = CARTESIAN_POINT ( 'NONE',  ( 24.50000000000000000, 35.99999999999997158, 10.00000000000000000 ) ) ;
#60327 = CARTESIAN_POINT ( 'NONE',  ( 18.52753015748617571, 23.09226448433411960, 4.923371831947298993 ) ) ;
#60328 = CARTESIAN_POINT ( 'NONE',  ( 17.20831665107776587, 12.88393115100078390, 7.208316651077764980 ) ) ;
#60330 = EDGE_LOOP ( 'NONE', ( #5507, #64913, #58804, #33682, #20090, #72688 ) ) ;
#60329 = CARTESIAN_POINT ( 'NONE',  ( -1.099225684535947600, 4.540301336597087456, 6.408140936763237150 ) ) ;
#60331 = PRESENTATION_LAYER_ASSIGNMENT (  '', '', ( #9234 ) ) ;
#60332 = CARTESIAN_POINT ( 'NONE',  ( 14.92337183194729633, 62.67559781766745886, 8.527530157486181039 ) ) ;
#60333 = CARTESIAN_POINT ( 'NONE',  ( 6.935134328184320296, -80.57830137102044432, -2.500000000001611156 ) ) ;
#60334 = CARTESIAN_POINT ( 'NONE',  ( 7.084665262690076126, 2.022018677488171434, -10.88017736071110164 ) ) ;
#60335 = CARTESIAN_POINT ( 'NONE',  ( 2.791683348922237240, 45.38393115100079456, -7.208316651077763204 ) ) ;
#60336 = CARTESIAN_POINT ( 'NONE',  ( -9.876730923139437124, 14.49999999999999112, 11.28938378619059613 ) ) ;
#60337 = CARTESIAN_POINT ( 'NONE',  ( 4.559911319644449179, 3.897018677488171434, 9.422509992056141925 ) ) ;
#60338 = DIRECTION ( 'NONE',  ( 0.5519369853120676961, 0.000000000000000000, -0.8338858220671618859 ) ) ;
#60339 = CARTESIAN_POINT ( 'NONE',  ( 20.88017736071110164, 30.35535201082151247, 2.915334737309930979 ) ) ;
#60340 = CARTESIAN_POINT ( 'NONE',  ( 6.204703633549690345, 47.84541550158064638, 14.16423886937410082 ) ) ;
#60342 = LINE ( 'NONE', #31310, #39905 ) ;
#60341 = CARTESIAN_POINT ( 'NONE',  ( 24.16423886937410614, 64.30374883491396076, 8.672049930838204340E-16 ) ) ;
#60343 = CARTESIAN_POINT ( 'NONE',  ( 0.1532563361054083140, 6.008931151000784787, 1.131784320476157264E-15 ) ) ;
#60344 = CARTESIAN_POINT ( 'NONE',  ( 10.00000000000000178, 27.25893115100078390, 9.846743663894594434 ) ) ;
#60345 = CARTESIAN_POINT ( 'NONE',  ( 22.81628187352648496, 6.831968003263753531, -3.434112377981050290 ) ) ;
#60346 = SURFACE_SIDE_STYLE ('',( #39338 ) ) ;
#60347 = CIRCLE ( 'NONE', #17273, 15.00000000000000000 ) ;
#60348 = FACE_OUTER_BOUND ( 'NONE', #75346, .T. ) ;
#60349 = CARTESIAN_POINT ( 'NONE',  ( 24.16423886937410614, 4.512082168247300906, -3.795296366450302550 ) ) ;
#60350 = CARTESIAN_POINT ( 'NONE',  ( 19.84674366389459621, 23.50893115100078390, 7.409399052514197653E-17 ) ) ;
#60351 = CARTESIAN_POINT ( 'NONE',  ( 3.969999999999999751, 37.25000000000000000, 4.000000000000000000 ) ) ;
#60352 = CARTESIAN_POINT ( 'NONE',  ( 20.36894250292379382, 38.67874883491396076, 10.36894250292379205 ) ) ;
#60353 = CARTESIAN_POINT ( 'NONE',  ( 2.791683348922237240, 5.383931151000785675, -7.208316651077763204 ) ) ;
#60355 = CARTESIAN_POINT ( 'NONE',  ( 0.000000000000000000, 0.5000000000000004441, 0.000000000000000000 ) ) ;
#60354 = CARTESIAN_POINT ( 'NONE',  ( -6.867320125584340573, -58.36821204062217561, -2.500000000000000000 ) ) ;
#60356 = CARTESIAN_POINT ( 'NONE',  ( 20.88017736071110519, 35.56368534415484106, 2.639326808657452039E-16 ) ) ;
#60357 = CARTESIAN_POINT ( 'NONE',  ( 22.81628187352647785, 51.41530133659708923, 3.434112377981063169 ) ) ;
#60358 = CARTESIAN_POINT ( 'NONE',  ( 22.81628187352648496, 36.83196800326376064, -3.434112377981050290 ) ) ;
#60359 = ORIENTED_EDGE ( 'NONE', *, *, #77894, .F. ) ;
#60360 = B_SPLINE_CURVE_WITH_KNOTS ( 'NONE', 3,
 ( #40702, #92708, #56202, #10697, #56678, #93195 ),
 .UNSPECIFIED., .F., .F.,
 ( 4, 2, 4 ),
 ( 0.0002800912045253039183, 0.0006862973266949682705, 0.001092503448864632623 ),
 .UNSPECIFIED. ) ;
#60361 = CARTESIAN_POINT ( 'NONE',  ( 11.48952521350015488, 15.00000000000000000, 8.845383562533813304 ) ) ;
#60362 = CARTESIAN_POINT ( 'NONE',  ( 17.08211943468705130, 38.47041550158063217, 12.26659068614894998 ) ) ;
#60363 = CARTESIAN_POINT ( 'NONE',  ( 24.16423886937410614, 9.303748834913967869, 8.672049930838204340E-16 ) ) ;
#60364 = CARTESIAN_POINT ( 'NONE',  ( 10.00000000000000000, 6.813685344154838397, -10.88017736071110342 ) ) ;
#60365 = CARTESIAN_POINT ( 'NONE',  ( 15.44008868035555793, 26.39701867748817321, -9.422509992056140149 ) ) ;
#60366 = CARTESIAN_POINT ( 'NONE',  ( 10.17198128013144043, 14.76930270348881180, -10.94389562857665688 ) ) ;
#60367 = LINE ( 'NONE', #66890, #46377 ) ;
#60368 = CARTESIAN_POINT ( 'NONE',  ( 17.96484262340118221, 49.93868534415484106, 7.964842623401181321 ) ) ;
#60369 = CARTESIAN_POINT ( 'NONE',  ( -0.8801773607111008646, 58.27201867748816966, 2.915334737309923430 ) ) ;
#60370 = CARTESIAN_POINT ( 'NONE',  ( 22.81628187352647785, 26.41530133659708923, 3.434112377981063169 ) ) ;
#60371 = CARTESIAN_POINT ( 'NONE',  ( 19.72487221294570858, 70.00000000000000000, -6.000000000000000000 ) ) ;
#60372 = DIRECTION ( 'NONE',  ( -0.000000000000000000, -1.000000000000000000, -0.000000000000000000 ) ) ;
#60373 = CARTESIAN_POINT ( 'NONE',  ( 10.00000000000000178, 27.25893115100078390, 9.846743663894594434 ) ) ;
#60374 = EDGE_CURVE ( 'NONE', #30081, #49327, #370, .T. ) ;
#60375 = UNCERTAINTY_MEASURE_WITH_UNIT (LENGTH_MEASURE( 1.000000000000000082E-05 ), #15029, 'distance_accuracy_value', 'NONE');
#60376 = CARTESIAN_POINT ( 'NONE',  ( 10.00000000000000000, 12.87363466993042138, -12.81628187352647608 ) ) ;
#60377 = LINE ( 'NONE', #82891, #1140 ) ;
#60378 = CARTESIAN_POINT ( 'NONE',  ( 7.084665262690076126, 9.105352010821503583, 10.88017736071109987 ) ) ;
#60379 = CARTESIAN_POINT ( 'NONE',  ( 17.20831665107776587, 37.88393115100078745, 7.208316651077764980 ) ) ;
#60380 = CARTESIAN_POINT ( 'NONE',  ( 21.09922568453594849, 56.20696800326375353, 6.408140936763242479 ) ) ;
#60381 = CARTESIAN_POINT ( 'NONE',  ( 12.63842701281683922, 19.55059781766745175, -9.846743663894590881 ) ) ;
#60382 = CARTESIAN_POINT ( 'NONE',  ( 17.08211943468705130, 3.470415501580634388, 12.26659068614894998 ) ) ;
#60383 = CARTESIAN_POINT ( 'NONE',  ( 0.000000000000000000, 0.000000000000000000, 0.000000000000000000 ) ) ;
#60384 = CARTESIAN_POINT ( 'NONE',  ( 19.42250999205614548, 35.98035201082151247, -5.440088680355545492 ) ) ;
#60386 = CARTESIAN_POINT ( 'NONE',  ( -0.3689425029237898834, 36.17874883491396787, -10.36894250292378850 ) ) ;
#60385 = CARTESIAN_POINT ( 'NONE',  ( 14.99999999999998046, 79.82179676972448590, -6.500000000000000888 ) ) ;
#60387 = CARTESIAN_POINT ( 'NONE',  ( 12.63842701281683034, 37.46726448433411605, 9.846743663894596210 ) ) ;
#60388 = CARTESIAN_POINT ( 'NONE',  ( 19.42250999205614193, 30.14701867748817321, 5.440088680355555262 ) ) ;
#60389 = VECTOR ( 'NONE', #73274, 1000.000000000000000 ) ;
#60390 = CARTESIAN_POINT ( 'NONE',  ( 7.084665262690076126, 22.02201867748817321, -10.88017736071110164 ) ) ;
#60391 = ORIENTED_EDGE ( 'NONE', *, *, #27712, .F. ) ;
#60392 = EDGE_CURVE ( 'NONE', #98676, #38633, #22070, .T. ) ;
#60393 = CARTESIAN_POINT ( 'NONE',  ( -0.8801773607111009756, 28.06368534415484106, 1.068504757029289695E-15 ) ) ;
#60394 = CARTESIAN_POINT ( 'NONE',  ( 3.591859063236761518, 39.95696800326375353, 11.09922568453594849 ) ) ;
#60395 = CARTESIAN_POINT ( 'NONE',  ( 10.00000000000000000, 46.81368534415484106, -10.88017736071110342 ) ) ;
#60397 = CARTESIAN_POINT ( 'NONE',  ( 19.42250999205614193, 55.14701867748817676, 5.440088680355555262 ) ) ;
#60396 = CYLINDRICAL_SURFACE ( 'NONE', #77596, 6.999999999999995559 ) ;
#60398 = VERTEX_POINT ( 'NONE', #60540 ) ;
#60399 = CARTESIAN_POINT ( 'NONE',  ( 14.92337183194729988, 54.34226448433412315, -8.527530157486177487 ) ) ;
#60401 = EDGE_CURVE ( 'NONE', #15178, #79717, #44551, .T. ) ;
#60400 = CARTESIAN_POINT ( 'NONE',  ( 2.035157376598824452, 43.68868534415484106, 7.964842623401179544 ) ) ;
#60402 = CARTESIAN_POINT ( 'NONE',  ( 5.680373670949098397, -28.65980262290164049, 3.999999999990341504 ) ) ;
#60403 = SURFACE_SIDE_STYLE ('',( #28909 ) ) ;
#60404 = FACE_OUTER_BOUND ( 'NONE', #5696, .T. ) ;
#60405 = CARTESIAN_POINT ( 'NONE',  ( -0.3689425029237898834, 46.17874883491397497, -10.36894250292378850 ) ) ;
#60406 = CARTESIAN_POINT ( 'NONE',  ( 12.91533473730992121, 49.52201867748817676, 10.88017736071110164 ) ) ;
#60407 = CARTESIAN_POINT ( 'NONE',  ( 0.2751277870542911397, 55.30223176428831522, 6.499999999999992006 ) ) ;
#60408 = ADVANCED_FACE ( 'NONE', ( #83050 ), #82553, .T. ) ;
#60409 =( NAMED_UNIT ( * ) PLANE_ANGLE_UNIT ( ) SI_UNIT ( $, .RADIAN. ) );
#60410 = CARTESIAN_POINT ( 'NONE',  ( 2.791683348922237240, 65.38393115100078035, -7.208316651077763204 ) ) ;
#60411 = CARTESIAN_POINT ( 'NONE',  ( 2.035157376598824452, 3.688685344154837953, 7.964842623401179544 ) ) ;
#60412 = CARTESIAN_POINT ( 'NONE',  ( 2.791683348922237240, 35.38393115100079456, -7.208316651077763204 ) ) ;
#60413 = ORIENTED_EDGE ( 'NONE', *, *, #7373, .T. ) ;
#60414 = CARTESIAN_POINT ( 'NONE',  ( 7.361572987183170547, 37.05059781766744464, 9.846743663894590881 ) ) ;
#60415 = CARTESIAN_POINT ( 'NONE',  ( -3.434112377981047626, -19.83469866340291077, 12.81628187352647963 ) ) ;
#60416 = CARTESIAN_POINT ( 'NONE',  ( -0.8801773607110991993, 27.85535201082150181, -2.915334737309923874 ) ) ;
#60417 = CARTESIAN_POINT ( 'NONE',  ( 1.472469842513823179, 36.42559781766745175, 4.923371831947296329 ) ) ;
#60419 = CARTESIAN_POINT ( 'NONE',  ( 2.035157376598822676, 57.43868534415484106, -7.964842623401177768 ) ) ;
#60418 = LINE ( 'NONE', #92393, #16406 ) ;
#60420 = CARTESIAN_POINT ( 'NONE',  ( 12.91533473730993009, 31.60535201082150891, -10.88017736071109987 ) ) ;
#60421 = CARTESIAN_POINT ( 'NONE',  ( 20.36894250292379738, 39.92874883491396787, -10.36894250292379027 ) ) ;
#60422 = AXIS2_PLACEMENT_3D ( 'NONE', #470, #54407, #31407 ) ;
#60423 = AXIS2_PLACEMENT_3D ( 'NONE', #56484, #27448, #47984 ) ;
#60424 = DIRECTION ( 'NONE',  ( 0.000000000000000000, 0.000000000000000000, -1.000000000000000000 ) ) ;
#60425 = ORIENTED_EDGE ( 'NONE', *, *, #6143, .T. ) ;
#60426 = CARTESIAN_POINT ( 'NONE',  ( 13.43411237798106583, 17.66530133659708923, -12.81628187352647252 ) ) ;
#60427 = CARTESIAN_POINT ( 'NONE',  ( 2.035157376598822676, 12.43868534415483751, -7.964842623401177768 ) ) ;
#60428 = CARTESIAN_POINT ( 'NONE',  ( -0.8801773607111008646, 43.27201867748817676, 2.915334737309923430 ) ) ;
#60429 = DIRECTION ( 'NONE',  ( 0.000000000000000000, 0.000000000000000000, -1.000000000000000000 ) ) ;
#60431 = ORIENTED_EDGE ( 'NONE', *, *, #45890, .T. ) ;
#60430 = ADVANCED_FACE ( 'NONE', ( #15559 ), #76036, .F. ) ;
#60432 = CARTESIAN_POINT ( 'NONE',  ( 15.44008868035555793, 56.39701867748817676, -9.422509992056140149 ) ) ;
#60433 = CARTESIAN_POINT ( 'NONE',  ( 5.076628168052703671, 36.84226448433412315, 8.527530157486179263 ) ) ;
#60434 = CARTESIAN_POINT ( 'NONE',  ( 0.1532563361054100626, 20.80059781766744464, -2.638427012816831230 ) ) ;
#60435 = CARTESIAN_POINT ( 'NONE',  ( 14.92337183194729633, 7.675597817667451750, 8.527530157486181039 ) ) ;
#60436 = DIRECTION ( 'NONE',  ( 1.000000000000000000, 0.000000000000000000, 0.000000000000000000 ) ) ;
#60438 = CARTESIAN_POINT ( 'NONE',  ( 21.09922568453594849, 41.20696800326375353, 6.408140936763242479 ) ) ;
#60437 = CARTESIAN_POINT ( 'NONE',  ( 1.816707512666844604, 50.10290668512023871, -6.499999999999958256 ) ) ;
#60440 = CARTESIAN_POINT ( 'NONE',  ( 12.25993886608599581, 0.5000000000000004441, 8.642563219313704082 ) ) ;
#60439 = CARTESIAN_POINT ( 'NONE',  ( 18.52753015748617571, 8.092264484334117824, 4.923371831947298993 ) ) ;
#60441 = DIRECTION ( 'NONE',  ( 1.483861936729427615E-16, -1.000000000000000000, -0.000000000000000000 ) ) ;
#60443 = ORIENTED_EDGE ( 'NONE', *, *, #95101, .F. ) ;
#60442 = CARTESIAN_POINT ( 'NONE',  ( 19.84674366389459266, 33.30059781766744464, 2.638427012816836559 ) ) ;
#60444 = EDGE_CURVE ( 'NONE', #74987, #35164, #51567, .T. ) ;
#60445 =( BOUNDED_CURVE ( )  B_SPLINE_CURVE ( 2, ( #79267, #26749, #56282, #95241, #63755, #55789, #48760, #18777, #86285 ),
 .UNSPECIFIED., .F., .T. ) 
 B_SPLINE_CURVE_WITH_KNOTS ( ( 3, 2, 2, 2, 3 ),
 ( 0.5810855930462679453, 0.5833333333333333703, 0.5892857142857143016, 0.5952380952380952328, 0.5974858355251606579 ),
 .UNSPECIFIED. ) 
 CURVE ( )  GEOMETRIC_REPRESENTATION_ITEM ( )  RATIONAL_B_SPLINE_CURVE ( ( 0.9839835555609424134, 0.9871328979762477029, 1.000000000000000000, 0.9659258262890683122, 1.000000000000000000, 0.9659258262890683122, 1.000000000000000000, 0.9871328979762474809, 0.9839835555609424134 ) ) 
 REPRESENTATION_ITEM ( '' )  );
#60446 = CARTESIAN_POINT ( 'NONE',  ( -11.62719953690055164, 14.49999999999999112, -9.476720473302012948 ) ) ;
#60447 = CARTESIAN_POINT ( 'NONE',  ( 10.00000000000000000, 7.873634669930421381, -12.81628187352647608 ) ) ;
#60448 = CARTESIAN_POINT ( 'NONE',  ( 19.42250999205614548, 45.98035201082150536, -5.440088680355545492 ) ) ;
#60449 = CARTESIAN_POINT ( 'NONE',  ( 2.917880565312950480, 30.97041550158063572, -12.26659068614894821 ) ) ;
#60450 =( BOUNDED_CURVE ( )  B_SPLINE_CURVE ( 2, ( #459, #23438, #38924, #54395, #77885, #16418, #90917, #46414, #92887 ),
 .UNSPECIFIED., .F., .F. ) 
 B_SPLINE_CURVE_WITH_KNOTS ( ( 3, 2, 2, 2, 3 ),
 ( 0.7239427359034107390, 0.7261904761904761640, 0.7321428571428570953, 0.7380952380952381375, 0.7403429783823035626 ),
 .UNSPECIFIED. ) 
 CURVE ( )  GEOMETRIC_REPRESENTATION_ITEM ( )  RATIONAL_B_SPLINE_CURVE ( ( 0.9839835555609424134, 0.9871328979762474809, 1.000000000000000000, 0.9659258262890683122, 1.000000000000000000, 0.9659258262890683122, 1.000000000000000000, 0.9871328979762474809, 0.9839835555609424134 ) ) 
 REPRESENTATION_ITEM ( '' )  );
#60451 = UNCERTAINTY_MEASURE_WITH_UNIT (LENGTH_MEASURE( 1.000000000000000082E-05 ), #45703, 'distance_accuracy_value', 'NONE');
#60452 = CARTESIAN_POINT ( 'NONE',  ( -9.524127588829090385, 88.37770237763953673, 5.051303975186559825 ) ) ;
#60453 = CARTESIAN_POINT ( 'NONE',  ( -0.3689425029237898834, 26.17874883491396432, -10.36894250292378850 ) ) ;
#60454 = CARTESIAN_POINT ( 'NONE',  ( -4.164238869374099039, 51.80374883491396787, 8.674139862899312516E-16 ) ) ;
#60455 = CARTESIAN_POINT ( 'NONE',  ( -4.164238869374099039, 11.80374883491396965, 8.674139862899312516E-16 ) ) ;
#60457 = CARTESIAN_POINT ( 'NONE',  ( -13.57366680649685087, 90.98132597431157365, -7.967802692208045379 ) ) ;
#60456 = CARTESIAN_POINT ( 'NONE',  ( 24.16423886937409904, 29.09541550158063572, 3.795296366450317205 ) ) ;
#60458 = CARTESIAN_POINT ( 'NONE',  ( 15.44008868035555793, 51.39701867748816966, -9.422509992056140149 ) ) ;
#60459 = CARTESIAN_POINT ( 'NONE',  ( -5.624999999999996447, 10.95136696231598883, 9.742785792574938597 ) ) ;
#60460 = CIRCLE ( 'NONE', #73218, 15.00000000000000000 ) ;
#60461 = CARTESIAN_POINT ( 'NONE',  ( 2.791683348922237240, 35.38393115100079456, -7.208316651077763204 ) ) ;
#60463 = CARTESIAN_POINT ( 'NONE',  ( 12.63842701281683922, 39.55059781766744464, -9.846743663894590881 ) ) ;
#60462 = CARTESIAN_POINT ( 'NONE',  ( 15.44008868035555260, 64.73035201082151957, 9.422509992056143702 ) ) ;
#60464 = CARTESIAN_POINT ( 'NONE',  ( 17.96484262340118221, 19.93868534415484106, 7.964842623401181321 ) ) ;
#60465 = CARTESIAN_POINT ( 'NONE',  ( 10.00000000000000178, 60.37363466993041783, 12.81628187352647608 ) ) ;
#60466 = CARTESIAN_POINT ( 'NONE',  ( 2.791683348922237240, 60.38393115100078745, -7.208316651077763204 ) ) ;
#60467 = CARTESIAN_POINT ( 'NONE',  ( 20.00000000000000711, 79.40087001978915282, -5.000000000000000888 ) ) ;
#60468 = CARTESIAN_POINT ( 'NONE',  ( 10.00000000000000178, 27.25893115100078390, 9.846743663894594434 ) ) ;
#60469 = CARTESIAN_POINT ( 'NONE',  ( 16.40814093676323893, 60.79030133659709634, 11.09922568453595026 ) ) ;
#60470 = CARTESIAN_POINT ( 'NONE',  ( -12.26659068614894110, -17.77958449841936073, 7.082119434687058401 ) ) ;
#60471 = CARTESIAN_POINT ( 'NONE',  ( 17.96484262340118221, 41.18868534415484106, -7.964842623401177768 ) ) ;
#60472 = CARTESIAN_POINT ( 'NONE',  ( 18.52753015748617571, 53.09226448433412315, 4.923371831947298993 ) ) ;
#60473 = CARTESIAN_POINT ( 'NONE',  ( -4.164238869374098151, 41.59541550158061796, -3.795296366450310543 ) ) ;
#60474 = ORIENTED_EDGE ( 'NONE', *, *, #57319, .F. ) ;
#60475 = CARTESIAN_POINT ( 'NONE',  ( -4.164238869374098151, 1.595415501580634388, -3.795296366450310543 ) ) ;
#60476 = CARTESIAN_POINT ( 'NONE',  ( 10.00000000000000178, 64.31368534415483396, 10.88017736071110342 ) ) ;
#60477 = CARTESIAN_POINT ( 'NONE',  ( 7.084665262690076126, 62.02201867748816966, -10.88017736071110164 ) ) ;
#60478 = CARTESIAN_POINT ( 'NONE',  ( 22.26659068614894466, 63.88708216824730357, 7.082119434687054849 ) ) ;
#60479 = CARTESIAN_POINT ( 'NONE',  ( 10.00000000000000000, 7.873634669930421381, -12.81628187352647608 ) ) ;
#60480 = FACE_OUTER_BOUND ( 'NONE', #72597, .T. ) ;
#60481 = CARTESIAN_POINT ( 'NONE',  ( 4.559911319644449179, 52.23035201082151247, -9.422509992056141925 ) ) ;
#60482 = CARTESIAN_POINT ( 'NONE',  ( -9.159723438033276821, -0.03417435944610275333, 10.91613331444536250 ) ) ;
#60483 = LINE ( 'NONE', #88139, #35616 ) ;
#60484 = CARTESIAN_POINT ( 'NONE',  ( 16.40814093676323893, 30.79030133659708923, 11.09922568453595026 ) ) ;
#60485 = CARTESIAN_POINT ( 'NONE',  ( 6.204703633549690345, 50.76208216824730357, -14.16423886937410259 ) ) ;
#60486 = CARTESIAN_POINT ( 'NONE',  ( 5.440088680355549045, 26.39701867748816966, -9.422509992056141925 ) ) ;
#60487 = CARTESIAN_POINT ( 'NONE',  ( 19.42250999205614193, 10.14701867748816966, 5.440088680355555262 ) ) ;
#60488 = CARTESIAN_POINT ( 'NONE',  ( 0.5774900079438590739, 27.64701867748817676, -5.440088680355550821 ) ) ;
#60489 = CARTESIAN_POINT ( 'NONE',  ( 12.63842701281683034, 52.46726448433413026, 9.846743663894596210 ) ) ;
#60490 = CARTESIAN_POINT ( 'NONE',  ( 6.565887622018943937, 50.16530133659708213, 12.81628187352647430 ) ) ;
#60491 = CARTESIAN_POINT ( 'NONE',  ( 1.274849032794231007, 43.57228050351031357, 6.499999999999895195 ) ) ;
#60492 = EDGE_LOOP ( 'NONE', ( #58657, #32642, #41657, #24420 ) ) ;
#60493 = EDGE_CURVE ( 'NONE', #44552, #88245, #26532, .T. ) ;
#60494 = AXIS2_PLACEMENT_3D ( 'NONE', #12324, #43310, #8160 ) ;
#60495 = CARTESIAN_POINT ( 'NONE',  ( 17.96484262340118221, 16.18868534415483396, -7.964842623401177768 ) ) ;
#60496 = CARTESIAN_POINT ( 'NONE',  ( 22.81628187352647785, 21.41530133659708923, 3.434112377981063169 ) ) ;
#60497 = DIRECTION ( 'NONE',  ( -0.9099612708765398850, 0.000000000000000000, -0.4146932426562461860 ) ) ;
#60498 = CIRCLE ( 'NONE', #84424, 0.2500000000000002220 ) ;
#60499 = CARTESIAN_POINT ( 'NONE',  ( 18.52753015748618282, 53.92559781766745175, -4.923371831947291888 ) ) ;
#60500 = CARTESIAN_POINT ( 'NONE',  ( 10.00000000000000000, 31.81368534415483751, -10.88017736071110342 ) ) ;
#60501 = CARTESIAN_POINT ( 'NONE',  ( -2.816281873526473856, 19.33196800326375708, 3.434112377981055619 ) ) ;
#60503 = LINE ( 'NONE', #46974, #8130 ) ;
#60502 = CARTESIAN_POINT ( 'NONE',  ( 15.44008868035555260, 44.73035201082151247, 9.422509992056143702 ) ) ;
#60504 = DIRECTION ( 'NONE',  ( -0.000000000000000000, -1.000000000000000000, -0.000000000000000000 ) ) ;
#60505 = CARTESIAN_POINT ( 'NONE',  ( 3.591859063236761518, 49.95696800326375353, 11.09922568453594849 ) ) ;
#60506 = ORIENTED_EDGE ( 'NONE', *, *, #90514, .F. ) ;
#60507 = CARTESIAN_POINT ( 'NONE',  ( -0.8801773607111008646, 48.27201867748816966, 2.915334737309923430 ) ) ;
#60508 = CARTESIAN_POINT ( 'NONE',  ( -2.816281873526471635, 38.91530133659708213, -3.434112377981056508 ) ) ;
#60509 = CARTESIAN_POINT ( 'NONE',  ( 12.91533473730992121, 39.52201867748817676, 10.88017736071110164 ) ) ;
#60510 = DIRECTION ( 'NONE',  ( -0.000000000000000000, -1.000000000000000000, -0.000000000000000000 ) ) ;
#60511 = CARTESIAN_POINT ( 'NONE',  ( 5.076628168052703671, 66.84226448433412315, 8.527530157486179263 ) ) ;
#60512 = CARTESIAN_POINT ( 'NONE',  ( 18.52753015748617571, 13.09226448433411960, 4.923371831947298993 ) ) ;
#60513 = CARTESIAN_POINT ( 'NONE',  ( 10.00000000000000000, 9.758931151000785675, -9.846743663894594434 ) ) ;
#60514 = DIRECTION ( 'NONE',  ( 0.000000000000000000, 0.000000000000000000, -1.000000000000000000 ) ) ;
#60515 = CARTESIAN_POINT ( 'NONE',  ( 10.00000000000000178, 38.05374883491396787, 14.16423886937410082 ) ) ;
#60516 = DIRECTION ( 'NONE',  ( -0.9588197348681947174, 0.000000000000000000, 0.2840153447039170387 ) ) ;
#60517 = MECHANICAL_DESIGN_GEOMETRIC_PRESENTATION_REPRESENTATION (  '', ( #6280 ), #66945 ) ;
#60518 = CARTESIAN_POINT ( 'NONE',  ( 4.559911319644449179, 2.230352010821504471, -9.422509992056141925 ) ) ;
#60519 = CARTESIAN_POINT ( 'NONE',  ( -4.537879770911400712, -17.56524742834905695, -3.999999999996772360 ) ) ;
#60520 = VERTEX_POINT ( 'NONE', #78501 ) ;
#60521 = CARTESIAN_POINT ( 'NONE',  ( 19.42250999205614193, 5.147018677488171434, 5.440088680355555262 ) ) ;
#60523 = EDGE_CURVE ( 'NONE', #28000, #68696, #32499, .T. ) ;
#60522 = CARTESIAN_POINT ( 'NONE',  ( -2.266590686148945544, 61.38708216824730357, -7.082119434687050408 ) ) ;
#60524 = CARTESIAN_POINT ( 'NONE',  ( 19.84674366389459621, 38.50893115100078745, 7.409399052514197653E-17 ) ) ;
#60525 = CARTESIAN_POINT ( 'NONE',  ( 3.591859063236761518, 34.95696800326375353, 11.09922568453594849 ) ) ;
#60526 = DIRECTION ( 'NONE',  ( -0.000000000000000000, -0.000000000000000000, 1.000000000000000000 ) ) ;
#60528 = CARTESIAN_POINT ( 'NONE',  ( 2.917880565312950480, 0.9704155015806342766, -12.26659068614894821 ) ) ;
#60527 = CARTESIAN_POINT ( 'NONE',  ( -8.350463100006260575, 86.22728700194303997, -4.047063141920883567 ) ) ;
#60529 = CARTESIAN_POINT ( 'NONE',  ( 4.559911319644449179, 13.89701867748817143, 9.422509992056141925 ) ) ;
#60530 = CARTESIAN_POINT ( 'NONE',  ( -4.164238869374098151, 51.59541550158063217, -3.795296366450310543 ) ) ;
#60531 = CARTESIAN_POINT ( 'NONE',  ( 2.791683348922237240, 40.38393115100078035, -7.208316651077763204 ) ) ;
#60532 = EDGE_CURVE ( 'NONE', #63992, #60570, #78987, .T. ) ;
#60533 = CARTESIAN_POINT ( 'NONE',  ( 12.22506292814020945, 14.76930270348882068, -8.589871424854703008 ) ) ;
#60534 = CARTESIAN_POINT ( 'NONE',  ( 18.52753015748618282, 23.92559781766745530, -4.923371831947291888 ) ) ;
#60535 = FACE_OUTER_BOUND ( 'NONE', #60153, .T. ) ;
#60536 = CARTESIAN_POINT ( 'NONE',  ( -8.527530157486173934, 21.42559781766745175, 4.923371831947302546 ) ) ;
#60537 = ORIENTED_EDGE ( 'NONE', *, *, #70589, .T. ) ;
#60538 = VECTOR ( 'NONE', #31103, 1000.000000000000000 ) ;
#60539 = ORIENTED_EDGE ( 'NONE', *, *, #22299, .T. ) ;
#60540 = CARTESIAN_POINT ( 'NONE',  ( 17.75000000000000000, 84.07179676972448590, -4.000000000000000000 ) ) ;
#60541 = ORIENTED_EDGE ( 'NONE', *, *, #93367, .T. ) ;
#60542 = CARTESIAN_POINT ( 'NONE',  ( 2.791683348922240793, 61.63393115100079456, 7.208316651077764092 ) ) ;
#60544 = CARTESIAN_POINT ( 'NONE',  ( 19.42250999205614193, 35.14701867748816966, 5.440088680355555262 ) ) ;
#60543 = CARTESIAN_POINT ( 'NONE',  ( 12.91533473730992121, 34.52201867748817676, 10.88017736071110164 ) ) ;
#60546 = CARTESIAN_POINT ( 'NONE',  ( 22.81628187352648496, 36.83196800326376064, -3.434112377981050290 ) ) ;
#60545 = CARTESIAN_POINT ( 'NONE',  ( 2.791683348922237240, 60.38393115100078745, -7.208316651077763204 ) ) ;
#60547 = CARTESIAN_POINT ( 'NONE',  ( 20.36894250292379738, 4.928748834913967869, -10.36894250292379027 ) ) ;
#60548 = CARTESIAN_POINT ( 'NONE',  ( 10.00000000000000000, 66.81368534415484817, -10.88017736071110342 ) ) ;
#60549 = ADVANCED_FACE ( 'NONE', ( #24536 ), #85020, .F. ) ;
#60550 = B_SPLINE_CURVE_WITH_KNOTS ( 'NONE', 3,
 ( #39982, #24500, #39499, #1516, #62964, #69988 ),
 .UNSPECIFIED., .F., .F.,
 ( 4, 2, 4 ),
 ( 3.409110551496101553E-05, 0.0004400426677367863006, 0.0008459942299586115924 ),
 .UNSPECIFIED. ) ;
#60551 = CARTESIAN_POINT ( 'NONE',  ( 6.565887622018943937, 35.16530133659708923, 12.81628187352647430 ) ) ;
#60552 = ORIENTED_EDGE ( 'NONE', *, *, #38085, .T. ) ;
#60553 = CARTESIAN_POINT ( 'NONE',  ( 14.92337183194729633, 47.67559781766745175, 8.527530157486181039 ) ) ;
#60554 = CARTESIAN_POINT ( 'NONE',  ( 0.5774900079438590739, 7.647018677488171434, -5.440088680355550821 ) ) ;
#60555 = ORIENTED_EDGE ( 'NONE', *, *, #56758, .T. ) ;
#60556 = CARTESIAN_POINT ( 'NONE',  ( 19.42250999205614548, 20.98035201082150891, -5.440088680355545492 ) ) ;
#60557 = B_SPLINE_CURVE_WITH_KNOTS ( 'NONE', 3,
 ( #35981, #20499, #66483, #50498, #27984, #6476 ),
 .UNSPECIFIED., .F., .F.,
 ( 4, 2, 4 ),
 ( 3.409110551494651432E-05, 0.0004400426677367942152, 0.0008459942299586418416 ),
 .UNSPECIFIED. ) ;
#60558 = ORIENTED_EDGE ( 'NONE', *, *, #86246, .F. ) ;
#60559 = CARTESIAN_POINT ( 'NONE',  ( 7.084665262690076126, 67.02201867748817676, -10.88017736071110164 ) ) ;
#60560 = CARTESIAN_POINT ( 'NONE',  ( 0.5774900079438590739, 57.64701867748817676, -5.440088680355550821 ) ) ;
#60561 = CARTESIAN_POINT ( 'NONE',  ( 7.084665262690076126, 59.10535201082150536, 10.88017736071109987 ) ) ;
#60562 =( NAMED_UNIT ( * ) PLANE_ANGLE_UNIT ( ) SI_UNIT ( $, .RADIAN. ) );
#60563 = CARTESIAN_POINT ( 'NONE',  ( 17.96484262340118221, 56.18868534415484817, -7.964842623401177768 ) ) ;
#60564 = CARTESIAN_POINT ( 'NONE',  ( -46.94000000000000483, 100.5295635078712593, 8.861295791683421186 ) ) ;
#60565 = VECTOR ( 'NONE', #76529, 1000.000000000000114 ) ;
#60566 = CARTESIAN_POINT ( 'NONE',  ( -46.94000000000001194, 103.2691844435154422, 6.361973263950303270 ) ) ;
#60568 = ORIENTED_EDGE ( 'NONE', *, *, #40605, .T. ) ;
#60567 = CARTESIAN_POINT ( 'NONE',  ( 8.705946125382041600, -3.115782928399954521, 4.000000000000000000 ) ) ;
#60569 = CARTESIAN_POINT ( 'NONE',  ( 17.20831665107776587, 47.88393115100078745, 7.208316651077764980 ) ) ;
#60570 = VERTEX_POINT ( 'NONE', #32988 ) ;
#60571 = FACE_OUTER_BOUND ( 'NONE', #64488, .T. ) ;
#60572 = CARTESIAN_POINT ( 'NONE',  ( 14.99847009497944583, 0.5000000000000004441, -0.2142307401080305596 ) ) ;
#60573 = CIRCLE ( 'NONE', #87913, 15.00000000000000000 ) ;
#60574 = CARTESIAN_POINT ( 'NONE',  ( 24.16423886937409904, 9.095415501580633943, 3.795296366450317205 ) ) ;
#60575 = DIRECTION ( 'NONE',  ( -0.000000000000000000, -1.000000000000000000, -0.000000000000000000 ) ) ;
#60576 = DIRECTION ( 'NONE',  ( 0.000000000000000000, 0.000000000000000000, 1.000000000000000000 ) ) ;
#60577 = CARTESIAN_POINT ( 'NONE',  ( 12.91533473730992121, 9.522018677488171434, 10.88017736071110164 ) ) ;
#60579 = ORIENTED_EDGE ( 'NONE', *, *, #43446, .F. ) ;
#60578 = CARTESIAN_POINT ( 'NONE',  ( -1.099225684535947600, 43.70696800326375353, -6.408140936763238038 ) ) ;
#60580 = CARTESIAN_POINT ( 'NONE',  ( 11.36220558718863138, 4.417444789370043464E-16, -9.008345252845243678 ) ) ;
#60581 = CARTESIAN_POINT ( 'NONE',  ( 0.1532563361054082862, 41.21726448433411605, 2.638427012816831674 ) ) ;
#60582 = FILL_AREA_STYLE_COLOUR ( '', #6817 ) ;
#60583 = CARTESIAN_POINT ( 'NONE',  ( 19.38216949554541557, 22.24863466993041428, -9.382169495545420901 ) ) ;
#60584 = CARTESIAN_POINT ( 'NONE',  ( 1.472469842513823179, 25.59226448433412315, -4.923371831947296329 ) ) ;
#60585 = CARTESIAN_POINT ( 'NONE',  ( 8.629999999999991900, 70.25000000000000000, 6.500000000000000888 ) ) ;
#60586 = CARTESIAN_POINT ( 'NONE',  ( -1.099225684535947600, 4.540301336597087456, 6.408140936763237150 ) ) ;
#60587 = LINE ( 'NONE', #45089, #50701 ) ;
#60588 = VERTEX_POINT ( 'NONE', #17025 ) ;
#60589 = ORIENTED_EDGE ( 'NONE', *, *, #75438, .T. ) ;
#60590 = CARTESIAN_POINT ( 'NONE',  ( 7.084665262690076126, 29.10535201082150181, 10.88017736071109987 ) ) ;
#60591 = CARTESIAN_POINT ( 'NONE',  ( -0.3689425029237881626, 17.42874883491397142, 10.36894250292379027 ) ) ;
#60592 = CARTESIAN_POINT ( 'NONE',  ( 1.472469842513823179, 25.59226448433412315, -4.923371831947296329 ) ) ;
#60593 = CARTESIAN_POINT ( 'NONE',  ( 12.63842701281683922, 4.550597817667451750, -9.846743663894590881 ) ) ;
#60595 = CARTESIAN_POINT ( 'NONE',  ( -6.757332319902496387, -55.97232334539076959, -2.750000000000000444 ) ) ;
#60594 = CARTESIAN_POINT ( 'NONE',  ( 0.6178305044545838731, 39.74863466993041072, 9.382169495545420901 ) ) ;
#60596 = CARTESIAN_POINT ( 'NONE',  ( 10.00000000000000000, 16.81368534415483751, -10.88017736071110342 ) ) ;
#60597 = DIRECTION ( 'NONE',  ( -0.000000000000000000, -0.000000000000000000, -1.000000000000000000 ) ) ;
#60598 = CARTESIAN_POINT ( 'NONE',  ( -1.099225684535947600, 9.540301336597087456, 6.408140936763237150 ) ) ;
#60599 = CARTESIAN_POINT ( 'NONE',  ( 21.09922568453595559, 2.040301336597086568, -6.408140936763230044 ) ) ;
#60600 = CARTESIAN_POINT ( 'NONE',  ( 2.791683348922240793, 31.63393115100078745, 7.208316651077764092 ) ) ;
#60601 = CARTESIAN_POINT ( 'NONE',  ( 7.964842623401177768, -8.811314655845162491, -7.964842623401181321 ) ) ;
#60602 = CARTESIAN_POINT ( 'NONE',  ( -2.816281873526473856, 39.12363466993041783, 9.499525473075851096E-16 ) ) ;
#60603 = CARTESIAN_POINT ( 'NONE',  ( 13.74344568549456902, 0.2301512731879840901, -5.860030649989653284 ) ) ;
#60605 = CARTESIAN_POINT ( 'NONE',  ( 14.56195259121195207, 15.00000000000000888, 1.374002722866818793 ) ) ;
#60604 = CARTESIAN_POINT ( 'NONE',  ( 20.88017736071110519, 35.56368534415484106, 2.639326808657452039E-16 ) ) ;
#60606 = EDGE_CURVE ( 'NONE', #23275, #97363, #19031, .T. ) ;
#60607 = CARTESIAN_POINT ( 'NONE',  ( 14.16722289976688032, 0.3639312946971514084, -4.928467845925542434 ) ) ;
#60608 = CARTESIAN_POINT ( 'NONE',  ( -0.3093388210927896509, 14.49999999999999112, 14.99680997725072373 ) ) ;
#60609 = CARTESIAN_POINT ( 'NONE',  ( 7.084665262690076126, 39.10535201082150536, 10.88017736071109987 ) ) ;
#60610 = CARTESIAN_POINT ( 'NONE',  ( 15.44008868035555260, 49.73035201082150536, 9.422509992056143702 ) ) ;
#60611 = CARTESIAN_POINT ( 'NONE',  ( 0.1532563361054083140, 61.00893115100078745, 1.131784320476157264E-15 ) ) ;
#60612 = CARTESIAN_POINT ( 'NONE',  ( 10.00000000000000000, 66.81368534415484817, -10.88017736071110342 ) ) ;
#60613 = CARTESIAN_POINT ( 'NONE',  ( 1.472469842513823179, 51.42559781766745886, 4.923371831947296329 ) ) ;
#60615 = CARTESIAN_POINT ( 'NONE',  ( 8.549759589250252034, 0.2301501389895041494, -12.25250350990697612 ) ) ;
#60614 = CARTESIAN_POINT ( 'NONE',  ( 20.88017736071110519, 5.563685344154837509, 2.639326808657452039E-16 ) ) ;
#60616 = CARTESIAN_POINT ( 'NONE',  ( 13.43411237798106583, 7.665301336597086568, -12.81628187352647252 ) ) ;
#60617 = ORIENTED_EDGE ( 'NONE', *, *, #55600, .T. ) ;
#60618 = CARTESIAN_POINT ( 'NONE',  ( 19.42250999205614193, 40.14701867748817676, 5.440088680355555262 ) ) ;
#60619 = CARTESIAN_POINT ( 'NONE',  ( 3.469446951953614189E-15, 6.368033628982654903, 11.25000000000000178 ) ) ;
#60620 = CARTESIAN_POINT ( 'NONE',  ( 4.559911319644449179, 28.89701867748817321, 9.422509992056141925 ) ) ;
#60621 = CARTESIAN_POINT ( 'NONE',  ( 1.472469842513823179, 11.42559781766745175, 4.923371831947296329 ) ) ;
#60622 = CARTESIAN_POINT ( 'NONE',  ( 10.00000000000000178, 33.05374883491396787, 14.16423886937410082 ) ) ;
#60623 = CARTESIAN_POINT ( 'NONE',  ( 18.52753015748617571, 23.09226448433411960, 4.923371831947298993 ) ) ;
#60624 = CARTESIAN_POINT ( 'NONE',  ( 12.91533473730992121, 44.52201867748816966, 10.88017736071110164 ) ) ;
#60625 = DIRECTION ( 'NONE',  ( 0.000000000000000000, 0.000000000000000000, 1.000000000000000000 ) ) ;
#60626 = CARTESIAN_POINT ( 'NONE',  ( 2.917880565312948704, 2.637082168247300906, 12.26659068614894643 ) ) ;
#60627 = LINE ( 'NONE', #5675, #69086 ) ;
#60628 = CARTESIAN_POINT ( 'NONE',  ( 5.076628168052703671, 61.84226448433412315, 8.527530157486179263 ) ) ;
#60629 = VERTEX_POINT ( 'NONE', #71012 ) ;
#60630 = EDGE_LOOP ( 'NONE', ( #44313, #11615, #1697, #13716 ) ) ;
#60631 = CARTESIAN_POINT ( 'NONE',  ( 24.16423886937409904, 19.09541550158063927, 3.795296366450317205 ) ) ;
#60633 = ADVANCED_FACE ( 'NONE', ( #86011 ), #12276, .T. ) ;
#60632 = CARTESIAN_POINT ( 'NONE',  ( -2.266590686148945544, 26.38708216824730357, -7.082119434687050408 ) ) ;
#60634 = CARTESIAN_POINT ( 'NONE',  ( 7.084665262690076126, 64.10535201082150536, 10.88017736071109987 ) ) ;
#60635 = CARTESIAN_POINT ( 'NONE',  ( -4.164238869374099039, 66.80374883491396076, 8.674139862899312516E-16 ) ) ;
#60636 = CARTESIAN_POINT ( 'NONE',  ( 18.52753015748618282, 43.92559781766745175, -4.923371831947291888 ) ) ;
#60637 = CARTESIAN_POINT ( 'NONE',  ( -11.37817008395673035, -77.84129771019460975, 4.000000000000000000 ) ) ;
#60639 = CARTESIAN_POINT ( 'NONE',  ( -2.816281873526473856, 14.12363466993041961, 9.499525473075851096E-16 ) ) ;
#60638 = CARTESIAN_POINT ( 'NONE',  ( 17.96484262340118221, 49.93868534415484106, 7.964842623401181321 ) ) ;
#60640 = CARTESIAN_POINT ( 'NONE',  ( 17.08211943468705130, 18.47041550158063572, 12.26659068614894998 ) ) ;
#60641 = CARTESIAN_POINT ( 'NONE',  ( 15.44008868035555793, 16.39701867748817321, -9.422509992056140149 ) ) ;
#60642 = CARTESIAN_POINT ( 'NONE',  ( 17.96484262340118221, 31.18868534415483751, -7.964842623401177768 ) ) ;
#60643 = CARTESIAN_POINT ( 'NONE',  ( -0.2418659066527499291, 2.234100856612035724, -6.114288769123083611 ) ) ;
#60644 = CARTESIAN_POINT ( 'NONE',  ( 19.42250999205614548, 60.98035201082151247, -5.440088680355545492 ) ) ;
#60645 = AXIS2_PLACEMENT_3D ( 'NONE', #86451, #87419, #70961 ) ;
#60646 = CARTESIAN_POINT ( 'NONE',  ( -1.099225684535947600, 49.54030133659708923, 6.408140936763237150 ) ) ;
#60647 = CARTESIAN_POINT ( 'NONE',  ( -7.208316651077764980, -29.61606884899920900, -7.208316651077759651 ) ) ;
#60648 = ORIENTED_EDGE ( 'NONE', *, *, #13576, .T. ) ;
#60649 = CARTESIAN_POINT ( 'NONE',  ( 19.80832241502127644, 34.75868815902068576, 6.499999999999991118 ) ) ;
#60650 = EDGE_LOOP ( 'NONE', ( #74358, #80667, #28257, #85134 ) ) ;
#60651 = LINE ( 'NONE', #53649, #4623 ) ;
#60652 = VECTOR ( 'NONE', #71263, 1000.000000000000000 ) ;
#60653 = ORIENTED_EDGE ( 'NONE', *, *, #64756, .T. ) ;
#60654 = LINE ( 'NONE', #38654, #7320 ) ;
#60656 = CARTESIAN_POINT ( 'NONE',  ( 6.204703633549690345, 67.84541550158060375, 14.16423886937410082 ) ) ;
#60655 = CARTESIAN_POINT ( 'NONE',  ( 2.917880565312950480, 55.97041550158063217, -12.26659068614894821 ) ) ;
#60658 = CARTESIAN_POINT ( 'NONE',  ( 5.076628168052704559, 65.17559781766745175, -8.527530157486179263 ) ) ;
#60657 = CARTESIAN_POINT ( 'NONE',  ( 12.63842701281683034, 17.46726448433411250, 9.846743663894596210 ) ) ;
#60659 = CARTESIAN_POINT ( 'NONE',  ( 4.559911319644449179, 67.23035201082150536, -9.422509992056141925 ) ) ;
#60660 = CARTESIAN_POINT ( 'NONE',  ( -6.408140936763232709, 24.95696800326376064, 11.09922568453595026 ) ) ;
#60661 = VERTEX_POINT ( 'NONE', #17165 ) ;
#60662 = CARTESIAN_POINT ( 'NONE',  ( 17.08211943468705840, 30.13708216824730357, -12.26659068614894466 ) ) ;
#60663 = VERTEX_POINT ( 'NONE', #93633 ) ;
#60664 = CARTESIAN_POINT ( 'NONE',  ( 20.36894250292379382, 38.67874883491396076, 10.36894250292379205 ) ) ;
#60665 = ORIENTED_EDGE ( 'NONE', *, *, #15044, .F. ) ;
#60666 = CARTESIAN_POINT ( 'NONE',  ( 19.38216949554541557, 62.24863466993041072, -9.382169495545420901 ) ) ;
#60667 = EDGE_CURVE ( 'NONE', #73802, #16898, #26484, .T. ) ;
#60668 = CARTESIAN_POINT ( 'NONE',  ( 4.559911319644449179, 23.89701867748817321, 9.422509992056141925 ) ) ;
#60669 = CARTESIAN_POINT ( 'NONE',  ( 0.1532563361054083140, 56.00893115100078745, 1.131784320476157264E-15 ) ) ;
#60670 = CARTESIAN_POINT ( 'NONE',  ( -0.8801773607111009756, 23.06368534415484106, 1.068504757029289695E-15 ) ) ;
#60671 = CARTESIAN_POINT ( 'NONE',  ( 13.30156849913881878, 0.2306972965111892537, 6.804875469488154138 ) ) ;
#60672 = DIRECTION ( 'NONE',  ( -1.000000000000000000, 0.000000000000000000, 0.000000000000000000 ) ) ;
#60673 = CARTESIAN_POINT ( 'NONE',  ( 7.361572987183169658, 54.96726448433413026, -9.846743663894592657 ) ) ;
#60674 = CARTESIAN_POINT ( 'NONE',  ( 12.63842701281683922, 44.55059781766745175, -9.846743663894590881 ) ) ;
#60675 = EDGE_CURVE ( 'NONE', #67193, #65046, #4004, .T. ) ;
#60677 = VERTEX_POINT ( 'NONE', #42483 ) ;
#60676 = CARTESIAN_POINT ( 'NONE',  ( 20.15039907845753930, 70.00000000000000000, 6.262539305110068177 ) ) ;
#60678 = CARTESIAN_POINT ( 'NONE',  ( -0.1034006766821533585, 0.000000000000000000, -14.49963131600461175 ) ) ;
#60679 = FILL_AREA_STYLE ('',( #9660 ) ) ;
#60680 = SURFACE_STYLE_FILL_AREA ( #76185 ) ;
#60681 = ORIENTED_EDGE ( 'NONE', *, *, #95280, .F. ) ;
#60682 = PRESENTATION_STYLE_ASSIGNMENT (( #36719 ) ) ;
#60683 = CARTESIAN_POINT ( 'NONE',  ( 2.791683348922237240, 25.38393115100078390, -7.208316651077763204 ) ) ;
#60684 = CARTESIAN_POINT ( 'NONE',  ( -46.34323875807881166, 103.6109741468810483, 6.190393423093146552 ) ) ;
#60685 = CARTESIAN_POINT ( 'NONE',  ( -1.099225684535947600, 38.70696800326375353, -6.408140936763238038 ) ) ;
#60686 = CARTESIAN_POINT ( 'NONE',  ( -45.94000000000000483, 103.0000000000000000, 5.000000000000000000 ) ) ;
#60687 = DIRECTION ( 'NONE',  ( -0.06975647374412512203, -0.9975640502598241977, 0.000000000000000000 ) ) ;
#60688 = LINE ( 'NONE', #84202, #92102 ) ;
#60689 = CARTESIAN_POINT ( 'NONE',  ( 2.791683348922240793, 36.63393115100078035, 7.208316651077764092 ) ) ;
#60690 = CARTESIAN_POINT ( 'NONE',  ( 10.00000000000000178, 28.05374883491396787, 14.16423886937410082 ) ) ;
#60691 = CARTESIAN_POINT ( 'NONE',  ( 7.361572987183169658, 39.96726448433411605, -9.846743663894592657 ) ) ;
#60692 = CARTESIAN_POINT ( 'NONE',  ( -9.240973841163672375, 15.00000000000000000, 11.17382667070363667 ) ) ;
#60693 = CARTESIAN_POINT ( 'NONE',  ( 12.63842701281683922, 4.550597817667451750, -9.846743663894590881 ) ) ;
#60694 = CARTESIAN_POINT ( 'NONE',  ( 20.36894250292379738, 4.928748834913967869, -10.36894250292379027 ) ) ;
#60695 = CARTESIAN_POINT ( 'NONE',  ( 14.92337183194729633, 42.67559781766745886, 8.527530157486181039 ) ) ;
#60696 = CARTESIAN_POINT ( 'NONE',  ( -0.8801773607111008646, 48.27201867748816966, 2.915334737309923430 ) ) ;
#60697 = B_SPLINE_CURVE_WITH_KNOTS ( 'NONE', 3,
 ( #60580, #67603, #60075, #90577, #98622, #91072 ),
 .UNSPECIFIED., .F., .F.,
 ( 4, 2, 4 ),
 ( 0.0002800338592536525577, 0.0006862394199285712457, 0.001092444980603490042 ),
 .UNSPECIFIED. ) ;
#60698 = CARTESIAN_POINT ( 'NONE',  ( 2.791683348922240793, 46.63393115100077324, 7.208316651077764092 ) ) ;
#60699 = PRODUCT_CONTEXT ( 'NONE', #4669, 'mechanical' ) ;
#60700 = CARTESIAN_POINT ( 'NONE',  ( 0.000000000000000000, 0.5000000000000004441, 0.000000000000000000 ) ) ;
#60701 = VECTOR ( 'NONE', #27166, 1000.000000000000000 ) ;
#60702 = CARTESIAN_POINT ( 'NONE',  ( 19.42250999205614193, 40.14701867748817676, 5.440088680355555262 ) ) ;
#60703 = ORIENTED_EDGE ( 'NONE', *, *, #52976, .F. ) ;
#60704 = DIRECTION ( 'NONE',  ( 0.8070303256584298035, -0.5905099943842175847, 0.000000000000000000 ) ) ;
#60705 = CARTESIAN_POINT ( 'NONE',  ( 15.44008868035555260, 34.73035201082151247, 9.422509992056143702 ) ) ;
#60707 = CARTESIAN_POINT ( 'NONE',  ( 19.42250999205614548, 45.98035201082150536, -5.440088680355545492 ) ) ;
#60706 = CARTESIAN_POINT ( 'NONE',  ( 1.472469842513823179, 66.42559781766745175, 4.923371831947296329 ) ) ;
#60708 = CARTESIAN_POINT ( 'NONE',  ( -1.926860441876564023, 47.87045670184115664, 3.195792623639529761 ) ) ;
#60709 = CARTESIAN_POINT ( 'NONE',  ( 10.00000000000000178, 69.31368534415484817, 10.88017736071110342 ) ) ;
#60710 = LINE ( 'NONE', #61209, #10262 ) ;
#60712 = CYLINDRICAL_SURFACE ( 'NONE', #77551, 15.00000000000000000 ) ;
#60711 = CARTESIAN_POINT ( 'NONE',  ( 2.035157376598822676, 37.43868534415484106, -7.964842623401177768 ) ) ;
#60713 = CARTESIAN_POINT ( 'NONE',  ( 5.076628168052703671, 16.84226448433411960, 8.527530157486179263 ) ) ;
#60714 = CARTESIAN_POINT ( 'NONE',  ( 17.20831665107776587, 34.13393115100078745, -7.208316651077762316 ) ) ;
#60715 = CARTESIAN_POINT ( 'NONE',  ( 19.72487221294571214, 57.80223176428831522, -6.499999999999988454 ) ) ;
#60716 = CARTESIAN_POINT ( 'NONE',  ( -3.795296366450300773, 22.84541550158063927, 14.16423886937410437 ) ) ;
#60717 = CARTESIAN_POINT ( 'NONE',  ( 16.40814093676323893, 0.7903013365970867898, 11.09922568453595026 ) ) ;
#60718 = AXIS2_PLACEMENT_3D ( 'NONE', #22204, #51708, #36205 ) ;
#60719 = CARTESIAN_POINT ( 'NONE',  ( 12.91533473730993009, 6.605352010821504471, -10.88017736071109987 ) ) ;
#60720 = CARTESIAN_POINT ( 'NONE',  ( -10.19513985507840736, 0.5000000000000004441, 11.00268709613209950 ) ) ;
#60721 = CARTESIAN_POINT ( 'NONE',  ( 2.917880565312950480, 25.97041550158063572, -12.26659068614894821 ) ) ;
#60722 = ADVANCED_FACE ( 'NONE', ( #72966 ), #34962, .F. ) ;
#60723 = CARTESIAN_POINT ( 'NONE',  ( 24.16423886937410614, 49.51208216824730357, -3.795296366450302550 ) ) ;
#60724 = VERTEX_POINT ( 'NONE', #45425 ) ;
#60725 = CARTESIAN_POINT ( 'NONE',  ( 0.1532563361054082862, 26.21726448433411605, 2.638427012816831674 ) ) ;
#60726 = CARTESIAN_POINT ( 'NONE',  ( 19.42250999205614548, 25.98035201082150891, -5.440088680355545492 ) ) ;
#60727 = EDGE_CURVE ( 'NONE', #80952, #5362, #84064, .T. ) ;
#60728 = CARTESIAN_POINT ( 'NONE',  ( 5.076628168052704559, 45.17559781766745175, -8.527530157486179263 ) ) ;
#60729 = CARTESIAN_POINT ( 'NONE',  ( 6.204703633549690345, 10.76208216824729824, -14.16423886937410259 ) ) ;
#60730 = DIRECTION ( 'NONE',  ( 0.5372996083468138950, 0.000000000000000000, 0.8433914458128921599 ) ) ;
#60731 = CARTESIAN_POINT ( 'NONE',  ( 7.361572987183169658, 4.967264484334119601, -9.846743663894592657 ) ) ;
#60732 = CARTESIAN_POINT ( 'NONE',  ( 6.565887622018943937, 38.08196800326376064, -12.81628187352647608 ) ) ;
#60733 = CARTESIAN_POINT ( 'NONE',  ( 12.63842701281683034, 42.46726448433412315, 9.846743663894596210 ) ) ;
#60734 = ORIENTED_EDGE ( 'NONE', *, *, #53750, .T. ) ;
#60735 = CARTESIAN_POINT ( 'NONE',  ( 10.00000000000000000, 4.758931151000784787, -9.846743663894594434 ) ) ;
#60736 = CARTESIAN_POINT ( 'NONE',  ( 11.20666035742026878, -56.81027457018397087, -4.000000000000000000 ) ) ;
#60737 = DIRECTION ( 'NONE',  ( 0.000000000000000000, 0.000000000000000000, 1.000000000000000000 ) ) ;
#60738 = CARTESIAN_POINT ( 'NONE',  ( 24.16423886937409904, 54.09541550158063217, 3.795296366450317205 ) ) ;
#60739 = CARTESIAN_POINT ( 'NONE',  ( 12.91533473730993009, 41.60535201082149825, -10.88017736071109987 ) ) ;
#60740 = CARTESIAN_POINT ( 'NONE',  ( -46.48928645636215151, 103.2957187381728232, 6.397878122523974476 ) ) ;
#60741 = PRESENTATION_STYLE_ASSIGNMENT (( #30237 ) ) ;
#60742 = CARTESIAN_POINT ( 'NONE',  ( 17.20831665107776587, 39.13393115100079456, -7.208316651077762316 ) ) ;
#60743 = CARTESIAN_POINT ( 'NONE',  ( -0.8801773607111009756, 8.063685344154837509, 1.068504757029289695E-15 ) ) ;
#60744 = CARTESIAN_POINT ( 'NONE',  ( 0.1532563361054100626, 35.80059781766745175, -2.638427012816831230 ) ) ;
#60745 = CARTESIAN_POINT ( 'NONE',  ( -0.7670050760944780999, -5.787280142670756450E-16, -2.805511429989595129 ) ) ;
#60746 = CARTESIAN_POINT ( 'NONE',  ( 2.791683348922240793, 51.63393115100078745, 7.208316651077764092 ) ) ;
#60747 = CARTESIAN_POINT ( 'NONE',  ( 0.5774900079438607392, 48.48035201082150536, 5.440088680355550821 ) ) ;
#60748 = ORIENTED_EDGE ( 'NONE', *, *, #16837, .T. ) ;
#60749 = ORIENTED_EDGE ( 'NONE', *, *, #12359, .F. ) ;
#60750 = AXIS2_PLACEMENT_3D ( 'NONE', #80122, #34118, #96627 ) ;
#60751 = CARTESIAN_POINT ( 'NONE',  ( -1.099225684535947600, 63.70696800326376774, -6.408140936763238038 ) ) ;
#60753 = EDGE_CURVE ( 'NONE', #40639, #37825, #1601, .T. ) ;
#60752 = CARTESIAN_POINT ( 'NONE',  ( 11.35178980618974087, 15.00000000000000000, -9.804941009311923139 ) ) ;
#60754 = CARTESIAN_POINT ( 'NONE',  ( 12.63842701281683922, 4.550597817667451750, -9.846743663894590881 ) ) ;
#60755 = CARTESIAN_POINT ( 'NONE',  ( 10.00000000000000000, 52.87363466993041783, -12.81628187352647608 ) ) ;
#60757 = CARTESIAN_POINT ( 'NONE',  ( 14.92337183194729988, 54.34226448433412315, -8.527530157486177487 ) ) ;
#60756 = CARTESIAN_POINT ( 'NONE',  ( 0.5774900079438607392, 3.480352010821504916, 5.440088680355550821 ) ) ;
#60758 = LINE ( 'NONE', #45774, #96521 ) ;
#60759 = CARTESIAN_POINT ( 'NONE',  ( 5.076628168052704559, 0.1755978176674514724, -8.527530157486179263 ) ) ;
#60760 = CARTESIAN_POINT ( 'NONE',  ( 2.917880565312948704, 27.63708216824730357, 12.26659068614894643 ) ) ;
#60761 = CARTESIAN_POINT ( 'NONE',  ( 6.204703633549690345, 40.76208216824731778, -14.16423886937410259 ) ) ;
#60762 = CARTESIAN_POINT ( 'NONE',  ( 2.791683348922237240, 60.38393115100078745, -7.208316651077763204 ) ) ;
#60763 = FACE_OUTER_BOUND ( 'NONE', #65152, .T. ) ;
#60764 = CARTESIAN_POINT ( 'NONE',  ( 2.035157376598822676, 52.43868534415483396, -7.964842623401177768 ) ) ;
#60765 = EDGE_CURVE ( 'NONE', #50106, #65696, #69713, .T. ) ;
#60766 = CARTESIAN_POINT ( 'NONE',  ( 19.84674366389459266, 8.300597817667451750, 2.638427012816836559 ) ) ;
#60767 =( LENGTH_UNIT ( ) NAMED_UNIT ( * ) SI_UNIT ( .MILLI., .METRE. ) );
#60768 = ORIENTED_EDGE ( 'NONE', *, *, #37027, .T. ) ;
#60769 = CARTESIAN_POINT ( 'NONE',  ( 6.565887622018943937, 60.16530133659707502, 12.81628187352647430 ) ) ;
#60770 = EDGE_LOOP ( 'NONE', ( #64809, #55383, #22576, #23301 ) ) ;
#60771 = CARTESIAN_POINT ( 'NONE',  ( 2.791683348922237240, 5.383931151000785675, -7.208316651077763204 ) ) ;
#60772 = ORIENTED_EDGE ( 'NONE', *, *, #47745, .F. ) ;
#60773 = CARTESIAN_POINT ( 'NONE',  ( 17.08211943468705840, 15.13708216824730179, -12.26659068614894466 ) ) ;
#60774 = CARTESIAN_POINT ( 'NONE',  ( 5.076628168052703671, 26.84226448433411960, 8.527530157486179263 ) ) ;
#60775 = CARTESIAN_POINT ( 'NONE',  ( 7.084665262690076126, 34.10535201082151247, 10.88017736071109987 ) ) ;
#60776 = ORIENTED_EDGE ( 'NONE', *, *, #40653, .T. ) ;
#60777 = AXIS2_PLACEMENT_3D ( 'NONE', #35523, #5539, #73021 ) ;
#60778 = CARTESIAN_POINT ( 'NONE',  ( 0.5774900079438590739, 22.64701867748817321, -5.440088680355550821 ) ) ;
#60779 =( BOUNDED_CURVE ( )  B_SPLINE_CURVE ( 2, ( #94883, #26382, #56881, #18902, #26879, #28836, #42384, #35855, #88371, #72861, #5860, #96882, #36353 ),
 .UNSPECIFIED., .F., .F. ) 
 B_SPLINE_CURVE_WITH_KNOTS ( ( 3, 2, 2, 2, 2, 2, 3 ),
 ( 0.6333333333333333037, 0.6388888888888888395, 0.6444444444444444864, 0.6500000000000000222, 0.6555555555555555580, 0.6611111111111110938, 0.6666666666666666297 ),
 .UNSPECIFIED. ) 
 CURVE ( )  GEOMETRIC_REPRESENTATION_ITEM ( )  RATIONAL_B_SPLINE_CURVE ( ( 1.000000000000000000, 0.9659258262890684232, 1.000000000000000000, 0.9659258262890684232, 1.000000000000000000, 0.9659258262890684232, 1.000000000000000000, 0.9659258262890684232, 1.000000000000000000, 0.9659258262890684232, 1.000000000000000000, 0.9659258262890684232, 1.000000000000000000 ) ) 
 REPRESENTATION_ITEM ( '' )  );
#60780 = ORIENTED_EDGE ( 'NONE', *, *, #22369, .F. ) ;
#60781 = CARTESIAN_POINT ( 'NONE',  ( 20.88017736071110164, 30.35535201082151247, 2.915334737309930979 ) ) ;
#60782 = CIRCLE ( 'NONE', #22469, 0.2500000000000002220 ) ;
#60783 = CARTESIAN_POINT ( 'NONE',  ( 2.603489959281590771, 46.58210964143328425, 6.500000000000003553 ) ) ;
#60784 = ORIENTED_EDGE ( 'NONE', *, *, #83927, .T. ) ;
#60785 = CARTESIAN_POINT ( 'NONE',  ( 16.40814093676323893, 15.79030133659708746, 11.09922568453595026 ) ) ;
#60786 = CARTESIAN_POINT ( 'NONE',  ( 1.046131998949937580, 20.73810908735720560, 6.499999999999992006 ) ) ;
#60787 = CARTESIAN_POINT ( 'NONE',  ( 1.472469842513823179, 11.42559781766745175, 4.923371831947296329 ) ) ;
#60788 =( LENGTH_UNIT ( ) NAMED_UNIT ( * ) SI_UNIT ( .MILLI., .METRE. ) );
#60789 = CARTESIAN_POINT ( 'NONE',  ( 0.2751277870542914172, 58.21833443783938833, 6.499999999999992006 ) ) ;
#60790 = CARTESIAN_POINT ( 'NONE',  ( 5.076628168052704559, 15.17559781766745175, -8.527530157486179263 ) ) ;
#60791 = CARTESIAN_POINT ( 'NONE',  ( 2.035157376598824452, 28.68868534415484106, 7.964842623401179544 ) ) ;
#60792 = EDGE_CURVE ( 'NONE', #37672, #16289, #83438, .T. ) ;
#60793 = EDGE_LOOP ( 'NONE', ( #8610, #56733, #26445, #37390 ) ) ;
#60794 = DIRECTION ( 'NONE',  ( -0.6883545756937501370, 0.000000000000000000, -0.7253743710122912969 ) ) ;
#60795 = CARTESIAN_POINT ( 'NONE',  ( 17.96484262340118221, 39.93868534415484106, 7.964842623401181321 ) ) ;
#60796 = CARTESIAN_POINT ( 'NONE',  ( 12.34086200392826882, -0.03417435944610275333, -7.124999999999971578 ) ) ;
#60797 = CARTESIAN_POINT ( 'NONE',  ( 6.565887622018943937, 58.08196800326376064, -12.81628187352647608 ) ) ;
#60798 = CARTESIAN_POINT ( 'NONE',  ( 12.91533473730992121, 54.52201867748816255, 10.88017736071110164 ) ) ;
#60799 = CARTESIAN_POINT ( 'NONE',  ( 17.20831665107776587, 64.13393115100079456, -7.208316651077762316 ) ) ;
#60800 = FACE_OUTER_BOUND ( 'NONE', #14700, .T. ) ;
#60801 = CARTESIAN_POINT ( 'NONE',  ( 0.1532563361054083140, 16.00893115100078390, 1.131784320476157264E-15 ) ) ;
#60802 = CARTESIAN_POINT ( 'NONE',  ( 0.6178305044545818747, 48.49863466993042493, -9.382169495545419124 ) ) ;
#60803 = DIRECTION ( 'NONE',  ( 0.000000000000000000, 0.000000000000000000, 1.000000000000000000 ) ) ;
#60804 = CARTESIAN_POINT ( 'NONE',  ( 2.791683348922240793, 11.63393115100078568, 7.208316651077764092 ) ) ;
#60805 = CARTESIAN_POINT ( 'NONE',  ( 3.591859063236763294, 13.29030133659708746, -11.09922568453595026 ) ) ;
#60807 = DIRECTION ( 'NONE',  ( 1.000000000000000000, 0.000000000000000000, 0.000000000000000000 ) ) ;
#60806 = LINE ( 'NONE', #46311, #57990 ) ;
#60808 = CARTESIAN_POINT ( 'NONE',  ( 15.44008868035555793, 31.39701867748817676, -9.422509992056140149 ) ) ;
#60809 = CARTESIAN_POINT ( 'NONE',  ( 7.361572987183169658, 59.96726448433410894, -9.846743663894592657 ) ) ;
#60810 = CARTESIAN_POINT ( 'NONE',  ( -7.750000000000000000, 0.000000000000000000, 3.750000000000000000 ) ) ;
#60811 = CARTESIAN_POINT ( 'NONE',  ( 18.52753015748618282, 23.92559781766745530, -4.923371831947291888 ) ) ;
#60812 = CARTESIAN_POINT ( 'NONE',  ( 10.00000000000000000, 9.758931151000785675, -9.846743663894594434 ) ) ;
#60814 = ORIENTED_EDGE ( 'NONE', *, *, #27988, .T. ) ;
#60813 = CARTESIAN_POINT ( 'NONE',  ( 3.591859063236761518, 4.956968003263753531, 11.09922568453594849 ) ) ;
#60815 = CARTESIAN_POINT ( 'NONE',  ( 7.084665262690076126, 7.022018677488169658, -10.88017736071110164 ) ) ;
#60816 = CARTESIAN_POINT ( 'NONE',  ( 1.472469842513823179, 61.42559781766745175, 4.923371831947296329 ) ) ;
#60817 = B_SPLINE_CURVE_WITH_KNOTS ( 'NONE', 3,
 ( #8620, #55088, #69129, #92116, #77594, #53618 ),
 .UNSPECIFIED., .F., .F.,
 ( 4, 2, 4 ),
 ( 0.0002800124554126355017, 0.0006862178066638149887, 0.001092423157914994367 ),
 .UNSPECIFIED. ) ;
#60818 = AXIS2_PLACEMENT_3D ( 'NONE', #41936, #71446, #2960 ) ;
#60819 = CARTESIAN_POINT ( 'NONE',  ( 6.683985746565565655, -73.15435785421902892, -2.500000000000000888 ) ) ;
#60820 = CARTESIAN_POINT ( 'NONE',  ( 4.559911319644449179, 2.230352010821504916, -9.422509992056141925 ) ) ;
#60821 = CARTESIAN_POINT ( 'NONE',  ( 5.076628168052703671, 51.84226448433412315, 8.527530157486179263 ) ) ;
#60822 = EDGE_CURVE ( 'NONE', #82667, #88856, #13967, .T. ) ;
#60823 = CARTESIAN_POINT ( 'NONE',  ( 0.2751277870542981341, 18.21833443783937767, 6.500000000000002665 ) ) ;
#60824 = CARTESIAN_POINT ( 'NONE',  ( 20.88017736071110519, 5.563685344154838397, 2.639326808657452039E-16 ) ) ;
#60825 = PLANE ( 'NONE',  #95059 ) ;
#60826 = CARTESIAN_POINT ( 'NONE',  ( 20.88017736071110519, 35.56368534415484106, 2.639326808657452039E-16 ) ) ;
#60827 = CARTESIAN_POINT ( 'NONE',  ( 24.16423886937410614, 44.30374883491397497, 8.672049930838204340E-16 ) ) ;
#60829 = CYLINDRICAL_SURFACE ( 'NONE', #92571, 0.5000000000000004441 ) ;
#60828 = CARTESIAN_POINT ( 'NONE',  ( 12.91533473730992121, 4.522018677488170546, 10.88017736071110164 ) ) ;
#60830 = FACE_OUTER_BOUND ( 'NONE', #23945, .T. ) ;
#60831 = CARTESIAN_POINT ( 'NONE',  ( 18.52753015748617571, 28.09226448433411960, 4.923371831947298993 ) ) ;
#60832 = CARTESIAN_POINT ( 'NONE',  ( 19.38216949554541557, 17.24863466993041783, -9.382169495545420901 ) ) ;
#60833 = VECTOR ( 'NONE', #93773, 1000.000000000000000 ) ;
#60834 = CARTESIAN_POINT ( 'NONE',  ( -46.48928645636214441, 103.2957187381728232, 6.397878122523972699 ) ) ;
#60835 = CARTESIAN_POINT ( 'NONE',  ( 13.55255535720595184, -0.03417435944610275333, -4.403492169842965431 ) ) ;
#60836 = CARTESIAN_POINT ( 'NONE',  ( 17.20831665107776587, 57.88393115100078745, 7.208316651077764980 ) ) ;
#60837 = CYLINDRICAL_SURFACE ( 'NONE', #29929, 0.5000000000000004441 ) ;
#60838 = EDGE_CURVE ( 'NONE', #16656, #48202, #67452, .T. ) ;
#60839 = CARTESIAN_POINT ( 'NONE',  ( -9.793405416303651023, -28.00185549904734472, -4.000000000000000888 ) ) ;
#60840 = CARTESIAN_POINT ( 'NONE',  ( 20.36894250292379382, 13.67874883491396965, 10.36894250292379205 ) ) ;
#60841 = AXIS2_PLACEMENT_3D ( 'NONE', #82818, #23329, #60803 ) ;
#60842 = CARTESIAN_POINT ( 'NONE',  ( 0.1532563361054082862, 21.21726448433412315, 2.638427012816831674 ) ) ;
#60843 = DIRECTION ( 'NONE',  ( 0.4924235601034769316, 0.000000000000000000, -0.8703556959398940363 ) ) ;
#60844 = CARTESIAN_POINT ( 'NONE',  ( 13.79529636645031943, 50.34541550158064638, -14.16423886937409904 ) ) ;
#60845 = ADVANCED_FACE ( 'NONE', ( #22452 ), #22953, .T. ) ;
#60846 = CARTESIAN_POINT ( 'NONE',  ( 0.1532563361054100626, 5.800597817667452638, -2.638427012816831230 ) ) ;
#60848 = CARTESIAN_POINT ( 'NONE',  ( 12.87890026492933515, 14.95077488074853456, 7.195834080858436899 ) ) ;
#60847 = DIRECTION ( 'NONE',  ( -1.000000000000000000, 0.000000000000000000, 0.000000000000000000 ) ) ;
#60849 = CARTESIAN_POINT ( 'NONE',  ( -0.8801773607111008646, 38.27201867748816255, 2.915334737309923430 ) ) ;
#60850 = CARTESIAN_POINT ( 'NONE',  ( 21.09922568453595559, 47.04030133659708923, -6.408140936763230044 ) ) ;
#60851 = CARTESIAN_POINT ( 'NONE',  ( 20.88017736071110875, 10.77201867748817143, -2.915334737309920765 ) ) ;
#60852 = CARTESIAN_POINT ( 'NONE',  ( 0.6178305044545818747, 33.49863466993042493, -9.382169495545419124 ) ) ;
#60853 = CARTESIAN_POINT ( 'NONE',  ( -2.816281873526473856, 4.331968003263754419, 3.434112377981055619 ) ) ;
#60854 = CARTESIAN_POINT ( 'NONE',  ( 1.472469842513823179, 6.425597817667451750, 4.923371831947296329 ) ) ;
#60855 = ORIENTED_EDGE ( 'NONE', *, *, #73045, .F. ) ;
#60856 = CARTESIAN_POINT ( 'NONE',  ( 2.377183314879979470, 10.78593319516822646, -6.500000000000010658 ) ) ;
#60857 = CARTESIAN_POINT ( 'NONE',  ( -14.99847009497948136, 0.3639309181704115104, -0.2142307401082224061 ) ) ;
#60858 = CARTESIAN_POINT ( 'NONE',  ( 2.917880565312948704, 42.63708216824729647, 12.26659068614894643 ) ) ;
#60859 = CARTESIAN_POINT ( 'NONE',  ( -0.3689425029237898834, 11.17874883491396787, -10.36894250292378850 ) ) ;
#60860 = CARTESIAN_POINT ( 'NONE',  ( -0.8801773607111009756, 3.063685344154837509, 1.068504757029289695E-15 ) ) ;
#60861 = CARTESIAN_POINT ( 'NONE',  ( -0.8801773607111008646, 33.27201867748817676, 2.915334737309923430 ) ) ;
#60862 = CARTESIAN_POINT ( 'NONE',  ( -6.000000000000009770, 40.74999999999999289, 4.000000000000000000 ) ) ;
#60863 = DIRECTION ( 'NONE',  ( 4.440892098500626162E-14, 0.000000000000000000, 1.000000000000000000 ) ) ;
#60864 = CARTESIAN_POINT ( 'NONE',  ( -0.8801773607111008646, 48.27201867748816966, 2.915334737309923430 ) ) ;
#60865 = CARTESIAN_POINT ( 'NONE',  ( 7.084665262690076126, 69.10535201082151957, 10.88017736071109987 ) ) ;
#60866 = CARTESIAN_POINT ( 'NONE',  ( 6.565887622018943937, 30.16530133659708568, 12.81628187352647430 ) ) ;
#60867 = CARTESIAN_POINT ( 'NONE',  ( 0.5600000000000083800, 105.0000000000000000, -5.000000000000000000 ) ) ;
#60868 = CARTESIAN_POINT ( 'NONE',  ( -9.722841580490317881, -0.03417435944610275333, -12.70211588817950066 ) ) ;
#60869 = CARTESIAN_POINT ( 'NONE',  ( 18.52753015748618282, 38.92559781766745175, -4.923371831947291888 ) ) ;
#60871 = EDGE_CURVE ( 'NONE', #16289, #25004, #74176, .T. ) ;
#60870 = CARTESIAN_POINT ( 'NONE',  ( 16.40814093676324603, 17.45696800326375353, -11.09922568453594671 ) ) ;
#60872 = CARTESIAN_POINT ( 'NONE',  ( 17.20831665107776587, 7.883931151000784787, 7.208316651077764980 ) ) ;
#60873 = CARTESIAN_POINT ( 'NONE',  ( 20.88017736071110875, 15.77201867748817143, -2.915334737309920765 ) ) ;
#60874 = CARTESIAN_POINT ( 'NONE',  ( 19.84674366389459266, 38.30059781766745175, 2.638427012816836559 ) ) ;
#60875 = CARTESIAN_POINT ( 'NONE',  ( 19.38216949554541557, 62.24863466993041072, -9.382169495545420901 ) ) ;
#60876 = CARTESIAN_POINT ( 'NONE',  ( 14.92337183194729988, 24.34226448433411960, -8.527530157486177487 ) ) ;
#60877 = CARTESIAN_POINT ( 'NONE',  ( 2.917880565312948704, 7.637082168247301794, 12.26659068614894643 ) ) ;
#60878 = CARTESIAN_POINT ( 'NONE',  ( -3.750000000000000000, 0.000000000000000000, 2.750000000000000000 ) ) ;
#60879 = CARTESIAN_POINT ( 'NONE',  ( 2.035157376598824452, 28.68868534415484106, 7.964842623401179544 ) ) ;
#60881 = CARTESIAN_POINT ( 'NONE',  ( -2.266590686148945544, 37.22041550158063217, 7.082119434687048631 ) ) ;
#60880 = CARTESIAN_POINT ( 'NONE',  ( 0.5774900079438590739, 12.64701867748817143, -5.440088680355550821 ) ) ;
#60882 = ADVANCED_FACE ( 'NONE', ( #97973 ), #15526, .T. ) ;
#60883 = CARTESIAN_POINT ( 'NONE',  ( 20.88017736071110164, 30.35535201082151247, 2.915334737309930979 ) ) ;
#60884 = CARTESIAN_POINT ( 'NONE',  ( 15.44008868035555793, 16.39701867748817321, -9.422509992056140149 ) ) ;
#60885 = ORIENTED_EDGE ( 'NONE', *, *, #45642, .T. ) ;
#60886 = CARTESIAN_POINT ( 'NONE',  ( 10.00000000000000178, 44.31368534415484106, 10.88017736071110342 ) ) ;
#60887 = AXIS2_PLACEMENT_3D ( 'NONE', #62802, #3297, #9816 ) ;
#60888 = CARTESIAN_POINT ( 'NONE',  ( 21.09922568453595559, 42.04030133659708213, -6.408140936763230044 ) ) ;
#60889 = CARTESIAN_POINT ( 'NONE',  ( 10.00000000000000178, 49.31368534415484106, 10.88017736071110342 ) ) ;
#60891 = CARTESIAN_POINT ( 'NONE',  ( 15.44008868035555260, 49.73035201082150536, 9.422509992056143702 ) ) ;
#60890 = SURFACE_STYLE_FILL_AREA ( #59900 ) ;
#60892 = VERTEX_POINT ( 'NONE', #74217 ) ;
#60893 = CARTESIAN_POINT ( 'NONE',  ( -0.8801773607111009756, 53.06368534415484106, 1.068504757029289695E-15 ) ) ;
#60894 = DIRECTION ( 'NONE',  ( 0.000000000000000000, 1.000000000000000000, 0.000000000000000000 ) ) ;
#60895 = CIRCLE ( 'NONE', #96096, 0.2500000000000002220 ) ;
#60896 = CYLINDRICAL_SURFACE ( 'NONE', #41298, 0.2500000000000002220 ) ;
#60897 = CARTESIAN_POINT ( 'NONE',  ( 24.16423886937410614, 49.30374883491396787, 8.672049930838204340E-16 ) ) ;
#60898 = CARTESIAN_POINT ( 'NONE',  ( 4.559911319644449179, 62.23035201082150536, -9.422509992056141925 ) ) ;
#60899 = SURFACE_STYLE_FILL_AREA ( #83905 ) ;
#60900 = CARTESIAN_POINT ( 'NONE',  ( -43.70923076923077844, 103.3461538461538396, -9.500000000000000000 ) ) ;
#60901 = CARTESIAN_POINT ( 'NONE',  ( 10.00000000000000000, 59.75893115100078745, -9.846743663894594434 ) ) ;
#60902 = CARTESIAN_POINT ( 'NONE',  ( -14.11917416961162353, 0.2306972965111909191, -4.887430353539129690 ) ) ;
#60903 = CARTESIAN_POINT ( 'NONE',  ( 19.84674366389459621, 33.50893115100078745, 7.409399052514197653E-17 ) ) ;
#60904 = ORIENTED_EDGE ( 'NONE', *, *, #8210, .T. ) ;
#60905 = CARTESIAN_POINT ( 'NONE',  ( 1.472469842513823179, 31.42559781766745530, 4.923371831947296329 ) ) ;
#60906 = CARTESIAN_POINT ( 'NONE',  ( 12.81628187352647608, -8.376365330069578619, -2.602085213965210642E-15 ) ) ;
#60907 = CARTESIAN_POINT ( 'NONE',  ( 12.91533473730992121, 24.52201867748816966, 10.88017736071110164 ) ) ;
#60908 = CARTESIAN_POINT ( 'NONE',  ( 10.00000000000000178, 37.25893115100078745, 9.846743663894594434 ) ) ;
#60910 = CARTESIAN_POINT ( 'NONE',  ( 21.09922568453595559, 27.04030133659708568, -6.408140936763230044 ) ) ;
#60909 = AXIS2_PLACEMENT_3D ( 'NONE', #12137, #42640, #78676 ) ;
#60911 = DIRECTION ( 'NONE',  ( 0.000000000000000000, 0.000000000000000000, 1.000000000000000000 ) ) ;
#60912 = CARTESIAN_POINT ( 'NONE',  ( 15.44008868035555793, 46.39701867748817676, -9.422509992056140149 ) ) ;
#60913 = CARTESIAN_POINT ( 'NONE',  ( 22.26659068614895176, 64.72041550158064638, -7.082119434687042414 ) ) ;
#60914 = CARTESIAN_POINT ( 'NONE',  ( 3.591859063236763294, 28.29030133659708568, -11.09922568453595026 ) ) ;
#60915 = LINE ( 'NONE', #47384, #5235 ) ;
#60916 = ORIENTED_EDGE ( 'NONE', *, *, #46150, .F. ) ;
#60917 = CARTESIAN_POINT ( 'NONE',  ( 22.81628187352648496, 11.83196800326375531, -3.434112377981050290 ) ) ;
#60918 = CARTESIAN_POINT ( 'NONE',  ( 15.44008868035555793, 21.39701867748817321, -9.422509992056140149 ) ) ;
#60919 = CARTESIAN_POINT ( 'NONE',  ( 7.084665262690076126, 59.10535201082150536, 10.88017736071109987 ) ) ;
#60920 = CIRCLE ( 'NONE', #81612, 18.93999999999999773 ) ;
#60921 = ORIENTED_EDGE ( 'NONE', *, *, #48100, .T. ) ;
#60922 = CARTESIAN_POINT ( 'NONE',  ( -0.8801773607111008646, 63.27201867748817676, 2.915334737309923430 ) ) ;
#60923 = AXIS2_PLACEMENT_3D ( 'NONE', #72606, #11625, #80622 ) ;
#60924 = CARTESIAN_POINT ( 'NONE',  ( 1.472469842513823179, 40.59226448433411605, -4.923371831947296329 ) ) ;
#60925 = CARTESIAN_POINT ( 'NONE',  ( 12.63842701281683922, 19.55059781766745175, -9.846743663894590881 ) ) ;
#60926 = CARTESIAN_POINT ( 'NONE',  ( 0.1532563361054083140, 11.00893115100078568, 1.131784320476157264E-15 ) ) ;
#60927 = CARTESIAN_POINT ( 'NONE',  ( 20.15039907845753220, 57.62777174578613426, -6.262539305110077947 ) ) ;
#60929 = CARTESIAN_POINT ( 'NONE',  ( 22.81628187352648496, 41.83196800326375353, -3.434112377981050290 ) ) ;
#60928 = FACE_OUTER_BOUND ( 'NONE', #21842, .T. ) ;
#60931 = CARTESIAN_POINT ( 'NONE',  ( -8.157990163924628391, 14.76930270348881002, -12.51739793958124380 ) ) ;
#60930 = CARTESIAN_POINT ( 'NONE',  ( 19.84674366389459266, 18.30059781766745175, 2.638427012816836559 ) ) ;
#60932 = CARTESIAN_POINT ( 'NONE',  ( 20.32896413005680358, 44.74545670184113533, 5.963430220938287007 ) ) ;
#60934 = ORIENTED_EDGE ( 'NONE', *, *, #67409, .F. ) ;
#60933 = CARTESIAN_POINT ( 'NONE',  ( 0.1532563361054083140, 36.00893115100078745, 1.131784320476157264E-15 ) ) ;
#60935 = CARTESIAN_POINT ( 'NONE',  ( 21.09922568453595559, 7.040301336597086568, -6.408140936763230044 ) ) ;
#60936 = CARTESIAN_POINT ( 'NONE',  ( 7.084665262690076126, 49.10535201082149825, 10.88017736071109987 ) ) ;
#60937 = CARTESIAN_POINT ( 'NONE',  ( 10.00000000000000178, 33.05374883491396787, 14.16423886937410082 ) ) ;
#60938 = CARTESIAN_POINT ( 'NONE',  ( -8.854007681963667054, 87.37522428062567315, 4.483348028977646393 ) ) ;
#60939 = CARTESIAN_POINT ( 'NONE',  ( -2.266590686148945544, 31.38708216824730002, -7.082119434687050408 ) ) ;
#60940 = CARTESIAN_POINT ( 'NONE',  ( 24.16423886937410614, 64.30374883491396076, 8.672049930838204340E-16 ) ) ;
#60941 = CARTESIAN_POINT ( 'NONE',  ( 24.16423886937409904, 14.09541550158063217, 3.795296366450317205 ) ) ;
#60943 = CARTESIAN_POINT ( 'NONE',  ( -2.863771337576333842, 14.95037103301162418, -14.47259902956233013 ) ) ;
#60942 = CARTESIAN_POINT ( 'NONE',  ( 20.36894250292379738, 19.92874883491396787, -10.36894250292379027 ) ) ;
#60944 = CARTESIAN_POINT ( 'NONE',  ( 4.559911319644449179, 53.89701867748817676, 9.422509992056141925 ) ) ;
#60945 = CARTESIAN_POINT ( 'NONE',  ( -11.25000000000000178, 9.909700295649315649, -3.014428414850122806 ) ) ;
#60946 = ADVANCED_FACE ( 'NONE', ( #12738 ), #50753, .F. ) ;
#60948 = CARTESIAN_POINT ( 'NONE',  ( 7.361572987183170547, 47.05059781766745175, 9.846743663894590881 ) ) ;
#60947 = CARTESIAN_POINT ( 'NONE',  ( 18.95785429995052596, 62.24216108172004880, 6.499999999999944933 ) ) ;
#60949 = CARTESIAN_POINT ( 'NONE',  ( 7.084665262690076126, 27.02201867748817676, -10.88017736071110164 ) ) ;
#60950 = DIRECTION ( 'NONE',  ( -0.000000000000000000, -1.000000000000000000, -0.000000000000000000 ) ) ;
#60951 = CARTESIAN_POINT ( 'NONE',  ( 19.84674366389459621, 58.50893115100078745, 7.409399052514197653E-17 ) ) ;
#60952 = CARTESIAN_POINT ( 'NONE',  ( 19.50000000000000711, 79.40087001978915282, -5.000000000000000888 ) ) ;
#60953 = CARTESIAN_POINT ( 'NONE',  ( 5.076628168052703671, 31.84226448433412315, 8.527530157486179263 ) ) ;
#60954 = CARTESIAN_POINT ( 'NONE',  ( 19.38216949554541557, 52.24863466993041072, -9.382169495545420901 ) ) ;
#60955 = CARTESIAN_POINT ( 'NONE',  ( -10.36894250292378317, -7.571251165086024137, 10.36894250292379560 ) ) ;
#60956 = CARTESIAN_POINT ( 'NONE',  ( 19.84674366389459266, 43.71726448433410894, -2.638427012816827677 ) ) ;
#60957 = CARTESIAN_POINT ( 'NONE',  ( 12.63842701281683034, 52.46726448433413026, 9.846743663894596210 ) ) ;
#60958 = EDGE_CURVE ( 'NONE', #61160, #92057, #87256, .T. ) ;
#60959 = CARTESIAN_POINT ( 'NONE',  ( 2.917880565312948704, 37.63708216824731068, 12.26659068614894643 ) ) ;
#60960 = ORIENTED_EDGE ( 'NONE', *, *, #65283, .T. ) ;
#60961 = CARTESIAN_POINT ( 'NONE',  ( 24.16423886937409904, 14.09541550158063217, 3.795296366450317205 ) ) ;
#60962 = EDGE_CURVE ( 'NONE', #76972, #35320, #97754, .T. ) ;
#60963 = CARTESIAN_POINT ( 'NONE',  ( 2.035157376598824452, 68.68868534415484817, 7.964842623401179544 ) ) ;
#60964 = DIRECTION ( 'NONE',  ( -1.000000000000000000, -1.244644646440729013E-15, 0.000000000000000000 ) ) ;
#60965 = CARTESIAN_POINT ( 'NONE',  ( 22.26659068614895176, 59.72041550158063927, -7.082119434687042414 ) ) ;
#60966 = CARTESIAN_POINT ( 'NONE',  ( 19.38216949554541202, 10.99863466993042138, 9.382169495545424454 ) ) ;
#60967 = DIRECTION ( 'NONE',  ( -0.3665012267243009103, 0.000000000000000000, 0.9304175679820231304 ) ) ;
#60968 = CARTESIAN_POINT ( 'NONE',  ( -0.8801773607110991993, 52.85535201082151247, -2.915334737309923874 ) ) ;
#60969 = CARTESIAN_POINT ( 'NONE',  ( 1.274849032794294290, 58.57228050351032778, 6.499999999999979572 ) ) ;
#60970 = CARTESIAN_POINT ( 'NONE',  ( 0.1532563361054083140, 31.00893115100078390, 1.131784320476157264E-15 ) ) ;
#60971 = CARTESIAN_POINT ( 'NONE',  ( -2.266590686148945544, 57.22041550158063217, 7.082119434687048631 ) ) ;
#60972 = CARTESIAN_POINT ( 'NONE',  ( -10.88017736071109987, 33.27201867748819097, 2.915334737309934532 ) ) ;
#60973 = CARTESIAN_POINT ( 'NONE',  ( 15.44008868035555793, 16.39701867748817321, -9.422509992056140149 ) ) ;
#60974 = CARTESIAN_POINT ( 'NONE',  ( 20.88017736071110875, 30.77201867748816966, -2.915334737309920765 ) ) ;
#60975 = CARTESIAN_POINT ( 'NONE',  ( 1.472469842513823179, 50.59226448433411605, -4.923371831947296329 ) ) ;
#60976 = CARTESIAN_POINT ( 'NONE',  ( 0.1532563361054100626, 50.80059781766745175, -2.638427012816831230 ) ) ;
#60977 = CARTESIAN_POINT ( 'NONE',  ( 19.38216949554541557, 47.24863466993041783, -9.382169495545420901 ) ) ;
#60978 = CARTESIAN_POINT ( 'NONE',  ( 7.361572987183169658, -0.03273551566588185635, -9.846743663894592657 ) ) ;
#60979 = EDGE_LOOP ( 'NONE', ( #43853, #2574, #31794, #62512 ) ) ;
#60980 = CARTESIAN_POINT ( 'NONE',  ( 17.96484262340118221, 21.18868534415483396, -7.964842623401177768 ) ) ;
#60981 = CARTESIAN_POINT ( 'NONE',  ( 6.565887622018943937, 20.16530133659708213, 12.81628187352647430 ) ) ;
#60982 = CARTESIAN_POINT ( 'NONE',  ( -15.94536257719939698, -0.03417435944610275333, -1.273895096820171657 ) ) ;
#60983 = CIRCLE ( 'NONE', #21094, 14.49999999999999822 ) ;
#60984 = CARTESIAN_POINT ( 'NONE',  ( 7.361572987183169658, 54.96726448433413026, -9.846743663894592657 ) ) ;
#60985 = CARTESIAN_POINT ( 'NONE',  ( 15.44008868035555260, 29.73035201082150891, 9.422509992056143702 ) ) ;
#60986 = CARTESIAN_POINT ( 'NONE',  ( 22.81628187352647785, 26.41530133659708923, 3.434112377981063169 ) ) ;
#60988 = CARTESIAN_POINT ( 'NONE',  ( 0.000000000000000000, 15.00000000000000000, 0.000000000000000000 ) ) ;
#60987 = CARTESIAN_POINT ( 'NONE',  ( 15.44008868035555793, 46.39701867748817676, -9.422509992056140149 ) ) ;
#60989 = CARTESIAN_POINT ( 'NONE',  ( -5.149999999999995026, 98.50000000000000000, -8.000000000000000000 ) ) ;
#60990 = CIRCLE ( 'NONE', #78558, 0.2500000000000002220 ) ;
#60991 = CARTESIAN_POINT ( 'NONE',  ( 10.00000000000000000, 47.87363466993042493, -12.81628187352647608 ) ) ;
#60992 = VERTEX_POINT ( 'NONE', #58221 ) ;
#60993 = CARTESIAN_POINT ( 'NONE',  ( 19.84674366389459266, 63.71726448433412315, -2.638427012816827677 ) ) ;
#60994 = CARTESIAN_POINT ( 'NONE',  ( 17.96484262340118221, 51.18868534415483396, -7.964842623401177768 ) ) ;
#60996 = CARTESIAN_POINT ( 'NONE',  ( 13.79529636645030344, 3.262082168247301350, 14.16423886937410614 ) ) ;
#60995 = CARTESIAN_POINT ( 'NONE',  ( 16.40814093676323893, 35.79030133659708923, 11.09922568453595026 ) ) ;
#60997 = EDGE_CURVE ( 'NONE', #24087, #3541, #8497, .T. ) ;
#60998 = CARTESIAN_POINT ( 'NONE',  ( 7.084665262690076126, 47.02201867748818387, -10.88017736071110164 ) ) ;
#60999 = MECHANICAL_DESIGN_GEOMETRIC_PRESENTATION_REPRESENTATION (  '', ( #97791 ), #11536 ) ;
#61000 = CARTESIAN_POINT ( 'NONE',  ( 2.917880565312948704, 47.63708216824730357, 12.26659068614894643 ) ) ;
#61001 = FACE_OUTER_BOUND ( 'NONE', #90059, .T. ) ;
#61002 = CARTESIAN_POINT ( 'NONE',  ( 10.00000000000000000, 14.75893115100078568, -9.846743663894594434 ) ) ;
#61003 = CARTESIAN_POINT ( 'NONE',  ( 18.52753015748617571, 8.092264484334117824, 4.923371831947298993 ) ) ;
#61004 = LINE ( 'NONE', #55, #63501 ) ;
#61005 = CARTESIAN_POINT ( 'NONE',  ( 24.16423886937410614, 39.51208216824731068, -3.795296366450302550 ) ) ;
#61006 = STYLED_ITEM ( 'NONE', ( #61456 ), #75652 ) ;
#61007 = CARTESIAN_POINT ( 'NONE',  ( 6.382347221874455023, 14.63606860869882986, -13.57444820018230480 ) ) ;
#61008 = CARTESIAN_POINT ( 'NONE',  ( 2.035157376598824452, 13.68868534415483751, 7.964842623401179544 ) ) ;
#61009 = CARTESIAN_POINT ( 'NONE',  ( -1.783843307429720415, 13.12729635533385597, -10.00000000000000000 ) ) ;
#61010 = B_SPLINE_CURVE_WITH_KNOTS ( 'NONE', 3,
 ( #66829, #81340, #80361, #28340, #95867, #27350 ),
 .UNSPECIFIED., .F., .F.,
 ( 4, 2, 4 ),
 ( 3.409110551496214039E-05, 0.0004400426677368013710, 0.0008459942299586405406 ),
 .UNSPECIFIED. ) ;
#61011 = ORIENTED_EDGE ( 'NONE', *, *, #1268, .T. ) ;
#61012 = ORIENTED_EDGE ( 'NONE', *, *, #28997, .T. ) ;
#61013 = CARTESIAN_POINT ( 'NONE',  ( 7.084665262690076126, 14.10535201082150358, 10.88017736071109987 ) ) ;
#61014 = CARTESIAN_POINT ( 'NONE',  ( -4.164238869374099927, 62.01208216824728936, 3.795296366450308767 ) ) ;
#61015 = CARTESIAN_POINT ( 'NONE',  ( 14.92337183194729633, 47.67559781766745175, 8.527530157486181039 ) ) ;
#61016 = CARTESIAN_POINT ( 'NONE',  ( 22.81628187352648496, 36.83196800326376064, -3.434112377981050290 ) ) ;
#61018 = CARTESIAN_POINT ( 'NONE',  ( 17.08211943468705130, 3.470415501580634388, 12.26659068614894998 ) ) ;
#61017 = CARTESIAN_POINT ( 'NONE',  ( -13.38735934610854628, 90.81479509783851256, -7.611013694208273783 ) ) ;
#61019 = CARTESIAN_POINT ( 'NONE',  ( 10.00000000000000178, 24.31368534415484106, 10.88017736071110342 ) ) ;
#61020 = CARTESIAN_POINT ( 'NONE',  ( 24.16423886937410614, 64.51208216824728936, -3.795296366450302550 ) ) ;
#61021 = CARTESIAN_POINT ( 'NONE',  ( 2.791683348922240793, 41.63393115100078745, 7.208316651077764092 ) ) ;
#61022 = CARTESIAN_POINT ( 'NONE',  ( 18.28836319691942336, 44.34492782695770074, 6.500000000000077272 ) ) ;
#61023 = CARTESIAN_POINT ( 'NONE',  ( 7.361572987183170547, 17.05059781766745530, 9.846743663894590881 ) ) ;
#61024 = DIRECTION ( 'NONE',  ( -0.000000000000000000, 1.000000000000000000, -0.000000000000000000 ) ) ;
#61025 = CARTESIAN_POINT ( 'NONE',  ( 7.208316651077762316, 14.13393115100078923, -7.208316651077764980 ) ) ;
#61026 = ORIENTED_EDGE ( 'NONE', *, *, #12413, .F. ) ;
#61027 = CARTESIAN_POINT ( 'NONE',  ( 1.326261724323017699, 14.76984959128329677, -14.88164196614431845 ) ) ;
#61028 = ORIENTED_EDGE ( 'NONE', *, *, #21324, .T. ) ;
#61029 = CARTESIAN_POINT ( 'NONE',  ( 12.63842701281683034, 62.46726448433410894, 9.846743663894596210 ) ) ;
#61031 = CARTESIAN_POINT ( 'NONE',  ( 7.084665262690076126, 39.10535201082150536, 10.88017736071109987 ) ) ;
#61030 = CARTESIAN_POINT ( 'NONE',  ( 19.42250999205614193, 35.14701867748816966, 5.440088680355555262 ) ) ;
#61033 = CARTESIAN_POINT ( 'NONE',  ( 0.6178305044545818747, 28.49863466993041783, -9.382169495545419124 ) ) ;
#61032 = CARTESIAN_POINT ( 'NONE',  ( 10.00000000000000178, 62.25893115100078745, 9.846743663894594434 ) ) ;
#61034 = CARTESIAN_POINT ( 'NONE',  ( 24.16423886937410614, 14.30374883491396787, 8.672049930838204340E-16 ) ) ;
#61035 = CIRCLE ( 'NONE', #48326, 0.5000000000000004441 ) ;
#61036 = CARTESIAN_POINT ( 'NONE',  ( 22.81628187352648496, 41.83196800326375353, -3.434112377981050290 ) ) ;
#61037 = ORIENTED_EDGE ( 'NONE', *, *, #93966, .T. ) ;
#61038 = CARTESIAN_POINT ( 'NONE',  ( 7.361572987183170547, 42.05059781766745886, 9.846743663894590881 ) ) ;
#61039 = CARTESIAN_POINT ( 'NONE',  ( 12.91533473730992121, 9.522018677488171434, 10.88017736071110164 ) ) ;
#61040 = VERTEX_POINT ( 'NONE', #59719 ) ;
#61041 = CARTESIAN_POINT ( 'NONE',  ( 20.88017736071110875, 20.77201867748816611, -2.915334737309920765 ) ) ;
#61042 = EDGE_LOOP ( 'NONE', ( #10878, #59834, #41561, #71707 ) ) ;
#61043 = CARTESIAN_POINT ( 'NONE',  ( 0.5774900079438590739, 62.64701867748817676, -5.440088680355550821 ) ) ;
#61044 = CARTESIAN_POINT ( 'NONE',  ( 4.559911319644449179, 58.89701867748817676, 9.422509992056141925 ) ) ;
#61046 = ADVANCED_FACE ( 'NONE', ( #96763 ), #28238, .T. ) ;
#61045 = CARTESIAN_POINT ( 'NONE',  ( 19.42250999205614193, 60.14701867748817676, 5.440088680355555262 ) ) ;
#61047 = CARTESIAN_POINT ( 'NONE',  ( 0.1532563361054100626, 0.8005978176674514168, -2.638427012816831230 ) ) ;
#61048 = CARTESIAN_POINT ( 'NONE',  ( 10.00000000000000000, 51.81368534415484106, -10.88017736071110342 ) ) ;
#61049 = FACE_OUTER_BOUND ( 'NONE', #39182, .T. ) ;
#61050 = EDGE_CURVE ( 'NONE', #77207, #51781, #81437, .T. ) ;
#61051 = CARTESIAN_POINT ( 'NONE',  ( -46.94000000000247752, 100.6180954154858398, 9.128675877383326309 ) ) ;
#61054 = ORIENTED_EDGE ( 'NONE', *, *, #82507, .F. ) ;
#61053 = VECTOR ( 'NONE', #97733, 1000.000000000000000 ) ;
#61052 = DIRECTION ( 'NONE',  ( 0.000000000000000000, 0.000000000000000000, -1.000000000000000000 ) ) ;
#61055 = CARTESIAN_POINT ( 'NONE',  ( 5.076628168052703671, 46.84226448433412315, 8.527530157486179263 ) ) ;
#61056 = VERTEX_POINT ( 'NONE', #5750 ) ;
#61057 = FACE_OUTER_BOUND ( 'NONE', #21824, .T. ) ;
#61058 = CIRCLE ( 'NONE', #64250, 0.5000000000000004441 ) ;
#61059 = VECTOR ( 'NONE', #11137, 1000.000000000000000 ) ;
#61060 = B_SPLINE_CURVE_WITH_KNOTS ( 'NONE', 3,
 ( #56559, #87053, #1616, #78573 ),
 .UNSPECIFIED., .F., .F.,
 ( 4, 4 ),
 ( 1.361094815542225550E-17, 0.002562518741975313395 ),
 .UNSPECIFIED. ) ;
#61061 = AXIS2_PLACEMENT_3D ( 'NONE', #97961, #30901, #91413 ) ;
#61062 = CARTESIAN_POINT ( 'NONE',  ( 20.36894250292379382, 13.67874883491396965, 10.36894250292379205 ) ) ;
#61063 = EDGE_LOOP ( 'NONE', ( #32468, #39869, #37796, #84470, #87886, #88553 ) ) ;
#61064 = CARTESIAN_POINT ( 'NONE',  ( 0.000000000000000000, 15.00000000000000000, 0.000000000000000000 ) ) ;
#61065 = CARTESIAN_POINT ( 'NONE',  ( 0.000000000000000000, 0.5000000000000004441, 0.000000000000000000 ) ) ;
#61066 = CARTESIAN_POINT ( 'NONE',  ( 0.5774900079438590739, 7.647018677488171434, -5.440088680355550821 ) ) ;
#61067 = CARTESIAN_POINT ( 'NONE',  ( 3.591859063236763294, 38.29030133659708923, -11.09922568453595026 ) ) ;
#61069 = VECTOR ( 'NONE', #90848, 1000.000000000000000 ) ;
#61068 = CARTESIAN_POINT ( 'NONE',  ( 6.579634127946654587, -87.99828267815715321, -2.750000000000000444 ) ) ;
#61070 = CARTESIAN_POINT ( 'NONE',  ( 10.00000000000000000, 49.75893115100078745, -9.846743663894594434 ) ) ;
#61071 = CARTESIAN_POINT ( 'NONE',  ( 13.43411237798105340, 20.58196800326374643, 12.81628187352647963 ) ) ;
#61072 = CARTESIAN_POINT ( 'NONE',  ( 7.361572987183169658, 29.96726448433411960, -9.846743663894592657 ) ) ;
#61073 = CARTESIAN_POINT ( 'NONE',  ( -0.3077640640439943676, 70.00000000000000000, -6.000000000000270894 ) ) ;
#61074 = CARTESIAN_POINT ( 'NONE',  ( -1.099225684535947600, 18.70696800326375353, -6.408140936763238038 ) ) ;
#61075 = AXIS2_PLACEMENT_3D ( 'NONE', #2, #83959, #15485 ) ;
#61076 = DIRECTION ( 'NONE',  ( -0.5150380749100542666, 0.000000000000000000, 0.8571673007021122226 ) ) ;
#61077 = EDGE_CURVE ( 'NONE', #47253, #17634, #80257, .T. ) ;
#61078 = CARTESIAN_POINT ( 'NONE',  ( 14.92337183194729633, 12.67559781766745353, 8.527530157486181039 ) ) ;
#61079 = ORIENTED_EDGE ( 'NONE', *, *, #49247, .F. ) ;
#61080 = ORIENTED_EDGE ( 'NONE', *, *, #73156, .T. ) ;
#61081 = EDGE_CURVE ( 'NONE', #13218, #49035, #22523, .T. ) ;
#61082 = CARTESIAN_POINT ( 'NONE',  ( 10.00000000000000178, 24.31368534415484106, 10.88017736071110342 ) ) ;
#61083 = CARTESIAN_POINT ( 'NONE',  ( -0.3689425029237881626, 22.42874883491397142, 10.36894250292379027 ) ) ;
#61084 = CARTESIAN_POINT ( 'NONE',  ( 5.076628168052703671, 46.84226448433412315, 8.527530157486179263 ) ) ;
#61085 = CARTESIAN_POINT ( 'NONE',  ( 0.1532563361054100626, 5.800597817667452638, -2.638427012816831230 ) ) ;
#61087 = DIRECTION ( 'NONE',  ( 0.000000000000000000, 1.000000000000000000, 0.000000000000000000 ) ) ;
#61086 = CARTESIAN_POINT ( 'NONE',  ( -2.816281873526473856, 44.12363466993042493, 9.499525473075851096E-16 ) ) ;
#61088 = CARTESIAN_POINT ( 'NONE',  ( 7.084665262690076126, 19.10535201082150181, 10.88017736071109987 ) ) ;
#61089 = CARTESIAN_POINT ( 'NONE',  ( -13.82192141328807011, 3.982798640990670655E-16, -4.382292601468863680 ) ) ;
#61090 = AXIS2_PLACEMENT_3D ( 'NONE', #80493, #42492, #6960 ) ;
#61091 = CARTESIAN_POINT ( 'NONE',  ( 0.6178305044545838731, 9.748634669930416052, 9.382169495545420901 ) ) ;
#61092 = CARTESIAN_POINT ( 'NONE',  ( 18.52753015748617571, 23.09226448433411960, 4.923371831947298993 ) ) ;
#61093 = CARTESIAN_POINT ( 'NONE',  ( -10.88017736071109987, -6.727981322511824125, 2.915334737309934532 ) ) ;
#61094 = CARTESIAN_POINT ( 'NONE',  ( -1.099225684535947600, 33.70696800326375353, -6.408140936763238038 ) ) ;
#61095 = DIRECTION ( 'NONE',  ( 0.000000000000000000, -0.000000000000000000, 1.000000000000000000 ) ) ;
#61097 = DIRECTION ( 'NONE',  ( -8.673617379884027583E-16, -1.000000000000000000, 0.000000000000000000 ) ) ;
#61096 = CARTESIAN_POINT ( 'NONE',  ( -0.8801773607110991993, 52.85535201082151247, -2.915334737309923874 ) ) ;
#61098 = DIRECTION ( 'NONE',  ( 1.000000000000000000, 0.000000000000000000, 0.000000000000000000 ) ) ;
#61099 = CARTESIAN_POINT ( 'NONE',  ( -0.3093388210927806581, 14.63606905933214364, 14.99680997725070242 ) ) ;
#61100 = CARTESIAN_POINT ( 'NONE',  ( 0.5774900079438590739, 42.64701867748816966, -5.440088680355550821 ) ) ;
#61102 = CARTESIAN_POINT ( 'NONE',  ( 17.96484262340118221, 49.93868534415484106, 7.964842623401181321 ) ) ;
#61101 = AXIS2_PLACEMENT_3D ( 'NONE', #39790, #48254, #77769 ) ;
#61103 = CARTESIAN_POINT ( 'NONE',  ( 17.20831665107776587, 59.13393115100078745, -7.208316651077762316 ) ) ;
#61104 = CARTESIAN_POINT ( 'NONE',  ( 15.44008868035555793, 61.39701867748817676, -9.422509992056140149 ) ) ;
#61105 = ADVANCED_FACE ( 'NONE', ( #4767 ), #35238, .F. ) ;
#61106 = CARTESIAN_POINT ( 'NONE',  ( 2.791683348922237240, 55.38393115100078745, -7.208316651077763204 ) ) ;
#61108 = DIRECTION ( 'NONE',  ( -0.1478094111296046620, 0.000000000000000000, -0.9890158633619178241 ) ) ;
#61107 = CARTESIAN_POINT ( 'NONE',  ( -0.8801773607111009756, 8.063685344154837509, 1.068504757029289695E-15 ) ) ;
#61109 = CARTESIAN_POINT ( 'NONE',  ( 6.565887622018943937, 10.16530133659708746, 12.81628187352647430 ) ) ;
#61110 = ORIENTED_EDGE ( 'NONE', *, *, #25755, .F. ) ;
#61111 = CARTESIAN_POINT ( 'NONE',  ( 2.035157376598824452, 38.68868534415483396, 7.964842623401179544 ) ) ;
#61113 = FACE_OUTER_BOUND ( 'NONE', #16768, .T. ) ;
#61112 = CARTESIAN_POINT ( 'NONE',  ( 0.1532563361054082862, 61.21726448433412315, 2.638427012816831674 ) ) ;
#61114 = EDGE_CURVE ( 'NONE', #32515, #16129, #52227, .T. ) ;
#61115 = CARTESIAN_POINT ( 'NONE',  ( 10.00000000000000178, 14.31368534415483751, 10.88017736071110342 ) ) ;
#61116 = CARTESIAN_POINT ( 'NONE',  ( 17.96484262340118221, 21.18868534415483396, -7.964842623401177768 ) ) ;
#61117 = CARTESIAN_POINT ( 'NONE',  ( 2.917880565312950480, 35.97041550158063217, -12.26659068614894821 ) ) ;
#61118 = CARTESIAN_POINT ( 'NONE',  ( 17.20831665107776587, 27.88393115100078390, 7.208316651077764980 ) ) ;
#61119 = CARTESIAN_POINT ( 'NONE',  ( 0.5774900079438590739, 47.64701867748817676, -5.440088680355550821 ) ) ;
#61120 =( NAMED_UNIT ( * ) PLANE_ANGLE_UNIT ( ) SI_UNIT ( $, .RADIAN. ) );
#61121 = CIRCLE ( 'NONE', #33914, 2.750000000000000888 ) ;
#61122 = CARTESIAN_POINT ( 'NONE',  ( -46.68456736488007408, 103.6675473310227034, 5.775421524742653467 ) ) ;
#61123 = CARTESIAN_POINT ( 'NONE',  ( 19.84674366389459266, 58.30059781766745886, 2.638427012816836559 ) ) ;
#61124 = VERTEX_POINT ( 'NONE', #69695 ) ;
#61125 = ORIENTED_EDGE ( 'NONE', *, *, #37057, .T. ) ;
#61126 = CARTESIAN_POINT ( 'NONE',  ( 17.08211943468705840, 40.13708216824731068, -12.26659068614894466 ) ) ;
#61127 = CARTESIAN_POINT ( 'NONE',  ( 24.16423886937409904, 29.09541550158063572, 3.795296366450317205 ) ) ;
#61128 = CARTESIAN_POINT ( 'NONE',  ( 2.791683348922240793, 1.633931151000784565, 7.208316651077764092 ) ) ;
#61129 = CARTESIAN_POINT ( 'NONE',  ( 12.63842701281683922, 44.55059781766745175, -9.846743663894590881 ) ) ;
#61130 = CARTESIAN_POINT ( 'NONE',  ( -11.23896940073626105, -88.22260584719931842, 4.000000000000000000 ) ) ;
#61132 = CARTESIAN_POINT ( 'NONE',  ( 10.00000000000000178, 15.37363466993042138, 12.81628187352647608 ) ) ;
#61131 = CARTESIAN_POINT ( 'NONE',  ( 15.44008868035555260, 39.73035201082150536, 9.422509992056143702 ) ) ;
#61133 = CARTESIAN_POINT ( 'NONE',  ( 6.204703633549690345, 35.76208216824729647, -14.16423886937410259 ) ) ;
#61134 = CARTESIAN_POINT ( 'NONE',  ( 7.084665262690076126, 9.105352010821503583, 10.88017736071109987 ) ) ;
#61135 =( GEOMETRIC_REPRESENTATION_CONTEXT ( 3 ) GLOBAL_UNCERTAINTY_ASSIGNED_CONTEXT ( ( #25228 ) ) GLOBAL_UNIT_ASSIGNED_CONTEXT ( ( #77653, #23705, #8196 ) ) REPRESENTATION_CONTEXT ( 'NONE', 'WORKASPACE' ) );
#61136 = CARTESIAN_POINT ( 'NONE',  ( -0.8801773607111009756, 28.06368534415484106, 1.068504757029289695E-15 ) ) ;
#61137 = VECTOR ( 'NONE', #32910, 1000.000000000000000 ) ;
#61138 = PLANE ( 'NONE',  #9264 ) ;
#61139 = CARTESIAN_POINT ( 'NONE',  ( -0.8801773607111009756, 63.06368534415484106, 1.068504757029289695E-15 ) ) ;
#61140 = CARTESIAN_POINT ( 'NONE',  ( 0.6178305044545838731, 49.74863466993041072, 9.382169495545420901 ) ) ;
#61141 = CARTESIAN_POINT ( 'NONE',  ( 8.527530157486175710, -21.07440218233254470, -4.923371831947298993 ) ) ;
#61142 = ORIENTED_EDGE ( 'NONE', *, *, #26876, .F. ) ;
#61143 = CARTESIAN_POINT ( 'NONE',  ( 20.05723567505238947, 0.1676365378933190875, 6.413539670616452248 ) ) ;
#61144 = VECTOR ( 'NONE', #88560, 1000.000000000000000 ) ;
#61145 = VERTEX_POINT ( 'NONE', #244 ) ;
#61146 = DIRECTION ( 'NONE',  ( 0.000000000000000000, 0.000000000000000000, 1.000000000000000000 ) ) ;
#61148 = CARTESIAN_POINT ( 'NONE',  ( 17.08211943468705840, 65.13708216824730357, -12.26659068614894466 ) ) ;
#61147 = CARTESIAN_POINT ( 'NONE',  ( 2.917880565312948704, 62.63708216824730357, 12.26659068614894643 ) ) ;
#61150 = CARTESIAN_POINT ( 'NONE',  ( 18.52753015748617571, 63.09226448433412315, 4.923371831947298993 ) ) ;
#61149 = CARTESIAN_POINT ( 'NONE',  ( 0.1532563361054083140, 21.00893115100078745, 1.131784320476157264E-15 ) ) ;
#61151 = CARTESIAN_POINT ( 'NONE',  ( 20.24186590665277308, 50.59014588040356841, -6.114288769123048972 ) ) ;
#61152 = DIRECTION ( 'NONE',  ( 0.000000000000000000, 1.000000000000000000, 0.000000000000000000 ) ) ;
#61153 = CARTESIAN_POINT ( 'NONE',  ( 5.076628168052704559, 10.17559781766745175, -8.527530157486179263 ) ) ;
#61154 = B_SPLINE_CURVE_WITH_KNOTS ( 'NONE', 3,
 ( #40057, #30570, #53572, #1590, #1094, #38585 ),
 .UNSPECIFIED., .F., .F.,
 ( 4, 2, 4 ),
 ( 3.409110551494641945E-05, 0.0004400426677367909084, 0.0008459942299586353364 ),
 .UNSPECIFIED. ) ;
#61155 = CARTESIAN_POINT ( 'NONE',  ( -2.816281873526471635, 3.915301336597087456, -3.434112377981056508 ) ) ;
#61156 = CARTESIAN_POINT ( 'NONE',  ( 6.408140936763243367, 25.79030133659709989, 11.09922568453594494 ) ) ;
#61157 = VERTEX_POINT ( 'NONE', #38226 ) ;
#61158 = CARTESIAN_POINT ( 'NONE',  ( 6.204703633549690345, 35.76208216824729647, -14.16423886937410259 ) ) ;
#61159 = CARTESIAN_POINT ( 'NONE',  ( 24.16423886937410614, 39.30374883491396787, 8.672049930838204340E-16 ) ) ;
#61160 = VERTEX_POINT ( 'NONE', #76217 ) ;
#61161 = STYLED_ITEM ( 'NONE', ( #87944 ), #9364 ) ;
#61162 = CARTESIAN_POINT ( 'NONE',  ( 16.40814093676324603, 52.45696800326375353, -11.09922568453594671 ) ) ;
#61163 = CARTESIAN_POINT ( 'NONE',  ( 2.035157376598824452, 28.68868534415484106, 7.964842623401179544 ) ) ;
#61164 = CARTESIAN_POINT ( 'NONE',  ( 14.92337183194729988, 44.34226448433412315, -8.527530157486177487 ) ) ;
#61165 = CARTESIAN_POINT ( 'NONE',  ( 20.88017736071110164, 25.35535201082150891, 2.915334737309930979 ) ) ;
#61166 = CARTESIAN_POINT ( 'NONE',  ( 10.00000000000000000, 62.87363466993042493, -12.81628187352647608 ) ) ;
#61167 = CARTESIAN_POINT ( 'NONE',  ( 10.58223187591001135, 14.76930270348881002, 10.54772123337538048 ) ) ;
#61168 = CARTESIAN_POINT ( 'NONE',  ( 14.92337183194729633, 52.67559781766745175, 8.527530157486181039 ) ) ;
#61169 = CARTESIAN_POINT ( 'NONE',  ( 5.076628168052704559, 55.17559781766745175, -8.527530157486179263 ) ) ;
#61170 = VECTOR ( 'NONE', #87416, 1000.000000000000000 ) ;
#61171 = EDGE_CURVE ( 'NONE', #74685, #66694, #52148, .T. ) ;
#61173 = ORIENTED_EDGE ( 'NONE', *, *, #64354, .T. ) ;
#61172 = CARTESIAN_POINT ( 'NONE',  ( -3.836325488036278042, 14.63595249122790598, 14.50112432709420318 ) ) ;
#61174 = AXIS2_PLACEMENT_3D ( 'NONE', #72714, #59197, #36212 ) ;
#61175 = CARTESIAN_POINT ( 'NONE',  ( -14.42956166533734041, -3.121739927105722716E-15, -2.386684097925192205 ) ) ;
#61176 = CARTESIAN_POINT ( 'NONE',  ( 18.52753015748618282, 3.925597817667451306, -4.923371831947291888 ) ) ;
#61177 = LINE ( 'NONE', #23700, #2112 ) ;
#61178 = ORIENTED_EDGE ( 'NONE', *, *, #8490, .F. ) ;
#61179 = CARTESIAN_POINT ( 'NONE',  ( 14.92337183194729988, 29.34226448433411960, -8.527530157486177487 ) ) ;
#61180 = DIRECTION ( 'NONE',  ( -0.5547001962252291474, -0.8320502943378437211, -0.000000000000000000 ) ) ;
#61181 = CARTESIAN_POINT ( 'NONE',  ( -2.816281873526473856, 39.12363466993041783, 9.499525473075851096E-16 ) ) ;
#61182 = CARTESIAN_POINT ( 'NONE',  ( 0.000000000000000000, 0.5000000000000004441, 0.000000000000000000 ) ) ;
#61183 = LINE ( 'NONE', #5369, #2791 ) ;
#61184 = EDGE_LOOP ( 'NONE', ( #94598, #25406, #95989, #13811, #77249, #24347 ) ) ;
#61185 = DIRECTION ( 'NONE',  ( -0.02617694830786282401, 0.000000000000000000, -0.9996573249755575929 ) ) ;
#61186 = FACE_OUTER_BOUND ( 'NONE', #80680, .T. ) ;
#61187 = CARTESIAN_POINT ( 'NONE',  ( 17.20831665107776587, 49.13393115100078745, -7.208316651077762316 ) ) ;
#61188 = CARTESIAN_POINT ( 'NONE',  ( 6.204703633549690345, 37.84541550158063927, 14.16423886937410082 ) ) ;
#61189 = CARTESIAN_POINT ( 'NONE',  ( 19.84674366389459621, 63.50893115100078745, 7.409399052514197653E-17 ) ) ;
#61190 = DIRECTION ( 'NONE',  ( -0.000000000000000000, 1.000000000000000000, 0.000000000000000000 ) ) ;
#61191 = CARTESIAN_POINT ( 'NONE',  ( 1.472469842513823179, 1.425597817667451528, 4.923371831947296329 ) ) ;
#61192 = CARTESIAN_POINT ( 'NONE',  ( -0.3689425029237881626, 2.428748834913967869, 10.36894250292379027 ) ) ;
#61193 = CARTESIAN_POINT ( 'NONE',  ( 0.1532563361054083140, 51.00893115100078745, 1.131784320476157264E-15 ) ) ;
#61194 = CARTESIAN_POINT ( 'NONE',  ( 19.42250999205614548, 55.98035201082150536, -5.440088680355545492 ) ) ;
#61195 = CARTESIAN_POINT ( 'NONE',  ( 12.63842701281683034, 47.46726448433412315, 9.846743663894596210 ) ) ;
#61196 = EDGE_LOOP ( 'NONE', ( #15067, #87812, #59407, #73918 ) ) ;
#61197 = EDGE_CURVE ( 'NONE', #69916, #92653, #9040, .T. ) ;
#61198 = CARTESIAN_POINT ( 'NONE',  ( 7.084665262690076126, 62.02201867748816966, -10.88017736071110164 ) ) ;
#61199 = AXIS2_PLACEMENT_3D ( 'NONE', #61656, #16184, #52694 ) ;
#61200 = ORIENTED_EDGE ( 'NONE', *, *, #73948, .T. ) ;
#61201 = EDGE_CURVE ( 'NONE', #50558, #10425, #64903, .T. ) ;
#61202 = DIRECTION ( 'NONE',  ( 0.9998643952135762847, -0.01646788341559294114, 0.000000000000000000 ) ) ;
#61203 = CARTESIAN_POINT ( 'NONE',  ( 15.44008868035555793, 31.39701867748817676, -9.422509992056140149 ) ) ;
#61205 = CARTESIAN_POINT ( 'NONE',  ( 17.96484262340118221, 61.18868534415482685, -7.964842623401177768 ) ) ;
#61204 = CARTESIAN_POINT ( 'NONE',  ( 12.63842701281683922, 64.55059781766745175, -9.846743663894590881 ) ) ;
#61206 = CARTESIAN_POINT ( 'NONE',  ( -0.3289641300567998083, 48.07879003517447103, 5.963430220938281678 ) ) ;
#61207 = VECTOR ( 'NONE', #5033, 1000.000000000000114 ) ;
#61208 = CARTESIAN_POINT ( 'NONE',  ( -7.640985187756333730, 0.04962896822202291641, 12.62032702733647049 ) ) ;
#61209 = CARTESIAN_POINT ( 'NONE',  ( -11.81378540890942119, 15.00000000000000000, 7.968498874458034287 ) ) ;
#61211 = CARTESIAN_POINT ( 'NONE',  ( -5.056330833731569108, 4.047076681631624764E-16, -13.58983143750706724 ) ) ;
#61210 = CARTESIAN_POINT ( 'NONE',  ( 12.91533473730992121, 39.52201867748817676, 10.88017736071110164 ) ) ;
#61212 = CARTESIAN_POINT ( 'NONE',  ( 7.361572987183170547, 12.05059781766744997, 9.846743663894590881 ) ) ;
#61213 = CARTESIAN_POINT ( 'NONE',  ( 17.20831665107776587, 42.88393115100077324, 7.208316651077764980 ) ) ;
#61214 = DIRECTION ( 'NONE',  ( 0.000000000000000000, 0.000000000000000000, 1.000000000000000000 ) ) ;
#61215 = PRESENTATION_LAYER_ASSIGNMENT (  '', '', ( #46792 ) ) ;
#61216 = CARTESIAN_POINT ( 'NONE',  ( 3.795296366450314540, 13.26208216824729647, 14.16423886937410082 ) ) ;
#61217 = CARTESIAN_POINT ( 'NONE',  ( 17.20831665107776587, 59.13393115100078745, -7.208316651077762316 ) ) ;
#61218 = CARTESIAN_POINT ( 'NONE',  ( 2.917880565312950480, 65.97041550158063217, -12.26659068614894821 ) ) ;
#61219 = FACE_BOUND ( 'NONE', #25652, .T. ) ;
#61220 = CARTESIAN_POINT ( 'NONE',  ( -0.3689425029237898834, 16.17874883491396076, -10.36894250292378850 ) ) ;
#61221 = CARTESIAN_POINT ( 'NONE',  ( -4.164238869374099039, 56.80374883491397497, 8.674139862899312516E-16 ) ) ;
#61222 = CARTESIAN_POINT ( 'NONE',  ( 17.20831665107776587, 12.88393115100078390, 7.208316651077764980 ) ) ;
#61223 = VERTEX_POINT ( 'NONE', #16204 ) ;
#61224 = CARTESIAN_POINT ( 'NONE',  ( 18.52753015748618282, 23.92559781766745530, -4.923371831947291888 ) ) ;
#61225 = CARTESIAN_POINT ( 'NONE',  ( 17.96484262340118221, 24.93868534415484461, 7.964842623401181321 ) ) ;
#61226 = CARTESIAN_POINT ( 'NONE',  ( -2.816281873526473856, -0.8763653300695799508, 9.499525473075851096E-16 ) ) ;
#61228 =( NAMED_UNIT ( * ) PLANE_ANGLE_UNIT ( ) SI_UNIT ( $, .RADIAN. ) );
#61227 = CARTESIAN_POINT ( 'NONE',  ( 6.204703633549690345, 2.845415501580634388, 14.16423886937410082 ) ) ;
#61229 = FACE_BOUND ( 'NONE', #23755, .T. ) ;
#61230 = CARTESIAN_POINT ( 'NONE',  ( 1.472469842513823179, 11.42559781766745175, 4.923371831947296329 ) ) ;
#61231 = CARTESIAN_POINT ( 'NONE',  ( 13.43411237798106583, 37.66530133659708923, -12.81628187352647252 ) ) ;
#61232 = CARTESIAN_POINT ( 'NONE',  ( 17.20831665107776587, 44.13393115100078745, -7.208316651077762316 ) ) ;
#61233 = ORIENTED_EDGE ( 'NONE', *, *, #73229, .F. ) ;
#61234 = CARTESIAN_POINT ( 'NONE',  ( 2.791683348922237240, 20.38393115100078745, -7.208316651077763204 ) ) ;
#61235 = CARTESIAN_POINT ( 'NONE',  ( 10.95672020365094923, -56.81584260457628233, -4.000000000000000000 ) ) ;
#61236 = CARTESIAN_POINT ( 'NONE',  ( 24.16423886937410614, 49.51208216824730357, -3.795296366450302550 ) ) ;
#61237 = CARTESIAN_POINT ( 'NONE',  ( 0.5774900079438607392, 58.48035201082151247, 5.440088680355550821 ) ) ;
#61238 = CARTESIAN_POINT ( 'NONE',  ( 0.1916775849787264729, 32.25868815902069997, -6.499999999999991118 ) ) ;
#61239 = DIRECTION ( 'NONE',  ( 0.000000000000000000, 1.000000000000000000, 0.000000000000000000 ) ) ;
#61240 = CARTESIAN_POINT ( 'NONE',  ( 12.63842701281683922, 39.55059781766744464, -9.846743663894590881 ) ) ;
#61241 = CARTESIAN_POINT ( 'NONE',  ( 4.559911319644449179, 8.897018677488171434, 9.422509992056141925 ) ) ;
#61242 = CARTESIAN_POINT ( 'NONE',  ( 0.1532563361054082862, 46.21726448433411605, 2.638427012816831674 ) ) ;
#61243 = CARTESIAN_POINT ( 'NONE',  ( 12.63842701281683922, 54.55059781766745175, -9.846743663894590881 ) ) ;
#61244 = CIRCLE ( 'NONE', #86800, 0.2500000000000004441 ) ;
#61245 = ADVANCED_FACE ( 'NONE', ( #8692 ), #92049, .T. ) ;
#61246 = CARTESIAN_POINT ( 'NONE',  ( 10.00000000000000178, 44.31368534415484106, 10.88017736071110342 ) ) ;
#61247 = EDGE_LOOP ( 'NONE', ( #28199, #61992, #12212, #91979, #56629, #92374, #71614, #45298, #3966, #91538, #34795, #13852, #93153, #82532, #71163, #93482 ) ) ;
#61248 = ORIENTED_EDGE ( 'NONE', *, *, #65480, .F. ) ;
#61249 = LINE ( 'NONE', #93711, #13377 ) ;
#61250 = FACE_OUTER_BOUND ( 'NONE', #49502, .T. ) ;
#61251 = CARTESIAN_POINT ( 'NONE',  ( 0.1532563361054083140, 6.008931151000784787, 1.131784320476157264E-15 ) ) ;
#61252 = CARTESIAN_POINT ( 'NONE',  ( 21.09922568453595559, 57.04030133659708923, -6.408140936763230044 ) ) ;
#61254 = CARTESIAN_POINT ( 'NONE',  ( 1.472469842513823179, 55.59226448433412315, -4.923371831947296329 ) ) ;
#61253 = CARTESIAN_POINT ( 'NONE',  ( 12.91533473730993009, 6.605352010821504471, -10.88017736071109987 ) ) ;
#61255 = DIRECTION ( 'NONE',  ( -1.000000000000000000, -0.000000000000000000, -0.000000000000000000 ) ) ;
#61256 = CARTESIAN_POINT ( 'NONE',  ( 2.917880565312950480, 30.97041550158063572, -12.26659068614894821 ) ) ;
#61257 = CARTESIAN_POINT ( 'NONE',  ( -4.164238869374098151, 61.59541550158063217, -3.795296366450310543 ) ) ;
#61258 = CARTESIAN_POINT ( 'NONE',  ( 17.20831665107776587, 52.88393115100078035, 7.208316651077764980 ) ) ;
#61259 = CARTESIAN_POINT ( 'NONE',  ( 20.88017736071110519, 45.56368534415484106, 2.639326808657452039E-16 ) ) ;
#61260 = CARTESIAN_POINT ( 'NONE',  ( -0.8801773607111008646, 68.27201867748817676, 2.915334737309923430 ) ) ;
#61261 = FILL_AREA_STYLE_COLOUR ( '', #74902 ) ;
#61262 = ORIENTED_EDGE ( 'NONE', *, *, #77311, .F. ) ;
#61263 = CARTESIAN_POINT ( 'NONE',  ( 6.565887622018943937, 63.08196800326376064, -12.81628187352647608 ) ) ;
#61264 = ORIENTED_EDGE ( 'NONE', *, *, #30815, .T. ) ;
#61265 = CARTESIAN_POINT ( 'NONE',  ( 0.1532563361054083140, 11.00893115100078568, 1.131784320476157264E-15 ) ) ;
#61266 = ORIENTED_EDGE ( 'NONE', *, *, #61523, .F. ) ;
#61267 = CARTESIAN_POINT ( 'NONE',  ( 20.36894250292379738, 14.92874883491396432, -10.36894250292379027 ) ) ;
#61268 = CARTESIAN_POINT ( 'NONE',  ( 14.92337183194729633, 22.67559781766745175, 8.527530157486181039 ) ) ;
#61269 = CARTESIAN_POINT ( 'NONE',  ( 20.88017736071110875, 35.77201867748816966, -2.915334737309920765 ) ) ;
#61270 = CARTESIAN_POINT ( 'NONE',  ( 3.866399090317279796, 14.95077488074853456, -14.23717170745771909 ) ) ;
#61271 = ORIENTED_EDGE ( 'NONE', *, *, #20474, .F. ) ;
#61272 = CARTESIAN_POINT ( 'NONE',  ( 20.88017736071110164, 30.35535201082151247, 2.915334737309930979 ) ) ;
#61273 = AXIS2_PLACEMENT_3D ( 'NONE', #66155, #59150, #43170 ) ;
#61274 = ORIENTED_EDGE ( 'NONE', *, *, #69435, .T. ) ;
#61275 = CARTESIAN_POINT ( 'NONE',  ( -0.8801773607111008646, 33.27201867748817676, 2.915334737309923430 ) ) ;
#61276 = CYLINDRICAL_SURFACE ( 'NONE', #98422, 0.5000000000000004441 ) ;
#61277 = ORIENTED_EDGE ( 'NONE', *, *, #50275, .F. ) ;
#61278 = SURFACE_STYLE_USAGE ( .BOTH. , #30773 ) ;
#61279 = ORIENTED_EDGE ( 'NONE', *, *, #19291, .F. ) ;
#61280 = CARTESIAN_POINT ( 'NONE',  ( 19.38216949554541202, 20.99863466993042138, 9.382169495545424454 ) ) ;
#61281 = CARTESIAN_POINT ( 'NONE',  ( 19.84674366389459266, 13.30059781766745353, 2.638427012816836559 ) ) ;
#61282 = CARTESIAN_POINT ( 'NONE',  ( 14.11917416961165195, 0.2306972965111870610, 4.887430353539040873 ) ) ;
#61283 = CARTESIAN_POINT ( 'NONE',  ( 0.2751277870542967463, 0.000000000000000000, 6.500000000000000888 ) ) ;
#61284 = CARTESIAN_POINT ( 'NONE',  ( 10.00000000000000178, 22.25893115100078745, 9.846743663894594434 ) ) ;
#61285 = CARTESIAN_POINT ( 'NONE',  ( 7.084665262690076126, 27.02201867748817676, -10.88017736071110164 ) ) ;
#61286 = EDGE_CURVE ( 'NONE', #7312, #22776, #92199, .T. ) ;
#61287 = ORIENTED_EDGE ( 'NONE', *, *, #7812, .T. ) ;
#61288 = VERTEX_POINT ( 'NONE', #8216 ) ;
#61289 = CARTESIAN_POINT ( 'NONE',  ( 22.81628187352648496, 61.83196800326376774, -3.434112377981050290 ) ) ;
#61290 = CARTESIAN_POINT ( 'NONE',  ( 20.88017736071110875, 60.77201867748817676, -2.915334737309920765 ) ) ;
#61291 = CARTESIAN_POINT ( 'NONE',  ( -0.2418659066527775181, 23.09014588040356841, 6.114288769123032985 ) ) ;
#61292 = CARTESIAN_POINT ( 'NONE',  ( 10.00000000000000178, 55.37363466993042493, 12.81628187352647608 ) ) ;
#61293 = CARTESIAN_POINT ( 'NONE',  ( 20.88017736071110164, 65.35535201082150536, 2.915334737309930979 ) ) ;
#61294 = CARTESIAN_POINT ( 'NONE',  ( 6.565887622018943937, 0.1653013365970866511, 12.81628187352647430 ) ) ;
#61295 = FACE_OUTER_BOUND ( 'NONE', #23168, .T. ) ;
#61296 = CARTESIAN_POINT ( 'NONE',  ( 14.92337183194729633, 27.67559781766745530, 8.527530157486181039 ) ) ;
#61297 = CARTESIAN_POINT ( 'NONE',  ( 10.00000000000000000, 47.87363466993042493, -12.81628187352647608 ) ) ;
#61298 = CARTESIAN_POINT ( 'NONE',  ( 0.000000000000000000, 77.77738620402351444, 8.380889435745553229 ) ) ;
#61299 = CARTESIAN_POINT ( 'NONE',  ( 18.52753015748618282, 23.92559781766745530, -4.923371831947291888 ) ) ;
#61300 = CARTESIAN_POINT ( 'NONE',  ( -2.816281873526471635, 18.91530133659708213, -3.434112377981056508 ) ) ;
#61301 = CYLINDRICAL_SURFACE ( 'NONE', #40228, 15.00000000000000000 ) ;
#61302 = CARTESIAN_POINT ( 'NONE',  ( 20.88017736071110164, 30.35535201082151247, 2.915334737309930979 ) ) ;
#61303 = CARTESIAN_POINT ( 'NONE',  ( 0.6178305044545838731, -0.2513653300695798953, 9.382169495545420901 ) ) ;
#61304 = FACE_OUTER_BOUND ( 'NONE', #36097, .T. ) ;
#61305 = CARTESIAN_POINT ( 'NONE',  ( 1.472469842513823179, 16.42559781766745175, 4.923371831947296329 ) ) ;
#61306 = CARTESIAN_POINT ( 'NONE',  ( 2.791683348922240793, 11.63393115100078568, 7.208316651077764092 ) ) ;
#61307 = CARTESIAN_POINT ( 'NONE',  ( 2.035157376598824452, 13.68868534415483751, 7.964842623401179544 ) ) ;
#61308 = CARTESIAN_POINT ( 'NONE',  ( 22.81628187352648496, 11.83196800326375531, -3.434112377981050290 ) ) ;
#61309 = SHAPE_REPRESENTATION ( 'MAS-685', ( #64670, #40794, #39160, #87031, #72671, #7253 ), #95016 ) ;
#61310 = CARTESIAN_POINT ( 'NONE',  ( 7.361572987183169658, 59.96726448433410894, -9.846743663894592657 ) ) ;
#61311 = EDGE_CURVE ( 'NONE', #83674, #10324, #44719, .T. ) ;
#61312 = CARTESIAN_POINT ( 'NONE',  ( 6.574584770534515066, -50.88238473842280030, -2.499999999999998224 ) ) ;
#61313 = CARTESIAN_POINT ( 'NONE',  ( 2.035157376598824452, 8.688685344154839285, 7.964842623401179544 ) ) ;
#61314 = CARTESIAN_POINT ( 'NONE',  ( 19.84674366389459266, 38.71726448433412315, -2.638427012816827677 ) ) ;
#61315 = ORIENTED_EDGE ( 'NONE', *, *, #29174, .F. ) ;
#61316 = CARTESIAN_POINT ( 'NONE',  ( 6.034042420216372271, -36.05779855192275107, 2.750000000000000000 ) ) ;
#61317 = EDGE_CURVE ( 'NONE', #79877, #91116, #60129, .T. ) ;
#61318 = CARTESIAN_POINT ( 'NONE',  ( 10.00000000000000000, 16.81368534415483751, -10.88017736071110342 ) ) ;
#61319 = CARTESIAN_POINT ( 'NONE',  ( -45.94000000000000483, 93.00000000000000000, 9.000000000000000000 ) ) ;
#61320 = CARTESIAN_POINT ( 'NONE',  ( 10.00000000000000178, 34.31368534415484106, 10.88017736071110342 ) ) ;
#61322 = CARTESIAN_POINT ( 'NONE',  ( 15.00000000000000000, 77.07179676972447169, -6.500000000000000888 ) ) ;
#61321 = CARTESIAN_POINT ( 'NONE',  ( 6.204703633549690345, 65.76208216824731778, -14.16423886937410259 ) ) ;
#61323 = CARTESIAN_POINT ( 'NONE',  ( 0.1532563361054082862, 6.217264484334118713, 2.638427012816831674 ) ) ;
#61324 = B_SPLINE_CURVE_WITH_KNOTS ( 'NONE', 3,
 ( #71876, #55904, #9915, #41895, #63388, #40904 ),
 .UNSPECIFIED., .F., .F.,
 ( 4, 2, 4 ),
 ( 0.000000000000000000, 0.0002565770811490922947, 0.0005131541622981845895 ),
 .UNSPECIFIED. ) ;
#61325 = CARTESIAN_POINT ( 'NONE',  ( 19.84674366389459266, 18.71726448433411960, -2.638427012816827677 ) ) ;
#61326 = CARTESIAN_POINT ( 'NONE',  ( -1.099225684535947600, 8.706968003263753531, -6.408140936763238038 ) ) ;
#61327 = CARTESIAN_POINT ( 'NONE',  ( -46.94000000000001194, 103.2282880252848685, 5.913372230041396449 ) ) ;
#61328 = CARTESIAN_POINT ( 'NONE',  ( -11.81378540890942119, -0.03417435944610275333, 7.968498874458034287 ) ) ;
#61329 = CARTESIAN_POINT ( 'NONE',  ( -1.099225684535947600, -0.4596986634029132657, 6.408140936763237150 ) ) ;
#61330 = LINE ( 'NONE', #22864, #66705 ) ;
#61331 = CARTESIAN_POINT ( 'NONE',  ( -0.3689425029237881626, 17.42874883491397142, 10.36894250292379027 ) ) ;
#61332 = B_SPLINE_CURVE_WITH_KNOTS ( 'NONE', 3,
 ( #47970, #63473, #2018, #9491, #46990, #55985, #78479, #48469, #78967, #3478 ),
 .UNSPECIFIED., .F., .F.,
 ( 4, 3, 3, 4 ),
 ( 1.648129954184481677E-17, 0.0006253016069560848747, 0.001250604074564934734, 0.002501455912506530058 ),
 .UNSPECIFIED. ) ;
#61333 = CARTESIAN_POINT ( 'NONE',  ( 18.52753015748617571, 43.09226448433412315, 4.923371831947298993 ) ) ;
#61334 =( LENGTH_UNIT ( ) NAMED_UNIT ( * ) SI_UNIT ( .MILLI., .METRE. ) );
#61335 = ORIENTED_EDGE ( 'NONE', *, *, #43887, .F. ) ;
#61336 = VECTOR ( 'NONE', #19496, 1000.000000000000114 ) ;
#61337 = CARTESIAN_POINT ( 'NONE',  ( 20.36894250292379738, 59.92874883491397497, -10.36894250292379027 ) ) ;
#61338 = CARTESIAN_POINT ( 'NONE',  ( 18.52753015748617571, 13.09226448433411960, 4.923371831947298993 ) ) ;
#61340 = CARTESIAN_POINT ( 'NONE',  ( 11.24699797944280100, 54.09857164847241506, 2.899999999999999467 ) ) ;
#61339 = CARTESIAN_POINT ( 'NONE',  ( 14.88232117145535760, 14.49999999999999112, 1.875237731503272887 ) ) ;
#61341 = CARTESIAN_POINT ( 'NONE',  ( -0.8801773607111009756, 43.06368534415484106, 1.068504757029289695E-15 ) ) ;
#61342 = CARTESIAN_POINT ( 'NONE',  ( 6.565887622018943937, 45.16530133659708923, 12.81628187352647430 ) ) ;
#61343 = CARTESIAN_POINT ( 'NONE',  ( 17.96484262340118221, 11.18868534415483929, -7.964842623401177768 ) ) ;
#61344 = CARTESIAN_POINT ( 'NONE',  ( 21.09922568453595559, 47.04030133659708923, -6.408140936763230044 ) ) ;
#61345 = CARTESIAN_POINT ( 'NONE',  ( 6.565887622018943937, 0.1653013365970866511, 12.81628187352647430 ) ) ;
#61346 =( LENGTH_UNIT ( ) NAMED_UNIT ( * ) SI_UNIT ( .MILLI., .METRE. ) );
#61347 = ORIENTED_EDGE ( 'NONE', *, *, #34080, .T. ) ;
#61348 = AXIS2_PLACEMENT_3D ( 'NONE', #18670, #94160, #77681 ) ;
#61349 = CARTESIAN_POINT ( 'NONE',  ( -8.218815441056078086, -9.362071622917410352, -4.000000000000000888 ) ) ;
#61350 = CARTESIAN_POINT ( 'NONE',  ( -0.3689425029237898834, 46.17874883491397497, -10.36894250292378850 ) ) ;
#61351 = CARTESIAN_POINT ( 'NONE',  ( 24.16423886937410614, 14.30374883491396787, 8.672049930838204340E-16 ) ) ;
#61352 = CARTESIAN_POINT ( 'NONE',  ( 2.035157376598824452, 18.68868534415484106, 7.964842623401179544 ) ) ;
#61353 = CARTESIAN_POINT ( 'NONE',  ( 19.42250999205614548, 30.98035201082150536, -5.440088680355545492 ) ) ;
#61354 = CARTESIAN_POINT ( 'NONE',  ( 9.399392868737814766, 15.00000000000000000, -11.04089732309474314 ) ) ;
#61355 = CARTESIAN_POINT ( 'NONE',  ( 0.000000000000000000, 0.000000000000000000, 0.000000000000000000 ) ) ;
#61356 = CARTESIAN_POINT ( 'NONE',  ( 20.88017736071110164, 60.35535201082151957, 2.915334737309930979 ) ) ;
#61357 = CARTESIAN_POINT ( 'NONE',  ( 7.084665262690076126, 62.02201867748816966, -10.88017736071110164 ) ) ;
#61358 = CARTESIAN_POINT ( 'NONE',  ( 6.565887622018943937, 28.08196800326375353, -12.81628187352647608 ) ) ;
#61359 = DIRECTION ( 'NONE',  ( -1.000000000000000000, 0.000000000000000000, 0.000000000000000000 ) ) ;
#61360 = CARTESIAN_POINT ( 'NONE',  ( -11.92686044187656336, 2.870456701841150871, 3.195792623639540864 ) ) ;
#61361 = CARTESIAN_POINT ( 'NONE',  ( 19.84674366389459621, 33.50893115100078745, 7.409399052514197653E-17 ) ) ;
#61362 = EDGE_CURVE ( 'NONE', #97076, #47923, #37752, .T. ) ;
#61363 = CARTESIAN_POINT ( 'NONE',  ( 20.88017736071110875, 10.77201867748817143, -2.915334737309920765 ) ) ;
#61364 = CARTESIAN_POINT ( 'NONE',  ( 16.40814093676324603, 22.45696800326375353, -11.09922568453594671 ) ) ;
#61365 = CARTESIAN_POINT ( 'NONE',  ( 7.361572987183170547, 12.05059781766744997, 9.846743663894590881 ) ) ;
#61366 = CARTESIAN_POINT ( 'NONE',  ( -0.8801773607111008646, 8.272018677488171434, 2.915334737309923430 ) ) ;
#61367 = CARTESIAN_POINT ( 'NONE',  ( 7.361572987183170547, 32.05059781766745175, 9.846743663894590881 ) ) ;
#61368 = CARTESIAN_POINT ( 'NONE',  ( 19.38216949554541557, 57.24863466993042493, -9.382169495545420901 ) ) ;
#61369 = CARTESIAN_POINT ( 'NONE',  ( 19.84674366389459621, 38.50893115100078745, 7.409399052514197653E-17 ) ) ;
#61370 = CARTESIAN_POINT ( 'NONE',  ( 22.26659068614894466, 18.88708216824730002, 7.082119434687054849 ) ) ;
#61371 = CARTESIAN_POINT ( 'NONE',  ( 17.96484262340118221, 34.93868534415482685, 7.964842623401181321 ) ) ;
#61372 = CARTESIAN_POINT ( 'NONE',  ( -0.8801773607110991993, 7.855352010821504471, -2.915334737309923874 ) ) ;
#61373 = EDGE_CURVE ( 'NONE', #17685, #93052, #45217, .T. ) ;
#61374 = CARTESIAN_POINT ( 'NONE',  ( 2.035157376598824452, 28.68868534415484106, 7.964842623401179544 ) ) ;
#61375 = CARTESIAN_POINT ( 'NONE',  ( 15.44008868035555260, 29.73035201082150891, 9.422509992056143702 ) ) ;
#61376 = VERTEX_POINT ( 'NONE', #735 ) ;
#61377 = CARTESIAN_POINT ( 'NONE',  ( 17.96484262340118221, 46.18868534415484106, -7.964842623401177768 ) ) ;
#61378 = VECTOR ( 'NONE', #8745, 1000.000000000000227 ) ;
#61379 = CARTESIAN_POINT ( 'NONE',  ( 3.591859063236761518, 64.95696800326376774, 11.09922568453594849 ) ) ;
#61380 = CARTESIAN_POINT ( 'NONE',  ( 15.44008868035555260, 44.73035201082151247, 9.422509992056143702 ) ) ;
#61381 = CARTESIAN_POINT ( 'NONE',  ( 15.44008868035555793, 46.39701867748817676, -9.422509992056140149 ) ) ;
#61382 = ORIENTED_EDGE ( 'NONE', *, *, #59709, .F. ) ;
#61383 = CARTESIAN_POINT ( 'NONE',  ( 20.88017736071110519, 50.56368534415484106, 2.639326808657452039E-16 ) ) ;
#61384 = DIRECTION ( 'NONE',  ( -6.938893903907222067E-15, 1.000000000000000000, 0.000000000000000000 ) ) ;
#61385 = CARTESIAN_POINT ( 'NONE',  ( 4.180366052176762715, -2.683400376901622685E-15, 14.01545757926331071 ) ) ;
#61386 = CARTESIAN_POINT ( 'NONE',  ( 6.204703633549690345, 65.76208216824731778, -14.16423886937410259 ) ) ;
#61387 = CARTESIAN_POINT ( 'NONE',  ( 5.076628168052703671, 1.842264484334118047, 8.527530157486179263 ) ) ;
#61388 = CARTESIAN_POINT ( 'NONE',  ( -13.82192141328815715, 15.00000000000000000, 4.382292601468586568 ) ) ;
#61389 = CARTESIAN_POINT ( 'NONE',  ( -14.56311970191030625, 14.76984991344722253, 3.337330457605781397 ) ) ;
#61390 = CARTESIAN_POINT ( 'NONE',  ( 12.63842701281683922, 39.55059781766744464, -9.846743663894590881 ) ) ;
#61391 = ORIENTED_EDGE ( 'NONE', *, *, #3243, .T. ) ;
#61392 = CARTESIAN_POINT ( 'NONE',  ( 2.791683348922237240, 30.38393115100078390, -7.208316651077763204 ) ) ;
#61393 = CARTESIAN_POINT ( 'NONE',  ( 15.44008868035555793, 46.39701867748817676, -9.422509992056140149 ) ) ;
#61394 = CARTESIAN_POINT ( 'NONE',  ( 7.361572987183169658, 39.96726448433411605, -9.846743663894592657 ) ) ;
#61395 = CARTESIAN_POINT ( 'NONE',  ( -2.816281873526471635, 23.91530133659708568, -3.434112377981056508 ) ) ;
#61396 = CARTESIAN_POINT ( 'NONE',  ( 19.72487221294571214, 2.802231764288312998, -6.500000000000001776 ) ) ;
#61398 = FILL_AREA_STYLE ('',( #45417 ) ) ;
#61397 = CARTESIAN_POINT ( 'NONE',  ( -0.8801773607110991993, 47.85535201082150536, -2.915334737309923874 ) ) ;
#61399 = CARTESIAN_POINT ( 'NONE',  ( 24.16423886937409904, 54.09541550158063217, 3.795296366450317205 ) ) ;
#61400 = EDGE_CURVE ( 'NONE', #59039, #71742, #61698, .T. ) ;
#61401 = MECHANICAL_DESIGN_GEOMETRIC_PRESENTATION_REPRESENTATION (  '', ( #48622 ), #10385 ) ;
#61402 = CARTESIAN_POINT ( 'NONE',  ( 16.40814093676323893, 20.79030133659708923, 11.09922568453595026 ) ) ;
#61403 = CARTESIAN_POINT ( 'NONE',  ( 18.17884179759847996, 23.66688879859523453, -6.499999999999984901 ) ) ;
#61404 = EDGE_CURVE ( 'NONE', #18352, #51389, #33598, .T. ) ;
#61405 = EDGE_LOOP ( 'NONE', ( #14773, #3135, #47753, #89561 ) ) ;
#61406 = STYLED_ITEM ( 'NONE', ( #65487 ), #90027 ) ;
#61407 = CARTESIAN_POINT ( 'NONE',  ( 19.38216949554541202, 15.99863466993042138, 9.382169495545424454 ) ) ;
#61408 = CARTESIAN_POINT ( 'NONE',  ( 19.42250999205614548, 20.98035201082150891, -5.440088680355545492 ) ) ;
#61409 = CARTESIAN_POINT ( 'NONE',  ( 19.42250999205614548, 65.98035201082151957, -5.440088680355545492 ) ) ;
#61410 = AXIS2_PLACEMENT_3D ( 'NONE', #87044, #8590, #25576 ) ;
#61411 = ORIENTED_EDGE ( 'NONE', *, *, #22160, .T. ) ;
#61412 = CARTESIAN_POINT ( 'NONE',  ( 10.00000000000000000, 66.81368534415484817, -10.88017736071110342 ) ) ;
#61413 = VECTOR ( 'NONE', #34742, 1000.000000000000000 ) ;
#61414 = CARTESIAN_POINT ( 'NONE',  ( 5.076628168052703671, 46.84226448433412315, 8.527530157486179263 ) ) ;
#61415 = EDGE_CURVE ( 'NONE', #30159, #31207, #47956, .T. ) ;
#61416 = CARTESIAN_POINT ( 'NONE',  ( 12.63842701281683034, 32.46726448433412315, 9.846743663894596210 ) ) ;
#61417 = CARTESIAN_POINT ( 'NONE',  ( 17.20831665107776587, 32.88393115100078745, 7.208316651077764980 ) ) ;
#61418 = CARTESIAN_POINT ( 'NONE',  ( 22.81628187352647785, 36.41530133659707502, 3.434112377981063169 ) ) ;
#61420 = CYLINDRICAL_SURFACE ( 'NONE', #35543, 2.000000000000001776 ) ;
#61419 = CARTESIAN_POINT ( 'NONE',  ( 17.20831665107776587, 14.13393115100078568, -7.208316651077762316 ) ) ;
#61421 = CARTESIAN_POINT ( 'NONE',  ( 8.813102413620015341, -0.03417435944610275333, 13.34940531570970457 ) ) ;
#61423 = EDGE_LOOP ( 'NONE', ( #20696, #65164, #89723, #23900 ) ) ;
#61422 = CARTESIAN_POINT ( 'NONE',  ( 1.472469842513823179, 51.42559781766745886, 4.923371831947296329 ) ) ;
#61424 = CARTESIAN_POINT ( 'NONE',  ( 13.43411237798106583, 62.66530133659708923, -12.81628187352647252 ) ) ;
#61425 = CARTESIAN_POINT ( 'NONE',  ( 17.39651004071842166, 32.93575266056827644, 6.499999999999998224 ) ) ;
#61426 = CARTESIAN_POINT ( 'NONE',  ( 22.81628187352647785, 11.62363466993042138, 6.195893100308588602E-16 ) ) ;
#61427 = CIRCLE ( 'NONE', #16775, 14.49999999999999822 ) ;
#61428 = CARTESIAN_POINT ( 'NONE',  ( 2.035157376598822676, 52.43868534415483396, -7.964842623401177768 ) ) ;
#61429 = CARTESIAN_POINT ( 'NONE',  ( 17.08211943468705840, 35.13708216824730357, -12.26659068614894466 ) ) ;
#61430 = CARTESIAN_POINT ( 'NONE',  ( -39.69000000000001194, 92.00000000000000000, -9.500000000000000000 ) ) ;
#61431 = CARTESIAN_POINT ( 'NONE',  ( -46.82017113615791004, 100.6079546444643427, 9.324761308090124601 ) ) ;
#61432 = EDGE_CURVE ( 'NONE', #49375, #6101, #83744, .T. ) ;
#61433 = CARTESIAN_POINT ( 'NONE',  ( 24.16423886937410614, 24.30374883491396787, 8.672049930838204340E-16 ) ) ;
#61434 = CARTESIAN_POINT ( 'NONE',  ( 6.204703633549690345, 65.76208216824731778, -14.16423886937410259 ) ) ;
#61435 = CARTESIAN_POINT ( 'NONE',  ( 10.00000000000000178, 8.053748834913967869, 14.16423886937410082 ) ) ;
#61437 = CARTESIAN_POINT ( 'NONE',  ( -9.159723438033054776, 15.00000000000000000, -10.91613331444555079 ) ) ;
#61436 = CARTESIAN_POINT ( 'NONE',  ( 22.26659068614895176, 24.72041550158063572, -7.082119434687042414 ) ) ;
#61438 = CARTESIAN_POINT ( 'NONE',  ( -0.1038446121089043744, 29.24302437010794620, -6.337995344473781323 ) ) ;
#61440 = CARTESIAN_POINT ( 'NONE',  ( 0.1532563361054100626, 45.80059781766745886, -2.638427012816831230 ) ) ;
#61439 = DIRECTION ( 'NONE',  ( -0.000000000000000000, -0.000000000000000000, -1.000000000000000000 ) ) ;
#61441 = VERTEX_POINT ( 'NONE', #84698 ) ;
#61442 = CARTESIAN_POINT ( 'NONE',  ( 10.00000000000000178, 24.31368534415484106, 10.88017736071110342 ) ) ;
#61443 = CARTESIAN_POINT ( 'NONE',  ( 2.602085213965210642E-15, 78.91966277462714174, -9.500000000000000000 ) ) ;
#61444 = CARTESIAN_POINT ( 'NONE',  ( 19.84674366389459266, 63.30059781766745886, 2.638427012816836559 ) ) ;
#61445 = AXIS2_PLACEMENT_3D ( 'NONE', #23178, #36695, #28681 ) ;
#61446 = CARTESIAN_POINT ( 'NONE',  ( 11.62006642628028175, 14.99999999999807088, -8.881585844848984834 ) ) ;
#61447 = CARTESIAN_POINT ( 'NONE',  ( 10.00000000000000178, 42.25893115100078745, 9.846743663894594434 ) ) ;
#61448 = CARTESIAN_POINT ( 'NONE',  ( 6.565887622018943937, 50.16530133659708213, 12.81628187352647430 ) ) ;
#61449 = CARTESIAN_POINT ( 'NONE',  ( -7.082119434687044190, -12.36291783175269643, 12.26659068614894998 ) ) ;
#61450 = CARTESIAN_POINT ( 'NONE',  ( 1.472469842513823179, 40.59226448433411605, -4.923371831947296329 ) ) ;
#61451 = CARTESIAN_POINT ( 'NONE',  ( 1.472469842513823179, 51.42559781766745886, 4.923371831947296329 ) ) ;
#61452 = CARTESIAN_POINT ( 'NONE',  ( -2.266590686148945544, 37.22041550158063217, 7.082119434687048631 ) ) ;
#61453 = VERTEX_POINT ( 'NONE', #46687 ) ;
#61454 = CARTESIAN_POINT ( 'NONE',  ( 22.26659068614895176, 14.72041550158063572, -7.082119434687042414 ) ) ;
#61455 = CARTESIAN_POINT ( 'NONE',  ( 7.084665262690076126, 59.10535201082150536, 10.88017736071109987 ) ) ;
#61456 = PRESENTATION_STYLE_ASSIGNMENT (( #30463 ) ) ;
#61457 = CARTESIAN_POINT ( 'NONE',  ( 13.79529636645031943, 60.34541550158063927, -14.16423886937409904 ) ) ;
#61458 = CARTESIAN_POINT ( 'NONE',  ( 13.43411237798106583, 12.66530133659708746, -12.81628187352647252 ) ) ;
#61459 = CARTESIAN_POINT ( 'NONE',  ( 20.15039907845753930, 1.748846992468885198, 6.262539305110068177 ) ) ;
#61460 = CARTESIAN_POINT ( 'NONE',  ( 0.1532563361054083140, 1.008931151000784787, 1.131784320476157264E-15 ) ) ;
#61461 = CARTESIAN_POINT ( 'NONE',  ( 4.395886034088992034, -0.8422402087801302839, -4.000000000000000000 ) ) ;
#61462 = CARTESIAN_POINT ( 'NONE',  ( 0.1532563361054082862, 31.21726448433412315, 2.638427012816831674 ) ) ;
#61463 = CARTESIAN_POINT ( 'NONE',  ( -2.816281873526473856, 34.12363466993042493, 9.499525473075851096E-16 ) ) ;
#61464 = CARTESIAN_POINT ( 'NONE',  ( 20.36894250292379382, 63.67874883491396787, 10.36894250292379205 ) ) ;
#61465 = CARTESIAN_POINT ( 'NONE',  ( -14.56089864659467814, -3.220842781934475856E-15, -1.374314915485489896 ) ) ;
#61466 = CARTESIAN_POINT ( 'NONE',  ( 17.96484262340118221, 26.18868534415483396, -7.964842623401177768 ) ) ;
#61467 = CARTESIAN_POINT ( 'NONE',  ( 10.00000000000000000, 21.81368534415484106, -10.88017736071110342 ) ) ;
#61468 = CARTESIAN_POINT ( 'NONE',  ( 1.472469842513823179, 55.59226448433412315, -4.923371831947296329 ) ) ;
#61469 = CARTESIAN_POINT ( 'NONE',  ( 19.84674366389459266, 58.30059781766745886, 2.638427012816836559 ) ) ;
#61470 = CARTESIAN_POINT ( 'NONE',  ( 22.81628187352648496, 56.83196800326374643, -3.434112377981050290 ) ) ;
#61471 = LINE ( 'NONE', #45996, #8885 ) ;
#61472 = ORIENTED_EDGE ( 'NONE', *, *, #9519, .F. ) ;
#61473 = CARTESIAN_POINT ( 'NONE',  ( 15.44008868035555793, 16.39701867748817321, -9.422509992056140149 ) ) ;
#61474 = EDGE_CURVE ( 'NONE', #15967, #44777, #77184, .T. ) ;
#61475 = CARTESIAN_POINT ( 'NONE',  ( 13.43411237798106583, 17.66530133659708923, -12.81628187352647252 ) ) ;
#61476 = DIRECTION ( 'NONE',  ( 0.2672383760782571227, 0.000000000000000000, 0.9636304532086229502 ) ) ;
#61477 = CARTESIAN_POINT ( 'NONE',  ( 0.1532563361054082862, 51.21726448433412315, 2.638427012816831674 ) ) ;
#61478 = CARTESIAN_POINT ( 'NONE',  ( -0.8801773607111009756, 43.06368534415484106, 1.068504757029289695E-15 ) ) ;
#61479 = AXIS2_PLACEMENT_3D ( 'NONE', #22838, #68826, #45323 ) ;
#61480 = CARTESIAN_POINT ( 'NONE',  ( 0.6178305044545838731, 19.74863466993042138, 9.382169495545420901 ) ) ;
#61482 = DIRECTION ( 'NONE',  ( 0.02970531260815257105, -0.9995586998285053149, 1.111794303139694811E-13 ) ) ;
#61481 = CARTESIAN_POINT ( 'NONE',  ( 7.084665262690076126, 49.10535201082149825, 10.88017736071109987 ) ) ;
#61483 = SURFACE_STYLE_USAGE ( .BOTH. , #38508 ) ;
#61484 = CARTESIAN_POINT ( 'NONE',  ( 10.00000000000000000, 62.87363466993042493, -12.81628187352647608 ) ) ;
#61485 = ORIENTED_EDGE ( 'NONE', *, *, #86594, .F. ) ;
#61486 = FILL_AREA_STYLE_COLOUR ( '', #97993 ) ;
#61487 = CARTESIAN_POINT ( 'NONE',  ( 0.5774900079438607392, 43.48035201082151247, 5.440088680355550821 ) ) ;
#61489 = CARTESIAN_POINT ( 'NONE',  ( 17.08211943468705840, 10.13708216824730179, -12.26659068614894466 ) ) ;
#61488 = CARTESIAN_POINT ( 'NONE',  ( 22.81628187352647785, 46.41530133659708213, 3.434112377981063169 ) ) ;
#61490 = CARTESIAN_POINT ( 'NONE',  ( 10.00000000000000000, 64.75893115100078035, -9.846743663894594434 ) ) ;
#61491 = CARTESIAN_POINT ( 'NONE',  ( 10.00000000000000178, 2.258931151000784787, 9.846743663894594434 ) ) ;
#61492 = CARTESIAN_POINT ( 'NONE',  ( 0.000000000000000000, 14.49999999999999822, 0.000000000000000000 ) ) ;
#61493 = CARTESIAN_POINT ( 'NONE',  ( 24.16423886937409904, 44.09541550158063927, 3.795296366450317205 ) ) ;
#61494 = CARTESIAN_POINT ( 'NONE',  ( 15.44008868035555793, 6.397018677488170546, -9.422509992056140149 ) ) ;
#61495 = CARTESIAN_POINT ( 'NONE',  ( 19.42250999205614193, 5.147018677488171434, 5.440088680355555262 ) ) ;
#61496 = DIRECTION ( 'NONE',  ( -0.6755902076156641289, 0.000000000000000000, 0.7372773368101205316 ) ) ;
#61497 = ORIENTED_EDGE ( 'NONE', *, *, #73376, .F. ) ;
#61498 = VERTEX_POINT ( 'NONE', #77675 ) ;
#61499 = CARTESIAN_POINT ( 'NONE',  ( 10.00000000000000000, 6.813685344154838397, -10.88017736071110342 ) ) ;
#61500 = CARTESIAN_POINT ( 'NONE',  ( 7.084665262690076126, 9.105352010821503583, 10.88017736071109987 ) ) ;
#61501 = CARTESIAN_POINT ( 'NONE',  ( 19.84674366389459621, 43.50893115100078745, 7.409399052514197653E-17 ) ) ;
#61502 = AXIS2_PLACEMENT_3D ( 'NONE', #75571, #68571, #16057 ) ;
#61503 = CARTESIAN_POINT ( 'NONE',  ( -1.099225684535947600, 38.70696800326375353, -6.408140936763238038 ) ) ;
#61504 = DIRECTION ( 'NONE',  ( -0.8320502943378437211, 0.5547001962252290364, 0.000000000000000000 ) ) ;
#61506 = CARTESIAN_POINT ( 'NONE',  ( 6.204703633549690345, 12.84541550158063572, 14.16423886937410082 ) ) ;
#61505 = DIRECTION ( 'NONE',  ( -0.000000000000000000, 0.000000000000000000, 1.000000000000000000 ) ) ;
#61507 = CARTESIAN_POINT ( 'NONE',  ( 2.035157376598822676, 27.43868534415483396, -7.964842623401177768 ) ) ;
#61508 = CARTESIAN_POINT ( 'NONE',  ( -0.8801773607110991993, 2.855352010821504471, -2.915334737309923874 ) ) ;
#61509 = CARTESIAN_POINT ( 'NONE',  ( 10.00000000000000000, 44.75893115100078745, -9.846743663894594434 ) ) ;
#61510 = SURFACE_STYLE_USAGE ( .BOTH. , #74 ) ;
#61511 = CARTESIAN_POINT ( 'NONE',  ( 2.791683348922237240, 25.38393115100078390, -7.208316651077763204 ) ) ;
#61512 = CARTESIAN_POINT ( 'NONE',  ( 1.274849032794324932, 32.55509018479936145, -6.500000000000021316 ) ) ;
#61513 = CARTESIAN_POINT ( 'NONE',  ( 11.09922568453595026, -38.79303199673623936, 6.408140936763232709 ) ) ;
#61514 = ORIENTED_EDGE ( 'NONE', *, *, #4197, .T. ) ;
#61515 = ORIENTED_EDGE ( 'NONE', *, *, #70529, .T. ) ;
#61516 = CARTESIAN_POINT ( 'NONE',  ( 10.00000000000000000, 54.75893115100078745, -9.846743663894594434 ) ) ;
#61518 = CARTESIAN_POINT ( 'NONE',  ( 10.00000000000000000, 36.81368534415484106, -10.88017736071110342 ) ) ;
#61517 = CARTESIAN_POINT ( 'NONE',  ( 15.44008868035555260, 34.73035201082151247, 9.422509992056143702 ) ) ;
#61520 = CARTESIAN_POINT ( 'NONE',  ( 0.6178305044545818747, 33.49863466993042493, -9.382169495545419124 ) ) ;
#61519 = CARTESIAN_POINT ( 'NONE',  ( 7.084665262690076126, 9.105352010821503583, 10.88017736071109987 ) ) ;
#61521 = CARTESIAN_POINT ( 'NONE',  ( 10.00000000000000000, 15.55374883491396787, -14.16423886937410082 ) ) ;
#61522 = VECTOR ( 'NONE', #81078, 1000.000000000000114 ) ;
#61523 = EDGE_CURVE ( 'NONE', #55728, #71988, #48934, .T. ) ;
#61524 = VECTOR ( 'NONE', #19663, 1000.000000000000000 ) ;
#61525 = ADVANCED_FACE ( 'NONE', ( #3666 ), #96854, .T. ) ;
#61526 = CARTESIAN_POINT ( 'NONE',  ( -1.099225684535947600, 49.54030133659708923, 6.408140936763237150 ) ) ;
#61527 = ADVANCED_FACE ( 'NONE', ( #94651 ), #86177, .F. ) ;
#61528 = ORIENTED_EDGE ( 'NONE', *, *, #10862, .T. ) ;
#61529 = CARTESIAN_POINT ( 'NONE',  ( 18.52753015748618282, 48.92559781766745886, -4.923371831947291888 ) ) ;
#61530 = CARTESIAN_POINT ( 'NONE',  ( 15.44008868035555793, 26.39701867748817321, -9.422509992056140149 ) ) ;
#61531 = VERTEX_POINT ( 'NONE', #48159 ) ;
#61532 = CARTESIAN_POINT ( 'NONE',  ( 12.91533473730993009, 16.60535201082150891, -10.88017736071109987 ) ) ;
#61533 = EDGE_LOOP ( 'NONE', ( #52496, #38510, #81083, #61662, #55522, #80356 ) ) ;
#61534 = CARTESIAN_POINT ( 'NONE',  ( -0.8801773607110991993, 57.85535201082149825, -2.915334737309923874 ) ) ;
#61535 = PRESENTATION_STYLE_ASSIGNMENT (( #76546 ) ) ;
#61536 = CARTESIAN_POINT ( 'NONE',  ( -0.8801773607110991993, 67.85535201082151957, -2.915334737309923874 ) ) ;
#61537 = CIRCLE ( 'NONE', #35982, 19.43999999999999773 ) ;
#61538 = CARTESIAN_POINT ( 'NONE',  ( 14.92337183194729988, 14.34226448433411782, -8.527530157486177487 ) ) ;
#61539 = CARTESIAN_POINT ( 'NONE',  ( 20.88017736071110519, 55.56368534415484817, 2.639326808657452039E-16 ) ) ;
#61540 = CARTESIAN_POINT ( 'NONE',  ( 4.130000000000002558, 1.019547802438464768, 2.750000000000000000 ) ) ;
#61541 = CARTESIAN_POINT ( 'NONE',  ( -46.69421152571126044, 101.0768001808267229, 8.798454068542781670 ) ) ;
#61543 = EDGE_LOOP ( 'NONE', ( #6583, #67526, #46896, #94476, #93385, #30897 ) ) ;
#61542 = CARTESIAN_POINT ( 'NONE',  ( 7.361572987183170547, 2.050597817667451750, 9.846743663894590881 ) ) ;
#61544 =( BOUNDED_SURFACE ( )  B_SPLINE_SURFACE ( 1, 2, ( 
 ( #72259, #41305, #34748, #42757, #2820, #3287, #65237, #56769, #65737, #12250, #64254, #87265, #11267, #95255, #95762, #72741, #18786, #57744, #96266, #50240, #27740, #57253, #41787, #3788, #80755, #33752, #34243, #49748, #80258, #86295, #48280, #78792, #33270, #63764, #94271, #29710, #13738, #97261, #90214, #44221, #52228, #6239, #37736, #50754, #5751, #44720, #89725, #12739, #20253, #28239, #89239, #81724, #43238, #58734, #20747, #14744, #83221, #67734, #28730, #29221, #82224, #59221, #68235, #13238, #88743, #81240, #45218, #96764, #21747, #43732, #51238, #60218, #74218, #66229, #98252, #36741, #21242, #75217, #75715, #90712, #36240, #51740, #7229, #59720, #66736, #74725, #98752, #73733, #58222, #67232, #22237, #97755, #82720, #14239, #5263, #6729, #37245, #35741, #52714, #16205, #76696, #62171, #62668, #24205, #61683, #85681, #9189, #78173, #77676, #9683, #92679, #85191, #91202, #54672, #7731, #23724, #8217, #92200, #38227, #84221, #93169, #245, #68713, #70190, #47171, #38711, #54187, #91709, #76218, #84699, #23228, #31679, #46688, #22730, #16698, #69210, #17202, #40180, #8693, #30693, #39703, #53700, #61203, #15730, #70687, #46210, #736, #1708, #39209, #31189, #30202, #32167, #24694, #15235, #77185, #55166, #47679, #69696, #60705, #53213, #83715, #1226, #45716, #87635, #72140, #11151, #19149, #40677, #4157, #64134, #26160, #64622, #18172, #41182, #26643, #2703, #18664, #57630, #2205, #42159, #80136, #95642, #93667, #50132, #3667, #49152, #10668, #34130, #32666, #72624, #95131, #94156, #71663, #33154, #55679, #19639, #3173, #42638, #63159, #71177, #87141, #33637, #34624, #25201, #63648, #65123, #94652, #41671, #56655, #12135, #25682, #86178, #17688, #27128, #56175, #57139, #86668, #48654, #88127, #79154, #10183, #80639, #79653, #49626, #11646, #48160, #78674, #5137, #51626, #35628, #27626, #20127, #66113, #90100, #58111, #5636, #82106, #13617, #44607, #66620, #81122, #60089, #96642, #28119, #13120, #73613, #36114, #50631, #44098, #52113, #4657, #43125, #74609, #65617, #88620, #12623, #6122, #35118, #67112, #21628, #67618, #58619, #51120, #29587, #75102, #89120, #36628, #97147, #20631, #81611, #90591, #52598, #43616, #74103, #6609, #59105, #28618, #82605, #22118, #96143, #89614, #14123, #21127, #83101, #98126, #97637, #29102, #59604, #37122, #14629, #73116, #84097, #69583, #32050, #62062, #24590, #54074, #23111, #61572, #92565, #7622, #53583, #76580, #69094, #24091, #23609, #30580, #8586, #62552, #15612, #16585, #628, #46096, #77074, #31074, #39092, #92083, #55053, #37616, #91595, #31566, #8100, #98635, #7112, #15118 ),
 ( #45094, #85076, #46575, #30086, #83604, #84589, #75600, #1103, #54559, #39588, #76092, #38596, #1600, #47061, #38114, #16089, #77559, #53092, #9075, #93057, #85572, #70079, #68110, #60593, #91088, #68603, #22615, #45594, #131, #61085, #95023, #25571, #34513, #42053, #94050, #86557, #10553, #94536, #64517, #41566, #56063, #72033, #4051, #34020, #95533, #26055, #18062, #33529, #26531, #78557, #48541, #79040, #41064, #57028, #56545, #2590, #79545, #65006, #71561, #87529, #3073, #64024, #49041, #87040, #11045, #18549, #28381, #9567, #63540, #3560, #19043, #70569, #78064, #86067, #48044, #40567, #2095, #17578, #10068, #72517, #58872, #49519, #80028, #11532, #17086, #47566, #40069, #71065, #32554, #63055, #93552, #55568, #25085, #33045, #59360, #91340, #13878, #97389, #30335, #67867, #21880, #75852, #7861, #60842, #21376, #98389, #51874, #43859, #36377, #82357, #7372, #74354, #52360, #29845, #60350, #22868, #82861, #28856, #76344, #44361, #74863, #29351, #89862, #14378, #66871, #90843, #68367, #20888, #6362, #22372, #81863, #59855, #15373, #52848, #36875, #44847, #38359, #51374, #68854, #90344, #98884, #75352, #67365, #6867, #5881, #97893, #83356, #37377, #14880, #45348, #37871, #53338, #83847, #45854, #386, #30835, #89374, #13374, #93307, #2340, #9321, #1846, #23361, #77806, #8342, #1360, #16340, #31811, #38849, #23852, #47803, #69338, #863, #55311, #32304, #46823, #69836, #31322, #76828, #62307, #61822, #47306, #92815, #53845, #39825, #77313, #40323, #32795, #54808, #92330, #24831, #54318, #84833, #8827, #63291, #39342, #24345, #85818, #85319, #16831, #93800, #17333, #70330, #15855, #62809, #78303, #9822, #70827, #61333, #91844, #84355, #46340, #92167, #38197, #22701, #60674, #68684, #90183, #53670, #14711, #75683, #15200, #67704, #90680, #76180, #52197, #68198, #8183, #51710, #91677, #30663, #46179, #44188, #703, #53179, #98719, #60184, #83685, #82194, #23196, #45682, #44690, #22206, #82691, #6208, #69180, #52685, #13703, #74698, #21713, #37700, #83186, #84185, #36710, #14209, #15695, #45185, #91172, #7197, #30170, #7700, #76665, #67201, #75185, #38680, #212, #61169, #31156, #61646, #97727, #29190, #6698, #59688, #37216, #98215, #29674, #53823, #38338, #30812, #75828, #90319, #69321, #75330, #14353, #22351, #82833, #14858, #59825, #22844, #61310, #13854, #52338, #53319, #74839, #36851, #21858, #60816, #44334, #76322, #91822, #76808, #44822, #60332, #38828, #84335, #6843, #83826, #7349, #37356, #90825, #840, #61802, #29822, #52825, #15836, #68341, #67847, #23341, #31301, #6339, #98364, #46322, #83332, #92309, #8324 ) ),
 .UNSPECIFIED., .F., .F., .F. ) 
 B_SPLINE_SURFACE_WITH_KNOTS ( ( 2, 2 ),
 ( 3, 2, 2, 2, 2, 2, 2, 2, 2, 2, 2, 2, 2, 2, 2, 2, 2, 2, 2, 2, 2, 2, 2, 2, 2, 2, 2, 2, 2, 2, 2, 2, 2, 2, 2, 2, 2, 2, 2, 2, 2, 2, 2, 2, 2, 2, 2, 2, 2, 2, 2, 2, 2, 2, 2, 2, 2, 2, 2, 2, 2, 2, 2, 2, 2, 2, 2, 2, 2, 2, 2, 2, 2, 2, 2, 2, 2, 2, 2, 2, 2, 2, 2, 2, 2, 2, 2, 2, 2, 2, 2, 2, 2, 2, 2, 2, 2, 2, 2, 2, 2, 2, 2, 2, 2, 2, 2, 2, 2, 2, 2, 2, 2, 2, 2, 2, 2, 2, 2, 2, 2, 2, 2, 2, 2, 2, 2, 2, 2, 2, 2, 2, 2, 2, 2, 2, 2, 2, 2, 2, 2, 2, 2, 2, 2, 2, 2, 2, 2, 2, 2, 2, 2, 2, 2, 2, 2, 2, 2, 2, 2, 2, 3 ),
 ( 0.000000000000000000, 1.000000000000000000 ),
 ( 0.000000000000000000, 0.005952380952380952051, 0.01190476190476190410, 0.01785714285714285615, 0.02380952380952380820, 0.02976190476190476025, 0.03571428571428571230, 0.04166666666666666435, 0.04761904761904761640, 0.05357142857142856845, 0.05952380952380952051, 0.06547619047619047949, 0.07142857142857142461, 0.07738095238095238360, 0.08333333333333332871, 0.08928571428571428770, 0.09523809523809523281, 0.1011904761904761918, 0.1071428571428571369, 0.1130952380952380959, 0.1190476190476190410, 0.1250000000000000000, 0.1309523809523809590, 0.1369047619047619180, 0.1428571428571428492, 0.1488095238095238082, 0.1547619047619047672, 0.1607142857142857262, 0.1666666666666666574, 0.1726190476190476164, 0.1785714285714285754, 0.1845238095238095344, 0.1904761904761904656, 0.1964285714285714246, 0.2023809523809523836, 0.2083333333333333426, 0.2142857142857142738, 0.2202380952380952328, 0.2261904761904761918, 0.2321428571428571508, 0.2380952380952380820, 0.2440476190476190410, 0.2500000000000000000, 0.2559523809523809312, 0.2619047619047619180, 0.2678571428571428492, 0.2738095238095238360, 0.2797619047619047672, 0.2857142857142856984, 0.2916666666666666852, 0.2976190476190476164, 0.3035714285714285476, 0.3095238095238095344, 0.3154761904761904656, 0.3214285714285714524, 0.3273809523809523836, 0.3333333333333333148, 0.3392857142857143016, 0.3452380952380952328, 0.3511904761904761640, 0.3571428571428571508, 0.3630952380952380820, 0.3690476190476190688, 0.3750000000000000000, 0.3809523809523809312, 0.3869047619047619180, 0.3928571428571428492, 0.3988095238095238360, 0.4047619047619047672, 0.4107142857142856984, 0.4166666666666666852, 0.4226190476190476164, 0.4285714285714285476, 0.4345238095238095344, 0.4404761904761904656, 0.4464285714285714524, 0.4523809523809523836, 0.4583333333333333148, 0.4642857142857143016, 0.4702380952380952328, 0.4761904761904761640, 0.4821428571428571508, 0.4880952380952380820, 0.4940476190476190688, 0.5000000000000000000, 0.5059523809523809312, 0.5119047619047618625, 0.5178571428571429047, 0.5238095238095238360, 0.5297619047619047672, 0.5357142857142856984, 0.5416666666666666297, 0.5476190476190476719, 0.5535714285714286031, 0.5595238095238095344, 0.5654761904761904656, 0.5714285714285713969, 0.5773809523809523281, 0.5833333333333333703, 0.5892857142857143016, 0.5952380952380952328, 0.6011904761904761640, 0.6071428571428570953, 0.6130952380952381375, 0.6190476190476190688, 0.6250000000000000000, 0.6309523809523809312, 0.6369047619047618625, 0.6428571428571429047, 0.6488095238095238360, 0.6547619047619047672, 0.6607142857142856984, 0.6666666666666666297, 0.6726190476190476719, 0.6785714285714286031, 0.6845238095238095344, 0.6904761904761904656, 0.6964285714285713969, 0.7023809523809523281, 0.7083333333333333703, 0.7142857142857143016, 0.7202380952380952328, 0.7261904761904761640, 0.7321428571428570953, 0.7380952380952381375, 0.7440476190476190688, 0.7500000000000000000, 0.7559523809523809312, 0.7619047619047618625, 0.7678571428571429047, 0.7738095238095238360, 0.7797619047619047672, 0.7857142857142856984, 0.7916666666666666297, 0.7976190476190476719, 0.8035714285714286031, 0.8095238095238095344, 0.8154761904761904656, 0.8214285714285713969, 0.8273809523809523281, 0.8333333333333333703, 0.8392857142857143016, 0.8452380952380952328, 0.8511904761904761640, 0.8571428571428570953, 0.8630952380952381375, 0.8690476190476190688, 0.8750000000000000000, 0.8809523809523809312, 0.8869047619047618625, 0.8928571428571429047, 0.8988095238095238360, 0.9047619047619047672, 0.9107142857142856984, 0.9166666666666666297, 0.9226190476190476719, 0.9285714285714286031, 0.9345238095238095344, 0.9404761904761904656, 0.9464285714285713969, 0.9523809523809523281, 0.9583333333333333703, 0.9642857142857143016 ),
 .UNSPECIFIED. ) 
 GEOMETRIC_REPRESENTATION_ITEM ( )  RATIONAL_B_SPLINE_SURFACE ( (
 ( 1.000000000000000000, 0.9659258262890683122, 1.000000000000000000, 0.9659258262890683122, 1.000000000000000000, 0.9659258262890683122, 1.000000000000000000, 0.9659258262890683122, 1.000000000000000000, 0.9659258262890683122, 1.000000000000000000, 0.9659258262890683122, 1.000000000000000000, 0.9659258262890683122, 1.000000000000000000, 0.9659258262890683122, 1.000000000000000000, 0.9659258262890683122, 1.000000000000000000, 0.9659258262890683122, 1.000000000000000000, 0.9659258262890683122, 1.000000000000000000, 0.9659258262890683122, 1.000000000000000000, 0.9659258262890683122, 1.000000000000000000, 0.9659258262890683122, 1.000000000000000000, 0.9659258262890683122, 1.000000000000000000, 0.9659258262890683122, 1.000000000000000000, 0.9659258262890683122, 1.000000000000000000, 0.9659258262890683122, 1.000000000000000000, 0.9659258262890683122, 1.000000000000000000, 0.9659258262890683122, 1.000000000000000000, 0.9659258262890683122, 1.000000000000000000, 0.9659258262890683122, 1.000000000000000000, 0.9659258262890683122, 1.000000000000000000, 0.9659258262890683122, 1.000000000000000000, 0.9659258262890683122, 1.000000000000000000, 0.9659258262890683122, 1.000000000000000000, 0.9659258262890683122, 1.000000000000000000, 0.9659258262890683122, 1.000000000000000000, 0.9659258262890683122, 1.000000000000000000, 0.9659258262890683122, 1.000000000000000000, 0.9659258262890683122, 1.000000000000000000, 0.9659258262890683122, 1.000000000000000000, 0.9659258262890683122, 1.000000000000000000, 0.9659258262890683122, 1.000000000000000000, 0.9659258262890683122, 1.000000000000000000, 0.9659258262890683122, 1.000000000000000000, 0.9659258262890683122, 1.000000000000000000, 0.9659258262890683122, 1.000000000000000000, 0.9659258262890683122, 1.000000000000000000, 0.9659258262890683122, 1.000000000000000000, 0.9659258262890683122, 1.000000000000000000, 0.9659258262890683122, 1.000000000000000000, 0.9659258262890683122, 1.000000000000000000, 0.9659258262890683122, 1.000000000000000000, 0.9659258262890683122, 1.000000000000000000, 0.9659258262890683122, 1.000000000000000000, 0.9659258262890683122, 1.000000000000000000, 0.9659258262890683122, 1.000000000000000000, 0.9659258262890683122, 1.000000000000000000, 0.9659258262890683122, 1.000000000000000000, 0.9659258262890683122, 1.000000000000000000, 0.9659258262890683122, 1.000000000000000000, 0.9659258262890683122, 1.000000000000000000, 0.9659258262890683122, 1.000000000000000000, 0.9659258262890683122, 1.000000000000000000, 0.9659258262890683122, 1.000000000000000000, 0.9659258262890683122, 1.000000000000000000, 0.9659258262890683122, 1.000000000000000000, 0.9659258262890683122, 1.000000000000000000, 0.9659258262890683122, 1.000000000000000000, 0.9659258262890683122, 1.000000000000000000, 0.9659258262890683122, 1.000000000000000000, 0.9659258262890683122, 1.000000000000000000, 0.9659258262890683122, 1.000000000000000000, 0.9659258262890683122, 1.000000000000000000, 0.9659258262890683122, 1.000000000000000000, 0.9659258262890683122, 1.000000000000000000, 0.9659258262890683122, 1.000000000000000000, 0.9659258262890683122, 1.000000000000000000, 0.9659258262890683122, 1.000000000000000000, 0.9659258262890683122, 1.000000000000000000, 0.9659258262890683122, 1.000000000000000000, 0.9659258262890683122, 1.000000000000000000, 0.9659258262890683122, 1.000000000000000000, 0.9659258262890683122, 1.000000000000000000, 0.9659258262890683122, 1.000000000000000000, 0.9659258262890683122, 1.000000000000000000, 0.9659258262890683122, 1.000000000000000000, 0.9659258262890683122, 1.000000000000000000, 0.9659258262890683122, 1.000000000000000000, 0.9659258262890683122, 1.000000000000000000, 0.9659258262890683122, 1.000000000000000000, 0.9659258262890683122, 1.000000000000000000, 0.9659258262890683122, 1.000000000000000000, 0.9659258262890683122, 1.000000000000000000, 0.9659258262890683122, 1.000000000000000000, 0.9659258262890683122, 1.000000000000000000, 0.9659258262890683122, 1.000000000000000000, 0.9659258262890683122, 1.000000000000000000, 0.9659258262890683122, 1.000000000000000000, 0.9659258262890683122, 1.000000000000000000, 0.9659258262890683122, 1.000000000000000000, 0.9659258262890683122, 1.000000000000000000, 0.9659258262890683122, 1.000000000000000000, 0.9659258262890683122, 1.000000000000000000, 0.9659258262890683122, 1.000000000000000000, 0.9659258262890683122, 1.000000000000000000, 0.9659258262890683122, 1.000000000000000000, 0.9659258262890683122, 1.000000000000000000, 0.9659258262890683122, 1.000000000000000000, 0.9659258262890683122, 1.000000000000000000, 0.9659258262890683122, 1.000000000000000000, 0.9659258262890683122, 1.000000000000000000, 0.9659258262890683122, 1.000000000000000000, 0.9659258262890683122, 1.000000000000000000, 0.9659258262890683122, 1.000000000000000000, 0.9659258262890683122, 1.000000000000000000, 0.9659258262890683122, 1.000000000000000000, 0.9659258262890683122, 1.000000000000000000, 0.9659258262890683122, 1.000000000000000000, 0.9659258262890683122, 1.000000000000000000, 0.9659258262890683122, 1.000000000000000000, 0.9659258262890683122, 1.000000000000000000, 0.9659258262890683122, 1.000000000000000000, 0.9659258262890683122, 1.000000000000000000, 0.9659258262890683122, 1.000000000000000000, 0.9659258262890683122, 1.000000000000000000, 0.9659258262890683122, 1.000000000000000000, 0.9659258262890683122, 1.000000000000000000, 0.9659258262890683122, 1.000000000000000000, 0.9659258262890683122, 1.000000000000000000, 0.9659258262890683122, 1.000000000000000000, 0.9659258262890683122, 1.000000000000000000, 0.9659258262890683122, 1.000000000000000000, 0.9659258262890683122, 1.000000000000000000, 0.9659258262890683122, 1.000000000000000000, 0.9659258262890683122, 1.000000000000000000, 0.9659258262890683122, 1.000000000000000000, 0.9659258262890683122, 1.000000000000000000, 0.9659258262890683122, 1.000000000000000000, 0.9659258262890683122, 1.000000000000000000, 0.9659258262890683122, 1.000000000000000000, 0.9659258262890683122, 1.000000000000000000, 0.9659258262890683122, 1.000000000000000000, 0.9659258262890683122, 1.000000000000000000, 0.9659258262890683122, 1.000000000000000000, 0.9659258262890683122, 1.000000000000000000, 0.9659258262890683122, 1.000000000000000000, 0.9659258262890683122, 1.000000000000000000, 0.9659258262890683122, 1.000000000000000000, 0.9659258262890683122, 1.000000000000000000, 0.9659258262890683122, 1.000000000000000000, 0.9659258262890683122, 1.000000000000000000, 0.9659258262890683122, 1.000000000000000000, 0.9659258262890683122, 1.000000000000000000, 0.9659258262890683122, 1.000000000000000000, 0.9659258262890683122, 1.000000000000000000, 0.9659258262890683122, 1.000000000000000000, 0.9659258262890683122, 1.000000000000000000, 0.9659258262890683122, 1.000000000000000000, 0.9659258262890683122, 1.000000000000000000, 0.9659258262890683122, 1.000000000000000000, 0.9659258262890683122, 1.000000000000000000, 0.9659258262890683122, 1.000000000000000000, 0.9659258262890683122, 1.000000000000000000, 0.9659258262890683122, 1.000000000000000000, 0.9659258262890683122, 1.000000000000000000, 0.9659258262890683122, 1.000000000000000000, 0.9659258262890683122, 1.000000000000000000, 0.9659258262890683122, 1.000000000000000000, 0.9659258262890683122, 1.000000000000000000, 0.9659258262890683122, 1.000000000000000000),
 ( 1.000000000000000000, 0.9659258262890683122, 1.000000000000000000, 0.9659258262890683122, 1.000000000000000000, 0.9659258262890683122, 1.000000000000000000, 0.9659258262890683122, 1.000000000000000000, 0.9659258262890683122, 1.000000000000000000, 0.9659258262890683122, 1.000000000000000000, 0.9659258262890683122, 1.000000000000000000, 0.9659258262890683122, 1.000000000000000000, 0.9659258262890683122, 1.000000000000000000, 0.9659258262890683122, 1.000000000000000000, 0.9659258262890683122, 1.000000000000000000, 0.9659258262890683122, 1.000000000000000000, 0.9659258262890683122, 1.000000000000000000, 0.9659258262890683122, 1.000000000000000000, 0.9659258262890683122, 1.000000000000000000, 0.9659258262890683122, 1.000000000000000000, 0.9659258262890683122, 1.000000000000000000, 0.9659258262890683122, 1.000000000000000000, 0.9659258262890683122, 1.000000000000000000, 0.9659258262890683122, 1.000000000000000000, 0.9659258262890683122, 1.000000000000000000, 0.9659258262890683122, 1.000000000000000000, 0.9659258262890683122, 1.000000000000000000, 0.9659258262890683122, 1.000000000000000000, 0.9659258262890683122, 1.000000000000000000, 0.9659258262890683122, 1.000000000000000000, 0.9659258262890683122, 1.000000000000000000, 0.9659258262890683122, 1.000000000000000000, 0.9659258262890683122, 1.000000000000000000, 0.9659258262890683122, 1.000000000000000000, 0.9659258262890683122, 1.000000000000000000, 0.9659258262890683122, 1.000000000000000000, 0.9659258262890683122, 1.000000000000000000, 0.9659258262890683122, 1.000000000000000000, 0.9659258262890683122, 1.000000000000000000, 0.9659258262890683122, 1.000000000000000000, 0.9659258262890683122, 1.000000000000000000, 0.9659258262890683122, 1.000000000000000000, 0.9659258262890683122, 1.000000000000000000, 0.9659258262890683122, 1.000000000000000000, 0.9659258262890683122, 1.000000000000000000, 0.9659258262890683122, 1.000000000000000000, 0.9659258262890683122, 1.000000000000000000, 0.9659258262890683122, 1.000000000000000000, 0.9659258262890683122, 1.000000000000000000, 0.9659258262890683122, 1.000000000000000000, 0.9659258262890683122, 1.000000000000000000, 0.9659258262890683122, 1.000000000000000000, 0.9659258262890683122, 1.000000000000000000, 0.9659258262890683122, 1.000000000000000000, 0.9659258262890683122, 1.000000000000000000, 0.9659258262890683122, 1.000000000000000000, 0.9659258262890683122, 1.000000000000000000, 0.9659258262890683122, 1.000000000000000000, 0.9659258262890683122, 1.000000000000000000, 0.9659258262890683122, 1.000000000000000000, 0.9659258262890683122, 1.000000000000000000, 0.9659258262890683122, 1.000000000000000000, 0.9659258262890683122, 1.000000000000000000, 0.9659258262890683122, 1.000000000000000000, 0.9659258262890683122, 1.000000000000000000, 0.9659258262890683122, 1.000000000000000000, 0.9659258262890683122, 1.000000000000000000, 0.9659258262890683122, 1.000000000000000000, 0.9659258262890683122, 1.000000000000000000, 0.9659258262890683122, 1.000000000000000000, 0.9659258262890683122, 1.000000000000000000, 0.9659258262890683122, 1.000000000000000000, 0.9659258262890683122, 1.000000000000000000, 0.9659258262890683122, 1.000000000000000000, 0.9659258262890683122, 1.000000000000000000, 0.9659258262890683122, 1.000000000000000000, 0.9659258262890683122, 1.000000000000000000, 0.9659258262890683122, 1.000000000000000000, 0.9659258262890683122, 1.000000000000000000, 0.9659258262890683122, 1.000000000000000000, 0.9659258262890683122, 1.000000000000000000, 0.9659258262890683122, 1.000000000000000000, 0.9659258262890683122, 1.000000000000000000, 0.9659258262890683122, 1.000000000000000000, 0.9659258262890683122, 1.000000000000000000, 0.9659258262890683122, 1.000000000000000000, 0.9659258262890683122, 1.000000000000000000, 0.9659258262890683122, 1.000000000000000000, 0.9659258262890683122, 1.000000000000000000, 0.9659258262890683122, 1.000000000000000000, 0.9659258262890683122, 1.000000000000000000, 0.9659258262890683122, 1.000000000000000000, 0.9659258262890683122, 1.000000000000000000, 0.9659258262890683122, 1.000000000000000000, 0.9659258262890683122, 1.000000000000000000, 0.9659258262890683122, 1.000000000000000000, 0.9659258262890683122, 1.000000000000000000, 0.9659258262890683122, 1.000000000000000000, 0.9659258262890683122, 1.000000000000000000, 0.9659258262890683122, 1.000000000000000000, 0.9659258262890683122, 1.000000000000000000, 0.9659258262890683122, 1.000000000000000000, 0.9659258262890683122, 1.000000000000000000, 0.9659258262890683122, 1.000000000000000000, 0.9659258262890683122, 1.000000000000000000, 0.9659258262890683122, 1.000000000000000000, 0.9659258262890683122, 1.000000000000000000, 0.9659258262890683122, 1.000000000000000000, 0.9659258262890683122, 1.000000000000000000, 0.9659258262890683122, 1.000000000000000000, 0.9659258262890683122, 1.000000000000000000, 0.9659258262890683122, 1.000000000000000000, 0.9659258262890683122, 1.000000000000000000, 0.9659258262890683122, 1.000000000000000000, 0.9659258262890683122, 1.000000000000000000, 0.9659258262890683122, 1.000000000000000000, 0.9659258262890683122, 1.000000000000000000, 0.9659258262890683122, 1.000000000000000000, 0.9659258262890683122, 1.000000000000000000, 0.9659258262890683122, 1.000000000000000000, 0.9659258262890683122, 1.000000000000000000, 0.9659258262890683122, 1.000000000000000000, 0.9659258262890683122, 1.000000000000000000, 0.9659258262890683122, 1.000000000000000000, 0.9659258262890683122, 1.000000000000000000, 0.9659258262890683122, 1.000000000000000000, 0.9659258262890683122, 1.000000000000000000, 0.9659258262890683122, 1.000000000000000000, 0.9659258262890683122, 1.000000000000000000, 0.9659258262890683122, 1.000000000000000000, 0.9659258262890683122, 1.000000000000000000, 0.9659258262890683122, 1.000000000000000000, 0.9659258262890683122, 1.000000000000000000, 0.9659258262890683122, 1.000000000000000000, 0.9659258262890683122, 1.000000000000000000, 0.9659258262890683122, 1.000000000000000000, 0.9659258262890683122, 1.000000000000000000, 0.9659258262890683122, 1.000000000000000000, 0.9659258262890683122, 1.000000000000000000, 0.9659258262890683122, 1.000000000000000000, 0.9659258262890683122, 1.000000000000000000, 0.9659258262890683122, 1.000000000000000000, 0.9659258262890683122, 1.000000000000000000, 0.9659258262890683122, 1.000000000000000000, 0.9659258262890683122, 1.000000000000000000, 0.9659258262890683122, 1.000000000000000000, 0.9659258262890683122, 1.000000000000000000, 0.9659258262890683122, 1.000000000000000000, 0.9659258262890683122, 1.000000000000000000, 0.9659258262890683122, 1.000000000000000000, 0.9659258262890683122, 1.000000000000000000, 0.9659258262890683122, 1.000000000000000000, 0.9659258262890683122, 1.000000000000000000, 0.9659258262890683122, 1.000000000000000000, 0.9659258262890683122, 1.000000000000000000, 0.9659258262890683122, 1.000000000000000000, 0.9659258262890683122, 1.000000000000000000, 0.9659258262890683122, 1.000000000000000000, 0.9659258262890683122, 1.000000000000000000, 0.9659258262890683122, 1.000000000000000000, 0.9659258262890683122, 1.000000000000000000, 0.9659258262890683122, 1.000000000000000000, 0.9659258262890683122, 1.000000000000000000, 0.9659258262890683122, 1.000000000000000000, 0.9659258262890683122, 1.000000000000000000, 0.9659258262890683122, 1.000000000000000000) ) ) 
 REPRESENTATION_ITEM ( '' )  SURFACE ( )  );
#61545 = CARTESIAN_POINT ( 'NONE',  ( 2.791683348922237240, 45.38393115100079456, -7.208316651077763204 ) ) ;
#61546 = EDGE_LOOP ( 'NONE', ( #82206, #51917, #52403, #74421 ) ) ;
#61547 = ORIENTED_EDGE ( 'NONE', *, *, #34219, .F. ) ;
#61548 = CARTESIAN_POINT ( 'NONE',  ( 6.767445849361247490, 15.00000000000000000, -13.38662304974496564 ) ) ;
#61549 = VECTOR ( 'NONE', #90486, 1000.000000000000000 ) ;
#61550 = SURFACE_SIDE_STYLE ('',( #53063 ) ) ;
#61551 = EDGE_CURVE ( 'NONE', #80599, #31483, #66495, .T. ) ;
#61552 = CARTESIAN_POINT ( 'NONE',  ( 24.16423886937410614, 19.51208216824729647, -3.795296366450302550 ) ) ;
#61553 = DIRECTION ( 'NONE',  ( -0.000000000000000000, -1.000000000000000000, 0.000000000000000000 ) ) ;
#61555 = CARTESIAN_POINT ( 'NONE',  ( 15.44008868035555260, 59.73035201082151247, 9.422509992056143702 ) ) ;
#61554 = LINE ( 'NONE', #23590, #48229 ) ;
#61556 = CARTESIAN_POINT ( 'NONE',  ( -0.8801773607111009756, 8.063685344154837509, 1.068504757029289695E-15 ) ) ;
#61557 = CARTESIAN_POINT ( 'NONE',  ( -0.1038446121089037222, 59.24302437010793909, -6.337995344473782211 ) ) ;
#61558 = VERTEX_POINT ( 'NONE', #47678 ) ;
#61559 = CARTESIAN_POINT ( 'NONE',  ( 19.84674366389459266, 3.717264484334118713, -2.638427012816827677 ) ) ;
#61560 = CARTESIAN_POINT ( 'NONE',  ( 19.84674366389459621, 3.508931151000785231, 7.409399052514197653E-17 ) ) ;
#61561 = CARTESIAN_POINT ( 'NONE',  ( 6.565887622018943937, 33.08196800326374643, -12.81628187352647608 ) ) ;
#61562 = CARTESIAN_POINT ( 'NONE',  ( 14.92337183194729633, 22.67559781766745175, 8.527530157486181039 ) ) ;
#61563 = DIRECTION ( 'NONE',  ( 0.000000000000000000, 0.000000000000000000, -1.000000000000000000 ) ) ;
#61564 = CARTESIAN_POINT ( 'NONE',  ( 21.09922568453595559, 17.04030133659708923, -6.408140936763230044 ) ) ;
#61565 = CARTESIAN_POINT ( 'NONE',  ( 1.499999999999998668, 1.840000000000001412, 1.836970198721028701E-16 ) ) ;
#61566 = AXIS2_PLACEMENT_3D ( 'NONE', #986, #15973, #29107 ) ;
#61567 = CARTESIAN_POINT ( 'NONE',  ( 19.84674366389459621, 8.508931151000785675, 7.409399052514197653E-17 ) ) ;
#61568 = ORIENTED_EDGE ( 'NONE', *, *, #87719, .T. ) ;
#61569 = CARTESIAN_POINT ( 'NONE',  ( 19.42250999205614548, 25.98035201082150891, -5.440088680355545492 ) ) ;
#61570 = CARTESIAN_POINT ( 'NONE',  ( 17.08211943468705840, 25.13708216824730357, -12.26659068614894466 ) ) ;
#61571 = CARTESIAN_POINT ( 'NONE',  ( 10.00000000000000000, 44.75893115100078745, -9.846743663894594434 ) ) ;
#61572 = CARTESIAN_POINT ( 'NONE',  ( 4.559911319644449179, 63.89701867748817676, 9.422509992056141925 ) ) ;
#61574 = CARTESIAN_POINT ( 'NONE',  ( -7.118731320094870973, -71.92838106472885329, -3.750000000000000000 ) ) ;
#61573 = CARTESIAN_POINT ( 'NONE',  ( 10.00000000000000178, 40.37363466993042493, 12.81628187352647608 ) ) ;
#61575 = CARTESIAN_POINT ( 'NONE',  ( 20.88017736071110519, 25.56368534415483751, 2.639326808657452039E-16 ) ) ;
#61576 = LINE ( 'NONE', #54078, #51722 ) ;
#61577 = CARTESIAN_POINT ( 'NONE',  ( 0.6178305044545818747, 13.49863466993041783, -9.382169495545419124 ) ) ;
#61578 = CARTESIAN_POINT ( 'NONE',  ( 2.791683348922240793, 46.63393115100077324, 7.208316651077764092 ) ) ;
#61579 = CARTESIAN_POINT ( 'NONE',  ( 7.964842623401181321, -0.06131465584516315737, 7.964842623401174215 ) ) ;
#61580 = CARTESIAN_POINT ( 'NONE',  ( -1.099225684535947600, 48.70696800326375353, -6.408140936763238038 ) ) ;
#61581 = DIRECTION ( 'NONE',  ( -0.7132504491541847846, 0.000000000000000000, 0.7009092642998475675 ) ) ;
#61583 = DIRECTION ( 'NONE',  ( -0.1736481776669272503, 0.9848077530122086864, 0.000000000000000000 ) ) ;
#61582 = CARTESIAN_POINT ( 'NONE',  ( 7.084665262690076126, 49.10535201082149825, 10.88017736071109987 ) ) ;
#61584 = AXIS2_PLACEMENT_3D ( 'NONE', #66739, #36243, #34246 ) ;
#61585 = LINE ( 'NONE', #29603, #29001 ) ;
#61586 = CARTESIAN_POINT ( 'NONE',  ( 19.42250999205614548, 35.98035201082151247, -5.440088680355545492 ) ) ;
#61587 = CARTESIAN_POINT ( 'NONE',  ( 12.91533473730992121, 39.52201867748817676, 10.88017736071110164 ) ) ;
#61588 = DIRECTION ( 'NONE',  ( -0.000000000000000000, -1.000000000000000000, -0.000000000000000000 ) ) ;
#61589 = CARTESIAN_POINT ( 'NONE',  ( 19.42250999205614548, 60.98035201082151247, -5.440088680355545492 ) ) ;
#61590 = CARTESIAN_POINT ( 'NONE',  ( 17.20831665107776587, 52.88393115100078035, 7.208316651077764980 ) ) ;
#61592 = CARTESIAN_POINT ( 'NONE',  ( 17.39651004071842166, 22.93575266056828355, 6.499999999999998224 ) ) ;
#61591 = CARTESIAN_POINT ( 'NONE',  ( 15.44008868035555260, 14.73035201082150536, 9.422509992056143702 ) ) ;
#61593 = CARTESIAN_POINT ( 'NONE',  ( -2.816281873526471635, 8.915301336597083903, -3.434112377981056508 ) ) ;
#61594 = ORIENTED_EDGE ( 'NONE', *, *, #74873, .T. ) ;
#61595 = CARTESIAN_POINT ( 'NONE',  ( 20.88017736071110875, 35.77201867748816966, -2.915334737309920765 ) ) ;
#61597 = CARTESIAN_POINT ( 'NONE',  ( 34.56412365047464874, 28.99999999999999645, -9.500000000000000000 ) ) ;
#61596 = CARTESIAN_POINT ( 'NONE',  ( -1.099225684535947600, 9.540301336597087456, 6.408140936763237150 ) ) ;
#61598 = CARTESIAN_POINT ( 'NONE',  ( -0.8801773607111008646, 28.27201867748817321, 2.915334737309923430 ) ) ;
#61599 = CARTESIAN_POINT ( 'NONE',  ( -4.164238869374099927, 32.01208216824730357, 3.795296366450308767 ) ) ;
#61600 = CARTESIAN_POINT ( 'NONE',  ( 12.63842701281683034, 27.46726448433411250, 9.846743663894596210 ) ) ;
#61601 = CARTESIAN_POINT ( 'NONE',  ( 12.91533473730993009, 56.60535201082151247, -10.88017736071109987 ) ) ;
#61602 = LINE ( 'NONE', #85109, #63350 ) ;
#61603 = CARTESIAN_POINT ( 'NONE',  ( -4.164238869374099927, 7.012082168247302683, 3.795296366450308767 ) ) ;
#61604 = EDGE_CURVE ( 'NONE', #88696, #25751, #25681, .T. ) ;
#61605 = TOROIDAL_SURFACE ( 'NONE', #976, 2.250000000000001332, 0.2500000000000000000 ) ;
#61606 = CARTESIAN_POINT ( 'NONE',  ( 14.92337183194729633, 52.67559781766745175, 8.527530157486181039 ) ) ;
#61607 = AXIS2_PLACEMENT_3D ( 'NONE', #71847, #26832, #85876 ) ;
#61608 = ORIENTED_EDGE ( 'NONE', *, *, #3663, .F. ) ;
#61609 = ORIENTED_EDGE ( 'NONE', *, *, #10623, .F. ) ;
#61610 = CARTESIAN_POINT ( 'NONE',  ( -4.164238869374099039, 41.80374883491397497, 8.674139862899312516E-16 ) ) ;
#61611 = CARTESIAN_POINT ( 'NONE',  ( 10.00000000000000000, 40.55374883491397497, -14.16423886937410082 ) ) ;
#61612 = CARTESIAN_POINT ( 'NONE',  ( 4.559911319644449179, 67.23035201082150536, -9.422509992056141925 ) ) ;
#61613 = CARTESIAN_POINT ( 'NONE',  ( 17.20831665107776587, 59.13393115100078745, -7.208316651077762316 ) ) ;
#61614 = CARTESIAN_POINT ( 'NONE',  ( -11.51383254013138746, -65.37322064362177798, 4.000000000000000000 ) ) ;
#61616 = CARTESIAN_POINT ( 'NONE',  ( -1.099225684535947600, 24.54030133659708923, 6.408140936763237150 ) ) ;
#61615 = CARTESIAN_POINT ( 'NONE',  ( 17.96484262340118221, 64.93868534415483396, 7.964842623401181321 ) ) ;
#61617 = CARTESIAN_POINT ( 'NONE',  ( 6.204703633549690345, 25.76208216824730712, -14.16423886937410259 ) ) ;
#61618 = CARTESIAN_POINT ( 'NONE',  ( 17.96484262340118221, 11.18868534415484106, -7.964842623401177768 ) ) ;
#61619 = COLOUR_RGB ( '', 0.31764706, 0.68627451, 0.89019608) ;
#61620 = CARTESIAN_POINT ( 'NONE',  ( 2.035157376598822676, 32.43868534415483396, -7.964842623401177768 ) ) ;
#61621 = CARTESIAN_POINT ( 'NONE',  ( -0.7375392941519317569, 15.00000000000000000, 14.98185688723470044 ) ) ;
#61622 = CARTESIAN_POINT ( 'NONE',  ( 12.91533473730992121, 59.52201867748816966, 10.88017736071110164 ) ) ;
#61623 = CARTESIAN_POINT ( 'NONE',  ( 7.208316651077764980, -17.11606884899921255, 7.208316651077762316 ) ) ;
#61624 = ORIENTED_EDGE ( 'NONE', *, *, #66318, .T. ) ;
#61625 = CYLINDRICAL_SURFACE ( 'NONE', #2850, 11.92686044187656513 ) ;
#61626 = CARTESIAN_POINT ( 'NONE',  ( -0.3289641300568009741, 12.24545670184113888, -5.963430220938281678 ) ) ;
#61627 = ORIENTED_EDGE ( 'NONE', *, *, #58471, .F. ) ;
#61629 = CARTESIAN_POINT ( 'NONE',  ( -0.3689425029237898834, 61.17874883491396076, -10.36894250292378850 ) ) ;
#61628 = CARTESIAN_POINT ( 'NONE',  ( 20.36894250292379382, 58.67874883491396076, 10.36894250292379205 ) ) ;
#61631 = CARTESIAN_POINT ( 'NONE',  ( 14.92337183194729988, 59.34226448433412315, -8.527530157486177487 ) ) ;
#61630 = CARTESIAN_POINT ( 'NONE',  ( 0.1532563361054082862, 31.21726448433412315, 2.638427012816831674 ) ) ;
#61632 = LINE ( 'NONE', #23677, #51009 ) ;
#61633 = EDGE_CURVE ( 'NONE', #21334, #43301, #10624, .T. ) ;
#61634 = CARTESIAN_POINT ( 'NONE',  ( -1.099225684535947600, 3.706968003263753531, -6.408140936763238038 ) ) ;
#61635 = CARTESIAN_POINT ( 'NONE',  ( 9.382169495545419124, 20.99863466993042493, 9.382169495545417348 ) ) ;
#61636 = ADVANCED_FACE ( 'NONE', ( #85190 ), #79153, .F. ) ;
#61637 = ORIENTED_EDGE ( 'NONE', *, *, #28003, .F. ) ;
#61638 = CARTESIAN_POINT ( 'NONE',  ( 24.16423886937410614, 44.30374883491397497, 8.672049930838204340E-16 ) ) ;
#61639 = CARTESIAN_POINT ( 'NONE',  ( -0.3689425029237898834, 41.17874883491397497, -10.36894250292378850 ) ) ;
#61640 = VERTEX_POINT ( 'NONE', #18171 ) ;
#61641 = CARTESIAN_POINT ( 'NONE',  ( -1.099225684535947600, 58.70696800326375353, -6.408140936763238038 ) ) ;
#61642 = CARTESIAN_POINT ( 'NONE',  ( 5.076628168052704559, 45.17559781766745175, -8.527530157486179263 ) ) ;
#61643 = CARTESIAN_POINT ( 'NONE',  ( 17.96484262340118221, 29.93868534415484106, 7.964842623401181321 ) ) ;
#61644 = CARTESIAN_POINT ( 'NONE',  ( -3.335590168189929816, -2.700456006050037328, 2.500000000000000000 ) ) ;
#61645 = CARTESIAN_POINT ( 'NONE',  ( 0.1532563361054100626, 55.80059781766745175, -2.638427012816831230 ) ) ;
#61646 = CARTESIAN_POINT ( 'NONE',  ( 1.472469842513823179, 55.59226448433412315, -4.923371831947296329 ) ) ;
#61647 = AXIS2_PLACEMENT_3D ( 'NONE', #43119, #12131, #42631 ) ;
#61648 = CARTESIAN_POINT ( 'NONE',  ( -1.099225684535947600, 29.54030133659708923, 6.408140936763237150 ) ) ;
#61649 = LINE ( 'NONE', #6210, #77612 ) ;
#61650 = B_SPLINE_CURVE_WITH_KNOTS ( 'NONE', 3,
 ( #84922, #90933, #98480, #84441 ),
 .UNSPECIFIED., .F., .F.,
 ( 4, 4 ),
 ( 6.213755518593340002E-17, 0.001060528352562006968 ),
 .UNSPECIFIED. ) ;
#61651 = DIRECTION ( 'NONE',  ( 0.000000000000000000, 0.000000000000000000, 1.000000000000000000 ) ) ;
#61652 = CARTESIAN_POINT ( 'NONE',  ( 0.2751277870542967463, 70.00000000000000000, 6.000000000000000000 ) ) ;
#61653 = VERTEX_POINT ( 'NONE', #40676 ) ;
#61654 = DIRECTION ( 'NONE',  ( 0.8616291604415267091, 0.000000000000000000, 0.5075383629607025382 ) ) ;
#61655 = CARTESIAN_POINT ( 'NONE',  ( 17.20831665107776587, 27.88393115100078390, 7.208316651077764980 ) ) ;
#61656 = CARTESIAN_POINT ( 'NONE',  ( 19.72487221294570858, 70.00000000000000000, -6.000000000000000000 ) ) ;
#61657 = VECTOR ( 'NONE', #4470, 1000.000000000000000 ) ;
#61658 = CARTESIAN_POINT ( 'NONE',  ( 0.6178305044545818747, 38.49863466993042493, -9.382169495545419124 ) ) ;
#61659 = DIRECTION ( 'NONE',  ( 0.6246950475544238435, 0.7808688094430307203, 0.000000000000000000 ) ) ;
#61660 = EDGE_CURVE ( 'NONE', #41466, #33199, #24107, .T. ) ;
#61661 = FACE_OUTER_BOUND ( 'NONE', #47971, .T. ) ;
#61662 = ORIENTED_EDGE ( 'NONE', *, *, #90871, .T. ) ;
#61663 = CARTESIAN_POINT ( 'NONE',  ( 0.1532563361054082862, 66.21726448433413736, 2.638427012816831674 ) ) ;
#61664 = CARTESIAN_POINT ( 'NONE',  ( 3.640395162852214650, 101.0000000000000000, 9.500000000000000000 ) ) ;
#61665 = CARTESIAN_POINT ( 'NONE',  ( 14.92337183194729988, 54.34226448433412315, -8.527530157486177487 ) ) ;
#61666 = CARTESIAN_POINT ( 'NONE',  ( 24.16423886937410614, 29.51208216824729647, -3.795296366450302550 ) ) ;
#61667 = CARTESIAN_POINT ( 'NONE',  ( 7.361572987183170547, 62.05059781766745886, 9.846743663894590881 ) ) ;
#61668 = B_SPLINE_CURVE_WITH_KNOTS ( 'NONE', 3,
 ( #51464, #44939, #13467, #75445, #89949, #43949 ),
 .UNSPECIFIED., .F., .F.,
 ( 4, 2, 4 ),
 ( 3.409110551496204552E-05, 0.0004400426677368010999, 0.0008459942299586402153 ),
 .UNSPECIFIED. ) ;
#61669 = DIRECTION ( 'NONE',  ( -0.07626964003977962370, 0.9970872288863209532, 0.000000000000000000 ) ) ;
#61670 = CARTESIAN_POINT ( 'NONE',  ( 14.92337183194729988, 19.34226448433411960, -8.527530157486177487 ) ) ;
#61671 = CARTESIAN_POINT ( 'NONE',  ( -2.816281873526473856, 49.12363466993042493, 9.499525473075851096E-16 ) ) ;
#61672 = CARTESIAN_POINT ( 'NONE',  ( 0.1532563361054100626, 65.80059781766745175, -2.638427012816831230 ) ) ;
#61673 = CARTESIAN_POINT ( 'NONE',  ( 7.084665262690076126, 54.10535201082151247, 10.88017736071109987 ) ) ;
#61674 = CARTESIAN_POINT ( 'NONE',  ( 0.1532563361054100626, 40.80059781766745886, -2.638427012816831230 ) ) ;
#61675 = CONTEXT_DEPENDENT_SHAPE_REPRESENTATION ( #87717, #2809 ) ;
#61677 =( GEOMETRIC_REPRESENTATION_CONTEXT ( 3 ) GLOBAL_UNCERTAINTY_ASSIGNED_CONTEXT ( ( #75123 ) ) GLOBAL_UNIT_ASSIGNED_CONTEXT ( ( #2327, #16325, #39325 ) ) REPRESENTATION_CONTEXT ( 'NONE', 'WORKASPACE' ) );
#61676 = CARTESIAN_POINT ( 'NONE',  ( 3.969999999999999751, 37.25000000000000000, -3.750000000000000000 ) ) ;
#61678 = AXIS2_PLACEMENT_3D ( 'NONE', #2773, #55245, #55755 ) ;
#61679 = B_SPLINE_CURVE_WITH_KNOTS ( 'NONE', 3,
 ( #75539, #67052, #60033, #58553 ),
 .UNSPECIFIED., .F., .F.,
 ( 4, 4 ),
 ( 4.336808689942017736E-19, 0.001036303429213369844 ),
 .UNSPECIFIED. ) ;
#61680 = CARTESIAN_POINT ( 'NONE',  ( 10.00000000000000000, 61.81368534415484106, -10.88017736071110342 ) ) ;
#61681 = VERTEX_POINT ( 'NONE', #25200 ) ;
#61682 = CARTESIAN_POINT ( 'NONE',  ( 6.728956594450720807, 1.228197773518735097E-15, 12.98689685418147555 ) ) ;
#61683 = CARTESIAN_POINT ( 'NONE',  ( 0.5774900079438607392, 23.48035201082150536, 5.440088680355550821 ) ) ;
#61685 = CARTESIAN_POINT ( 'NONE',  ( 10.00000000000000178, 54.31368534415484106, 10.88017736071110342 ) ) ;
#61684 = CARTESIAN_POINT ( 'NONE',  ( 13.43411237798105340, 5.581968003263753531, 12.81628187352647963 ) ) ;
#61686 = LINE ( 'NONE', #44723, #83933 ) ;
#61687 = CARTESIAN_POINT ( 'NONE',  ( -0.8801773607111009756, 68.06368534415484817, 1.068504757029289695E-15 ) ) ;
#61689 = FACE_OUTER_BOUND ( 'NONE', #29939, .T. ) ;
#61688 = CARTESIAN_POINT ( 'NONE',  ( 20.88017736071110164, 35.35535201082150536, 2.915334737309930979 ) ) ;
#61690 = CARTESIAN_POINT ( 'NONE',  ( 19.84674366389459266, 43.71726448433410894, -2.638427012816827677 ) ) ;
#61691 = CARTESIAN_POINT ( 'NONE',  ( 1.780824192092403058, 0.5000000000000004441, 14.89391369643514729 ) ) ;
#61692 = CARTESIAN_POINT ( 'NONE',  ( -7.082119434687058401, 20.97041550158063217, -12.26659068614894110 ) ) ;
#61693 = CARTESIAN_POINT ( 'NONE',  ( 18.52753015748618282, 63.92559781766745886, -4.923371831947291888 ) ) ;
#61695 = DIRECTION ( 'NONE',  ( -0.8320502943378437211, 0.5547001962252290364, 0.000000000000000000 ) ) ;
#61694 = CARTESIAN_POINT ( 'NONE',  ( 2.035157376598822676, 7.438685344154837509, -7.964842623401177768 ) ) ;
#61696 = FACE_BOUND ( 'NONE', #41960, .T. ) ;
#61697 = CARTESIAN_POINT ( 'NONE',  ( 22.26659068614895176, 24.72041550158063572, -7.082119434687042414 ) ) ;
#61698 = CIRCLE ( 'NONE', #28161, 0.2500000000000002220 ) ;
#61699 = CARTESIAN_POINT ( 'NONE',  ( 20.36894250292379382, 63.67874883491396787, 10.36894250292379205 ) ) ;
#61700 = CIRCLE ( 'NONE', #26596, 0.5000000000000000000 ) ;
#61701 = CARTESIAN_POINT ( 'NONE',  ( 19.84674366389459621, 23.50893115100078390, 7.409399052514197653E-17 ) ) ;
#61702 = CARTESIAN_POINT ( 'NONE',  ( -13.82192141328815715, 15.00000000000000000, 4.382292601468586568 ) ) ;
#61703 = VERTEX_POINT ( 'NONE', #2702 ) ;
#61704 = CARTESIAN_POINT ( 'NONE',  ( 17.20831665107776587, 29.13393115100078390, -7.208316651077762316 ) ) ;
#61705 = CARTESIAN_POINT ( 'NONE',  ( 19.42250999205614193, 25.14701867748817321, 5.440088680355555262 ) ) ;
#61706 = CARTESIAN_POINT ( 'NONE',  ( 5.076628168052703671, 61.84226448433412315, 8.527530157486179263 ) ) ;
#61708 = DIRECTION ( 'NONE',  ( 0.000000000000000000, 1.000000000000000000, 0.000000000000000000 ) ) ;
#61707 = CARTESIAN_POINT ( 'NONE',  ( 13.79529636645031943, 10.34541550158063394, -14.16423886937409904 ) ) ;
#61709 = PLANE ( 'NONE',  #27974 ) ;
#61710 = CARTESIAN_POINT ( 'NONE',  ( 1.472469842513823179, 16.42559781766745175, 4.923371831947296329 ) ) ;
#61711 = CARTESIAN_POINT ( 'NONE',  ( 22.81628187352648496, 31.83196800326375353, -3.434112377981050290 ) ) ;
#61712 = CARTESIAN_POINT ( 'NONE',  ( 1.472469842513823179, 41.42559781766745886, 4.923371831947296329 ) ) ;
#61713 = VERTEX_POINT ( 'NONE', #3172 ) ;
#61714 = CARTESIAN_POINT ( 'NONE',  ( 0.1532563361054100626, 20.80059781766744464, -2.638427012816831230 ) ) ;
#61715 = FACE_OUTER_BOUND ( 'NONE', #57098, .T. ) ;
#61716 = DIRECTION ( 'NONE',  ( 0.000000000000000000, 1.000000000000000000, 0.000000000000000000 ) ) ;
#61717 = CARTESIAN_POINT ( 'NONE',  ( 6.204703633549690345, 55.76208216824730357, -14.16423886937410259 ) ) ;
#61718 = CARTESIAN_POINT ( 'NONE',  ( 7.084665262690076126, 57.02201867748817676, -10.88017736071110164 ) ) ;
#61719 = CARTESIAN_POINT ( 'NONE',  ( -2.266590686148945544, 1.387082168247301128, -7.082119434687050408 ) ) ;
#61720 = CARTESIAN_POINT ( 'NONE',  ( 2.035157376598824452, 53.68868534415484817, 7.964842623401179544 ) ) ;
#61721 = CARTESIAN_POINT ( 'NONE',  ( 7.361572987183169658, 34.96726448433411605, -9.846743663894592657 ) ) ;
#61722 = CARTESIAN_POINT ( 'NONE',  ( 2.035157376598822676, 2.438685344154837953, -7.964842623401177768 ) ) ;
#61723 = CARTESIAN_POINT ( 'NONE',  ( 0.1532563361054083140, 46.00893115100079456, 1.131784320476157264E-15 ) ) ;
#61724 = EDGE_CURVE ( 'NONE', #26974, #77529, #83190, .T. ) ;
#61725 = CARTESIAN_POINT ( 'NONE',  ( 4.559911319644449179, 47.23035201082150536, -9.422509992056141925 ) ) ;
#61726 = CARTESIAN_POINT ( 'NONE',  ( 12.63842701281683922, 4.550597817667451750, -9.846743663894590881 ) ) ;
#61727 = ORIENTED_EDGE ( 'NONE', *, *, #26520, .T. ) ;
#61728 = EDGE_LOOP ( 'NONE', ( #95082, #17719, #88886, #82066 ) ) ;
#61729 = DIRECTION ( 'NONE',  ( 1.000000000000000000, -5.782411586589362323E-17, 0.000000000000000000 ) ) ;
#61730 = CARTESIAN_POINT ( 'NONE',  ( 5.625000000000005329, 4.588468844518209799, 9.742785792574933268 ) ) ;
#61731 = CARTESIAN_POINT ( 'NONE',  ( 19.84674366389459266, 28.30059781766745886, 2.638427012816836559 ) ) ;
#61732 = CARTESIAN_POINT ( 'NONE',  ( 16.40814093676323893, 50.79030133659708923, 11.09922568453595026 ) ) ;
#61734 = CARTESIAN_POINT ( 'NONE',  ( 18.52753015748618282, 43.92559781766745175, -4.923371831947291888 ) ) ;
#61733 = CARTESIAN_POINT ( 'NONE',  ( 0.5774900079438607392, 18.48035201082150536, 5.440088680355550821 ) ) ;
#61735 = CARTESIAN_POINT ( 'NONE',  ( -0.2418659066527637791, 35.11633188102327097, 6.114288769123057854 ) ) ;
#61736 = CARTESIAN_POINT ( 'NONE',  ( -2.266590686148945544, 32.22041550158063927, 7.082119434687048631 ) ) ;
#61737 = AXIS2_PLACEMENT_3D ( 'NONE', #1526, #38522, #93479 ) ;
#61738 = CARTESIAN_POINT ( 'NONE',  ( 20.36894250292379382, 58.67874883491396076, 10.36894250292379205 ) ) ;
#61739 = CARTESIAN_POINT ( 'NONE',  ( 7.361572987183170547, 57.05059781766744464, 9.846743663894590881 ) ) ;
#61740 = CARTESIAN_POINT ( 'NONE',  ( 18.00000000000000000, 78.65120189252176885, 3.750000044091261309 ) ) ;
#61741 = CARTESIAN_POINT ( 'NONE',  ( -0.8801773607110991993, 57.85535201082149825, -2.915334737309923874 ) ) ;
#61742 = CARTESIAN_POINT ( 'NONE',  ( 19.84674366389459621, 18.50893115100078745, 7.409399052514197653E-17 ) ) ;
#61743 = CARTESIAN_POINT ( 'NONE',  ( 6.879999999999995453, 43.00000000000000000, 6.500000000000000888 ) ) ;
#61744 = ORIENTED_EDGE ( 'NONE', *, *, #89951, .T. ) ;
#61745 = DIRECTION ( 'NONE',  ( -0.02617694830787627158, 0.000000000000000000, 0.9996573249755572599 ) ) ;
#61746 = ORIENTED_EDGE ( 'NONE', *, *, #65112, .T. ) ;
#61747 = CARTESIAN_POINT ( 'NONE',  ( 19.84674366389459266, 13.30059781766745353, 2.638427012816836559 ) ) ;
#61748 = AXIS2_PLACEMENT_3D ( 'NONE', #1353, #32298, #77308 ) ;
#61749 = VERTEX_POINT ( 'NONE', #71176 ) ;
#61750 = CARTESIAN_POINT ( 'NONE',  ( -2.266590686148945544, 22.22041550158063572, 7.082119434687048631 ) ) ;
#61751 = CARTESIAN_POINT ( 'NONE',  ( 14.92337183194729633, 17.67559781766745175, 8.527530157486181039 ) ) ;
#61752 = CARTESIAN_POINT ( 'NONE',  ( 19.42250999205614193, 40.14701867748817676, 5.440088680355555262 ) ) ;
#61753 = CARTESIAN_POINT ( 'NONE',  ( -46.44000000000001194, 93.00000000000000000, 9.000000000000000000 ) ) ;
#61754 = MECHANICAL_DESIGN_GEOMETRIC_PRESENTATION_REPRESENTATION (  '', ( #18657 ), #69554 ) ;
#61755 = ORIENTED_EDGE ( 'NONE', *, *, #38637, .F. ) ;
#61756 = CARTESIAN_POINT ( 'NONE',  ( -0.8801773607110991993, 32.85535201082151247, -2.915334737309923874 ) ) ;
#61757 = EDGE_CURVE ( 'NONE', #85730, #663, #87140, .T. ) ;
#61758 = DIRECTION ( 'NONE',  ( -0.000000000000000000, -1.000000000000000000, -0.000000000000000000 ) ) ;
#61759 = VECTOR ( 'NONE', #55150, 1000.000000000000000 ) ;
#61760 = ADVANCED_FACE ( 'NONE', ( #41181 ), #11313, .T. ) ;
#61761 = ORIENTED_EDGE ( 'NONE', *, *, #84025, .T. ) ;
#61762 = CARTESIAN_POINT ( 'NONE',  ( 17.96484262340118221, 39.93868534415484106, 7.964842623401181321 ) ) ;
#61763 = CARTESIAN_POINT ( 'NONE',  ( 19.72487221294571569, 55.71833443783938833, -6.499999999999990230 ) ) ;
#61764 = FACE_OUTER_BOUND ( 'NONE', #79783, .T. ) ;
#61765 = ORIENTED_EDGE ( 'NONE', *, *, #2386, .F. ) ;
#61766 = CARTESIAN_POINT ( 'NONE',  ( 22.81628187352648496, 16.83196800326374998, -3.434112377981050290 ) ) ;
#61767 = CARTESIAN_POINT ( 'NONE',  ( 18.52753015748617571, 8.092264484334117824, 4.923371831947298993 ) ) ;
#61768 = DIRECTION ( 'NONE',  ( 0.000000000000000000, 0.000000000000000000, 1.000000000000000000 ) ) ;
#61769 =( NAMED_UNIT ( * ) SI_UNIT ( $, .STERADIAN. ) SOLID_ANGLE_UNIT ( ) );
#61770 = CARTESIAN_POINT ( 'NONE',  ( 7.361572987183170547, 22.05059781766745530, 9.846743663894590881 ) ) ;
#61771 = CARTESIAN_POINT ( 'NONE',  ( 10.00000000000000178, 29.31368534415483751, 10.88017736071110342 ) ) ;
#61772 = AXIS2_PLACEMENT_3D ( 'NONE', #89891, #29382, #37903 ) ;
#61773 = CIRCLE ( 'NONE', #66572, 0.2500000000000002220 ) ;
#61774 = TOROIDAL_SURFACE ( 'NONE', #77765, 14.49999999999999822, 0.5000000000000000000 ) ;
#61775 = ORIENTED_EDGE ( 'NONE', *, *, #52851, .T. ) ;
#61776 = TOROIDAL_SURFACE ( 'NONE', #58572, 99.50000000000000000, 0.5000000000000000000 ) ;
#61777 = CARTESIAN_POINT ( 'NONE',  ( -8.900000000000000355, 75.76920769491746910, 3.000000000000000000 ) ) ;
#61778 = CARTESIAN_POINT ( 'NONE',  ( 4.559911319644449179, 52.23035201082151247, -9.422509992056141925 ) ) ;
#61779 = CARTESIAN_POINT ( 'NONE',  ( 1.707155281725207585, 7.901890803972831279, 6.499999999999992006 ) ) ;
#61780 = ADVANCED_FACE ( 'NONE', ( #11150 ), #26292, .T. ) ;
#61781 = B_SPLINE_CURVE_WITH_KNOTS ( 'NONE', 3,
 ( #43483, #97014, #20998, #51486, #81981, #47425 ),
 .UNSPECIFIED., .F., .F.,
 ( 4, 2, 4 ),
 ( 3.409110551467034092E-05, 0.0004400426677364971981, 0.0008459942299583240620 ),
 .UNSPECIFIED. ) ;
#61782 = CARTESIAN_POINT ( 'NONE',  ( 2.035157376598824452, 58.68868534415482685, 7.964842623401179544 ) ) ;
#61783 = CARTESIAN_POINT ( 'NONE',  ( -2.816281873526473856, -0.8763653300695799508, 9.499525473075851096E-16 ) ) ;
#61784 = ORIENTED_EDGE ( 'NONE', *, *, #56818, .T. ) ;
#61785 = CARTESIAN_POINT ( 'NONE',  ( 12.63842701281683034, 37.46726448433411605, 9.846743663894596210 ) ) ;
#61786 = CARTESIAN_POINT ( 'NONE',  ( 21.09922568453594849, 51.20696800326375353, 6.408140936763242479 ) ) ;
#61787 = CARTESIAN_POINT ( 'NONE',  ( 7.860426697680415131, 15.00000000000000000, 13.93165778241937680 ) ) ;
#61788 = CARTESIAN_POINT ( 'NONE',  ( 10.00000000000000178, 22.25893115100078745, 9.846743663894594434 ) ) ;
#61789 = CARTESIAN_POINT ( 'NONE',  ( 22.81628187352648496, 21.83196800326374643, -3.434112377981050290 ) ) ;
#61792 = AXIS2_PLACEMENT_3D ( 'NONE', #43385, #65390, #27397 ) ;
#61791 = CARTESIAN_POINT ( 'NONE',  ( -3.500000492100856953, 0.08994241822825245480, -2.750000000000000888 ) ) ;
#61790 = DIRECTION ( 'NONE',  ( 0.8070303256584298035, -0.5905099943842175847, 0.000000000000000000 ) ) ;
#61793 = CARTESIAN_POINT ( 'NONE',  ( 7.084665262690076126, 52.02201867748816255, -10.88017736071110164 ) ) ;
#61794 = CARTESIAN_POINT ( 'NONE',  ( 0.1532563361054082862, 61.21726448433412315, 2.638427012816831674 ) ) ;
#61795 = CYLINDRICAL_SURFACE ( 'NONE', #19949, 0.2500000000000002220 ) ;
#61796 = CARTESIAN_POINT ( 'NONE',  ( 14.92337183194729988, 24.34226448433411960, -8.527530157486177487 ) ) ;
#61797 = CARTESIAN_POINT ( 'NONE',  ( 17.20831665107776587, 14.13393115100078568, -7.208316651077762316 ) ) ;
#61798 = CARTESIAN_POINT ( 'NONE',  ( 4.559911319644449179, 8.897018677488171434, 9.422509992056141925 ) ) ;
#61799 = CARTESIAN_POINT ( 'NONE',  ( 10.00000000000000000, 12.87363466993042138, -12.81628187352647608 ) ) ;
#61801 =( LENGTH_UNIT ( ) NAMED_UNIT ( * ) SI_UNIT ( .MILLI., .METRE. ) );
#61800 =( GEOMETRIC_REPRESENTATION_CONTEXT ( 3 ) GLOBAL_UNCERTAINTY_ASSIGNED_CONTEXT ( ( #42432 ) ) GLOBAL_UNIT_ASSIGNED_CONTEXT ( ( #21396, #5898, #44379 ) ) REPRESENTATION_CONTEXT ( 'NONE', 'WORKASPACE' ) );
#61802 = CARTESIAN_POINT ( 'NONE',  ( 12.63842701281683922, 64.55059781766745175, -9.846743663894590881 ) ) ;
#61803 = CARTESIAN_POINT ( 'NONE',  ( 5.678900477192378560, -28.62996443916036782, -2.749999999998390177 ) ) ;
#61804 = CARTESIAN_POINT ( 'NONE',  ( 15.44008868035555260, 14.73035201082150536, 9.422509992056143702 ) ) ;
#61805 = CARTESIAN_POINT ( 'NONE',  ( 0.1532563361054100626, 40.80059781766745886, -2.638427012816831230 ) ) ;
#61806 = VECTOR ( 'NONE', #38934, 1000.000000000000000 ) ;
#61807 = CARTESIAN_POINT ( 'NONE',  ( 6.905552584538047434, -69.44516986195191066, 2.750000000000000444 ) ) ;
#61808 = CARTESIAN_POINT ( 'NONE',  ( 7.084665262690076126, 19.10535201082150181, 10.88017736071109987 ) ) ;
#61809 = DIRECTION ( 'NONE',  ( -0.1132032137678971873, 0.000000000000000000, -0.9935718556765885667 ) ) ;
#61810 = CARTESIAN_POINT ( 'NONE',  ( 0.5774900079438590739, 32.64701867748816966, -5.440088680355550821 ) ) ;
#61812 = CARTESIAN_POINT ( 'NONE',  ( -13.78891971893204804, 14.49999999999999112, -5.904717858191772528 ) ) ;
#61811 = CARTESIAN_POINT ( 'NONE',  ( 2.917880565312948704, 62.63708216824730357, 12.26659068614894643 ) ) ;
#61813 = CARTESIAN_POINT ( 'NONE',  ( 17.35999999999999588, 33.99999999999997158, -7.000000000000000888 ) ) ;
#61814 =( BOUNDED_SURFACE ( )  B_SPLINE_SURFACE ( 1, 2, ( 
 ( #39927, #31419, #31907, #23467, #53942, #1455, #62408, #93907, #86417, #46919, #32903, #69439, #958, #77412, #2446, #24443, #54910, #10414, #85424, #70430, #32411, #62911, #70928, #47903, #24936, #85926, #17435, #78408, #9926, #63402, #17918, #95890, #17646, #94983, #42009, #64964, #57481, #12473, #11985, #49480, #3514, #33485, #4009, #58453, #19487, #72476, #65463, #49980, #27472, #80487, #12961, #56508, #34471, #73457, #79988, #95490, #26489, #88969, #34966, #26982, #11006, #33973, #87490, #20478, #41522, #42488, #50964, #42977, #71990, #11490, #72969, #57965, #4985, #88469, #19971, #35466, #96489, #27960, #43456, #73958, #63983, #56763, #72251, #3784, #86289, #41299, #34238, #94764, #85798, #63760, #17310, #9300, #1827, #47787, #71771, #39810, #17797, #94265, #56287, #26264, #9799, #93780, #70806, #79764, #78284, #25309, #40299, #48273, #64735, #24812, #78786, #10293, #16811, #3282, #95247, #86782, #33745, #47287, #18285, #32281, #71291, #32776, #48765, #62788, #2323, #18781, #63273, #93287, #49264, #64247, #55794, #79272, #11262, #54788, #41781, #85305, #77788, #70311, #19258, #28230, #73233, #82218, #36736, #66224, #95757, #66730, #50233, #27241, #57737, #13230, #50748, #89232, #49742, #96756, #4761, #67227, #28724, #20741, #42265, #20246, #58728, #43726, #74213, #26753, #97254, #57248, #5743, #19749, #59214, #13730, #44214, #80251, #88241, #34740, #88734, #73726, #80748, #12243, #42752, #96258, #35232, #65730, #27735, #58218, #22722, #76689, #23720, #14234, #46684, #52709, #29702, #15721, #8211, #91197, #16201, #45212, #14736, #61674, #54179, #98242, #53205, #68227, #29214, #59713, #37239, #38705, #44712, #90706, #60211, #67728, #84691, #83710, #38222, #98747, #37724, #8688, #68708, #75710, #15228, #75211, #6722, #7224, #30197, #69205, #45708, #60698, #7725, #728, #239, #61195, #91703, #23221, #84216, #54666, #85183, #62166, #47164, #9183, #92671, #16693, #1220, #31674, #89821, #65338, #58325, #35342, #64839, #95358, #4378, #43821, #49850, #57840, #95865, #34843, #28821, #88842, #5360, #65834, #4864, #21340, #35839, #27347, #20351, #82318, #26857, #44320, #96365, #74317, #50846, #81338, #74820, #66828, #57355, #66327, #42367, #12835, #43335, #73830, #96862, #88349, #20845, #81820, #19847, #28338, #87847, #13338, #13838, #58827, #51337, #19367, #89335, #72840, #5843, #42854, #36334, #50339, #80850, #97350, #12348, #73337, #59320, #51831, #80359, #11859, #98348, #16303, #98841, #68814, #77278, #60799, #29314, #38318, #83315, #92293, #84795, #15336, #6826, #46304, #60314, #37340, #67830, #91803, #91299, #347, #97850 ),
 ( #53806, #45818, #22334, #29806, #36835, #7331, #61783, #22825, #75809, #30791, #53302, #61294, #83810, #46786, #59810, #37832, #76790, #14840, #45313, #90806, #23816, #7824, #68323, #90305, #52808, #30296, #54277, #21839, #76306, #67326, #84317, #44808, #23325, #15817, #8307, #38809, #69303, #825, #31284, #52322, #82815, #14335, #75314, #94247, #26251, #48747, #39793, #86271, #70293, #24307, #54770, #1808, #25777, #16795, #40280, #17782, #48257, #79256, #62772, #9782, #24795, #33731, #93271, #70788, #55271, #2305, #87240, #77772, #63256, #93764, #10766, #47271, #85783, #2798, #17294, #78768, #39307, #33251, #56271, #3264, #55776, #10276, #94747, #41281, #40775, #63744, #86764, #18268, #71755, #56746, #18766, #49246, #8788, #69800, #31775, #72718, #89215, #72235, #3767, #19242, #58714, #88223, #97241, #5729, #57721, #50218, #73214, #58201, #28215, #5241, #12226, #96240, #89704, #27223, #59200, #88717, #19732, #27720, #96740, #42249, #80732, #42736, #4745, #20728, #20228, #65216, #49724, #79748, #35212, #36216, #65714, #50732, #12721, #81220, #73709, #43213, #21218, #34222, #35719, #51217, #66208, #81703, #4253, #66716, #13216, #43709, #64719, #80233, #11740, #28709, #95228, #74196, #11244, #41764, #87729, #57232, #26737, #34723, #95742, #90194, #21723, #7712, #68693, #52206, #7207, #13714, #224, #713, #83695, #38206, #44197, #15213, #29198, #75695, #60194, #37708, #59696, #6706, #84197, #82700, #14219, #91687, #30673, #90690, #68210, #75196, #31169, #98731, #45692, #92179, #30181, #74708, #53193, #98225, #8194, #61658, #60685, #67711, #61181, #22218, #52695, #83199, #23205, #91184, #76191, #6217, #22710, #53680, #51721, #15706, #46192, #36722, #76675, #38691, #69190, #82203, #67211, #97736, #54165, #33132, #39684, #25661, #25178, #32647, #63627, #62149, #48630, #85659, #40160, #10160, #16185, #46668, #24673, #63142, #17178, #32144, #10645, #94133, #79134, #41159, #77166, #71644, #55145, #54652, #3152, #8674, #39186, #1204, #85170, #49603, #29443, #21980, #95109, #89470, #65094, #37472, #26140, #34108, #74958, #79631, #87611, #26618, #64600, #59947, #20985, #36475, #27105, #34601, #82958, #66968, #57114, #81959, #14473, #56634, #75451, #13474, #6461, #74455, #5983, #6964, #97986, #87121, #97488, #72117, #28954, #59456, #89957, #21473, #51972, #13982, #19122, #90437, #82459, #44456, #36969, #18640, #49129, #67465, #44946, #41650, #80112, #3644, #11619, #42136, #72601, #4137, #75945, #83942, #98980, #16437, #62402, #61424, #23461, #92908, #3400, #64855, #95374, #18897, #41903, #26874, #93406, #11876, #20367, #89837, #95882 ) ),
 .UNSPECIFIED., .F., .F., .F. ) 
 B_SPLINE_SURFACE_WITH_KNOTS ( ( 2, 2 ),
 ( 3, 2, 2, 2, 2, 2, 2, 2, 2, 2, 2, 2, 2, 2, 2, 2, 2, 2, 2, 2, 2, 2, 2, 2, 2, 2, 2, 2, 2, 2, 2, 2, 2, 2, 2, 2, 2, 2, 2, 2, 2, 2, 2, 2, 2, 2, 2, 2, 2, 2, 2, 2, 2, 2, 2, 2, 2, 2, 2, 2, 2, 2, 2, 2, 2, 2, 2, 2, 2, 2, 2, 2, 2, 2, 2, 2, 2, 2, 2, 2, 2, 2, 2, 2, 2, 2, 2, 2, 2, 2, 2, 2, 2, 2, 2, 2, 2, 2, 2, 2, 2, 2, 2, 2, 2, 2, 2, 2, 2, 2, 2, 2, 2, 2, 2, 2, 2, 2, 2, 2, 2, 2, 2, 2, 2, 2, 2, 2, 2, 2, 2, 2, 2, 2, 2, 2, 2, 2, 2, 2, 2, 2, 2, 2, 2, 2, 2, 2, 2, 2, 2, 2, 2, 2, 2, 2, 2, 2, 2, 2, 2, 2, 3 ),
 ( 0.000000000000000000, 1.000000000000000000 ),
 ( 0.000000000000000000, 0.005952380952380952051, 0.01190476190476190410, 0.01785714285714285615, 0.02380952380952380820, 0.02976190476190476025, 0.03571428571428571230, 0.04166666666666666435, 0.04761904761904761640, 0.05357142857142856845, 0.05952380952380952051, 0.06547619047619047949, 0.07142857142857142461, 0.07738095238095238360, 0.08333333333333332871, 0.08928571428571428770, 0.09523809523809523281, 0.1011904761904761918, 0.1071428571428571369, 0.1130952380952380959, 0.1190476190476190410, 0.1250000000000000000, 0.1309523809523809590, 0.1369047619047619180, 0.1428571428571428492, 0.1488095238095238082, 0.1547619047619047672, 0.1607142857142857262, 0.1666666666666666574, 0.1726190476190476164, 0.1785714285714285754, 0.1845238095238095344, 0.1904761904761904656, 0.1964285714285714246, 0.2023809523809523836, 0.2083333333333333426, 0.2142857142857142738, 0.2202380952380952328, 0.2261904761904761918, 0.2321428571428571508, 0.2380952380952380820, 0.2440476190476190410, 0.2500000000000000000, 0.2559523809523809312, 0.2619047619047619180, 0.2678571428571428492, 0.2738095238095238360, 0.2797619047619047672, 0.2857142857142856984, 0.2916666666666666852, 0.2976190476190476164, 0.3035714285714285476, 0.3095238095238095344, 0.3154761904761904656, 0.3214285714285714524, 0.3273809523809523836, 0.3333333333333333148, 0.3392857142857143016, 0.3452380952380952328, 0.3511904761904761640, 0.3571428571428571508, 0.3630952380952380820, 0.3690476190476190688, 0.3750000000000000000, 0.3809523809523809312, 0.3869047619047619180, 0.3928571428571428492, 0.3988095238095238360, 0.4047619047619047672, 0.4107142857142856984, 0.4166666666666666852, 0.4226190476190476164, 0.4285714285714285476, 0.4345238095238095344, 0.4404761904761904656, 0.4464285714285714524, 0.4523809523809523836, 0.4583333333333333148, 0.4642857142857143016, 0.4702380952380952328, 0.4761904761904761640, 0.4821428571428571508, 0.4880952380952380820, 0.4940476190476190688, 0.5000000000000000000, 0.5059523809523809312, 0.5119047619047618625, 0.5178571428571429047, 0.5238095238095238360, 0.5297619047619047672, 0.5357142857142856984, 0.5416666666666666297, 0.5476190476190476719, 0.5535714285714286031, 0.5595238095238095344, 0.5654761904761904656, 0.5714285714285713969, 0.5773809523809523281, 0.5833333333333333703, 0.5892857142857143016, 0.5952380952380952328, 0.6011904761904761640, 0.6071428571428570953, 0.6130952380952381375, 0.6190476190476190688, 0.6250000000000000000, 0.6309523809523809312, 0.6369047619047618625, 0.6428571428571429047, 0.6488095238095238360, 0.6547619047619047672, 0.6607142857142856984, 0.6666666666666666297, 0.6726190476190476719, 0.6785714285714286031, 0.6845238095238095344, 0.6904761904761904656, 0.6964285714285713969, 0.7023809523809523281, 0.7083333333333333703, 0.7142857142857143016, 0.7202380952380952328, 0.7261904761904761640, 0.7321428571428570953, 0.7380952380952381375, 0.7440476190476190688, 0.7500000000000000000, 0.7559523809523809312, 0.7619047619047618625, 0.7678571428571429047, 0.7738095238095238360, 0.7797619047619047672, 0.7857142857142856984, 0.7916666666666666297, 0.7976190476190476719, 0.8035714285714286031, 0.8095238095238095344, 0.8154761904761904656, 0.8214285714285713969, 0.8273809523809523281, 0.8333333333333333703, 0.8392857142857143016, 0.8452380952380952328, 0.8511904761904761640, 0.8571428571428570953, 0.8630952380952381375, 0.8690476190476190688, 0.8750000000000000000, 0.8809523809523809312, 0.8869047619047618625, 0.8928571428571429047, 0.8988095238095238360, 0.9047619047619047672, 0.9107142857142856984, 0.9166666666666666297, 0.9226190476190476719, 0.9285714285714286031, 0.9345238095238095344, 0.9404761904761904656, 0.9464285714285713969, 0.9523809523809523281, 0.9583333333333333703, 0.9642857142857143016 ),
 .UNSPECIFIED. ) 
 GEOMETRIC_REPRESENTATION_ITEM ( )  RATIONAL_B_SPLINE_SURFACE ( (
 ( 1.000000000000000000, 0.9659258262890683122, 1.000000000000000000, 0.9659258262890683122, 1.000000000000000000, 0.9659258262890683122, 1.000000000000000000, 0.9659258262890683122, 1.000000000000000000, 0.9659258262890683122, 1.000000000000000000, 0.9659258262890683122, 1.000000000000000000, 0.9659258262890683122, 1.000000000000000000, 0.9659258262890683122, 1.000000000000000000, 0.9659258262890683122, 1.000000000000000000, 0.9659258262890683122, 1.000000000000000000, 0.9659258262890683122, 1.000000000000000000, 0.9659258262890683122, 1.000000000000000000, 0.9659258262890683122, 1.000000000000000000, 0.9659258262890683122, 1.000000000000000000, 0.9659258262890683122, 1.000000000000000000, 0.9659258262890683122, 1.000000000000000000, 0.9659258262890683122, 1.000000000000000000, 0.9659258262890683122, 1.000000000000000000, 0.9659258262890683122, 1.000000000000000000, 0.9659258262890683122, 1.000000000000000000, 0.9659258262890683122, 1.000000000000000000, 0.9659258262890683122, 1.000000000000000000, 0.9659258262890683122, 1.000000000000000000, 0.9659258262890683122, 1.000000000000000000, 0.9659258262890683122, 1.000000000000000000, 0.9659258262890683122, 1.000000000000000000, 0.9659258262890683122, 1.000000000000000000, 0.9659258262890683122, 1.000000000000000000, 0.9659258262890683122, 1.000000000000000000, 0.9659258262890683122, 1.000000000000000000, 0.9659258262890683122, 1.000000000000000000, 0.9659258262890683122, 1.000000000000000000, 0.9659258262890683122, 1.000000000000000000, 0.9659258262890683122, 1.000000000000000000, 0.9659258262890683122, 1.000000000000000000, 0.9659258262890683122, 1.000000000000000000, 0.9659258262890683122, 1.000000000000000000, 0.9659258262890683122, 1.000000000000000000, 0.9659258262890683122, 1.000000000000000000, 0.9659258262890683122, 1.000000000000000000, 0.9659258262890683122, 1.000000000000000000, 0.9659258262890683122, 1.000000000000000000, 0.9659258262890683122, 1.000000000000000000, 0.9659258262890683122, 1.000000000000000000, 0.9659258262890683122, 1.000000000000000000, 0.9659258262890683122, 1.000000000000000000, 0.9659258262890683122, 1.000000000000000000, 0.9659258262890683122, 1.000000000000000000, 0.9659258262890683122, 1.000000000000000000, 0.9659258262890683122, 1.000000000000000000, 0.9659258262890683122, 1.000000000000000000, 0.9659258262890683122, 1.000000000000000000, 0.9659258262890683122, 1.000000000000000000, 0.9659258262890683122, 1.000000000000000000, 0.9659258262890683122, 1.000000000000000000, 0.9659258262890683122, 1.000000000000000000, 0.9659258262890683122, 1.000000000000000000, 0.9659258262890683122, 1.000000000000000000, 0.9659258262890683122, 1.000000000000000000, 0.9659258262890683122, 1.000000000000000000, 0.9659258262890683122, 1.000000000000000000, 0.9659258262890683122, 1.000000000000000000, 0.9659258262890683122, 1.000000000000000000, 0.9659258262890683122, 1.000000000000000000, 0.9659258262890683122, 1.000000000000000000, 0.9659258262890683122, 1.000000000000000000, 0.9659258262890683122, 1.000000000000000000, 0.9659258262890683122, 1.000000000000000000, 0.9659258262890683122, 1.000000000000000000, 0.9659258262890683122, 1.000000000000000000, 0.9659258262890683122, 1.000000000000000000, 0.9659258262890683122, 1.000000000000000000, 0.9659258262890683122, 1.000000000000000000, 0.9659258262890683122, 1.000000000000000000, 0.9659258262890683122, 1.000000000000000000, 0.9659258262890683122, 1.000000000000000000, 0.9659258262890683122, 1.000000000000000000, 0.9659258262890683122, 1.000000000000000000, 0.9659258262890683122, 1.000000000000000000, 0.9659258262890683122, 1.000000000000000000, 0.9659258262890683122, 1.000000000000000000, 0.9659258262890683122, 1.000000000000000000, 0.9659258262890683122, 1.000000000000000000, 0.9659258262890683122, 1.000000000000000000, 0.9659258262890683122, 1.000000000000000000, 0.9659258262890683122, 1.000000000000000000, 0.9659258262890683122, 1.000000000000000000, 0.9659258262890683122, 1.000000000000000000, 0.9659258262890683122, 1.000000000000000000, 0.9659258262890683122, 1.000000000000000000, 0.9659258262890683122, 1.000000000000000000, 0.9659258262890683122, 1.000000000000000000, 0.9659258262890683122, 1.000000000000000000, 0.9659258262890683122, 1.000000000000000000, 0.9659258262890683122, 1.000000000000000000, 0.9659258262890683122, 1.000000000000000000, 0.9659258262890683122, 1.000000000000000000, 0.9659258262890683122, 1.000000000000000000, 0.9659258262890683122, 1.000000000000000000, 0.9659258262890683122, 1.000000000000000000, 0.9659258262890683122, 1.000000000000000000, 0.9659258262890683122, 1.000000000000000000, 0.9659258262890683122, 1.000000000000000000, 0.9659258262890683122, 1.000000000000000000, 0.9659258262890683122, 1.000000000000000000, 0.9659258262890683122, 1.000000000000000000, 0.9659258262890683122, 1.000000000000000000, 0.9659258262890683122, 1.000000000000000000, 0.9659258262890683122, 1.000000000000000000, 0.9659258262890683122, 1.000000000000000000, 0.9659258262890683122, 1.000000000000000000, 0.9659258262890683122, 1.000000000000000000, 0.9659258262890683122, 1.000000000000000000, 0.9659258262890683122, 1.000000000000000000, 0.9659258262890683122, 1.000000000000000000, 0.9659258262890683122, 1.000000000000000000, 0.9659258262890683122, 1.000000000000000000, 0.9659258262890683122, 1.000000000000000000, 0.9659258262890683122, 1.000000000000000000, 0.9659258262890683122, 1.000000000000000000, 0.9659258262890683122, 1.000000000000000000, 0.9659258262890683122, 1.000000000000000000, 0.9659258262890683122, 1.000000000000000000, 0.9659258262890683122, 1.000000000000000000, 0.9659258262890683122, 1.000000000000000000, 0.9659258262890683122, 1.000000000000000000, 0.9659258262890683122, 1.000000000000000000, 0.9659258262890683122, 1.000000000000000000, 0.9659258262890683122, 1.000000000000000000, 0.9659258262890683122, 1.000000000000000000, 0.9659258262890683122, 1.000000000000000000, 0.9659258262890683122, 1.000000000000000000, 0.9659258262890683122, 1.000000000000000000, 0.9659258262890683122, 1.000000000000000000, 0.9659258262890683122, 1.000000000000000000, 0.9659258262890683122, 1.000000000000000000, 0.9659258262890683122, 1.000000000000000000, 0.9659258262890683122, 1.000000000000000000, 0.9659258262890683122, 1.000000000000000000, 0.9659258262890683122, 1.000000000000000000, 0.9659258262890683122, 1.000000000000000000, 0.9659258262890683122, 1.000000000000000000, 0.9659258262890683122, 1.000000000000000000, 0.9659258262890683122, 1.000000000000000000, 0.9659258262890683122, 1.000000000000000000, 0.9659258262890683122, 1.000000000000000000, 0.9659258262890683122, 1.000000000000000000, 0.9659258262890683122, 1.000000000000000000, 0.9659258262890683122, 1.000000000000000000, 0.9659258262890683122, 1.000000000000000000, 0.9659258262890683122, 1.000000000000000000, 0.9659258262890683122, 1.000000000000000000, 0.9659258262890683122, 1.000000000000000000, 0.9659258262890683122, 1.000000000000000000, 0.9659258262890683122, 1.000000000000000000, 0.9659258262890683122, 1.000000000000000000, 0.9659258262890683122, 1.000000000000000000, 0.9659258262890683122, 1.000000000000000000, 0.9659258262890683122, 1.000000000000000000, 0.9659258262890683122, 1.000000000000000000, 0.9659258262890683122, 1.000000000000000000, 0.9659258262890683122, 1.000000000000000000),
 ( 1.000000000000000000, 0.9659258262890683122, 1.000000000000000000, 0.9659258262890683122, 1.000000000000000000, 0.9659258262890683122, 1.000000000000000000, 0.9659258262890683122, 1.000000000000000000, 0.9659258262890683122, 1.000000000000000000, 0.9659258262890683122, 1.000000000000000000, 0.9659258262890683122, 1.000000000000000000, 0.9659258262890683122, 1.000000000000000000, 0.9659258262890683122, 1.000000000000000000, 0.9659258262890683122, 1.000000000000000000, 0.9659258262890683122, 1.000000000000000000, 0.9659258262890683122, 1.000000000000000000, 0.9659258262890683122, 1.000000000000000000, 0.9659258262890683122, 1.000000000000000000, 0.9659258262890683122, 1.000000000000000000, 0.9659258262890683122, 1.000000000000000000, 0.9659258262890683122, 1.000000000000000000, 0.9659258262890683122, 1.000000000000000000, 0.9659258262890683122, 1.000000000000000000, 0.9659258262890683122, 1.000000000000000000, 0.9659258262890683122, 1.000000000000000000, 0.9659258262890683122, 1.000000000000000000, 0.9659258262890683122, 1.000000000000000000, 0.9659258262890683122, 1.000000000000000000, 0.9659258262890683122, 1.000000000000000000, 0.9659258262890683122, 1.000000000000000000, 0.9659258262890683122, 1.000000000000000000, 0.9659258262890683122, 1.000000000000000000, 0.9659258262890683122, 1.000000000000000000, 0.9659258262890683122, 1.000000000000000000, 0.9659258262890683122, 1.000000000000000000, 0.9659258262890683122, 1.000000000000000000, 0.9659258262890683122, 1.000000000000000000, 0.9659258262890683122, 1.000000000000000000, 0.9659258262890683122, 1.000000000000000000, 0.9659258262890683122, 1.000000000000000000, 0.9659258262890683122, 1.000000000000000000, 0.9659258262890683122, 1.000000000000000000, 0.9659258262890683122, 1.000000000000000000, 0.9659258262890683122, 1.000000000000000000, 0.9659258262890683122, 1.000000000000000000, 0.9659258262890683122, 1.000000000000000000, 0.9659258262890683122, 1.000000000000000000, 0.9659258262890683122, 1.000000000000000000, 0.9659258262890683122, 1.000000000000000000, 0.9659258262890683122, 1.000000000000000000, 0.9659258262890683122, 1.000000000000000000, 0.9659258262890683122, 1.000000000000000000, 0.9659258262890683122, 1.000000000000000000, 0.9659258262890683122, 1.000000000000000000, 0.9659258262890683122, 1.000000000000000000, 0.9659258262890683122, 1.000000000000000000, 0.9659258262890683122, 1.000000000000000000, 0.9659258262890683122, 1.000000000000000000, 0.9659258262890683122, 1.000000000000000000, 0.9659258262890683122, 1.000000000000000000, 0.9659258262890683122, 1.000000000000000000, 0.9659258262890683122, 1.000000000000000000, 0.9659258262890683122, 1.000000000000000000, 0.9659258262890683122, 1.000000000000000000, 0.9659258262890683122, 1.000000000000000000, 0.9659258262890683122, 1.000000000000000000, 0.9659258262890683122, 1.000000000000000000, 0.9659258262890683122, 1.000000000000000000, 0.9659258262890683122, 1.000000000000000000, 0.9659258262890683122, 1.000000000000000000, 0.9659258262890683122, 1.000000000000000000, 0.9659258262890683122, 1.000000000000000000, 0.9659258262890683122, 1.000000000000000000, 0.9659258262890683122, 1.000000000000000000, 0.9659258262890683122, 1.000000000000000000, 0.9659258262890683122, 1.000000000000000000, 0.9659258262890683122, 1.000000000000000000, 0.9659258262890683122, 1.000000000000000000, 0.9659258262890683122, 1.000000000000000000, 0.9659258262890683122, 1.000000000000000000, 0.9659258262890683122, 1.000000000000000000, 0.9659258262890683122, 1.000000000000000000, 0.9659258262890683122, 1.000000000000000000, 0.9659258262890683122, 1.000000000000000000, 0.9659258262890683122, 1.000000000000000000, 0.9659258262890683122, 1.000000000000000000, 0.9659258262890683122, 1.000000000000000000, 0.9659258262890683122, 1.000000000000000000, 0.9659258262890683122, 1.000000000000000000, 0.9659258262890683122, 1.000000000000000000, 0.9659258262890683122, 1.000000000000000000, 0.9659258262890683122, 1.000000000000000000, 0.9659258262890683122, 1.000000000000000000, 0.9659258262890683122, 1.000000000000000000, 0.9659258262890683122, 1.000000000000000000, 0.9659258262890683122, 1.000000000000000000, 0.9659258262890683122, 1.000000000000000000, 0.9659258262890683122, 1.000000000000000000, 0.9659258262890683122, 1.000000000000000000, 0.9659258262890683122, 1.000000000000000000, 0.9659258262890683122, 1.000000000000000000, 0.9659258262890683122, 1.000000000000000000, 0.9659258262890683122, 1.000000000000000000, 0.9659258262890683122, 1.000000000000000000, 0.9659258262890683122, 1.000000000000000000, 0.9659258262890683122, 1.000000000000000000, 0.9659258262890683122, 1.000000000000000000, 0.9659258262890683122, 1.000000000000000000, 0.9659258262890683122, 1.000000000000000000, 0.9659258262890683122, 1.000000000000000000, 0.9659258262890683122, 1.000000000000000000, 0.9659258262890683122, 1.000000000000000000, 0.9659258262890683122, 1.000000000000000000, 0.9659258262890683122, 1.000000000000000000, 0.9659258262890683122, 1.000000000000000000, 0.9659258262890683122, 1.000000000000000000, 0.9659258262890683122, 1.000000000000000000, 0.9659258262890683122, 1.000000000000000000, 0.9659258262890683122, 1.000000000000000000, 0.9659258262890683122, 1.000000000000000000, 0.9659258262890683122, 1.000000000000000000, 0.9659258262890683122, 1.000000000000000000, 0.9659258262890683122, 1.000000000000000000, 0.9659258262890683122, 1.000000000000000000, 0.9659258262890683122, 1.000000000000000000, 0.9659258262890683122, 1.000000000000000000, 0.9659258262890683122, 1.000000000000000000, 0.9659258262890683122, 1.000000000000000000, 0.9659258262890683122, 1.000000000000000000, 0.9659258262890683122, 1.000000000000000000, 0.9659258262890683122, 1.000000000000000000, 0.9659258262890683122, 1.000000000000000000, 0.9659258262890683122, 1.000000000000000000, 0.9659258262890683122, 1.000000000000000000, 0.9659258262890683122, 1.000000000000000000, 0.9659258262890683122, 1.000000000000000000, 0.9659258262890683122, 1.000000000000000000, 0.9659258262890683122, 1.000000000000000000, 0.9659258262890683122, 1.000000000000000000, 0.9659258262890683122, 1.000000000000000000, 0.9659258262890683122, 1.000000000000000000, 0.9659258262890683122, 1.000000000000000000, 0.9659258262890683122, 1.000000000000000000, 0.9659258262890683122, 1.000000000000000000, 0.9659258262890683122, 1.000000000000000000, 0.9659258262890683122, 1.000000000000000000, 0.9659258262890683122, 1.000000000000000000, 0.9659258262890683122, 1.000000000000000000, 0.9659258262890683122, 1.000000000000000000, 0.9659258262890683122, 1.000000000000000000, 0.9659258262890683122, 1.000000000000000000, 0.9659258262890683122, 1.000000000000000000, 0.9659258262890683122, 1.000000000000000000, 0.9659258262890683122, 1.000000000000000000, 0.9659258262890683122, 1.000000000000000000, 0.9659258262890683122, 1.000000000000000000, 0.9659258262890683122, 1.000000000000000000, 0.9659258262890683122, 1.000000000000000000, 0.9659258262890683122, 1.000000000000000000, 0.9659258262890683122, 1.000000000000000000, 0.9659258262890683122, 1.000000000000000000, 0.9659258262890683122, 1.000000000000000000, 0.9659258262890683122, 1.000000000000000000, 0.9659258262890683122, 1.000000000000000000, 0.9659258262890683122, 1.000000000000000000, 0.9659258262890683122, 1.000000000000000000) ) ) 
 REPRESENTATION_ITEM ( '' )  SURFACE ( )  );
#61815 = CARTESIAN_POINT ( 'NONE',  ( 18.52753015748618282, 28.92559781766745175, -4.923371831947291888 ) ) ;
#61816 = CARTESIAN_POINT ( 'NONE',  ( 3.591859063236761518, 9.956968003263753531, 11.09922568453594849 ) ) ;
#61817 = CARTESIAN_POINT ( 'NONE',  ( -5.815502996284770632, 0.2306972965111892260, -13.76292046016129866 ) ) ;
#61818 = DIRECTION ( 'NONE',  ( -0.9981347984218673641, 0.000000000000000000, 0.06104853953484969120 ) ) ;
#61819 = PLANE ( 'NONE',  #34791 ) ;
#61820 =( BOUNDED_CURVE ( )  B_SPLINE_CURVE ( 2, ( #80766, #88756, #41797, #73746, #34759, #95776, #65748, #64265, #81737 ),
 .UNSPECIFIED., .F., .F. ) 
 B_SPLINE_CURVE_WITH_KNOTS ( ( 3, 2, 2, 2, 3 ),
 ( 0.6901409369402313754, 0.6904761904761904656, 0.6964285714285713969, 0.7023809523809523281, 0.7027162059169114183 ),
 .UNSPECIFIED. ) 
 CURVE ( )  GEOMETRIC_REPRESENTATION_ITEM ( )  RATIONAL_B_SPLINE_CURVE ( ( 0.9963778908391764944, 0.9980808541467923733, 1.000000000000000000, 0.9659258262890682012, 1.000000000000000000, 0.9659258262890682012, 1.000000000000000000, 0.9980808541467923733, 0.9963778908391766054 ) ) 
 REPRESENTATION_ITEM ( '' )  );
#61821 = CARTESIAN_POINT ( 'NONE',  ( 22.26659068614894466, 8.887082168247300018, 7.082119434687054849 ) ) ;
#61822 = CARTESIAN_POINT ( 'NONE',  ( 10.00000000000000178, 37.25893115100078745, 9.846743663894594434 ) ) ;
#61823 = CYLINDRICAL_SURFACE ( 'NONE', #45793, 3.000000000000000000 ) ;
#61824 = ORIENTED_EDGE ( 'NONE', *, *, #30600, .F. ) ;
#61825 = CARTESIAN_POINT ( 'NONE',  ( 20.36894250292379382, 48.67874883491396076, 10.36894250292379205 ) ) ;
#61826 = CARTESIAN_POINT ( 'NONE',  ( 0.1532563361054082862, 26.21726448433411605, 2.638427012816831674 ) ) ;
#61828 = CARTESIAN_POINT ( 'NONE',  ( -0.1491070598754174470, 61.94583914210339515, -4.500000000000001776 ) ) ;
#61827 = DIRECTION ( 'NONE',  ( -0.000000000000000000, -0.000000000000000000, 1.000000000000000000 ) ) ;
#61829 = CARTESIAN_POINT ( 'NONE',  ( 0.5774900079438590739, 42.64701867748816966, -5.440088680355550821 ) ) ;
#61830 = CARTESIAN_POINT ( 'NONE',  ( 3.591859063236761518, 49.95696800326375353, 11.09922568453594849 ) ) ;
#61831 = CARTESIAN_POINT ( 'NONE',  ( 10.00000000000000178, 24.31368534415484106, 10.88017736071110342 ) ) ;
#61832 = CARTESIAN_POINT ( 'NONE',  ( 13.43411237798106583, 52.66530133659708213, -12.81628187352647252 ) ) ;
#61833 = CARTESIAN_POINT ( 'NONE',  ( 2.791683348922240793, 66.63393115100079456, 7.208316651077764092 ) ) ;
#61834 = CARTESIAN_POINT ( 'NONE',  ( 1.472469842513823179, 1.425597817667451528, 4.923371831947296329 ) ) ;
#61835 = VERTEX_POINT ( 'NONE', #84112 ) ;
#61836 = CARTESIAN_POINT ( 'NONE',  ( 3.640395162852214650, 89.00000000000000000, 5.000000000000000000 ) ) ;
#61837 = CARTESIAN_POINT ( 'NONE',  ( 8.880000000000020322, 80.07179676972448590, 4.250000000000000000 ) ) ;
#61838 = CARTESIAN_POINT ( 'NONE',  ( 6.204703633549690345, 60.76208216824730357, -14.16423886937410259 ) ) ;
#61839 = CARTESIAN_POINT ( 'NONE',  ( 17.08211943468705130, 18.47041550158063572, 12.26659068614894998 ) ) ;
#61840 = CARTESIAN_POINT ( 'NONE',  ( -0.8801773607111009756, 18.06368534415484106, 1.068504757029289695E-15 ) ) ;
#61841 = VECTOR ( 'NONE', #93519, 1000.000000000000114 ) ;
#61842 = CARTESIAN_POINT ( 'NONE',  ( 20.88017736071110875, 40.77201867748818387, -2.915334737309920765 ) ) ;
#61843 = CARTESIAN_POINT ( 'NONE',  ( 6.879999999999995453, 43.00000000000000000, -6.500000000000000888 ) ) ;
#61844 = DIRECTION ( 'NONE',  ( -0.000000000000000000, -0.000000000000000000, -1.000000000000000000 ) ) ;
#61845 = CARTESIAN_POINT ( 'NONE',  ( -0.8801773607110991993, 67.85535201082151957, -2.915334737309923874 ) ) ;
#61846 = CARTESIAN_POINT ( 'NONE',  ( 4.559911319644449179, 58.89701867748817676, 9.422509992056141925 ) ) ;
#61847 = CARTESIAN_POINT ( 'NONE',  ( 22.81628187352648496, 26.83196800326374998, -3.434112377981050290 ) ) ;
#61848 = LINE ( 'NONE', #24370, #15589 ) ;
#61849 = CARTESIAN_POINT ( 'NONE',  ( 14.92337183194729988, 4.342264484334117824, -8.527530157486177487 ) ) ;
#61850 = CARTESIAN_POINT ( 'NONE',  ( 5.076628168052704559, 30.17559781766745175, -8.527530157486179263 ) ) ;
#61851 = CIRCLE ( 'NONE', #76204, 0.5000000000000004441 ) ;
#61852 = EDGE_CURVE ( 'NONE', #11368, #60663, #30061, .T. ) ;
#61853 = CARTESIAN_POINT ( 'NONE',  ( 4.559911319644449179, 12.23035201082150536, -9.422509992056141925 ) ) ;
#61854 = VECTOR ( 'NONE', #77168, 1000.000000000000000 ) ;
#61855 = VECTOR ( 'NONE', #14302, 1000.000000000000000 ) ;
#61856 = CARTESIAN_POINT ( 'NONE',  ( -2.816281873526473856, 29.33196800326376064, 3.434112377981055619 ) ) ;
#61857 = CARTESIAN_POINT ( 'NONE',  ( 2.791683348922240793, 6.633931151000785675, 7.208316651077764092 ) ) ;
#61858 = DIRECTION ( 'NONE',  ( -1.000000000000000000, 0.000000000000000000, 0.000000000000000000 ) ) ;
#61859 = CARTESIAN_POINT ( 'NONE',  ( 19.84674366389459266, 58.30059781766745886, 2.638427012816836559 ) ) ;
#61860 = CARTESIAN_POINT ( 'NONE',  ( 0.1532563361054083140, 31.00893115100078390, 1.131784320476157264E-15 ) ) ;
#61861 = CARTESIAN_POINT ( 'NONE',  ( 24.16423886937410614, 14.51208216824730179, -3.795296366450302550 ) ) ;
#61862 = CARTESIAN_POINT ( 'NONE',  ( 12.91533473730992121, 29.52201867748817321, 10.88017736071110164 ) ) ;
#61863 = CARTESIAN_POINT ( 'NONE',  ( 15.44008868035555260, 9.730352010821505360, 9.422509992056143702 ) ) ;
#61864 = CARTESIAN_POINT ( 'NONE',  ( -0.8801773607111009756, 43.06368534415484106, 1.068504757029289695E-15 ) ) ;
#61865 = CARTESIAN_POINT ( 'NONE',  ( 20.88017736071110875, 30.77201867748816966, -2.915334737309920765 ) ) ;
#61866 = ORIENTED_EDGE ( 'NONE', *, *, #96714, .T. ) ;
#61867 = CARTESIAN_POINT ( 'NONE',  ( 22.81628187352647785, 36.41530133659707502, 3.434112377981063169 ) ) ;
#61868 = CARTESIAN_POINT ( 'NONE',  ( -0.8801773607111009756, 38.06368534415484106, 1.068504757029289695E-15 ) ) ;
#61869 = ORIENTED_EDGE ( 'NONE', *, *, #67877, .T. ) ;
#61870 = CARTESIAN_POINT ( 'NONE',  ( 6.565887622018943937, 55.16530133659709634, 12.81628187352647430 ) ) ;
#61871 = CARTESIAN_POINT ( 'NONE',  ( -0.8801773607110991993, 47.85535201082150536, -2.915334737309923874 ) ) ;
#61872 = ORIENTED_EDGE ( 'NONE', *, *, #26849, .T. ) ;
#61873 = CARTESIAN_POINT ( 'NONE',  ( 20.88017736071110875, 45.77201867748816966, -2.915334737309920765 ) ) ;
#61874 = CARTESIAN_POINT ( 'NONE',  ( 4.573751236499521866, -6.413519960490759786, 4.000000000000000000 ) ) ;
#61875 = EDGE_CURVE ( 'NONE', #73541, #14052, #148, .T. ) ;
#61876 = CARTESIAN_POINT ( 'NONE',  ( 13.79529636645031943, 60.34541550158063927, -14.16423886937409904 ) ) ;
#61877 = CARTESIAN_POINT ( 'NONE',  ( 15.44008868035555260, 64.73035201082151957, 9.422509992056143702 ) ) ;
#61878 = LINE ( 'NONE', #98446, #92956 ) ;
#61879 = AXIS2_PLACEMENT_3D ( 'NONE', #87371, #19854, #57848 ) ;
#61880 = CARTESIAN_POINT ( 'NONE',  ( 7.361572987183169658, -0.03273551566588185635, -9.846743663894592657 ) ) ;
#61881 = DIRECTION ( 'NONE',  ( 0.000000000000000000, -1.000000000000000000, 0.000000000000000000 ) ) ;
#61882 = CARTESIAN_POINT ( 'NONE',  ( 19.84674366389459266, 28.30059781766745886, 2.638427012816836559 ) ) ;
#61883 = ORIENTED_EDGE ( 'NONE', *, *, #51385, .T. ) ;
#61884 = CARTESIAN_POINT ( 'NONE',  ( 17.20831665107776587, 37.88393115100078745, 7.208316651077764980 ) ) ;
#61885 = CARTESIAN_POINT ( 'NONE',  ( 2.035157376598824452, 38.68868534415483396, 7.964842623401179544 ) ) ;
#61886 = CARTESIAN_POINT ( 'NONE',  ( 0.1532563361054082862, 41.21726448433411605, 2.638427012816831674 ) ) ;
#61887 = CARTESIAN_POINT ( 'NONE',  ( 21.09922568453594849, 16.20696800326375353, 6.408140936763242479 ) ) ;
#61889 = CARTESIAN_POINT ( 'NONE',  ( 0.000000000000000000, 15.00000000000000000, 0.000000000000000000 ) ) ;
#61888 = CARTESIAN_POINT ( 'NONE',  ( 19.80427997160308706, 2.757339608395440678, -6.500000000000000000 ) ) ;
#61890 = CARTESIAN_POINT ( 'NONE',  ( -0.8801773607111009756, 43.06368534415484106, 1.068504757029289695E-15 ) ) ;
#61891 = CARTESIAN_POINT ( 'NONE',  ( 17.08211943468705130, 63.47041550158063927, 12.26659068614894998 ) ) ;
#61892 = CIRCLE ( 'NONE', #46001, 3.000000000000000888 ) ;
#61893 = CARTESIAN_POINT ( 'NONE',  ( 22.81628187352647785, 21.62363466993041783, 6.195893100308588602E-16 ) ) ;
#61894 = CARTESIAN_POINT ( 'NONE',  ( 17.39651004071842522, 24.08210964143329491, -6.499999999999992895 ) ) ;
#61895 = ORIENTED_EDGE ( 'NONE', *, *, #16177, .F. ) ;
#61896 = CARTESIAN_POINT ( 'NONE',  ( 16.40814093676323893, 30.79030133659708923, 11.09922568453595026 ) ) ;
#61897 = CARTESIAN_POINT ( 'NONE',  ( 20.88017736071110164, 20.35535201082150891, 2.915334737309930979 ) ) ;
#61898 = CARTESIAN_POINT ( 'NONE',  ( 0.5774900079438590739, 57.64701867748817676, -5.440088680355550821 ) ) ;
#61899 = ORIENTED_EDGE ( 'NONE', *, *, #78556, .T. ) ;
#61900 = ORIENTED_EDGE ( 'NONE', *, *, #19665, .T. ) ;
#61901 = AXIS2_PLACEMENT_3D ( 'NONE', #34194, #57198, #73182 ) ;
#61902 = EDGE_CURVE ( 'NONE', #11978, #51199, #88516, .T. ) ;
#61903 = CARTESIAN_POINT ( 'NONE',  ( 0.1532563361054083140, 6.008931151000784787, 1.131784320476157264E-15 ) ) ;
#61904 = CARTESIAN_POINT ( 'NONE',  ( 19.84674366389459266, 48.30059781766745175, 2.638427012816836559 ) ) ;
#61905 = CARTESIAN_POINT ( 'NONE',  ( 5.076628168052704559, 40.17559781766745175, -8.527530157486179263 ) ) ;
#61906 = CARTESIAN_POINT ( 'NONE',  ( 0.000000000000000000, 14.49999999999999822, 0.000000000000000000 ) ) ;
#61907 = CARTESIAN_POINT ( 'NONE',  ( 2.791683348922240793, 31.63393115100078745, 7.208316651077764092 ) ) ;
#61908 = CARTESIAN_POINT ( 'NONE',  ( 14.94699059465105684, 14.63606911935685595, -1.259949270174804736 ) ) ;
#61909 = DIRECTION ( 'NONE',  ( -0.9961946980917462113, 0.08715574274765140739, -0.000000000000000000 ) ) ;
#61910 = EDGE_CURVE ( 'NONE', #74651, #87105, #25315, .T. ) ;
#61913 = CARTESIAN_POINT ( 'NONE',  ( 12.03829478939421982, 8.656676720938946507E-16, 8.307695547791484003 ) ) ;
#61912 = PRESENTATION_LAYER_ASSIGNMENT (  '', '', ( #71513 ) ) ;
#61911 = CARTESIAN_POINT ( 'NONE',  ( 0.1532563361054083140, 16.00893115100078390, 1.131784320476157264E-15 ) ) ;
#61914 = DIRECTION ( 'NONE',  ( 1.000000000000000000, -0.000000000000000000, -0.000000000000000000 ) ) ;
#61916 = ORIENTED_EDGE ( 'NONE', *, *, #72024, .T. ) ;
#61915 = CARTESIAN_POINT ( 'NONE',  ( 12.63842701281683034, 47.46726448433412315, 9.846743663894596210 ) ) ;
#61917 = VECTOR ( 'NONE', #25144, 1000.000000000000000 ) ;
#61918 = CARTESIAN_POINT ( 'NONE',  ( 2.815433093577122126, 0.5000000000000004441, -14.73340885523749932 ) ) ;
#61919 = CARTESIAN_POINT ( 'NONE',  ( 0.6178305044545818747, 8.498634669930421381, -9.382169495545419124 ) ) ;
#61920 = CARTESIAN_POINT ( 'NONE',  ( 10.00000000000000000, 56.81368534415484106, -10.88017736071110342 ) ) ;
#61921 = CARTESIAN_POINT ( 'NONE',  ( 2.917880565312950480, 45.97041550158063927, -12.26659068614894821 ) ) ;
#61922 = DIRECTION ( 'NONE',  ( -0.000000000000000000, 1.000000000000000000, 0.000000000000000000 ) ) ;
#61923 = DIRECTION ( 'NONE',  ( 1.000000000000000000, 0.000000000000000000, 0.000000000000000000 ) ) ;
#61924 = CARTESIAN_POINT ( 'NONE',  ( 2.917880565312948704, 42.63708216824729647, 12.26659068614894643 ) ) ;
#61925 = EDGE_CURVE ( 'NONE', #16030, #15047, #49621, .T. ) ;
#61926 = CARTESIAN_POINT ( 'NONE',  ( 24.16423886937409904, 54.09541550158063217, 3.795296366450317205 ) ) ;
#61927 = CARTESIAN_POINT ( 'NONE',  ( 6.204703633549690345, 22.84541550158062861, 14.16423886937410082 ) ) ;
#61929 = DIRECTION ( 'NONE',  ( 0.000000000000000000, -1.000000000000000000, 0.000000000000000000 ) ) ;
#61928 = CARTESIAN_POINT ( 'NONE',  ( 13.79529636645030344, 23.26208216824730002, 14.16423886937410614 ) ) ;
#61930 = LINE ( 'NONE', #75464, #3624 ) ;
#61932 = CARTESIAN_POINT ( 'NONE',  ( 7.361572987183170547, 42.05059781766745886, 9.846743663894590881 ) ) ;
#61931 = CARTESIAN_POINT ( 'NONE',  ( 4.395712687476568625, -0.8323168404034876344, 2.500000000000000000 ) ) ;
#61933 = CARTESIAN_POINT ( 'NONE',  ( 20.88017736071110164, 20.35535201082150891, 2.915334737309930979 ) ) ;
#61934 = DIRECTION ( 'NONE',  ( 0.000000000000000000, 0.000000000000000000, 1.000000000000000000 ) ) ;
#61935 = CARTESIAN_POINT ( 'NONE',  ( -0.1503990784575328643, 70.00000000000000000, 6.262539305110068177 ) ) ;
#61936 = CARTESIAN_POINT ( 'NONE',  ( 20.00000000000000000, 89.79522682798472033, -5.338983947147861286 ) ) ;
#61937 = CARTESIAN_POINT ( 'NONE',  ( 19.84674366389459266, 33.71726448433410894, -2.638427012816827677 ) ) ;
#61938 = CARTESIAN_POINT ( 'NONE',  ( 19.38216949554541202, 60.99863466993042493, 9.382169495545424454 ) ) ;
#61939 = B_SPLINE_CURVE_WITH_KNOTS ( 'NONE', 3,
 ( #34021, #96031, #74001, #20521, #27515, #58007 ),
 .UNSPECIFIED., .F., .F.,
 ( 4, 2, 4 ),
 ( 3.409110551494655498E-05, 0.0004400426677367920468, 0.0008459942299586376132 ),
 .UNSPECIFIED. ) ;
#61940 = CARTESIAN_POINT ( 'NONE',  ( -14.16423886937409726, -7.987917831752695541, 3.795296366450320757 ) ) ;
#61941 = CARTESIAN_POINT ( 'NONE',  ( 0.1532563361054082862, 46.21726448433411605, 2.638427012816831674 ) ) ;
#61942 = CARTESIAN_POINT ( 'NONE',  ( 17.20831665107776587, 49.13393115100078745, -7.208316651077762316 ) ) ;
#61943 = CARTESIAN_POINT ( 'NONE',  ( -2.266590686148945544, 42.22041550158063217, 7.082119434687048631 ) ) ;
#61944 = ORIENTED_EDGE ( 'NONE', *, *, #7702, .F. ) ;
#61945 = CARTESIAN_POINT ( 'NONE',  ( 10.00000000000000000, 15.55374883491396787, -14.16423886937410082 ) ) ;
#61946 = DIRECTION ( 'NONE',  ( 0.000000000000000000, 1.000000000000000000, 0.000000000000000000 ) ) ;
#61948 = DIRECTION ( 'NONE',  ( -0.2334453638558956767, 0.000000000000000000, -0.9723699203976788885 ) ) ;
#61947 = CARTESIAN_POINT ( 'NONE',  ( 19.05914839598885635, 44.96693863883977116, 6.499999999999962697 ) ) ;
#61949 = CARTESIAN_POINT ( 'NONE',  ( 17.96484262340118221, 4.938685344154837509, 7.964842623401181321 ) ) ;
#61950 = CARTESIAN_POINT ( 'NONE',  ( 6.565887622018943937, 5.165301336597086568, 12.81628187352647430 ) ) ;
#61951 = CARTESIAN_POINT ( 'NONE',  ( -0.1503990784575282014, 57.22266099184919597, -6.262539305110077947 ) ) ;
#61952 = CARTESIAN_POINT ( 'NONE',  ( 0.5774900079438607392, 68.48035201082150536, 5.440088680355550821 ) ) ;
#61953 = CARTESIAN_POINT ( 'NONE',  ( 20.32896413005680714, 42.60497603579417358, -5.963430220938276349 ) ) ;
#61954 = CARTESIAN_POINT ( 'NONE',  ( -0.1038446121089120627, 14.24302437010793376, -6.337995344473772441 ) ) ;
#61955 = CARTESIAN_POINT ( 'NONE',  ( 0.000000000000000000, 0.5000000000000004441, 0.000000000000000000 ) ) ;
#61956 = CARTESIAN_POINT ( 'NONE',  ( 20.36894250292379738, 64.92874883491397497, -10.36894250292379027 ) ) ;
#61957 = DIRECTION ( 'NONE',  ( -0.000000000000000000, -0.000000000000000000, 1.000000000000000000 ) ) ;
#61958 = CARTESIAN_POINT ( 'NONE',  ( 12.91533473730993009, 21.60535201082150536, -10.88017736071109987 ) ) ;
#61959 = CARTESIAN_POINT ( 'NONE',  ( -0.8801773607111008646, 18.27201867748817321, 2.915334737309923430 ) ) ;
#61960 = CARTESIAN_POINT ( 'NONE',  ( 5.076628168052703671, 61.84226448433412315, 8.527530157486179263 ) ) ;
#61961 = CARTESIAN_POINT ( 'NONE',  ( 5.076628168052703671, 51.84226448433412315, 8.527530157486179263 ) ) ;
#61962 = CARTESIAN_POINT ( 'NONE',  ( 0.6178305044545818747, 58.49863466993042493, -9.382169495545419124 ) ) ;
#61963 = DIRECTION ( 'NONE',  ( 0.000000000000000000, 1.000000000000000000, 0.000000000000000000 ) ) ;
#61964 = ORIENTED_EDGE ( 'NONE', *, *, #93389, .T. ) ;
#61965 = CARTESIAN_POINT ( 'NONE',  ( 17.96484262340118221, 31.18868534415483751, -7.964842623401177768 ) ) ;
#61966 = EDGE_CURVE ( 'NONE', #44781, #69690, #79977, .T. ) ;
#61967 = CARTESIAN_POINT ( 'NONE',  ( 10.00000000000000000, 17.87363466993041783, -12.81628187352647608 ) ) ;
#61968 = CARTESIAN_POINT ( 'NONE',  ( -0.2418659066527727997, 54.26028685723174050, -6.114288769123041867 ) ) ;
#61969 = AXIS2_PLACEMENT_3D ( 'NONE', #58930, #74413, #66926 ) ;
#61970 = CARTESIAN_POINT ( 'NONE',  ( 14.92337183194729633, 62.67559781766745886, 8.527530157486181039 ) ) ;
#61971 = ADVANCED_FACE ( 'NONE', ( #92096 ), #37629, .T. ) ;
#61972 = CARTESIAN_POINT ( 'NONE',  ( 17.96484262340118221, 49.93868534415484106, 7.964842623401181321 ) ) ;
#61973 = CARTESIAN_POINT ( 'NONE',  ( 21.09922568453594849, 26.20696800326375353, 6.408140936763242479 ) ) ;
#61975 = CARTESIAN_POINT ( 'NONE',  ( -0.1503990784575294781, 48.10158574516642460, 6.262539305110072618 ) ) ;
#61974 = CARTESIAN_POINT ( 'NONE',  ( -0.8801773607110991993, 62.85535201082150536, -2.915334737309923874 ) ) ;
#61976 = CARTESIAN_POINT ( 'NONE',  ( 0.1143410931637273975, 50.21691075486305067, 6.480892540919861666 ) ) ;
#61977 = CARTESIAN_POINT ( 'NONE',  ( -2.816281873526471635, 63.91530133659708923, -3.434112377981056508 ) ) ;
#61978 = ORIENTED_EDGE ( 'NONE', *, *, #51562, .T. ) ;
#61979 = CARTESIAN_POINT ( 'NONE',  ( 19.42250999205614548, 50.98035201082151247, -5.440088680355545492 ) ) ;
#61981 = CARTESIAN_POINT ( 'NONE',  ( 20.36894250292379738, 19.92874883491396787, -10.36894250292379027 ) ) ;
#61980 = CARTESIAN_POINT ( 'NONE',  ( -1.099225684535947600, 53.70696800326376064, -6.408140936763238038 ) ) ;
#61982 = PRESENTATION_LAYER_ASSIGNMENT (  '', '', ( #47644 ) ) ;
#61983 = CYLINDRICAL_SURFACE ( 'NONE', #51352, 15.00000000000000000 ) ;
#61984 = CARTESIAN_POINT ( 'NONE',  ( 5.076628168052704559, 25.17559781766745175, -8.527530157486179263 ) ) ;
#61985 = DIRECTION ( 'NONE',  ( 0.000000000000000000, -1.000000000000000000, 0.000000000000000000 ) ) ;
#61986 = CARTESIAN_POINT ( 'NONE',  ( -4.164238869374099927, 62.01208216824728936, 3.795296366450308767 ) ) ;
#61987 = EDGE_LOOP ( 'NONE', ( #85527, #46735, #25969, #71259 ) ) ;
#61988 = CARTESIAN_POINT ( 'NONE',  ( 17.96484262340118221, 4.938685344154837509, 7.964842623401181321 ) ) ;
#61989 = AXIS2_PLACEMENT_3D ( 'NONE', #53258, #45769, #30249 ) ;
#61990 = CARTESIAN_POINT ( 'NONE',  ( 19.42250999205614193, 10.14701867748816966, 5.440088680355555262 ) ) ;
#61991 = DIRECTION ( 'NONE',  ( -0.000000000000000000, -1.000000000000000000, -0.000000000000000000 ) ) ;
#61992 = ORIENTED_EDGE ( 'NONE', *, *, #57443, .T. ) ;
#61993 = CARTESIAN_POINT ( 'NONE',  ( -0.8801773607111008646, 8.272018677488171434, 2.915334737309923430 ) ) ;
#61994 = CARTESIAN_POINT ( 'NONE',  ( 20.88017736071110519, 15.56368534415483751, 2.639326808657452039E-16 ) ) ;
#61995 = CARTESIAN_POINT ( 'NONE',  ( 0.1532563361054100626, 40.80059781766745886, -2.638427012816831230 ) ) ;
#61996 = ADVANCED_FACE ( 'NONE', ( #17099 ), #47582, .F. ) ;
#61997 = CARTESIAN_POINT ( 'NONE',  ( 13.43411237798106583, 42.66530133659707502, -12.81628187352647252 ) ) ;
#61998 = CARTESIAN_POINT ( 'NONE',  ( 64.56412365047461321, 11.49999999999999467, -10.00000000000000000 ) ) ;
#61999 = CARTESIAN_POINT ( 'NONE',  ( -2.266590686148945544, 26.38708216824730357, -7.082119434687050408 ) ) ;
#62000 = CARTESIAN_POINT ( 'NONE',  ( 20.88017736071110875, 25.77201867748816966, -2.915334737309920765 ) ) ;
#62001 = CARTESIAN_POINT ( 'NONE',  ( 20.88017736071110519, 5.563685344154838397, 2.639326808657452039E-16 ) ) ;
#62002 = CARTESIAN_POINT ( 'NONE',  ( 17.20831665107776587, 42.88393115100077324, 7.208316651077764980 ) ) ;
#62003 = LINE ( 'NONE', #77015, #97141 ) ;
#62004 = CARTESIAN_POINT ( 'NONE',  ( 0.1532563361054082862, 26.21726448433411605, 2.638427012816831674 ) ) ;
#62005 = ADVANCED_FACE ( 'NONE', ( #34032 ), #2605, .F. ) ;
#62006 = SURFACE_STYLE_USAGE ( .BOTH. , #570 ) ;
#62007 = CARTESIAN_POINT ( 'NONE',  ( 12.81628187352647608, -38.58469866340291077, 3.434112377981052511 ) ) ;
#62008 = VERTEX_POINT ( 'NONE', #85090 ) ;
#62009 = CARTESIAN_POINT ( 'NONE',  ( 0.5774900079438590739, 2.647018677488170990, -5.440088680355550821 ) ) ;
#62010 = CARTESIAN_POINT ( 'NONE',  ( 2.035157376598824452, 63.68868534415484106, 7.964842623401179544 ) ) ;
#62011 = CARTESIAN_POINT ( 'NONE',  ( 17.20831665107776587, 52.88393115100078035, 7.208316651077764980 ) ) ;
#62013 = CARTESIAN_POINT ( 'NONE',  ( 0.5774900079438607392, 43.48035201082151247, 5.440088680355550821 ) ) ;
#62012 = CARTESIAN_POINT ( 'NONE',  ( 4.559911319644449179, 37.23035201082150536, -9.422509992056141925 ) ) ;
#62015 = CARTESIAN_POINT ( 'NONE',  ( 21.09922568453594849, 26.20696800326375353, 6.408140936763242479 ) ) ;
#62014 = CARTESIAN_POINT ( 'NONE',  ( 20.88017736071110875, 5.772018677488170546, -2.915334737309920765 ) ) ;
#62016 = CARTESIAN_POINT ( 'NONE',  ( -4.164238869374099927, 22.01208216824730357, 3.795296366450308767 ) ) ;
#62017 = VERTEX_POINT ( 'NONE', #9089 ) ;
#62018 = CARTESIAN_POINT ( 'NONE',  ( 21.09922568453595559, 47.04030133659708923, -6.408140936763230044 ) ) ;
#62019 = ORIENTED_EDGE ( 'NONE', *, *, #90552, .F. ) ;
#62020 = CARTESIAN_POINT ( 'NONE',  ( 1.472469842513823179, 41.42559781766745886, 4.923371831947296329 ) ) ;
#62021 = CARTESIAN_POINT ( 'NONE',  ( 15.44008868035555260, 19.73035201082150536, 9.422509992056143702 ) ) ;
#62022 = CARTESIAN_POINT ( 'NONE',  ( -0.8801773607110991993, 22.85535201082150181, -2.915334737309923874 ) ) ;
#62023 = VERTEX_POINT ( 'NONE', #64036 ) ;
#62024 = CARTESIAN_POINT ( 'NONE',  ( 20.88017736071110519, 60.56368534415484106, 2.639326808657452039E-16 ) ) ;
#62025 = FACE_OUTER_BOUND ( 'NONE', #88566, .T. ) ;
#62026 = CARTESIAN_POINT ( 'NONE',  ( 5.963430220938287007, 6.354976035794178024, 10.32896413005679825 ) ) ;
#62027 = CARTESIAN_POINT ( 'NONE',  ( 18.52753015748617571, 8.092264484334117824, 4.923371831947298993 ) ) ;
#62028 = CARTESIAN_POINT ( 'NONE',  ( 12.91533473730993009, 61.60535201082150536, -10.88017736071109987 ) ) ;
#62029 = ADVANCED_FACE ( 'NONE', ( #55068 ), #62568, .F. ) ;
#62030 = CARTESIAN_POINT ( 'NONE',  ( -46.94000000000001194, 100.5254250115999923, 8.865097534344174690 ) ) ;
#62032 = ORIENTED_EDGE ( 'NONE', *, *, #51544, .T. ) ;
#62031 = CARTESIAN_POINT ( 'NONE',  ( 0.1532563361054082862, 6.217264484334118713, 2.638427012816831674 ) ) ;
#62033 = CARTESIAN_POINT ( 'NONE',  ( 2.791683348922240793, 41.63393115100078745, 7.208316651077764092 ) ) ;
#62034 = ORIENTED_EDGE ( 'NONE', *, *, #45259, .T. ) ;
#62035 = VERTEX_POINT ( 'NONE', #85586 ) ;
#62036 = LINE ( 'NONE', #92536, #1142 ) ;
#62037 = DIRECTION ( 'NONE',  ( 0.000000000000000000, 0.000000000000000000, -1.000000000000000000 ) ) ;
#62038 = CARTESIAN_POINT ( 'NONE',  ( 0.6178305044545818747, 53.49863466993041072, -9.382169495545419124 ) ) ;
#62039 = CARTESIAN_POINT ( 'NONE',  ( -0.3689425029237898834, 1.178748834913967869, -10.36894250292378850 ) ) ;
#62040 = CARTESIAN_POINT ( 'NONE',  ( 22.26659068614895176, 24.72041550158063572, -7.082119434687042414 ) ) ;
#62041 = MECHANICAL_DESIGN_GEOMETRIC_PRESENTATION_REPRESENTATION (  '', ( #44496 ), #33275 ) ;
#62042 = PRESENTATION_STYLE_ASSIGNMENT (( #78043 ) ) ;
#62044 = CARTESIAN_POINT ( 'NONE',  ( 7.084665262690076126, 62.02201867748816966, -10.88017736071110164 ) ) ;
#62043 = CARTESIAN_POINT ( 'NONE',  ( 20.15039907845753930, 70.00000000000000000, 6.262539305110068177 ) ) ;
#62045 = CARTESIAN_POINT ( 'NONE',  ( 17.96484262340118221, 24.93868534415484461, 7.964842623401181321 ) ) ;
#62046 = CARTESIAN_POINT ( 'NONE',  ( 1.274849032794280523, 68.57228050351031357, 6.499999999999960032 ) ) ;
#62047 = ORIENTED_EDGE ( 'NONE', *, *, #16828, .T. ) ;
#62048 = CARTESIAN_POINT ( 'NONE',  ( 10.00000000000000000, 4.758931151000784787, -9.846743663894594434 ) ) ;
#62049 = CARTESIAN_POINT ( 'NONE',  ( 6.565887622018943937, 38.08196800326376064, -12.81628187352647608 ) ) ;
#62050 = CARTESIAN_POINT ( 'NONE',  ( 18.52753015748618282, 23.92559781766745530, -4.923371831947291888 ) ) ;
#62051 = AXIS2_PLACEMENT_3D ( 'NONE', #49098, #41622, #26586 ) ;
#62052 = CARTESIAN_POINT ( 'NONE',  ( -0.2538888227776796569, 70.00000000000000000, -6.092555545976966691 ) ) ;
#62053 = CARTESIAN_POINT ( 'NONE',  ( 22.81628187352647785, 16.41530133659708923, 3.434112377981063169 ) ) ;
#62054 = AXIS2_PLACEMENT_3D ( 'NONE', #88220, #28213, #41279 ) ;
#62055 = CARTESIAN_POINT ( 'NONE',  ( 4.219999999999999751, 10.25000000000000000, -2.750000000000000000 ) ) ;
#62056 = CARTESIAN_POINT ( 'NONE',  ( 7.361572987183170547, 7.050597817667451750, 9.846743663894590881 ) ) ;
#62057 = VERTEX_POINT ( 'NONE', #9582 ) ;
#62058 = CARTESIAN_POINT ( 'NONE',  ( 0.5774900079438607392, 23.48035201082150536, 5.440088680355550821 ) ) ;
#62059 = CARTESIAN_POINT ( 'NONE',  ( -4.164238869374099039, 36.80374883491396787, 8.674139862899312516E-16 ) ) ;
#62060 = CARTESIAN_POINT ( 'NONE',  ( 7.361572987183170547, 42.05059781766745886, 9.846743663894590881 ) ) ;
#62061 = ADVANCED_FACE ( 'NONE', ( #48553 ), #40083, .F. ) ;
#62062 = CARTESIAN_POINT ( 'NONE',  ( -0.8801773607111009756, 63.06368534415484106, 1.068504757029289695E-15 ) ) ;
#62064 = CARTESIAN_POINT ( 'NONE',  ( -7.045329894599615450, -66.66420243593404393, -2.750000000000000444 ) ) ;
#62063 = CARTESIAN_POINT ( 'NONE',  ( 3.591859063236763294, 58.29030133659708923, -11.09922568453595026 ) ) ;
#62065 = CARTESIAN_POINT ( 'NONE',  ( 0.5774900079438590739, 22.64701867748817321, -5.440088680355550821 ) ) ;
#62066 = CARTESIAN_POINT ( 'NONE',  ( -2.816281873526471635, 8.915301336597083903, -3.434112377981056508 ) ) ;
#62067 = CARTESIAN_POINT ( 'NONE',  ( 0.1532563361054082862, 36.21726448433410894, 2.638427012816831674 ) ) ;
#62068 = CARTESIAN_POINT ( 'NONE',  ( 9.422509992056141925, -4.852981322511822349, 5.440088680355547268 ) ) ;
#62069 = CARTESIAN_POINT ( 'NONE',  ( 13.43411237798105340, 50.58196800326375353, 12.81628187352647963 ) ) ;
#62070 = CARTESIAN_POINT ( 'NONE',  ( 14.94699059465104440, 0.3639308806417268505, 1.259949270174905767 ) ) ;
#62072 = FACE_OUTER_BOUND ( 'NONE', #43367, .T. ) ;
#62071 = CARTESIAN_POINT ( 'NONE',  ( 4.559911319644449179, 48.89701867748817676, 9.422509992056141925 ) ) ;
#62073 =( NAMED_UNIT ( * ) SI_UNIT ( $, .STERADIAN. ) SOLID_ANGLE_UNIT ( ) );
#62074 = SURFACE_STYLE_USAGE ( .BOTH. , #1118 ) ;
#62075 = CARTESIAN_POINT ( 'NONE',  ( 7.084665262690076126, 54.10535201082151247, 10.88017736071109987 ) ) ;
#62076 = CARTESIAN_POINT ( 'NONE',  ( 4.559911319644449179, 58.89701867748817676, 9.422509992056141925 ) ) ;
#62077 = DIRECTION ( 'NONE',  ( -1.000000000000000000, -0.000000000000000000, -0.000000000000000000 ) ) ;
#62078 = CARTESIAN_POINT ( 'NONE',  ( 4.559911319644449179, 63.89701867748817676, 9.422509992056141925 ) ) ;
#62079 = EDGE_CURVE ( 'NONE', #34327, #3454, #28855, .T. ) ;
#62080 = ADVANCED_FACE ( 'NONE', ( #94551 ), #79054, .T. ) ;
#62081 = CARTESIAN_POINT ( 'NONE',  ( -0.8801773607111009756, 13.06368534415483929, 1.068504757029289695E-15 ) ) ;
#62082 = CARTESIAN_POINT ( 'NONE',  ( 10.00000000000000000, 49.75893115100078745, -9.846743663894594434 ) ) ;
#62084 = FACE_OUTER_BOUND ( 'NONE', #89944, .T. ) ;
#62083 = CARTESIAN_POINT ( 'NONE',  ( 7.084665262690076126, 17.02201867748817676, -10.88017736071110164 ) ) ;
#62085 = CARTESIAN_POINT ( 'NONE',  ( 19.38216949554541202, 30.99863466993042138, 9.382169495545424454 ) ) ;
#62086 = ORIENTED_EDGE ( 'NONE', *, *, #64267, .F. ) ;
#62087 = CARTESIAN_POINT ( 'NONE',  ( -0.8801773607111008646, 38.27201867748816255, 2.915334737309923430 ) ) ;
#62088 = CARTESIAN_POINT ( 'NONE',  ( 21.09922568453594849, 11.20696800326375531, 6.408140936763242479 ) ) ;
#62089 = CARTESIAN_POINT ( 'NONE',  ( 12.91533473730992121, 14.52201867748817143, 10.88017736071110164 ) ) ;
#62090 = CARTESIAN_POINT ( 'NONE',  ( -0.8801773607111009756, 43.06368534415484106, 1.068504757029289695E-15 ) ) ;
#62091 = CARTESIAN_POINT ( 'NONE',  ( -2.266590686148945544, 41.38708216824729647, -7.082119434687050408 ) ) ;
#62092 = CARTESIAN_POINT ( 'NONE',  ( 2.791683348922240793, 26.63393115100078745, 7.208316651077764092 ) ) ;
#62093 = COLOUR_RGB ( '', 0.72549020, 0.75294118, 0.79215686) ;
#62094 = CARTESIAN_POINT ( 'NONE',  ( 7.084665262690076126, 59.10535201082150536, 10.88017736071109987 ) ) ;
#62095 = LINE ( 'NONE', #15152, #28231 ) ;
#62096 = CARTESIAN_POINT ( 'NONE',  ( -2.266590686148945544, 22.22041550158063572, 7.082119434687048631 ) ) ;
#62097 = SURFACE_SIDE_STYLE ('',( #38630 ) ) ;
#62098 = CARTESIAN_POINT ( 'NONE',  ( 0.1532563361054083140, 56.00893115100078745, 1.131784320476157264E-15 ) ) ;
#62099 = VERTEX_POINT ( 'NONE', #10569 ) ;
#62100 = CARTESIAN_POINT ( 'NONE',  ( 2.917880565312948704, 37.63708216824731068, 12.26659068614894643 ) ) ;
#62101 = CARTESIAN_POINT ( 'NONE',  ( 6.204703633549690345, 32.84541550158063927, 14.16423886937410082 ) ) ;
#62102 = CARTESIAN_POINT ( 'NONE',  ( 17.20831665107776587, 7.883931151000784787, 7.208316651077764980 ) ) ;
#62103 = CARTESIAN_POINT ( 'NONE',  ( 0.1532563361054082862, 56.21726448433411605, 2.638427012816831674 ) ) ;
#62104 = CARTESIAN_POINT ( 'NONE',  ( -8.159331231882687163, -4.163042900874275531, 4.000000000000000000 ) ) ;
#62106 = CARTESIAN_POINT ( 'NONE',  ( -1.099225684535947600, 18.70696800326375353, -6.408140936763238038 ) ) ;
#62105 = CARTESIAN_POINT ( 'NONE',  ( 20.88017736071110164, 55.35535201082149825, 2.915334737309930979 ) ) ;
#62107 = CARTESIAN_POINT ( 'NONE',  ( 24.16423886937410614, 34.30374883491396787, 8.672049930838204340E-16 ) ) ;
#62108 = CARTESIAN_POINT ( 'NONE',  ( -0.8801773607111008646, 33.27201867748817676, 2.915334737309923430 ) ) ;
#62109 = CARTESIAN_POINT ( 'NONE',  ( 4.559911319644449179, 33.89701867748817676, 9.422509992056141925 ) ) ;
#62110 = LINE ( 'NONE', #69149, #38039 ) ;
#62111 = CARTESIAN_POINT ( 'NONE',  ( 7.084665262690076126, 54.10535201082151247, 10.88017736071109987 ) ) ;
#62112 = ADVANCED_FACE ( 'NONE', ( #95035 ), #63066, .T. ) ;
#62113 = AXIS2_PLACEMENT_3D ( 'NONE', #20316, #27306, #65299 ) ;
#62114 = CARTESIAN_POINT ( 'NONE',  ( -8.527530157486182816, -4.407735515665881287, -4.923371831947288335 ) ) ;
#62115 = ORIENTED_EDGE ( 'NONE', *, *, #70361, .F. ) ;
#62116 = DIRECTION ( 'NONE',  ( 0.000000000000000000, 0.000000000000000000, 1.000000000000000000 ) ) ;
#62117 = ORIENTED_EDGE ( 'NONE', *, *, #79376, .F. ) ;
#62118 = ORIENTED_EDGE ( 'NONE', *, *, #56748, .T. ) ;
#62119 = CARTESIAN_POINT ( 'NONE',  ( 13.79529636645030344, 3.262082168247301350, 14.16423886937410614 ) ) ;
#62121 = CARTESIAN_POINT ( 'NONE',  ( 2.917880565312950480, 65.97041550158063217, -12.26659068614894821 ) ) ;
#62120 = CARTESIAN_POINT ( 'NONE',  ( 2.917880565312950480, 60.97041550158063927, -12.26659068614894821 ) ) ;
#62123 = CARTESIAN_POINT ( 'NONE',  ( 0.1532563361054083140, 56.00893115100078745, 1.131784320476157264E-15 ) ) ;
#62122 = CARTESIAN_POINT ( 'NONE',  ( 2.791683348922237240, 40.38393115100078035, -7.208316651077763204 ) ) ;
#62124 = CARTESIAN_POINT ( 'NONE',  ( 9.879999999999990123, 20.99999999999999645, -1.249999999999987121 ) ) ;
#62125 = VECTOR ( 'NONE', #93002, 1000.000000000000000 ) ;
#62126 = AXIS2_PLACEMENT_3D ( 'NONE', #62642, #93147, #70663 ) ;
#62127 = CARTESIAN_POINT ( 'NONE',  ( 6.565887622018943937, 0.1653013365970866511, 12.81628187352647430 ) ) ;
#62128 = VERTEX_POINT ( 'NONE', #26544 ) ;
#62129 = CARTESIAN_POINT ( 'NONE',  ( 24.16423886937410614, 44.51208216824730357, -3.795296366450302550 ) ) ;
#62130 = B_SPLINE_CURVE_WITH_KNOTS ( 'NONE', 3,
 ( #68418, #29407, #59910, #53396, #7433, #77372 ),
 .UNSPECIFIED., .F., .F.,
 ( 4, 2, 4 ),
 ( 5.553824967135426632E-18, 0.0002605067024380922601, 0.0005210134048761789908 ),
 .UNSPECIFIED. ) ;
#62131 = CARTESIAN_POINT ( 'NONE',  ( -2.266590686148945544, 41.38708216824729647, -7.082119434687050408 ) ) ;
#62132 = ORIENTED_EDGE ( 'NONE', *, *, #44189, .T. ) ;
#62133 = CARTESIAN_POINT ( 'NONE',  ( 10.00000000000000178, 14.31368534415483751, 10.88017736071110342 ) ) ;
#62134 = CARTESIAN_POINT ( 'NONE',  ( 21.09922568453595559, 57.04030133659708923, -6.408140936763230044 ) ) ;
#62135 = CARTESIAN_POINT ( 'NONE',  ( 0.1532563361054083140, 51.00893115100078745, 1.131784320476157264E-15 ) ) ;
#62136 = CARTESIAN_POINT ( 'NONE',  ( -0.8801773607111009756, 38.06368534415484106, 1.068504757029289695E-15 ) ) ;
#62137 = CARTESIAN_POINT ( 'NONE',  ( -0.1503990784575242878, 64.24884699246891273, -6.262539305110083276 ) ) ;
#62138 = CARTESIAN_POINT ( 'NONE',  ( 19.84674366389459266, 53.30059781766744464, 2.638427012816836559 ) ) ;
#62139 = CARTESIAN_POINT ( 'NONE',  ( 19.42250999205614193, 60.14701867748817676, 5.440088680355555262 ) ) ;
#62140 = CARTESIAN_POINT ( 'NONE',  ( 0.5774900079438590739, 32.64701867748816966, -5.440088680355550821 ) ) ;
#62141 = VECTOR ( 'NONE', #23584, 1000.000000000000000 ) ;
#62142 = DIRECTION ( 'NONE',  ( -0.000000000000000000, -1.000000000000000000, -0.000000000000000000 ) ) ;
#62143 = CARTESIAN_POINT ( 'NONE',  ( 19.84674366389459621, 3.508931151000785231, 7.409399052514197653E-17 ) ) ;
#62144 = CARTESIAN_POINT ( 'NONE',  ( -8.606322355891443010, 15.00000000000000000, 11.66967075398801335 ) ) ;
#62145 = ORIENTED_EDGE ( 'NONE', *, *, #78041, .F. ) ;
#62146 = CARTESIAN_POINT ( 'NONE',  ( 8.991948000357622206, -4.139826107003811373, 4.000000000000000000 ) ) ;
#62147 = CARTESIAN_POINT ( 'NONE',  ( 0.1532563361054100626, 35.80059781766745175, -2.638427012816831230 ) ) ;
#62148 = DIRECTION ( 'NONE',  ( 1.000000000000000000, 0.000000000000000000, -0.000000000000000000 ) ) ;
#62149 = CARTESIAN_POINT ( 'NONE',  ( 0.6178305044545838731, 44.74863466993042493, 9.382169495545420901 ) ) ;
#62150 = CARTESIAN_POINT ( 'NONE',  ( 19.72487221294570858, 70.00000000000000000, 6.000000000000000000 ) ) ;
#62151 = CARTESIAN_POINT ( 'NONE',  ( -3.635384400432159158, -3.854802480546752896, 3.750000000000000444 ) ) ;
#62152 = ORIENTED_EDGE ( 'NONE', *, *, #96311, .F. ) ;
#62153 = VECTOR ( 'NONE', #42883, 1000.000000000000000 ) ;
#62154 = CARTESIAN_POINT ( 'NONE',  ( -9.990730578767625047, 46.91630561652144138, 0.000000000000000000 ) ) ;
#62155 = DIRECTION ( 'NONE',  ( -1.000000000000000000, 0.000000000000000000, 0.000000000000000000 ) ) ;
#62156 = CARTESIAN_POINT ( 'NONE',  ( 7.361572987183169658, 49.96726448433410894, -9.846743663894592657 ) ) ;
#62157 = CARTESIAN_POINT ( 'NONE',  ( -0.3689425029237898834, 51.17874883491397497, -10.36894250292378850 ) ) ;
#62158 = CARTESIAN_POINT ( 'NONE',  ( 0.1532563361054083140, 61.00893115100078745, 1.131784320476157264E-15 ) ) ;
#62159 = CARTESIAN_POINT ( 'NONE',  ( 8.879999999999991900, 76.07179676972447169, 4.250000000000000000 ) ) ;
#62160 = CARTESIAN_POINT ( 'NONE',  ( 7.361572987183170547, 22.05059781766745530, 9.846743663894590881 ) ) ;
#62161 = CARTESIAN_POINT ( 'NONE',  ( 3.591859063236761518, 49.95696800326375353, 11.09922568453594849 ) ) ;
#62162 = EDGE_CURVE ( 'NONE', #53783, #56374, #61060, .T. ) ;
#62163 = VECTOR ( 'NONE', #96917, 1000.000000000000000 ) ;
#62164 = CARTESIAN_POINT ( 'NONE',  ( 17.20831665107776587, 59.13393115100078745, -7.208316651077762316 ) ) ;
#62165 = CARTESIAN_POINT ( 'NONE',  ( 0.5774900079438590739, 47.64701867748817676, -5.440088680355550821 ) ) ;
#62166 = CARTESIAN_POINT ( 'NONE',  ( 19.84674366389459266, 48.71726448433413026, -2.638427012816827677 ) ) ;
#62167 = CARTESIAN_POINT ( 'NONE',  ( 6.910409932112633768, -84.29236789246745332, -2.750000000000000000 ) ) ;
#62168 = CARTESIAN_POINT ( 'NONE',  ( -0.8801773607111009756, 53.06368534415484106, 1.068504757029289695E-15 ) ) ;
#62169 = ORIENTED_EDGE ( 'NONE', *, *, #84063, .T. ) ;
#62170 = DIRECTION ( 'NONE',  ( 0.000000000000000000, -1.000000000000000000, 0.000000000000000000 ) ) ;
#62171 = CARTESIAN_POINT ( 'NONE',  ( -0.8801773607110991993, 22.85535201082150181, -2.915334737309923874 ) ) ;
#62173 = CARTESIAN_POINT ( 'NONE',  ( -0.8801773607111009756, 53.06368534415484106, 1.068504757029289695E-15 ) ) ;
#62172 = CARTESIAN_POINT ( 'NONE',  ( 0.6178305044545818747, 13.49863466993041783, -9.382169495545419124 ) ) ;
#62174 = DIRECTION ( 'NONE',  ( -0.000000000000000000, -1.000000000000000000, -0.000000000000000000 ) ) ;
#62175 = CARTESIAN_POINT ( 'NONE',  ( 0.000000000000000000, 40.74999999999999289, 4.000000000000000000 ) ) ;
#62176 = CARTESIAN_POINT ( 'NONE',  ( 20.15039907845753220, 45.60158574516643881, -6.262539305110077947 ) ) ;
#62178 = LINE ( 'NONE', #39710, #7350 ) ;
#62177 = CARTESIAN_POINT ( 'NONE',  ( 12.91533473730992121, 54.52201867748816255, 10.88017736071110164 ) ) ;
#62179 = CARTESIAN_POINT ( 'NONE',  ( 0.1532563361054100626, 35.80059781766745175, -2.638427012816831230 ) ) ;
#62180 = CARTESIAN_POINT ( 'NONE',  ( 0.1532563361054100626, 5.800597817667452638, -2.638427012816831230 ) ) ;
#62181 = CARTESIAN_POINT ( 'NONE',  ( 9.422509992056141925, -34.01964798917848753, -5.440088680355554374 ) ) ;
#62182 = CARTESIAN_POINT ( 'NONE',  ( 10.00000000000000000, 7.873634669930421381, -12.81628187352647608 ) ) ;
#62183 = ADVANCED_FACE ( 'NONE', ( #55583 ), #49056, .F. ) ;
#62185 = SURFACE_SIDE_STYLE ('',( #56186 ) ) ;
#62184 = CARTESIAN_POINT ( 'NONE',  ( 7.084665262690076126, 14.10535201082150358, 10.88017736071109987 ) ) ;
#62186 =( NAMED_UNIT ( * ) PLANE_ANGLE_UNIT ( ) SI_UNIT ( $, .RADIAN. ) );
#62187 = CARTESIAN_POINT ( 'NONE',  ( -0.3689425029237898834, 41.17874883491397497, -10.36894250292378850 ) ) ;
#62188 = CARTESIAN_POINT ( 'NONE',  ( 6.204703633549690345, 60.76208216824730357, -14.16423886937410259 ) ) ;
#62189 = CARTESIAN_POINT ( 'NONE',  ( 1.472469842513823179, 31.42559781766745530, 4.923371831947296329 ) ) ;
#62190 = CARTESIAN_POINT ( 'NONE',  ( 14.92337183194729988, 24.34226448433411960, -8.527530157486177487 ) ) ;
#62191 = CARTESIAN_POINT ( 'NONE',  ( -0.8801773607111009756, 18.06368534415484106, 1.068504757029289695E-15 ) ) ;
#62192 = EDGE_CURVE ( 'NONE', #23594, #52793, #41578, .T. ) ;
#62193 = ORIENTED_EDGE ( 'NONE', *, *, #49448, .T. ) ;
#62194 = CARTESIAN_POINT ( 'NONE',  ( 19.84674366389459266, 38.71726448433412315, -2.638427012816827677 ) ) ;
#62195 = CARTESIAN_POINT ( 'NONE',  ( 10.00000000000000178, 29.31368534415483751, 10.88017736071110342 ) ) ;
#62196 = B_SPLINE_CURVE_WITH_KNOTS ( 'NONE', 3,
 ( #28745, #60231, #29236, #52242, #90726, #22251 ),
 .UNSPECIFIED., .F., .F.,
 ( 4, 2, 4 ),
 ( 0.000000000000000000, 0.0002605067024380928564, 0.0005210134048761857128 ),
 .UNSPECIFIED. ) ;
#62197 = CARTESIAN_POINT ( 'NONE',  ( 0.1532563361054100626, 65.80059781766745175, -2.638427012816831230 ) ) ;
#62199 = CARTESIAN_POINT ( 'NONE',  ( -1.926860441876563801, 17.66212336850780673, 1.004413902775740978E-15 ) ) ;
#62198 = CARTESIAN_POINT ( 'NONE',  ( 24.16423886937409904, 9.095415501580633943, 3.795296366450317205 ) ) ;
#62200 = PLANE ( 'NONE',  #23224 ) ;
#62201 = EDGE_CURVE ( 'NONE', #54738, #87096, #40582, .T. ) ;
#62202 = UNCERTAINTY_MEASURE_WITH_UNIT (LENGTH_MEASURE( 1.000000000000000082E-05 ), #21044, 'distance_accuracy_value', 'NONE');
#62203 = CARTESIAN_POINT ( 'NONE',  ( 7.361572987183170547, 17.05059781766745530, 9.846743663894590881 ) ) ;
#62204 = CARTESIAN_POINT ( 'NONE',  ( 13.43411237798105340, 35.58196800326375353, 12.81628187352647963 ) ) ;
#62205 = CARTESIAN_POINT ( 'NONE',  ( 17.20831665107776587, 49.13393115100078745, -7.208316651077762316 ) ) ;
#62206 = EDGE_LOOP ( 'NONE', ( #58574, #30713, #59442, #44932 ) ) ;
#62207 = CARTESIAN_POINT ( 'NONE',  ( 5.076628168052703671, 16.84226448433411960, 8.527530157486179263 ) ) ;
#62208 = CYLINDRICAL_SURFACE ( 'NONE', #25374, 0.5000000000000004441 ) ;
#62209 = CARTESIAN_POINT ( 'NONE',  ( 67.06412365047464164, 14.00000000000000888, -10.00000000000000000 ) ) ;
#62210 = AXIS2_PLACEMENT_3D ( 'NONE', #27895, #11918, #21399 ) ;
#62211 = CARTESIAN_POINT ( 'NONE',  ( 2.917880565312948704, 52.63708216824730357, 12.26659068614894643 ) ) ;
#62212 = CARTESIAN_POINT ( 'NONE',  ( 10.00000000000000178, 49.31368534415484106, 10.88017736071110342 ) ) ;
#62213 = FACE_OUTER_BOUND ( 'NONE', #66109, .T. ) ;
#62214 = CARTESIAN_POINT ( 'NONE',  ( 12.91533473730993009, 51.60535201082149825, -10.88017736071109987 ) ) ;
#62215 = CARTESIAN_POINT ( 'NONE',  ( 0.1532563361054083140, 31.00893115100078390, 1.131784320476157264E-15 ) ) ;
#62216 = CARTESIAN_POINT ( 'NONE',  ( 0.5774900079438607392, 23.48035201082150536, 5.440088680355550821 ) ) ;
#62217 = DIRECTION ( 'NONE',  ( -1.000000000000000000, -0.000000000000000000, -0.000000000000000000 ) ) ;
#62218 = CARTESIAN_POINT ( 'NONE',  ( 1.472469842513823179, 50.59226448433411605, -4.923371831947296329 ) ) ;
#62219 = CIRCLE ( 'NONE', #68661, 14.49999999999999822 ) ;
#62220 = CIRCLE ( 'NONE', #89346, 8.000000000000007105 ) ;
#62221 = CARTESIAN_POINT ( 'NONE',  ( 17.96484262340118221, 46.18868534415484106, -7.964842623401177768 ) ) ;
#62222 = PLANE ( 'NONE',  #34667 ) ;
#62223 = ORIENTED_EDGE ( 'NONE', *, *, #39998, .F. ) ;
#62224 = VERTEX_POINT ( 'NONE', #33058 ) ;
#62225 = LINE ( 'NONE', #17246, #43705 ) ;
#62226 = SURFACE_STYLE_FILL_AREA ( #71225 ) ;
#62227 = CARTESIAN_POINT ( 'NONE',  ( 18.52753015748617571, 48.09226448433412315, 4.923371831947298993 ) ) ;
#62228 = CARTESIAN_POINT ( 'NONE',  ( 10.00000000000000178, 17.25893115100078745, 9.846743663894594434 ) ) ;
#62229 = CARTESIAN_POINT ( 'NONE',  ( 16.40814093676323893, 55.79030133659708923, 11.09922568453595026 ) ) ;
#62231 = CARTESIAN_POINT ( 'NONE',  ( 7.361572987183169658, 44.96726448433412315, -9.846743663894592657 ) ) ;
#62230 = CARTESIAN_POINT ( 'NONE',  ( 2.035157376598822676, 17.43868534415483751, -7.964842623401177768 ) ) ;
#62232 = DIRECTION ( 'NONE',  ( 0.000000000000000000, 0.000000000000000000, 1.000000000000000000 ) ) ;
#62233 = CARTESIAN_POINT ( 'NONE',  ( 13.79529636645031943, 45.34541550158062506, -14.16423886937409904 ) ) ;
#62234 = CARTESIAN_POINT ( 'NONE',  ( 10.00000000000000000, 55.55374883491396787, -14.16423886937410082 ) ) ;
#62235 = CARTESIAN_POINT ( 'NONE',  ( 4.469999999999999751, 37.00000000000000000, -4.000000000000000000 ) ) ;
#62236 = FACE_OUTER_BOUND ( 'NONE', #7936, .T. ) ;
#62237 = CARTESIAN_POINT ( 'NONE',  ( 15.44008868035555793, 51.39701867748816966, -9.422509992056140149 ) ) ;
#62238 = ADVANCED_FACE ( 'NONE', ( #39604 ), #74507, .F. ) ;
#62239 = CARTESIAN_POINT ( 'NONE',  ( 0.1532563361054082862, 21.21726448433412315, 2.638427012816831674 ) ) ;
#62240 = CARTESIAN_POINT ( 'NONE',  ( -6.031993939708439889, -39.82530731230075105, 3.749999999999193090 ) ) ;
#62241 = VERTEX_POINT ( 'NONE', #65016 ) ;
#62242 = CARTESIAN_POINT ( 'NONE',  ( 20.15039907845753220, 30.60158574516642815, -6.262539305110077947 ) ) ;
#62243 = EDGE_LOOP ( 'NONE', ( #57601, #66697, #68082, #29666 ) ) ;
#62244 = CARTESIAN_POINT ( 'NONE',  ( 0.1532563361054082862, 16.21726448433411960, 2.638427012816831674 ) ) ;
#62245 = ORIENTED_EDGE ( 'NONE', *, *, #38184, .F. ) ;
#62246 = CARTESIAN_POINT ( 'NONE',  ( 17.08211943468705130, 13.47041550158063572, 12.26659068614894998 ) ) ;
#62247 = CARTESIAN_POINT ( 'NONE',  ( 0.1532563361054083140, 16.00893115100078390, 1.131784320476157264E-15 ) ) ;
#62248 = CARTESIAN_POINT ( 'NONE',  ( 15.44008868035555260, 39.73035201082150536, 9.422509992056143702 ) ) ;
#62249 = CARTESIAN_POINT ( 'NONE',  ( 6.898461952320343649, 4.875757609050324087E-16, 12.75387089053313971 ) ) ;
#62251 = ADVANCED_FACE ( 'NONE', ( #50036 ), #5040, .T. ) ;
#62250 = EDGE_LOOP ( 'NONE', ( #16764, #69639, #66366, #16695 ) ) ;
#62252 = CARTESIAN_POINT ( 'NONE',  ( 19.42250999205614548, 40.98035201082150536, -5.440088680355545492 ) ) ;
#62253 = CARTESIAN_POINT ( 'NONE',  ( -0.04068437667224381049, 2.219743609177204036, -6.396802510829708410 ) ) ;
#62254 = EDGE_LOOP ( 'NONE', ( #32400, #37609, #85030, #17957 ) ) ;
#62255 = CARTESIAN_POINT ( 'NONE',  ( 24.16423886937409904, 9.095415501580633943, 3.795296366450317205 ) ) ;
#62256 = ORIENTED_EDGE ( 'NONE', *, *, #13597, .T. ) ;
#62257 = CARTESIAN_POINT ( 'NONE',  ( -1.099225684535947600, 14.54030133659708568, 6.408140936763237150 ) ) ;
#62258 = CARTESIAN_POINT ( 'NONE',  ( 14.92337183194729988, 9.342264484334119601, -8.527530157486177487 ) ) ;
#62259 = LINE ( 'NONE', #53791, #92891 ) ;
#62260 = CARTESIAN_POINT ( 'NONE',  ( 19.42250999205614193, 10.14701867748816966, 5.440088680355555262 ) ) ;
#62261 = CARTESIAN_POINT ( 'NONE',  ( 0.1532563361054100626, 20.80059781766744464, -2.638427012816831230 ) ) ;
#62262 = CARTESIAN_POINT ( 'NONE',  ( 7.084665262690076126, 37.02201867748817676, -10.88017736071110164 ) ) ;
#62263 = EDGE_LOOP ( 'NONE', ( #9729, #67298, #29075, #2586 ) ) ;
#62264 = CARTESIAN_POINT ( 'NONE',  ( 0.6178305044545818747, 63.49863466993043204, -9.382169495545419124 ) ) ;
#62265 = CARTESIAN_POINT ( 'NONE',  ( 15.44008868035555793, 56.39701867748817676, -9.422509992056140149 ) ) ;
#62266 = DIRECTION ( 'NONE',  ( 0.9975640502598257520, -0.06975647374410356982, 0.000000000000000000 ) ) ;
#62267 = CARTESIAN_POINT ( 'NONE',  ( 15.44008868035555793, 66.39701867748817676, -9.422509992056140149 ) ) ;
#62268 = EDGE_LOOP ( 'NONE', ( #72400, #42839, #50527, #58073 ) ) ;
#62269 = CARTESIAN_POINT ( 'NONE',  ( 11.12471383767606525, 12.50000000000035527, 1.674288514511126591 ) ) ;
#62270 = AXIS2_PLACEMENT_3D ( 'NONE', #94801, #10333, #40345 ) ;
#62271 = EDGE_CURVE ( 'NONE', #70565, #35851, #57625, .T. ) ;
#62272 = CARTESIAN_POINT ( 'NONE',  ( 1.472469842513823179, 26.42559781766745175, 4.923371831947296329 ) ) ;
#62273 = CARTESIAN_POINT ( 'NONE',  ( 3.591859063236763294, 58.29030133659708923, -11.09922568453595026 ) ) ;
#62274 = CARTESIAN_POINT ( 'NONE',  ( 17.08211943468705840, 5.137082168247300906, -12.26659068614894466 ) ) ;
#62275 = CARTESIAN_POINT ( 'NONE',  ( 12.63842701281683922, 19.55059781766745175, -9.846743663894590881 ) ) ;
#62276 = CARTESIAN_POINT ( 'NONE',  ( 0.6178305044545838731, 24.74863466993042493, 9.382169495545420901 ) ) ;
#62278 = CARTESIAN_POINT ( 'NONE',  ( -5.329637805456036936, -28.67156944097240512, -2.750000000000000000 ) ) ;
#62277 = CARTESIAN_POINT ( 'NONE',  ( -3.750000000000000000, 10.25000000000000000, 3.750000000000000000 ) ) ;
#62279 = CARTESIAN_POINT ( 'NONE',  ( 12.91533473730993009, 51.60535201082149825, -10.88017736071109987 ) ) ;
#62280 = VECTOR ( 'NONE', #17284, 1000.000000000000000 ) ;
#62281 = CARTESIAN_POINT ( 'NONE',  ( 19.84674366389459266, 63.71726448433412315, -2.638427012816827677 ) ) ;
#62282 = FACE_OUTER_BOUND ( 'NONE', #13015, .T. ) ;
#62283 = EDGE_CURVE ( 'NONE', #16435, #14763, #14960, .T. ) ;
#62284 = AXIS2_PLACEMENT_3D ( 'NONE', #45555, #95223, #2794 ) ;
#62285 = CARTESIAN_POINT ( 'NONE',  ( 12.63842701281683034, 32.46726448433412315, 9.846743663894596210 ) ) ;
#62286 = CARTESIAN_POINT ( 'NONE',  ( 0.1532563361054082862, 16.21726448433411960, 2.638427012816831674 ) ) ;
#62287 = CARTESIAN_POINT ( 'NONE',  ( 17.96484262340118221, 11.18868534415483929, -7.964842623401177768 ) ) ;
#62288 = CARTESIAN_POINT ( 'NONE',  ( 0.6178305044545818747, 18.49863466993041428, -9.382169495545419124 ) ) ;
#62289 = CARTESIAN_POINT ( 'NONE',  ( 7.084665262690076126, 4.105352010821503583, 10.88017736071109987 ) ) ;
#62290 = CARTESIAN_POINT ( 'NONE',  ( -8.000343251535921851, 84.06932101904432386, 3.750000000000000000 ) ) ;
#62291 = CARTESIAN_POINT ( 'NONE',  ( -0.8801773607111009756, 23.06368534415484106, 1.068504757029289695E-15 ) ) ;
#62292 = EDGE_LOOP ( 'NONE', ( #46275, #10298, #40040 ) ) ;
#62293 = CARTESIAN_POINT ( 'NONE',  ( 4.656459206270717743, -8.255604869861873141, 2.750000000000000000 ) ) ;
#62295 = CARTESIAN_POINT ( 'NONE',  ( 20.88017736071110875, 20.77201867748816611, -2.915334737309920765 ) ) ;
#62294 = CARTESIAN_POINT ( 'NONE',  ( 7.361572987183169658, 29.96726448433411960, -9.846743663894592657 ) ) ;
#62296 = CARTESIAN_POINT ( 'NONE',  ( -5.803070148808410877, 15.00000000000000000, 13.28812917035381780 ) ) ;
#62297 = CARTESIAN_POINT ( 'NONE',  ( 7.084665262690076126, 32.02201867748816966, -10.88017736071110164 ) ) ;
#62299 = CARTESIAN_POINT ( 'NONE',  ( 3.772706337463130544E-18, 0.2999999999999981570, 0.000000000000000000 ) ) ;
#62298 = CARTESIAN_POINT ( 'NONE',  ( -0.8801773607111009756, 3.063685344154838397, 1.068504757029289695E-15 ) ) ;
#62300 = CARTESIAN_POINT ( 'NONE',  ( 18.52753015748618282, 18.92559781766745175, -4.923371831947291888 ) ) ;
#62301 = CARTESIAN_POINT ( 'NONE',  ( 17.20831665107776587, 42.88393115100077324, 7.208316651077764980 ) ) ;
#62302 = CARTESIAN_POINT ( 'NONE',  ( 8.880000000000000782, 1.116573172248542834E-15, -6.250000000000000000 ) ) ;
#62303 = LINE ( 'NONE', #61328, #57669 ) ;
#62304 = CARTESIAN_POINT ( 'NONE',  ( 0.4195498155886495661, 0.4999999999999985012, -9.500000000000000000 ) ) ;
#62305 = CARTESIAN_POINT ( 'NONE',  ( -8.468261785896212146, -9.345432893202591629, -3.750000000000000000 ) ) ;
#62306 = CARTESIAN_POINT ( 'NONE',  ( 22.26659068614895176, 24.72041550158063572, -7.082119434687042414 ) ) ;
#62307 = CARTESIAN_POINT ( 'NONE',  ( 7.361572987183170547, 37.05059781766744464, 9.846743663894590881 ) ) ;
#62308 = ADVANCED_FACE ( 'NONE', ( #36526 ), #42537, .F. ) ;
#62309 = DIRECTION ( 'NONE',  ( -1.000000000000000000, 0.000000000000000000, 0.000000000000000000 ) ) ;
#62310 = EDGE_LOOP ( 'NONE', ( #68626, #48105, #7264, #62623 ) ) ;
#62311 = CARTESIAN_POINT ( 'NONE',  ( 24.16423886937409904, 54.09541550158063217, 3.795296366450317205 ) ) ;
#62312 = CARTESIAN_POINT ( 'NONE',  ( 0.1532563361054083140, 26.00893115100078745, 1.131784320476157264E-15 ) ) ;
#62314 = CARTESIAN_POINT ( 'NONE',  ( 4.181050312904970312, 15.00000000000000888, 14.01631781289605705 ) ) ;
#62313 = FACE_OUTER_BOUND ( 'NONE', #61184, .T. ) ;
#62315 = CARTESIAN_POINT ( 'NONE',  ( 7.084665262690076126, 42.02201867748816966, -10.88017736071110164 ) ) ;
#62316 = CARTESIAN_POINT ( 'NONE',  ( 21.09922568453595559, 52.04030133659708923, -6.408140936763230044 ) ) ;
#62317 = EDGE_CURVE ( 'NONE', #22095, #42454, #17684, .T. ) ;
#62318 = CARTESIAN_POINT ( 'NONE',  ( 4.559911319644449179, 13.89701867748817143, 9.422509992056141925 ) ) ;
#62319 = CARTESIAN_POINT ( 'NONE',  ( -1.099225684535947600, 44.54030133659708923, 6.408140936763237150 ) ) ;
#62320 = CARTESIAN_POINT ( 'NONE',  ( 19.38216949554541202, 0.9986346699304200492, 9.382169495545424454 ) ) ;
#62321 = CARTESIAN_POINT ( 'NONE',  ( 19.84674366389459266, 3.300597817667451750, 2.638427012816836559 ) ) ;
#62322 = ORIENTED_EDGE ( 'NONE', *, *, #13914, .T. ) ;
#62323 = DIRECTION ( 'NONE',  ( 0.3826834323650877834, -0.000000000000000000, -0.9238795325112876267 ) ) ;
#62324 = DIRECTION ( 'NONE',  ( 1.000000000000000000, 0.000000000000000000, 0.000000000000000000 ) ) ;
#62325 = CARTESIAN_POINT ( 'NONE',  ( -2.266590686148945544, 57.22041550158063217, 7.082119434687048631 ) ) ;
#62326 = CARTESIAN_POINT ( 'NONE',  ( 24.16423886937409904, 9.095415501580633943, 3.795296366450317205 ) ) ;
#62327 = CARTESIAN_POINT ( 'NONE',  ( 12.91533473730993009, 21.60535201082150536, -10.88017736071109987 ) ) ;
#62328 = CARTESIAN_POINT ( 'NONE',  ( 20.88017736071110519, 30.56368534415484106, 2.639326808657452039E-16 ) ) ;
#62329 = CARTESIAN_POINT ( 'NONE',  ( 13.95697193428308758, -2.801561473043597583E-15, 4.371663894958916607 ) ) ;
#62330 = DIRECTION ( 'NONE',  ( -2.569960705150826877E-16, 1.000000000000000000, 0.000000000000000000 ) ) ;
#62331 = CARTESIAN_POINT ( 'NONE',  ( 19.42250999205614193, 65.14701867748817676, 5.440088680355555262 ) ) ;
#62332 = FACE_OUTER_BOUND ( 'NONE', #48421, .T. ) ;
#62333 = CARTESIAN_POINT ( 'NONE',  ( 7.361572987183170547, 17.05059781766745530, 9.846743663894590881 ) ) ;
#62334 = CARTESIAN_POINT ( 'NONE',  ( 7.860426697680415131, -0.03417435944610275333, 13.93165778241937680 ) ) ;
#62335 = DIRECTION ( 'NONE',  ( -0.000000000000000000, -1.000000000000000000, -0.000000000000000000 ) ) ;
#62336 = CARTESIAN_POINT ( 'NONE',  ( 18.52753015748618282, 13.92559781766745175, -4.923371831947291888 ) ) ;
#62337 = CARTESIAN_POINT ( 'NONE',  ( 12.63842701281683034, 37.46726448433411605, 9.846743663894596210 ) ) ;
#62338 = CARTESIAN_POINT ( 'NONE',  ( 7.084665262690076126, 17.02201867748817676, -10.88017736071110164 ) ) ;
#62339 = CIRCLE ( 'NONE', #19236, 13.75000000000001776 ) ;
#62340 = CARTESIAN_POINT ( 'NONE',  ( 6.565887622018943937, 33.08196800326374643, -12.81628187352647608 ) ) ;
#62342 = EDGE_CURVE ( 'NONE', #73676, #98326, #84206, .T. ) ;
#62341 = CARTESIAN_POINT ( 'NONE',  ( 1.472469842513823179, 5.592264484334118713, -4.923371831947296329 ) ) ;
#62343 = CARTESIAN_POINT ( 'NONE',  ( -11.22915323889568562, -0.03417435944610275333, -8.773176023390764300 ) ) ;
#62344 = CARTESIAN_POINT ( 'NONE',  ( 5.076628168052704559, 55.17559781766745175, -8.527530157486179263 ) ) ;
#62345 = B_SPLINE_CURVE_WITH_KNOTS ( 'NONE', 3,
 ( #19235, #49717, #42243, #5721 ),
 .UNSPECIFIED., .F., .F.,
 ( 4, 4 ),
 ( 0.000000000000000000, 0.001036303429213390010 ),
 .UNSPECIFIED. ) ;
#62346 = CARTESIAN_POINT ( 'NONE',  ( 5.076628168052703671, 31.84226448433412315, 8.527530157486179263 ) ) ;
#62347 = CARTESIAN_POINT ( 'NONE',  ( 24.16423886937409904, 19.09541550158063927, 3.795296366450317205 ) ) ;
#62348 = MECHANICAL_DESIGN_GEOMETRIC_PRESENTATION_REPRESENTATION (  '', ( #49569 ), #12816 ) ;
#62349 = CARTESIAN_POINT ( 'NONE',  ( 12.91533473730993009, 46.60535201082150536, -10.88017736071109987 ) ) ;
#62350 = CARTESIAN_POINT ( 'NONE',  ( 0.5774900079438607392, 8.480352010821505360, 5.440088680355550821 ) ) ;
#62351 = EDGE_CURVE ( 'NONE', #13980, #65168, #78334, .T. ) ;
#62352 = CARTESIAN_POINT ( 'NONE',  ( 0.5774900079438590739, 47.64701867748817676, -5.440088680355550821 ) ) ;
#62353 = CARTESIAN_POINT ( 'NONE',  ( 2.035157376598822676, 32.43868534415483396, -7.964842623401177768 ) ) ;
#62354 = ORIENTED_EDGE ( 'NONE', *, *, #28961, .F. ) ;
#62355 = CARTESIAN_POINT ( 'NONE',  ( -0.8801773607111009756, 43.06368534415484106, 1.068504757029289695E-15 ) ) ;
#62356 = ORIENTED_EDGE ( 'NONE', *, *, #86246, .T. ) ;
#62357 = CARTESIAN_POINT ( 'NONE',  ( 3.591859063236761518, 59.95696800326375353, 11.09922568453594849 ) ) ;
#62358 = CARTESIAN_POINT ( 'NONE',  ( 2.035157376598822676, 47.43868534415484817, -7.964842623401177768 ) ) ;
#62359 = ORIENTED_EDGE ( 'NONE', *, *, #13989, .F. ) ;
#62360 = CARTESIAN_POINT ( 'NONE',  ( 7.084665262690076126, 47.02201867748818387, -10.88017736071110164 ) ) ;
#62361 = CARTESIAN_POINT ( 'NONE',  ( 4.906778809679744668, -8.256987753881587011, 4.000000000000000000 ) ) ;
#62362 = CARTESIAN_POINT ( 'NONE',  ( 19.10478245763049898, 41.02576239577082617, -5.990408912944356956 ) ) ;
#62363 = DIRECTION ( 'NONE',  ( -1.000000000000000000, 0.000000000000000000, 0.000000000000000000 ) ) ;
#62364 = CARTESIAN_POINT ( 'NONE',  ( -2.266590686148945544, 61.38708216824730357, -7.082119434687050408 ) ) ;
#62365 = CARTESIAN_POINT ( 'NONE',  ( 0.5774900079438590739, 67.64701867748817676, -5.440088680355550821 ) ) ;
#62366 = CARTESIAN_POINT ( 'NONE',  ( -4.164238869374098151, 11.59541550158063217, -3.795296366450310543 ) ) ;
#62367 = CARTESIAN_POINT ( 'NONE',  ( -4.021969307579355224, -6.415483651463646630, -4.000000000000000000 ) ) ;
#62368 = CARTESIAN_POINT ( 'NONE',  ( 17.96484262340118221, 6.188685344154836621, -7.964842623401177768 ) ) ;
#62369 = CARTESIAN_POINT ( 'NONE',  ( 10.00000000000000178, 47.25893115100078745, 9.846743663894594434 ) ) ;
#62370 = VERTEX_POINT ( 'NONE', #58017 ) ;
#62371 = CARTESIAN_POINT ( 'NONE',  ( 12.63842701281683034, 42.46726448433412315, 9.846743663894596210 ) ) ;
#62372 = CARTESIAN_POINT ( 'NONE',  ( 15.44008868035555260, 64.73035201082151957, 9.422509992056143702 ) ) ;
#62373 = CARTESIAN_POINT ( 'NONE',  ( 12.91533473730992121, 44.52201867748816966, 10.88017736071110164 ) ) ;
#62374 = CARTESIAN_POINT ( 'NONE',  ( 14.92337183194729988, 34.34226448433411605, -8.527530157486177487 ) ) ;
#62375 = DIRECTION ( 'NONE',  ( 1.000000000000000000, 0.000000000000000000, 0.000000000000000000 ) ) ;
#62376 = CARTESIAN_POINT ( 'NONE',  ( 15.44008868035555260, 39.73035201082150536, 9.422509992056143702 ) ) ;
#62377 = CARTESIAN_POINT ( 'NONE',  ( -0.3689425029237881626, 52.42874883491396076, 10.36894250292379027 ) ) ;
#62378 = PRESENTATION_LAYER_ASSIGNMENT (  '', '', ( #6507 ) ) ;
#62379 = B_SPLINE_CURVE_WITH_KNOTS ( 'NONE', 3,
 ( #94408, #34384, #77930, #18917, #56896, #72386, #93428, #26896 ),
 .UNSPECIFIED., .F., .F.,
 ( 4, 2, 2, 4 ),
 ( 0.000000000000000000, 0.004806130321901048823, 0.007209195482851595352, 0.009612260643802141014 ),
 .UNSPECIFIED. ) ;
#62380 = CARTESIAN_POINT ( 'NONE',  ( 10.00000000000000000, 17.87363466993041783, -12.81628187352647608 ) ) ;
#62381 = DIRECTION ( 'NONE',  ( 0.000000000000000000, 0.000000000000000000, 1.000000000000000000 ) ) ;
#62382 = ORIENTED_EDGE ( 'NONE', *, *, #85831, .T. ) ;
#62383 = B_SPLINE_CURVE_WITH_KNOTS ( 'NONE', 3,
 ( #61354, #882, #84853, #46841, #98903, #53866 ),
 .UNSPECIFIED., .F., .F.,
 ( 4, 2, 4 ),
 ( 0.0002800289709862387156, 0.0006862344838250689603, 0.001092439996663899368 ),
 .UNSPECIFIED. ) ;
#62384 = CARTESIAN_POINT ( 'NONE',  ( 10.00000000000000000, 22.87363466993042138, -12.81628187352647608 ) ) ;
#62385 = CARTESIAN_POINT ( 'NONE',  ( 15.44008868035555793, 26.39701867748817321, -9.422509992056140149 ) ) ;
#62386 = EDGE_LOOP ( 'NONE', ( #80217, #87365, #43942, #43150 ) ) ;
#62387 = CARTESIAN_POINT ( 'NONE',  ( 2.791683348922237240, 0.3839311510007847872, -7.208316651077763204 ) ) ;
#62388 = CARTESIAN_POINT ( 'NONE',  ( 10.00000000000000000, 49.75893115100078745, -9.846743663894594434 ) ) ;
#62390 = CARTESIAN_POINT ( 'NONE',  ( 1.472469842513823179, 31.42559781766745530, 4.923371831947296329 ) ) ;
#62389 = CARTESIAN_POINT ( 'NONE',  ( 7.361572987183170547, 12.05059781766744997, 9.846743663894590881 ) ) ;
#62391 = CARTESIAN_POINT ( 'NONE',  ( -11.48810437782082694, -88.25603173497155751, 3.750000000000001332 ) ) ;
#62392 = CARTESIAN_POINT ( 'NONE',  ( -14.24131928502210975, 15.00000000000000000, -0.4973178280107823923 ) ) ;
#62393 = CARTESIAN_POINT ( 'NONE',  ( 14.92337183194729633, 22.67559781766745175, 8.527530157486181039 ) ) ;
#62394 = CARTESIAN_POINT ( 'NONE',  ( -7.750000000000000000, 79.82179676972448590, 6.250000000000000000 ) ) ;
#62395 = ADVANCED_FACE ( 'NONE', ( #11544 ), #51212, .T. ) ;
#62396 = CARTESIAN_POINT ( 'NONE',  ( 2.791683348922237240, 10.38393115100078390, -7.208316651077763204 ) ) ;
#62397 = SURFACE_SIDE_STYLE ('',( #93402 ) ) ;
#62399 = ORIENTED_EDGE ( 'NONE', *, *, #51375, .F. ) ;
#62398 = CARTESIAN_POINT ( 'NONE',  ( 2.791683348922240793, 41.63393115100078745, 7.208316651077764092 ) ) ;
#62400 =( BOUNDED_CURVE ( )  B_SPLINE_CURVE ( 2, ( #84341, #84819, #68840, #91830, #97877, #372, #14362, #30323, #14864 ),
 .UNSPECIFIED., .F., .F. ) 
 B_SPLINE_CURVE_WITH_KNOTS ( ( 3, 2, 2, 2, 3 ),
 ( 0.1534289457926083233, 0.1547619047619047672, 0.1607142857142857262, 0.1666666666666666574, 0.1679996256359629347 ),
 .UNSPECIFIED. ) 
 CURVE ( )  GEOMETRIC_REPRESENTATION_ITEM ( )  RATIONAL_B_SPLINE_CURVE ( ( 0.9881565478350731180, 0.9923695281211489805, 1.000000000000000000, 0.9659258262890683122, 1.000000000000000000, 0.9659258262890683122, 1.000000000000000000, 0.9923695281211498687, 0.9881565478350742282 ) ) 
 REPRESENTATION_ITEM ( '' )  );
#62401 = AXIS2_PLACEMENT_3D ( 'NONE', #25584, #33542, #78078 ) ;
#62402 = CARTESIAN_POINT ( 'NONE',  ( 16.40814093676324603, 62.45696800326376064, -11.09922568453594671 ) ) ;
#62403 = CARTESIAN_POINT ( 'NONE',  ( 0.000000000000000000, 0.000000000000000000, 0.000000000000000000 ) ) ;
#62404 = CARTESIAN_POINT ( 'NONE',  ( 0.6178305044545838731, 19.74863466993042138, 9.382169495545420901 ) ) ;
#62405 = DIRECTION ( 'NONE',  ( 0.000000000000000000, 0.000000000000000000, -1.000000000000000000 ) ) ;
#62406 = CARTESIAN_POINT ( 'NONE',  ( 10.00000000000000000, 40.55374883491397497, -14.16423886937410082 ) ) ;
#62408 = CARTESIAN_POINT ( 'NONE',  ( 0.1532563361054083140, 1.008931151000784787, 1.131784320476157264E-15 ) ) ;
#62407 = PRESENTATION_LAYER_ASSIGNMENT (  '', '', ( #8123 ) ) ;
#62409 = CARTESIAN_POINT ( 'NONE',  ( -11.35178980618960409, 0.5000000000000004441, -9.804941009312079458 ) ) ;
#62410 = CARTESIAN_POINT ( 'NONE',  ( -2.266590686148945544, 37.22041550158063217, 7.082119434687048631 ) ) ;
#62411 =( GEOMETRIC_REPRESENTATION_CONTEXT ( 3 ) GLOBAL_UNCERTAINTY_ASSIGNED_CONTEXT ( ( #78198 ) ) GLOBAL_UNIT_ASSIGNED_CONTEXT ( ( #36411, #50418, #74895 ) ) REPRESENTATION_CONTEXT ( 'NONE', 'WORKASPACE' ) );
#62412 = CARTESIAN_POINT ( 'NONE',  ( 24.16423886937410614, 59.30374883491397497, 8.672049930838204340E-16 ) ) ;
#62413 = CARTESIAN_POINT ( 'NONE',  ( 6.204703633549690345, 17.84541550158063217, 14.16423886937410082 ) ) ;
#62415 = DIRECTION ( 'NONE',  ( -0.000000000000000000, -0.000000000000000000, 1.000000000000000000 ) ) ;
#62414 = CARTESIAN_POINT ( 'NONE',  ( 10.00000000000000000, 20.55374883491396787, -14.16423886937410082 ) ) ;
#62416 = CARTESIAN_POINT ( 'NONE',  ( -3.836325488035982278, 14.49999999999999112, -14.50112432709434351 ) ) ;
#62418 = CARTESIAN_POINT ( 'NONE',  ( 12.63842701281683922, 44.55059781766745175, -9.846743663894590881 ) ) ;
#62417 = CARTESIAN_POINT ( 'NONE',  ( 6.757497259948273438, -58.30388498758458127, 2.750000000000000000 ) ) ;
#62419 = ORIENTED_EDGE ( 'NONE', *, *, #9639, .F. ) ;
#62420 = CARTESIAN_POINT ( 'NONE',  ( 17.96484262340118221, 41.18868534415484106, -7.964842623401177768 ) ) ;
#62421 = CARTESIAN_POINT ( 'NONE',  ( -12.60589901313213979, 0.3639308464568737911, -8.129656208642234816 ) ) ;
#62422 = DIRECTION ( 'NONE',  ( -0.000000000000000000, -1.000000000000000000, -0.000000000000000000 ) ) ;
#62423 = CARTESIAN_POINT ( 'NONE',  ( 12.63842701281683922, 34.55059781766745886, -9.846743663894590881 ) ) ;
#62424 = CARTESIAN_POINT ( 'NONE',  ( 6.565887622018943937, 53.08196800326374643, -12.81628187352647608 ) ) ;
#62425 = CARTESIAN_POINT ( 'NONE',  ( 14.16423886937410437, -10.90458449841935717, 3.795296366450304770 ) ) ;
#62426 = CARTESIAN_POINT ( 'NONE',  ( 12.63842701281683922, 44.55059781766745175, -9.846743663894590881 ) ) ;
#62427 = CARTESIAN_POINT ( 'NONE',  ( 7.361572987183170547, 67.05059781766746596, 9.846743663894590881 ) ) ;
#62428 = EDGE_CURVE ( 'NONE', #85153, #88314, #73540, .T. ) ;
#62429 = ORIENTED_EDGE ( 'NONE', *, *, #66244, .F. ) ;
#62430 = CARTESIAN_POINT ( 'NONE',  ( -4.164238869374099927, 12.01208216824730357, 3.795296366450308767 ) ) ;
#62432 = CARTESIAN_POINT ( 'NONE',  ( 0.000000000000000000, 15.00000000000000000, 0.000000000000000000 ) ) ;
#62431 = CARTESIAN_POINT ( 'NONE',  ( -9.240973841163453883, 4.157471065789850032E-16, -11.17382667070385160 ) ) ;
#62433 = CARTESIAN_POINT ( 'NONE',  ( 20.88017736071110519, 10.56368534415483929, 2.639326808657452039E-16 ) ) ;
#62434 = CARTESIAN_POINT ( 'NONE',  ( 6.565887622018943937, 10.16530133659708746, 12.81628187352647430 ) ) ;
#62435 = ADVANCED_FACE ( 'NONE', ( #89024 ), #33710, .T. ) ;
#62436 = SURFACE_STYLE_FILL_AREA ( #25462 ) ;
#62437 = CARTESIAN_POINT ( 'NONE',  ( 12.91533473730992121, 64.52201867748817676, 10.88017736071110164 ) ) ;
#62438 = CARTESIAN_POINT ( 'NONE',  ( 4.471658927162282637, -3.629165645957387554, -4.000000000000000000 ) ) ;
#62439 = CARTESIAN_POINT ( 'NONE',  ( -46.58521628013341598, 101.6760492933278215, -7.987317478326372289 ) ) ;
#62440 = CARTESIAN_POINT ( 'NONE',  ( 0.1922240491738435031, 43.18878173731741299, 6.499999999999968914 ) ) ;
#62441 = CARTESIAN_POINT ( 'NONE',  ( 4.559911319644449179, 2.230352010821504916, -9.422509992056141925 ) ) ;
#62442 = CARTESIAN_POINT ( 'NONE',  ( 0.000000000000000000, 14.49999999999999822, 0.000000000000000000 ) ) ;
#62443 = CARTESIAN_POINT ( 'NONE',  ( 12.91533473730992121, 24.52201867748816966, 10.88017736071110164 ) ) ;
#62444 = CARTESIAN_POINT ( 'NONE',  ( 7.084665262690076126, 27.02201867748817676, -10.88017736071110164 ) ) ;
#62445 = CARTESIAN_POINT ( 'NONE',  ( 19.38216949554541202, 5.998634669930420493, 9.382169495545424454 ) ) ;
#62446 = CARTESIAN_POINT ( 'NONE',  ( 0.1532563361054100626, 55.80059781766745175, -2.638427012816831230 ) ) ;
#62447 = CARTESIAN_POINT ( 'NONE',  ( 21.09922568453594849, 61.20696800326376064, 6.408140936763242479 ) ) ;
#62448 = ORIENTED_EDGE ( 'NONE', *, *, #2058, .F. ) ;
#62449 = TOROIDAL_SURFACE ( 'NONE', #32111, 14.49999999999999822, 0.5000000000000000000 ) ;
#62450 = PRESENTATION_LAYER_ASSIGNMENT (  '', '', ( #46543 ) ) ;
#62451 = CARTESIAN_POINT ( 'NONE',  ( 17.96484262340118221, 29.93868534415484106, 7.964842623401181321 ) ) ;
#62452 = CARTESIAN_POINT ( 'NONE',  ( 21.09922568453595559, 27.04030133659708568, -6.408140936763230044 ) ) ;
#62453 = FACE_OUTER_BOUND ( 'NONE', #33601, .T. ) ;
#62454 =( GEOMETRIC_REPRESENTATION_CONTEXT ( 3 ) GLOBAL_UNCERTAINTY_ASSIGNED_CONTEXT ( ( #35266 ) ) GLOBAL_UNIT_ASSIGNED_CONTEXT ( ( #55945, #40457, #17943 ) ) REPRESENTATION_CONTEXT ( 'NONE', 'WORKASPACE' ) );
#62455 = CARTESIAN_POINT ( 'NONE',  ( 19.84674366389459266, 58.30059781766745886, 2.638427012816836559 ) ) ;
#62456 = CARTESIAN_POINT ( 'NONE',  ( 7.084665262690076126, 49.10535201082149825, 10.88017736071109987 ) ) ;
#62457 = CARTESIAN_POINT ( 'NONE',  ( 1.472469842513823179, 10.59226448433411782, -4.923371831947296329 ) ) ;
#62458 = CARTESIAN_POINT ( 'NONE',  ( 3.591859063236763294, 38.29030133659708923, -11.09922568453595026 ) ) ;
#62460 = CARTESIAN_POINT ( 'NONE',  ( 12.98685442714199390, 3.839196892837649736E-16, -6.449155920600954772 ) ) ;
#62459 = CARTESIAN_POINT ( 'NONE',  ( 20.88017736071110519, 60.56368534415484106, 2.639326808657452039E-16 ) ) ;
#62461 = CARTESIAN_POINT ( 'NONE',  ( 0.000000000000000000, 14.49999999999999822, 0.000000000000000000 ) ) ;
#62462 = EDGE_LOOP ( 'NONE', ( #89376, #35415, #59486, #21390 ) ) ;
#62463 = PRESENTATION_STYLE_ASSIGNMENT (( #32469 ) ) ;
#62464 = DIRECTION ( 'NONE',  ( -0.000000000000000000, -0.000000000000000000, 1.000000000000000000 ) ) ;
#62465 = CARTESIAN_POINT ( 'NONE',  ( -0.8801773607111008646, 13.27201867748817143, 2.915334737309923430 ) ) ;
#62467 = CARTESIAN_POINT ( 'NONE',  ( 6.204703633549690345, 15.76208216824730179, -14.16423886937410259 ) ) ;
#62466 = CARTESIAN_POINT ( 'NONE',  ( -1.099225684535947600, 49.54030133659708923, 6.408140936763237150 ) ) ;
#62468 = CARTESIAN_POINT ( 'NONE',  ( 10.00000000000000000, 14.75893115100078568, -9.846743663894594434 ) ) ;
#62469 = ADVANCED_FACE ( 'NONE', ( #12530 ), #69486, .F. ) ;
#62470 = CARTESIAN_POINT ( 'NONE',  ( 19.84674366389459266, 18.71726448433411960, -2.638427012816827677 ) ) ;
#62471 = CARTESIAN_POINT ( 'NONE',  ( 0.000000000000000000, 99.99999999999998579, 7.750000000000000000 ) ) ;
#62472 = CARTESIAN_POINT ( 'NONE',  ( 6.204703633549690345, 50.76208216824730357, -14.16423886937410259 ) ) ;
#62473 = VERTEX_POINT ( 'NONE', #76976 ) ;
#62474 = COLOUR_RGB ( '', 0.08235294, 0.09019608, 0.10196078) ;
#62475 = DIRECTION ( 'NONE',  ( -0.6225146366376129725, 0.000000000000000000, -0.7826081568524191345 ) ) ;
#62476 = ADVANCED_FACE ( 'NONE', ( #90490 ), #81604, .F. ) ;
#62477 = CARTESIAN_POINT ( 'NONE',  ( 0.5774900079438590739, 2.647018677488170990, -5.440088680355550821 ) ) ;
#62478 = DIRECTION ( 'NONE',  ( 0.000000000000000000, 1.000000000000000000, 0.000000000000000000 ) ) ;
#62479 = AXIS2_PLACEMENT_3D ( 'NONE', #68505, #46000, #22027 ) ;
#62480 = VERTEX_POINT ( 'NONE', #8004 ) ;
#62481 = ORIENTED_EDGE ( 'NONE', *, *, #60095, .F. ) ;
#62482 = CARTESIAN_POINT ( 'NONE',  ( 12.91533473730993009, 11.60535201082150714, -10.88017736071109987 ) ) ;
#62483 = CARTESIAN_POINT ( 'NONE',  ( -0.8801773607111008646, 13.27201867748817321, 2.915334737309923430 ) ) ;
#62484 = CARTESIAN_POINT ( 'NONE',  ( 12.63842701281683922, 39.55059781766744464, -9.846743663894590881 ) ) ;
#62485 = CARTESIAN_POINT ( 'NONE',  ( 22.81628187352647785, 51.62363466993042493, 6.195893100308588602E-16 ) ) ;
#62486 = FILL_AREA_STYLE_COLOUR ( '', #71624 ) ;
#62488 = CARTESIAN_POINT ( 'NONE',  ( 10.00000000000000000, 25.55374883491396787, -14.16423886937410082 ) ) ;
#62487 = CARTESIAN_POINT ( 'NONE',  ( 17.39651004071841456, 64.08210964143329136, -6.500000000000001776 ) ) ;
#62489 = CARTESIAN_POINT ( 'NONE',  ( 10.00000000000000000, 26.81368534415484106, -10.88017736071110342 ) ) ;
#62490 = CARTESIAN_POINT ( 'NONE',  ( 10.00000000000000000, 6.813685344154838397, -10.88017736071110342 ) ) ;
#62491 = CARTESIAN_POINT ( 'NONE',  ( 19.84674366389459266, 43.30059781766744464, 2.638427012816836559 ) ) ;
#62492 = LINE ( 'NONE', #24032, #9318 ) ;
#62493 = CARTESIAN_POINT ( 'NONE',  ( 7.361572987183170547, 32.05059781766745175, 9.846743663894590881 ) ) ;
#62494 = LINE ( 'NONE', #10009, #35086 ) ;
#62495 = CARTESIAN_POINT ( 'NONE',  ( 0.000000000000000000, -97.00000000000000000, -4.000000000000000000 ) ) ;
#62496 = CARTESIAN_POINT ( 'NONE',  ( -2.638427012816840111, 24.96726448433411960, -9.846743663894590881 ) ) ;
#62497 = ORIENTED_EDGE ( 'NONE', *, *, #91988, .T. ) ;
#62498 = CIRCLE ( 'NONE', #97649, 19.99999999999999645 ) ;
#62499 = DIRECTION ( 'NONE',  ( 0.000000000000000000, 0.000000000000000000, -1.000000000000000000 ) ) ;
#62500 = CARTESIAN_POINT ( 'NONE',  ( 0.5774900079438607392, 68.48035201082150536, 5.440088680355550821 ) ) ;
#62501 = CARTESIAN_POINT ( 'NONE',  ( 14.92337183194729988, 54.34226448433412315, -8.527530157486177487 ) ) ;
#62502 = CARTESIAN_POINT ( 'NONE',  ( 10.00000000000000000, 46.81368534415484106, -10.88017736071110342 ) ) ;
#62504 = CARTESIAN_POINT ( 'NONE',  ( 0.6178305044545818747, 43.49863466993042493, -9.382169495545419124 ) ) ;
#62503 = CARTESIAN_POINT ( 'NONE',  ( 15.44008868035555793, 11.39701867748817143, -9.422509992056140149 ) ) ;
#62505 = CARTESIAN_POINT ( 'NONE',  ( 17.08211943468705130, 18.47041550158063572, 12.26659068614894998 ) ) ;
#62506 = CARTESIAN_POINT ( 'NONE',  ( 13.43411237798105340, 40.58196800326375353, 12.81628187352647963 ) ) ;
#62507 = EDGE_LOOP ( 'NONE', ( #97624, #31047, #13437, #3017, #77724, #7323 ) ) ;
#62508 = CARTESIAN_POINT ( 'NONE',  ( 1.472469842513823179, 60.59226448433412315, -4.923371831947296329 ) ) ;
#62509 = CARTESIAN_POINT ( 'NONE',  ( 12.91533473730992121, 14.52201867748817143, 10.88017736071110164 ) ) ;
#62510 = ORIENTED_EDGE ( 'NONE', *, *, #655, .F. ) ;
#62511 = CARTESIAN_POINT ( 'NONE',  ( 7.084665262690076126, 29.10535201082150181, 10.88017736071109987 ) ) ;
#62512 = ORIENTED_EDGE ( 'NONE', *, *, #27915, .F. ) ;
#62513 = CARTESIAN_POINT ( 'NONE',  ( 12.91533473730992121, 64.52201867748817676, 10.88017736071110164 ) ) ;
#62514 = CARTESIAN_POINT ( 'NONE',  ( 7.084665262690076126, 2.022018677488170990, -10.88017736071110164 ) ) ;
#62515 = CARTESIAN_POINT ( 'NONE',  ( 5.795997163830076460, 15.00000000000000000, 13.01802277140709663 ) ) ;
#62516 = CARTESIAN_POINT ( 'NONE',  ( 1.472469842513823179, 5.592264484334118713, -4.923371831947296329 ) ) ;
#62517 = CARTESIAN_POINT ( 'NONE',  ( 17.20831665107776587, 2.883931151000785231, 7.208316651077764980 ) ) ;
#62518 = DIRECTION ( 'NONE',  ( 0.000000000000000000, 1.000000000000000000, 0.000000000000000000 ) ) ;
#62519 = EDGE_CURVE ( 'NONE', #19933, #92892, #25756, .T. ) ;
#62520 = CARTESIAN_POINT ( 'NONE',  ( -46.94000000000000483, 100.7316555907688809, 8.991040189367279112 ) ) ;
#62522 = EDGE_LOOP ( 'NONE', ( #50238, #18359, #87291, #78047 ) ) ;
#62521 = CARTESIAN_POINT ( 'NONE',  ( 0.1532563361054083140, 11.00893115100078568, 1.131784320476157264E-15 ) ) ;
#62523 =( GEOMETRIC_REPRESENTATION_CONTEXT ( 3 ) GLOBAL_UNCERTAINTY_ASSIGNED_CONTEXT ( ( #12489 ) ) GLOBAL_UNIT_ASSIGNED_CONTEXT ( ( #17357, #18822, #10826 ) ) REPRESENTATION_CONTEXT ( 'NONE', 'WORKASPACE' ) );
#62524 = CARTESIAN_POINT ( 'NONE',  ( 0.1532563361054100626, 35.80059781766745175, -2.638427012816831230 ) ) ;
#62525 = VERTEX_POINT ( 'NONE', #52019 ) ;
#62526 = ORIENTED_EDGE ( 'NONE', *, *, #72467, .T. ) ;
#62527 = CARTESIAN_POINT ( 'NONE',  ( 0.000000000000000000, 15.00000000000000000, 0.000000000000000000 ) ) ;
#62528 = CARTESIAN_POINT ( 'NONE',  ( 10.00000000000000000, 5.553748834913967869, -14.16423886937410082 ) ) ;
#62529 = CARTESIAN_POINT ( 'NONE',  ( 16.40814093676324603, 57.45696800326375353, -11.09922568453594671 ) ) ;
#62530 = CARTESIAN_POINT ( 'NONE',  ( 10.00000000000000000, 5.553748834913967869, -14.16423886937410082 ) ) ;
#62531 = CARTESIAN_POINT ( 'NONE',  ( 2.917880565312950480, 20.97041550158063217, -12.26659068614894821 ) ) ;
#62532 = PLANE ( 'NONE',  #49062 ) ;
#62534 = CARTESIAN_POINT ( 'NONE',  ( 2.035157376598824452, 63.68868534415484106, 7.964842623401179544 ) ) ;
#62533 = FACE_OUTER_BOUND ( 'NONE', #47989, .T. ) ;
#62535 = CARTESIAN_POINT ( 'NONE',  ( -0.8801773607110991993, 17.85535201082150536, -2.915334737309923874 ) ) ;
#62536 = FACE_OUTER_BOUND ( 'NONE', #57675, .T. ) ;
#62537 = ORIENTED_EDGE ( 'NONE', *, *, #7939, .T. ) ;
#62538 = CARTESIAN_POINT ( 'NONE',  ( 1.472469842513823179, 1.425597817667451528, 4.923371831947296329 ) ) ;
#62539 = CARTESIAN_POINT ( 'NONE',  ( 0.1532563361054100626, 5.800597817667452638, -2.638427012816831230 ) ) ;
#62540 = CARTESIAN_POINT ( 'NONE',  ( -2.816281873526471635, 28.91530133659708213, -3.434112377981056508 ) ) ;
#62541 = CARTESIAN_POINT ( 'NONE',  ( 17.20831665107776587, 39.13393115100079456, -7.208316651077762316 ) ) ;
#62542 = CARTESIAN_POINT ( 'NONE',  ( 19.38216949554541202, 15.99863466993042138, 9.382169495545424454 ) ) ;
#62543 = CARTESIAN_POINT ( 'NONE',  ( 0.2076750170234817061, 14.95077488074853811, 14.75137184266415247 ) ) ;
#62544 = MECHANICAL_DESIGN_GEOMETRIC_PRESENTATION_REPRESENTATION (  '', ( #49765 ), #67339 ) ;
#62545 = CARTESIAN_POINT ( 'NONE',  ( 5.076628168052704559, 10.17559781766745175, -8.527530157486179263 ) ) ;
#62546 = ADVANCED_FACE ( 'NONE', ( #68011 ), #15022, .F. ) ;
#62547 = ORIENTED_EDGE ( 'NONE', *, *, #97728, .T. ) ;
#62548 = ORIENTED_EDGE ( 'NONE', *, *, #40534, .T. ) ;
#62549 = CARTESIAN_POINT ( 'NONE',  ( 4.559911319644449179, 33.89701867748817676, 9.422509992056141925 ) ) ;
#62550 = CARTESIAN_POINT ( 'NONE',  ( -4.164238869374098151, 36.59541550158063217, -3.795296366450310543 ) ) ;
#62551 = CARTESIAN_POINT ( 'NONE',  ( 12.63842701281683034, 42.46726448433412315, 9.846743663894596210 ) ) ;
#62552 = CARTESIAN_POINT ( 'NONE',  ( 19.42250999205614548, 65.98035201082151957, -5.440088680355545492 ) ) ;
#62553 = MECHANICAL_DESIGN_GEOMETRIC_PRESENTATION_REPRESENTATION (  '', ( #70570 ), #69006 ) ;
#62555 = CARTESIAN_POINT ( 'NONE',  ( -6.560019409699617832, -50.64698701990471363, -3.750000000000000000 ) ) ;
#62554 = CARTESIAN_POINT ( 'NONE',  ( -1.099225684535947600, 49.54030133659708923, 6.408140936763237150 ) ) ;
#62556 = CARTESIAN_POINT ( 'NONE',  ( 12.91533473730992121, 24.52201867748816966, 10.88017736071110164 ) ) ;
#62557 = EDGE_CURVE ( 'NONE', #22303, #24915, #98538, .T. ) ;
#62558 = CARTESIAN_POINT ( 'NONE',  ( -0.9940297508535884674, 0.000000000000000000, -14.21528771620250886 ) ) ;
#62559 = CARTESIAN_POINT ( 'NONE',  ( 16.40814093676323893, 25.79030133659708923, 11.09922568453595026 ) ) ;
#62560 = CARTESIAN_POINT ( 'NONE',  ( 7.361572987183170547, 42.05059781766745886, 9.846743663894590881 ) ) ;
#62561 = CARTESIAN_POINT ( 'NONE',  ( -10.88017736071110342, 3.063685344154846835, 3.903127820947815962E-15 ) ) ;
#62562 = CARTESIAN_POINT ( 'NONE',  ( 22.81628187352647785, 51.62363466993042493, 6.195893100308588602E-16 ) ) ;
#62563 = FACE_OUTER_BOUND ( 'NONE', #27820, .T. ) ;
#62564 = TOROIDAL_SURFACE ( 'NONE', #48150, 14.49999999999999822, 0.5000000000000000000 ) ;
#62566 = LINE ( 'NONE', #69106, #92719 ) ;
#62565 = CARTESIAN_POINT ( 'NONE',  ( 10.00000000000000000, 51.81368534415484106, -10.88017736071110342 ) ) ;
#62567 = DIRECTION ( 'NONE',  ( -0.000000000000000000, -1.000000000000000000, -0.000000000000000000 ) ) ;
#62568 = PLANE ( 'NONE',  #22542 ) ;
#62569 = CARTESIAN_POINT ( 'NONE',  ( -0.8801773607111008646, 58.27201867748816966, 2.915334737309923430 ) ) ;
#62570 = CARTESIAN_POINT ( 'NONE',  ( 0.5774900079438590739, 57.64701867748817676, -5.440088680355550821 ) ) ;
#62571 = CARTESIAN_POINT ( 'NONE',  ( 34.56412365047464874, 29.50000000000000000, -9.500000000000000000 ) ) ;
#62572 = SURFACE_STYLE_USAGE ( .BOTH. , #63070 ) ;
#62573 = CARTESIAN_POINT ( 'NONE',  ( -0.8801773607111008646, 3.272018677488171434, 2.915334737309923430 ) ) ;
#62574 = CARTESIAN_POINT ( 'NONE',  ( 18.52753015748617571, 58.09226448433411605, 4.923371831947298993 ) ) ;
#62576 = CARTESIAN_POINT ( 'NONE',  ( -10.39655283154092125, 0.04922511925147211170, 10.46698568711257771 ) ) ;
#62575 = CARTESIAN_POINT ( 'NONE',  ( 15.44008868035555260, 19.73035201082150536, 9.422509992056143702 ) ) ;
#62577 = CARTESIAN_POINT ( 'NONE',  ( 19.38216949554541202, 20.99863466993042138, 9.382169495545424454 ) ) ;
#62578 = ORIENTED_EDGE ( 'NONE', *, *, #71722, .F. ) ;
#62579 = CARTESIAN_POINT ( 'NONE',  ( 12.91533473730993009, 31.60535201082150891, -10.88017736071109987 ) ) ;
#62580 = CARTESIAN_POINT ( 'NONE',  ( 13.43411237798105340, 5.581968003263753531, 12.81628187352647963 ) ) ;
#62581 = CARTESIAN_POINT ( 'NONE',  ( 4.559911319644449179, 12.23035201082150536, -9.422509992056141925 ) ) ;
#62582 = CARTESIAN_POINT ( 'NONE',  ( 15.44008868035555260, 44.73035201082151247, 9.422509992056143702 ) ) ;
#62583 = CARTESIAN_POINT ( 'NONE',  ( 6.204703633549690345, 45.76208216824729647, -14.16423886937410259 ) ) ;
#62584 = CARTESIAN_POINT ( 'NONE',  ( 0.1532563361054082862, 36.21726448433410894, 2.638427012816831674 ) ) ;
#62585 = CARTESIAN_POINT ( 'NONE',  ( 10.00000000000000178, 54.31368534415484106, 10.88017736071110342 ) ) ;
#62586 = CYLINDRICAL_SURFACE ( 'NONE', #5911, 0.5000000000000004441 ) ;
#62587 = CARTESIAN_POINT ( 'NONE',  ( -4.164238869374098151, 16.59541550158063927, -3.795296366450310543 ) ) ;
#62588 = EDGE_CURVE ( 'NONE', #14583, #84680, #44995, .T. ) ;
#62589 = DIRECTION ( 'NONE',  ( 0.000000000000000000, 1.000000000000000000, 0.000000000000000000 ) ) ;
#62590 = ORIENTED_EDGE ( 'NONE', *, *, #21380, .T. ) ;
#62591 = ORIENTED_EDGE ( 'NONE', *, *, #10058, .F. ) ;
#62592 = AXIS2_PLACEMENT_3D ( 'NONE', #45032, #67559, #43070 ) ;
#62593 = CARTESIAN_POINT ( 'NONE',  ( 20.36894250292379738, 34.92874883491396076, -10.36894250292379027 ) ) ;
#62594 = CARTESIAN_POINT ( 'NONE',  ( 22.26659068614894466, 38.88708216824731068, 7.082119434687054849 ) ) ;
#62595 = CARTESIAN_POINT ( 'NONE',  ( 14.92337183194729633, 2.675597817667451750, 8.527530157486181039 ) ) ;
#62596 = CARTESIAN_POINT ( 'NONE',  ( 17.20831665107776587, 64.13393115100079456, -7.208316651077762316 ) ) ;
#62597 = DIRECTION ( 'NONE',  ( -1.000000000000000000, 0.000000000000000000, 0.000000000000000000 ) ) ;
#62599 = CARTESIAN_POINT ( 'NONE',  ( 19.38216949554541557, 27.24863466993041783, -9.382169495545420901 ) ) ;
#62598 = CARTESIAN_POINT ( 'NONE',  ( -0.8801773607111009756, 53.06368534415484106, 1.068504757029289695E-15 ) ) ;
#62600 = CARTESIAN_POINT ( 'NONE',  ( 2.917880565312950480, 30.97041550158063572, -12.26659068614894821 ) ) ;
#62601 = CARTESIAN_POINT ( 'NONE',  ( 10.00000000000000000, 21.81368534415484106, -10.88017736071110342 ) ) ;
#62602 = CARTESIAN_POINT ( 'NONE',  ( 0.000000000000000000, 15.00000000000000000, 0.000000000000000000 ) ) ;
#62603 = FACE_OUTER_BOUND ( 'NONE', #48346, .T. ) ;
#62604 = CARTESIAN_POINT ( 'NONE',  ( -9.846743663894594434, -13.99106884899921432, 3.469446951953614189E-15 ) ) ;
#62605 = ORIENTED_EDGE ( 'NONE', *, *, #10297, .F. ) ;
#62606 = FACE_OUTER_BOUND ( 'NONE', #24738, .T. ) ;
#62607 = ORIENTED_EDGE ( 'NONE', *, *, #81288, .T. ) ;
#62608 = CARTESIAN_POINT ( 'NONE',  ( 0.000000000000000000, 0.5000000000000004441, 0.000000000000000000 ) ) ;
#62609 = ORIENTED_EDGE ( 'NONE', *, *, #51144, .F. ) ;
#62610 = CARTESIAN_POINT ( 'NONE',  ( 20.36894250292379738, 4.928748834913967869, -10.36894250292379027 ) ) ;
#62612 = CARTESIAN_POINT ( 'NONE',  ( 19.42250999205614548, 10.98035201082150536, -5.440088680355545492 ) ) ;
#62611 = CARTESIAN_POINT ( 'NONE',  ( 13.79529636645030344, 53.26208216824730357, 14.16423886937410614 ) ) ;
#62614 = CARTESIAN_POINT ( 'NONE',  ( 14.92337183194729633, 57.67559781766745886, 8.527530157486181039 ) ) ;
#62613 = CARTESIAN_POINT ( 'NONE',  ( 2.791683348922237240, 35.38393115100079456, -7.208316651077763204 ) ) ;
#62615 = CARTESIAN_POINT ( 'NONE',  ( 20.15039907845753575, 59.72266099184918176, 6.262539305110074395 ) ) ;
#62616 = CARTESIAN_POINT ( 'NONE',  ( -14.16722289976683946, 14.49999999999999112, -4.928467845925748492 ) ) ;
#62617 = CARTESIAN_POINT ( 'NONE',  ( 0.6178305044545838731, -0.2513653300695798953, 9.382169495545420901 ) ) ;
#62618 = CARTESIAN_POINT ( 'NONE',  ( -12.81628187352647252, 29.33196800326377840, 3.434112377981066722 ) ) ;
#62619 = VERTEX_POINT ( 'NONE', #98033 ) ;
#62620 = MECHANICAL_DESIGN_GEOMETRIC_PRESENTATION_REPRESENTATION (  '', ( #94609 ), #75411 ) ;
#62621 = AXIS2_PLACEMENT_3D ( 'NONE', #74592, #7095, #20111 ) ;
#62622 = CARTESIAN_POINT ( 'NONE',  ( 22.26659068614894466, 43.88708216824729647, 7.082119434687054849 ) ) ;
#62623 = ORIENTED_EDGE ( 'NONE', *, *, #7907, .F. ) ;
#62624 = COLOUR_RGB ( '', 0.72549020, 0.75294118, 0.79215686) ;
#62625 = CARTESIAN_POINT ( 'NONE',  ( -0.3689425029237881626, 42.42874883491396787, 10.36894250292379027 ) ) ;
#62626 = ORIENTED_EDGE ( 'NONE', *, *, #80132, .T. ) ;
#62627 = CARTESIAN_POINT ( 'NONE',  ( 20.88017736071110875, 25.77201867748816966, -2.915334737309920765 ) ) ;
#62628 = DIRECTION ( 'NONE',  ( 0.000000000000000000, 1.000000000000000000, 0.000000000000000000 ) ) ;
#62629 = CARTESIAN_POINT ( 'NONE',  ( 4.559911319644449179, 32.23035201082150536, -9.422509992056141925 ) ) ;
#62630 = CARTESIAN_POINT ( 'NONE',  ( 17.20831665107776587, 49.13393115100078745, -7.208316651077762316 ) ) ;
#62631 = CARTESIAN_POINT ( 'NONE',  ( 20.88017736071110875, 40.77201867748818387, -2.915334737309920765 ) ) ;
#62632 = CIRCLE ( 'NONE', #41890, 0.2500000000000002220 ) ;
#62633 = CARTESIAN_POINT ( 'NONE',  ( 2.035157376598822676, 62.43868534415483396, -7.964842623401177768 ) ) ;
#62634 = CARTESIAN_POINT ( 'NONE',  ( 2.035157376598824452, 33.68868534415484106, 7.964842623401179544 ) ) ;
#62635 = ADVANCED_FACE ( 'NONE', ( #14526 ), #7014, .F. ) ;
#62636 =( GEOMETRIC_REPRESENTATION_CONTEXT ( 3 ) GLOBAL_UNCERTAINTY_ASSIGNED_CONTEXT ( ( #8138 ) ) GLOBAL_UNIT_ASSIGNED_CONTEXT ( ( #18710, #73159, #78716 ) ) REPRESENTATION_CONTEXT ( 'NONE', 'WORKASPACE' ) );
#62637 = CARTESIAN_POINT ( 'NONE',  ( 0.000000000000000000, 15.00000000000000000, 0.000000000000000000 ) ) ;
#62638 = SURFACE_STYLE_FILL_AREA ( #60679 ) ;
#62639 = DIRECTION ( 'NONE',  ( 0.000000000000000000, 0.000000000000000000, 1.000000000000000000 ) ) ;
#62640 = ORIENTED_EDGE ( 'NONE', *, *, #416, .F. ) ;
#62641 = EDGE_CURVE ( 'NONE', #53155, #35322, #8489, .T. ) ;
#62642 = CARTESIAN_POINT ( 'NONE',  ( -8.000000000000000000, 0.000000000000000000, 4.000000000000000000 ) ) ;
#62643 = CARTESIAN_POINT ( 'NONE',  ( 19.84674366389459266, 38.71726448433412315, -2.638427012816827677 ) ) ;
#62644 = ADVANCED_FACE ( 'NONE', ( #29990 ), #38994, .F. ) ;
#62645 = DIRECTION ( 'NONE',  ( 1.000000000000000000, 2.081668171172167567E-14, 0.000000000000000000 ) ) ;
#62646 = DIRECTION ( 'NONE',  ( 1.000000000000000000, 0.000000000000000000, 0.000000000000000000 ) ) ;
#62647 = AXIS2_PLACEMENT_3D ( 'NONE', #92417, #59943, #77403 ) ;
#62648 = CYLINDRICAL_SURFACE ( 'NONE', #90606, 15.00000000000000000 ) ;
#62649 = EDGE_LOOP ( 'NONE', ( #44, #81161, #52907, #89516 ) ) ;
#62650 = CARTESIAN_POINT ( 'NONE',  ( 0.5600000000000083800, 105.0000000000000000, 5.000000000000000000 ) ) ;
#62651 = CARTESIAN_POINT ( 'NONE',  ( 0.8952175423694801459, 52.60160829253886305, -5.990408912944315212 ) ) ;
#62652 = CARTESIAN_POINT ( 'NONE',  ( 18.52753015748618282, 53.92559781766745175, -4.923371831947291888 ) ) ;
#62653 = CARTESIAN_POINT ( 'NONE',  ( 13.79529636645031943, 45.34541550158062506, -14.16423886937409904 ) ) ;
#62654 = CARTESIAN_POINT ( 'NONE',  ( 14.92337183194729988, 64.34226448433412315, -8.527530157486177487 ) ) ;
#62655 = VERTEX_POINT ( 'NONE', #59997 ) ;
#62656 = CARTESIAN_POINT ( 'NONE',  ( 18.00000000000000000, 78.80384757729335377, -3.750000000000000000 ) ) ;
#62657 = CARTESIAN_POINT ( 'NONE',  ( 10.00000000000000000, 14.75893115100078568, -9.846743663894594434 ) ) ;
#62658 = ADVANCED_FACE ( 'NONE', ( #23016 ), #75993, .F. ) ;
#62659 = CARTESIAN_POINT ( 'NONE',  ( 10.00000000000000000, 47.87363466993042493, -12.81628187352647608 ) ) ;
#62660 = CARTESIAN_POINT ( 'NONE',  ( 0.1532563361054083140, 66.00893115100079456, 1.131784320476157264E-15 ) ) ;
#62661 = CARTESIAN_POINT ( 'NONE',  ( -0.8801773607110991993, 57.85535201082149825, -2.915334737309923874 ) ) ;
#62662 = CARTESIAN_POINT ( 'NONE',  ( 4.380000000000000782, 0.09086787938152994515, -2.750000000000000888 ) ) ;
#62663 = AXIS2_PLACEMENT_3D ( 'NONE', #85894, #3378, #57350 ) ;
#62664 = EDGE_CURVE ( 'NONE', #66685, #43655, #45937, .T. ) ;
#62665 = EDGE_LOOP ( 'NONE', ( #56489, #12829, #91384, #85468 ) ) ;
#62666 = CARTESIAN_POINT ( 'NONE',  ( 6.204703633549690345, 65.76208216824731778, -14.16423886937410259 ) ) ;
#62667 = DIRECTION ( 'NONE',  ( 0.000000000000000000, -1.000000000000000000, 0.000000000000000000 ) ) ;
#62668 = CARTESIAN_POINT ( 'NONE',  ( -0.8801773607111009756, 23.06368534415484106, 1.068504757029289695E-15 ) ) ;
#62670 = CARTESIAN_POINT ( 'NONE',  ( 2.035157376598824452, 63.68868534415484106, 7.964842623401179544 ) ) ;
#62669 = CARTESIAN_POINT ( 'NONE',  ( 10.00000000000000178, 10.37363466993041961, 12.81628187352647608 ) ) ;
#62671 = LINE ( 'NONE', #40183, #60018 ) ;
#62672 = EDGE_CURVE ( 'NONE', #2288, #1302, #92508, .T. ) ;
#62673 = LINE ( 'NONE', #9688, #53932 ) ;
#62674 = FACE_OUTER_BOUND ( 'NONE', #70631, .T. ) ;
#62676 = DIRECTION ( 'NONE',  ( 0.08715574274765139351, 0.9961946980917461003, 0.000000000000000000 ) ) ;
#62675 = CARTESIAN_POINT ( 'NONE',  ( 20.88017736071110519, 50.56368534415484106, 2.639326808657452039E-16 ) ) ;
#62677 = CARTESIAN_POINT ( 'NONE',  ( 7.361572987183170547, 32.05059781766745175, 9.846743663894590881 ) ) ;
#62678 = CARTESIAN_POINT ( 'NONE',  ( 10.00000000000000000, -0.2410688489992152128, -9.846743663894594434 ) ) ;
#62679 = CARTESIAN_POINT ( 'NONE',  ( 10.88017736071109987, -34.22798132251183034, -2.915334737309928315 ) ) ;
#62680 = CARTESIAN_POINT ( 'NONE',  ( 6.565887622018943937, 15.16530133659708568, 12.81628187352647430 ) ) ;
#62681 = CARTESIAN_POINT ( 'NONE',  ( 17.96484262340118221, 14.93868534415484106, 7.964842623401181321 ) ) ;
#62682 = SURFACE_STYLE_FILL_AREA ( #70700 ) ;
#62683 = CARTESIAN_POINT ( 'NONE',  ( 17.08211943468705130, 38.47041550158063217, 12.26659068614894998 ) ) ;
#62684 = CARTESIAN_POINT ( 'NONE',  ( 20.36894250292379382, 33.67874883491396076, 10.36894250292379205 ) ) ;
#62685 = CARTESIAN_POINT ( 'NONE',  ( 2.035157376598822676, 2.438685344154838397, -7.964842623401177768 ) ) ;
#62686 = AXIS2_PLACEMENT_3D ( 'NONE', #26422, #65404, #97917 ) ;
#62687 = CARTESIAN_POINT ( 'NONE',  ( 1.472469842513823179, 21.42559781766745175, 4.923371831947296329 ) ) ;
#62688 = CARTESIAN_POINT ( 'NONE',  ( 2.035157376598822676, 7.438685344154837509, -7.964842623401177768 ) ) ;
#62689 = VERTEX_POINT ( 'NONE', #15993 ) ;
#62690 = CARTESIAN_POINT ( 'NONE',  ( 17.20831665107776587, 44.13393115100078745, -7.208316651077762316 ) ) ;
#62691 = CARTESIAN_POINT ( 'NONE',  ( 15.44008868035555793, 46.39701867748817676, -9.422509992056140149 ) ) ;
#62692 = CARTESIAN_POINT ( 'NONE',  ( 0.6178305044545818747, -1.501365330069579951, -9.382169495545419124 ) ) ;
#62694 = CARTESIAN_POINT ( 'NONE',  ( 2.603489959281613420, 60.43575266056826933, -6.500000000000031086 ) ) ;
#62693 = CARTESIAN_POINT ( 'NONE',  ( 24.16423886937410614, 24.30374883491396787, 8.672049930838204340E-16 ) ) ;
#62695 = CARTESIAN_POINT ( 'NONE',  ( -2.393480905992949381, 14.63595249122789177, -14.80781041047755409 ) ) ;
#62696 = CARTESIAN_POINT ( 'NONE',  ( 1.472469842513823179, 10.59226448433411782, -4.923371831947296329 ) ) ;
#62697 = CARTESIAN_POINT ( 'NONE',  ( 22.81628187352647785, 46.41530133659708213, 3.434112377981063169 ) ) ;
#62698 = CARTESIAN_POINT ( 'NONE',  ( 5.076628168052704559, 50.17559781766745886, -8.527530157486179263 ) ) ;
#62699 = ORIENTED_EDGE ( 'NONE', *, *, #37137, .T. ) ;
#62700 = COLOUR_RGB ( '', 0.72549020, 0.75294118, 0.79215686) ;
#62701 = CARTESIAN_POINT ( 'NONE',  ( 10.00000000000000178, 70.00000000000000000, 0.000000000000000000 ) ) ;
#62702 = DIRECTION ( 'NONE',  ( 0.000000000000000000, 1.000000000000000000, 0.000000000000000000 ) ) ;
#62703 = CARTESIAN_POINT ( 'NONE',  ( 12.91533473730993009, 6.605352010821504471, -10.88017736071109987 ) ) ;
#62704 = CARTESIAN_POINT ( 'NONE',  ( 15.44008868035555793, 51.39701867748816966, -9.422509992056140149 ) ) ;
#62705 = CARTESIAN_POINT ( 'NONE',  ( 22.26659068614894466, 13.88708216824730179, 7.082119434687054849 ) ) ;
#62706 = CARTESIAN_POINT ( 'NONE',  ( 0.5774900079438590739, 57.64701867748817676, -5.440088680355550821 ) ) ;
#62707 = CARTESIAN_POINT ( 'NONE',  ( 10.00000000000000178, 32.25893115100078745, 9.846743663894594434 ) ) ;
#62708 = CARTESIAN_POINT ( 'NONE',  ( 20.88017736071110875, 25.77201867748816966, -2.915334737309920765 ) ) ;
#62709 = CARTESIAN_POINT ( 'NONE',  ( -7.595945211628163385, 15.00000000000000000, -12.35117874301652030 ) ) ;
#62710 = CARTESIAN_POINT ( 'NONE',  ( 5.076628168052703671, 66.84226448433412315, 8.527530157486179263 ) ) ;
#62711 = ADVANCED_FACE ( 'NONE', ( #21525 ), #31951, .F. ) ;
#62712 = CARTESIAN_POINT ( 'NONE',  ( 0.1532563361054100626, 0.8005978176674514168, -2.638427012816831230 ) ) ;
#62713 = ORIENTED_EDGE ( 'NONE', *, *, #74082, .F. ) ;
#62714 = ORIENTED_EDGE ( 'NONE', *, *, #55391, .F. ) ;
#62715 = CARTESIAN_POINT ( 'NONE',  ( 14.47650479471825058, 14.49999999999999112, 3.928206833722148517 ) ) ;
#62716 = CARTESIAN_POINT ( 'NONE',  ( -9.159723438033054776, -0.03417435944610275333, -10.91613331444555079 ) ) ;
#62717 = CARTESIAN_POINT ( 'NONE',  ( -11.88139889192316900, -91.33459011216928047, 3.750000000000000000 ) ) ;
#62718 = CARTESIAN_POINT ( 'NONE',  ( -4.164238869374099039, 46.80374883491397497, 8.674139862899312516E-16 ) ) ;
#62719 = CARTESIAN_POINT ( 'NONE',  ( 19.84674366389459621, 38.50893115100078745, 7.409399052514197653E-17 ) ) ;
#62720 = CARTESIAN_POINT ( 'NONE',  ( 14.92337183194729988, 19.34226448433411960, -8.527530157486177487 ) ) ;
#62721 = CARTESIAN_POINT ( 'NONE',  ( 18.18329248733322956, 52.60290668512021739, 6.499999999999960920 ) ) ;
#62723 = CARTESIAN_POINT ( 'NONE',  ( 0.1532563361054082862, 51.21726448433412315, 2.638427012816831674 ) ) ;
#62722 = CARTESIAN_POINT ( 'NONE',  ( -0.8801773607111009756, 23.06368534415484106, 1.068504757029289695E-15 ) ) ;
#62724 = DIRECTION ( 'NONE',  ( 0.000000000000000000, 1.000000000000000000, 0.000000000000000000 ) ) ;
#62725 = CARTESIAN_POINT ( 'NONE',  ( -2.266590686148945544, 42.22041550158063217, 7.082119434687048631 ) ) ;
#62726 = CARTESIAN_POINT ( 'NONE',  ( 17.08211943468705840, 55.13708216824731068, -12.26659068614894466 ) ) ;
#62727 = CARTESIAN_POINT ( 'NONE',  ( 18.52753015748618282, 63.92559781766745886, -4.923371831947291888 ) ) ;
#62728 = CARTESIAN_POINT ( 'NONE',  ( 18.00000000000000000, 77.07179676972447169, 4.250000000000000000 ) ) ;
#62729 = CARTESIAN_POINT ( 'NONE',  ( 20.88017736071110875, 50.77201867748817676, -2.915334737309920765 ) ) ;
#62730 = CARTESIAN_POINT ( 'NONE',  ( 14.92337183194729988, 19.34226448433411960, -8.527530157486177487 ) ) ;
#62731 = VECTOR ( 'NONE', #31863, 1000.000000000000000 ) ;
#62732 = CARTESIAN_POINT ( 'NONE',  ( -5.331138373844170886, -28.69357394137554707, 4.000000000000000000 ) ) ;
#62733 = VERTEX_POINT ( 'NONE', #85471 ) ;
#62734 = CARTESIAN_POINT ( 'NONE',  ( -19.89999999999999858, 92.00000000000000000, 7.750000000000000000 ) ) ;
#62735 = EDGE_LOOP ( 'NONE', ( #98217, #62743, #7662, #40391 ) ) ;
#62736 = CARTESIAN_POINT ( 'NONE',  ( 18.52753015748618282, 13.92559781766745175, -4.923371831947291888 ) ) ;
#62737 = ORIENTED_EDGE ( 'NONE', *, *, #55835, .T. ) ;
#62738 = CARTESIAN_POINT ( 'NONE',  ( 2.917880565312950480, 20.97041550158063217, -12.26659068614894821 ) ) ;
#62739 = CARTESIAN_POINT ( 'NONE',  ( 5.076628168052704559, 20.17559781766745175, -8.527530157486179263 ) ) ;
#62740 = CARTESIAN_POINT ( 'NONE',  ( 7.084665262690076126, 39.10535201082150536, 10.88017736071109987 ) ) ;
#62741 = AXIS2_PLACEMENT_3D ( 'NONE', #36127, #79667, #20645 ) ;
#62742 = DIRECTION ( 'NONE',  ( 0.000000000000000000, 0.000000000000000000, 1.000000000000000000 ) ) ;
#62743 = ORIENTED_EDGE ( 'NONE', *, *, #53761, .T. ) ;
#62744 = CARTESIAN_POINT ( 'NONE',  ( 7.084665262690076126, 44.10535201082151247, 10.88017736071109987 ) ) ;
#62745 = VECTOR ( 'NONE', #33248, 1000.000000000000000 ) ;
#62746 = CARTESIAN_POINT ( 'NONE',  ( 14.99847009497944406, 0.5000000000000004441, 0.2142307401081381124 ) ) ;
#62747 = CARTESIAN_POINT ( 'NONE',  ( 12.81628187352647608, -3.584698663402908991, 3.434112377981052511 ) ) ;
#62748 = VERTEX_POINT ( 'NONE', #47947 ) ;
#62749 = CARTESIAN_POINT ( 'NONE',  ( 12.91533473730992121, 44.52201867748816966, 10.88017736071110164 ) ) ;
#62750 = CARTESIAN_POINT ( 'NONE',  ( 17.08211943468705130, 13.47041550158063572, 12.26659068614894998 ) ) ;
#62751 = ORIENTED_EDGE ( 'NONE', *, *, #18023, .T. ) ;
#62752 = CARTESIAN_POINT ( 'NONE',  ( 13.43411237798105340, 30.58196800326374998, 12.81628187352647963 ) ) ;
#62753 = CARTESIAN_POINT ( 'NONE',  ( 2.791683348922240793, 11.63393115100078568, 7.208316651077764092 ) ) ;
#62754 = CARTESIAN_POINT ( 'NONE',  ( 15.44008868035555793, 6.397018677488170546, -9.422509992056140149 ) ) ;
#62755 = EDGE_CURVE ( 'NONE', #40169, #68676, #2492, .T. ) ;
#62756 = CARTESIAN_POINT ( 'NONE',  ( 9.402796353261127393, 15.00000000000000000, -11.68706210897757103 ) ) ;
#62757 = CARTESIAN_POINT ( 'NONE',  ( 19.84674366389459266, 18.71726448433411960, -2.638427012816827677 ) ) ;
#62758 = CARTESIAN_POINT ( 'NONE',  ( 10.00000000000000178, 39.31368534415484106, 10.88017736071110342 ) ) ;
#62759 = TOROIDAL_SURFACE ( 'NONE', #33981, 0.5000000000000000000, 0.2500000000000000000 ) ;
#62760 = EDGE_CURVE ( 'NONE', #62619, #67069, #46966, .T. ) ;
#62761 = EDGE_LOOP ( 'NONE', ( #25645, #39644, #41715, #37471 ) ) ;
#62762 = EDGE_CURVE ( 'NONE', #50542, #23491, #48447, .T. ) ;
#62763 = EDGE_LOOP ( 'NONE', ( #44890, #60284, #85567, #45171 ) ) ;
#62764 = CARTESIAN_POINT ( 'NONE',  ( 17.35999999999999943, 37.99999999999997868, -9.500000000000000000 ) ) ;
#62765 = CARTESIAN_POINT ( 'NONE',  ( 15.44008868035555793, 51.39701867748816966, -9.422509992056140149 ) ) ;
#62766 = FACE_OUTER_BOUND ( 'NONE', #79995, .T. ) ;
#62767 = EDGE_CURVE ( 'NONE', #72922, #27809, #96064, .T. ) ;
#62768 = CARTESIAN_POINT ( 'NONE',  ( 6.565887622018943937, 65.16530133659709634, 12.81628187352647430 ) ) ;
#62769 = CARTESIAN_POINT ( 'NONE',  ( 19.42250999205614193, 60.14701867748817676, 5.440088680355555262 ) ) ;
#62770 = ADVANCED_FACE ( 'NONE', ( #70472 ), #48060, .T. ) ;
#62771 = VECTOR ( 'NONE', #45196, 1000.000000000000114 ) ;
#62772 = CARTESIAN_POINT ( 'NONE',  ( 3.591859063236761518, 9.956968003263753531, 11.09922568453594849 ) ) ;
#62774 = CARTESIAN_POINT ( 'NONE',  ( -0.1503990784575328643, 70.00000000000000000, -6.262539305110068177 ) ) ;
#62773 = CIRCLE ( 'NONE', #37248, 0.2500000000000002220 ) ;
#62775 = CARTESIAN_POINT ( 'NONE',  ( 5.076628168052704559, 35.17559781766745175, -8.527530157486179263 ) ) ;
#62776 = CARTESIAN_POINT ( 'NONE',  ( 1.683889348827610062E-15, 0.000000000000000000, 13.74999999999999467 ) ) ;
#62777 = CARTESIAN_POINT ( 'NONE',  ( -4.164238869374098151, 6.595415501580634832, -3.795296366450310543 ) ) ;
#62778 = CARTESIAN_POINT ( 'NONE',  ( 19.84674366389459621, 13.50893115100078568, 7.409399052514197653E-17 ) ) ;
#62779 = CARTESIAN_POINT ( 'NONE',  ( 21.09922568453594849, 26.20696800326375353, 6.408140936763242479 ) ) ;
#62780 = DIRECTION ( 'NONE',  ( 0.000000000000000000, -1.000000000000000000, 0.000000000000000000 ) ) ;
#62781 = CARTESIAN_POINT ( 'NONE',  ( 2.035157376598822676, 52.43868534415483396, -7.964842623401177768 ) ) ;
#62782 = CARTESIAN_POINT ( 'NONE',  ( 7.361572987183170547, 67.05059781766746596, 9.846743663894590881 ) ) ;
#62783 = EDGE_CURVE ( 'NONE', #14585, #38399, #55964, .T. ) ;
#62784 = CARTESIAN_POINT ( 'NONE',  ( 0.000000000000000000, -97.00000000000000000, 3.750000000000000000 ) ) ;
#62785 = CARTESIAN_POINT ( 'NONE',  ( 5.076628168052704559, 20.17559781766745175, -8.527530157486179263 ) ) ;
#62786 = CARTESIAN_POINT ( 'NONE',  ( 0.5774900079438590739, 17.64701867748817321, -5.440088680355550821 ) ) ;
#62787 = CARTESIAN_POINT ( 'NONE',  ( 10.00000000000000178, 15.37363466993042138, 12.81628187352647608 ) ) ;
#62788 = CARTESIAN_POINT ( 'NONE',  ( 2.791683348922237240, 25.38393115100078390, -7.208316651077763204 ) ) ;
#62789 = CARTESIAN_POINT ( 'NONE',  ( 0.000000000000000000, 14.49999999999999822, 0.000000000000000000 ) ) ;
#62790 = CARTESIAN_POINT ( 'NONE',  ( 17.96484262340118221, 21.18868534415483396, -7.964842623401177768 ) ) ;
#62791 = ORIENTED_EDGE ( 'NONE', *, *, #70485, .T. ) ;
#62792 = CARTESIAN_POINT ( 'NONE',  ( 17.96484262340118221, 66.18868534415483396, -7.964842623401177768 ) ) ;
#62793 = CARTESIAN_POINT ( 'NONE',  ( 4.380000000000002558, 0.09086787937427767692, 2.750000000000001332 ) ) ;
#62795 = CARTESIAN_POINT ( 'NONE',  ( 17.96484262340118221, 16.18868534415483396, -7.964842623401177768 ) ) ;
#62794 = CARTESIAN_POINT ( 'NONE',  ( 10.00000000000000000, 44.75893115100078745, -9.846743663894594434 ) ) ;
#62796 = EDGE_CURVE ( 'NONE', #47024, #6299, #31466, .T. ) ;
#62797 = CARTESIAN_POINT ( 'NONE',  ( 12.91533473730992121, 49.52201867748817676, 10.88017736071110164 ) ) ;
#62798 = CARTESIAN_POINT ( 'NONE',  ( 7.084665262690076126, 19.10535201082150181, 10.88017736071109987 ) ) ;
#62799 = CARTESIAN_POINT ( 'NONE',  ( 10.00000000000000000, 9.758931151000785675, -9.846743663894594434 ) ) ;
#62800 = CARTESIAN_POINT ( 'NONE',  ( 7.361572987183169658, 44.96726448433412315, -9.846743663894592657 ) ) ;
#62801 = CARTESIAN_POINT ( 'NONE',  ( 5.378451019861598681, 0.000000000000000000, -0.9000440264802418433 ) ) ;
#62802 = CARTESIAN_POINT ( 'NONE',  ( -7.749999999999996447, 83.99999999999994316, 3.750000000000000000 ) ) ;
#62803 = VECTOR ( 'NONE', #6744, 1000.000000000000000 ) ;
#62804 = CARTESIAN_POINT ( 'NONE',  ( 6.565887622018943937, -1.918031996736246692, -12.81628187352647608 ) ) ;
#62805 = CARTESIAN_POINT ( 'NONE',  ( -4.164238869374099039, 1.803748834913967647, 8.674139862899312516E-16 ) ) ;
#62806 = ADVANCED_FACE ( 'NONE', ( #62453 ), #12951, .T. ) ;
#62807 = CARTESIAN_POINT ( 'NONE',  ( 17.08211943468705130, 18.47041550158063572, 12.26659068614894998 ) ) ;
#62808 = CIRCLE ( 'NONE', #38848, 0.2500000000000034972 ) ;
#62809 = CARTESIAN_POINT ( 'NONE',  ( 10.00000000000000178, 42.25893115100078745, 9.846743663894594434 ) ) ;
#62810 = CARTESIAN_POINT ( 'NONE',  ( 12.35505582470273644, -0.03417435944610275333, -10.16021613965630443 ) ) ;
#62811 = ORIENTED_EDGE ( 'NONE', *, *, #36603, .T. ) ;
#62812 = CARTESIAN_POINT ( 'NONE',  ( 2.917880565312948704, 47.63708216824730357, 12.26659068614894643 ) ) ;
#62813 = CARTESIAN_POINT ( 'NONE',  ( 10.00000000000000178, 22.25893115100078745, 9.846743663894594434 ) ) ;
#62815 = CARTESIAN_POINT ( 'NONE',  ( -10.06059601896260247, 88.97539449291203084, -5.490105317800711759 ) ) ;
#62814 = LINE ( 'NONE', #9827, #13184 ) ;
#62816 = CARTESIAN_POINT ( 'NONE',  ( 20.88017736071110519, 45.56368534415484106, 2.639326808657452039E-16 ) ) ;
#62817 = CARTESIAN_POINT ( 'NONE',  ( 22.81628187352647785, 61.41530133659709634, 3.434112377981063169 ) ) ;
#62818 = CARTESIAN_POINT ( 'NONE',  ( 4.559911319644449179, 12.23035201082150536, -9.422509992056141925 ) ) ;
#62819 = CARTESIAN_POINT ( 'NONE',  ( -2.816281873526471635, 43.91530133659708923, -3.434112377981056508 ) ) ;
#62820 = CARTESIAN_POINT ( 'NONE',  ( 22.81628187352647785, 16.62363466993042138, 6.195893100308588602E-16 ) ) ;
#62821 = CARTESIAN_POINT ( 'NONE',  ( 14.92337183194729988, 14.34226448433411782, -8.527530157486177487 ) ) ;
#62822 = ORIENTED_EDGE ( 'NONE', *, *, #88225, .F. ) ;
#62823 = SURFACE_SIDE_STYLE ('',( #876 ) ) ;
#62824 = CARTESIAN_POINT ( 'NONE',  ( -6.430724159521294503, -88.51069574204372259, -4.000000000000000000 ) ) ;
#62825 = CARTESIAN_POINT ( 'NONE',  ( 2.917880565312948704, 47.63708216824730357, 12.26659068614894643 ) ) ;
#62826 = CARTESIAN_POINT ( 'NONE',  ( 20.36894250292379382, 33.67874883491396076, 10.36894250292379205 ) ) ;
#62827 = CARTESIAN_POINT ( 'NONE',  ( 0.5774900079438590739, 22.64701867748817321, -5.440088680355550821 ) ) ;
#62828 = CARTESIAN_POINT ( 'NONE',  ( 15.44008868035555260, 39.73035201082150536, 9.422509992056143702 ) ) ;
#62829 = SURFACE_SIDE_STYLE ('',( #93822 ) ) ;
#62830 = CARTESIAN_POINT ( 'NONE',  ( 8.209432707284774366, 15.00000000000000000, 12.55409154915492032 ) ) ;
#62831 = CARTESIAN_POINT ( 'NONE',  ( 7.361572987183170547, 2.050597817667451750, 9.846743663894590881 ) ) ;
#62832 = DIRECTION ( 'NONE',  ( 0.000000000000000000, 0.000000000000000000, -1.000000000000000000 ) ) ;
#62833 = CARTESIAN_POINT ( 'NONE',  ( 7.361572987183169658, 24.96726448433412315, -9.846743663894592657 ) ) ;
#62834 = DIRECTION ( 'NONE',  ( -0.8320502943378436100, 0.5547001962252291474, -0.000000000000000000 ) ) ;
#62835 = SURFACE_SIDE_STYLE ('',( #32330 ) ) ;
#62836 = CARTESIAN_POINT ( 'NONE',  ( 12.63842701281683034, 22.46726448433411605, 9.846743663894596210 ) ) ;
#62837 = CARTESIAN_POINT ( 'NONE',  ( 7.361572987183169658, 54.96726448433413026, -9.846743663894592657 ) ) ;
#62838 = CARTESIAN_POINT ( 'NONE',  ( 20.88017736071110164, 15.35535201082150358, 2.915334737309930979 ) ) ;
#62839 = CARTESIAN_POINT ( 'NONE',  ( 22.81628187352647785, 31.41530133659709279, 3.434112377981063169 ) ) ;
#62840 = VECTOR ( 'NONE', #36888, 1000.000000000000114 ) ;
#62841 = CARTESIAN_POINT ( 'NONE',  ( 0.5774900079438607392, 48.48035201082150536, 5.440088680355550821 ) ) ;
#62843 = CARTESIAN_POINT ( 'NONE',  ( 14.92337183194729633, 7.675597817667451750, 8.527530157486181039 ) ) ;
#62842 = CARTESIAN_POINT ( 'NONE',  ( 2.917880565312948704, 52.63708216824730357, 12.26659068614894643 ) ) ;
#62844 = DIRECTION ( 'NONE',  ( 0.6246950475544237324, 0.7808688094430306093, 0.000000000000000000 ) ) ;
#62845 = CARTESIAN_POINT ( 'NONE',  ( 5.076628168052703671, 51.84226448433412315, 8.527530157486179263 ) ) ;
#62846 = CIRCLE ( 'NONE', #24548, 0.2500000000000002220 ) ;
#62848 = CARTESIAN_POINT ( 'NONE',  ( 13.79529636645030344, 8.262082168247300018, 14.16423886937410614 ) ) ;
#62847 = CARTESIAN_POINT ( 'NONE',  ( 14.92337183194729988, 34.34226448433411605, -8.527530157486177487 ) ) ;
#62849 = CARTESIAN_POINT ( 'NONE',  ( -2.266590686148945544, 17.22041550158063572, 7.082119434687048631 ) ) ;
#62850 = CARTESIAN_POINT ( 'NONE',  ( 0.1532563361054100626, 35.80059781766745175, -2.638427012816831230 ) ) ;
#62851 = CARTESIAN_POINT ( 'NONE',  ( 20.88017736071110875, 40.77201867748818387, -2.915334737309920765 ) ) ;
#62852 = CARTESIAN_POINT ( 'NONE',  ( 10.00000000000000178, 14.31368534415483751, 10.88017736071110342 ) ) ;
#62853 = VECTOR ( 'NONE', #7486, 1000.000000000000000 ) ;
#62854 = CARTESIAN_POINT ( 'NONE',  ( 19.42250999205614193, 40.14701867748817676, 5.440088680355555262 ) ) ;
#62855 = EDGE_CURVE ( 'NONE', #18416, #59748, #28915, .T. ) ;
#62856 = CARTESIAN_POINT ( 'NONE',  ( 20.88017736071110519, 25.56368534415483751, 2.639326808657452039E-16 ) ) ;
#62857 = VERTEX_POINT ( 'NONE', #2977 ) ;
#62858 = CARTESIAN_POINT ( 'NONE',  ( 19.38216949554541557, 37.24863466993041783, -9.382169495545420901 ) ) ;
#62859 = CARTESIAN_POINT ( 'NONE',  ( 0.5774900079438607392, 33.48035201082150536, 5.440088680355550821 ) ) ;
#62860 = VERTEX_POINT ( 'NONE', #39971 ) ;
#62861 = EDGE_CURVE ( 'NONE', #36257, #43815, #26798, .T. ) ;
#62862 = CARTESIAN_POINT ( 'NONE',  ( 0.6178305044545838731, 64.74863466993043914, 9.382169495545420901 ) ) ;
#62863 = CARTESIAN_POINT ( 'NONE',  ( 20.88017736071110519, 65.56368534415483396, 2.639326808657452039E-16 ) ) ;
#62864 = ORIENTED_EDGE ( 'NONE', *, *, #10436, .F. ) ;
#62865 = CARTESIAN_POINT ( 'NONE',  ( 19.42250999205614193, 55.14701867748817676, 5.440088680355555262 ) ) ;
#62866 = LINE ( 'NONE', #54865, #96298 ) ;
#62867 = FILL_AREA_STYLE_COLOUR ( '', #82808 ) ;
#62868 = CARTESIAN_POINT ( 'NONE',  ( 22.26659068614895176, 64.72041550158064638, -7.082119434687042414 ) ) ;
#62869 = CARTESIAN_POINT ( 'NONE',  ( -0.8801773607111008646, 68.27201867748817676, 2.915334737309923430 ) ) ;
#62870 = CARTESIAN_POINT ( 'NONE',  ( -4.164238869374099927, 7.012082168247302683, 3.795296366450308767 ) ) ;
#62871 = CARTESIAN_POINT ( 'NONE',  ( 10.00000000000000000, 9.758931151000785675, -9.846743663894594434 ) ) ;
#62872 = CARTESIAN_POINT ( 'NONE',  ( 17.96484262340118221, 11.18868534415483929, -7.964842623401177768 ) ) ;
#62873 = CARTESIAN_POINT ( 'NONE',  ( 2.791683348922237240, 50.38393115100078035, -7.208316651077763204 ) ) ;
#62874 = ORIENTED_EDGE ( 'NONE', *, *, #36631, .F. ) ;
#62875 = CARTESIAN_POINT ( 'NONE',  ( 14.92337183194729988, 49.34226448433411605, -8.527530157486177487 ) ) ;
#62876 = CARTESIAN_POINT ( 'NONE',  ( 12.91533473730992121, 64.52201867748817676, 10.88017736071110164 ) ) ;
#62877 = CARTESIAN_POINT ( 'NONE',  ( -0.8801773607110991993, 42.85535201082150536, -2.915334737309923874 ) ) ;
#62878 = CARTESIAN_POINT ( 'NONE',  ( 0.1532563361054083140, 46.00893115100079456, 1.131784320476157264E-15 ) ) ;
#62879 = CARTESIAN_POINT ( 'NONE',  ( -2.816281873526471635, 28.91530133659708213, -3.434112377981056508 ) ) ;
#62881 = CARTESIAN_POINT ( 'NONE',  ( 15.44008868035555793, 66.39701867748817676, -9.422509992056140149 ) ) ;
#62880 = CARTESIAN_POINT ( 'NONE',  ( -14.02068044289383586, 0.3640475087720986269, 5.331089937175563342 ) ) ;
#62882 = CARTESIAN_POINT ( 'NONE',  ( 2.035157376598824452, 43.68868534415484106, 7.964842623401179544 ) ) ;
#62883 = CARTESIAN_POINT ( 'NONE',  ( 24.16423886937410614, 54.51208216824730357, -3.795296366450302550 ) ) ;
#62884 = ADVANCED_FACE ( 'NONE', ( #39311 ), #75266, .T. ) ;
#62885 = CARTESIAN_POINT ( 'NONE',  ( 21.09922568453594849, 16.20696800326375353, 6.408140936763242479 ) ) ;
#62886 = LINE ( 'NONE', #10877, #59457 ) ;
#62887 = ORIENTED_EDGE ( 'NONE', *, *, #71461, .F. ) ;
#62888 = CARTESIAN_POINT ( 'NONE',  ( -1.099225684535947600, 33.70696800326375353, -6.408140936763238038 ) ) ;
#62889 = CARTESIAN_POINT ( 'NONE',  ( 2.035157376598822676, 22.43868534415483396, -7.964842623401177768 ) ) ;
#62890 = ADVANCED_FACE ( 'NONE', ( #54284 ), #68853, .T. ) ;
#62891 = ORIENTED_EDGE ( 'NONE', *, *, #83578, .T. ) ;
#62892 = CARTESIAN_POINT ( 'NONE',  ( 2.035157376598822676, 67.43868534415484817, -7.964842623401177768 ) ) ;
#62893 = CARTESIAN_POINT ( 'NONE',  ( 1.472469842513823179, 51.42559781766745886, 4.923371831947296329 ) ) ;
#62895 = CARTESIAN_POINT ( 'NONE',  ( 19.84674366389459266, 43.30059781766744464, 2.638427012816836559 ) ) ;
#62894 = CARTESIAN_POINT ( 'NONE',  ( 0.1532563361054082862, 16.21726448433411960, 2.638427012816831674 ) ) ;
#62896 = CARTESIAN_POINT ( 'NONE',  ( -11.58017868921325189, -84.10256047875394358, 3.750000000000000888 ) ) ;
#62897 = CARTESIAN_POINT ( 'NONE',  ( 6.565887622018943937, 65.16530133659709634, 12.81628187352647430 ) ) ;
#62898 = LINE ( 'NONE', #70912, #29935 ) ;
#62899 = CARTESIAN_POINT ( 'NONE',  ( 9.159723438033203990, -0.03417435944610275333, -10.91613331444542645 ) ) ;
#62901 = CARTESIAN_POINT ( 'NONE',  ( -5.888281321711915872, 1.823139558123406223, -10.37198838585826266 ) ) ;
#62900 = CARTESIAN_POINT ( 'NONE',  ( 18.52753015748618282, 23.92559781766745530, -4.923371831947291888 ) ) ;
#62902 = DIRECTION ( 'NONE',  ( 0.000000000000000000, 1.000000000000000000, 0.000000000000000000 ) ) ;
#62904 = ORIENTED_EDGE ( 'NONE', *, *, #16369, .T. ) ;
#62903 = CARTESIAN_POINT ( 'NONE',  ( 0.1532563361054082862, 51.21726448433412315, 2.638427012816831674 ) ) ;
#62905 = CARTESIAN_POINT ( 'NONE',  ( -7.750000000000000000, 41.24999999999999289, 4.000000000000000000 ) ) ;
#62906 = CARTESIAN_POINT ( 'NONE',  ( 21.09922568453595559, 22.04030133659708923, -6.408140936763230044 ) ) ;
#62907 = VECTOR ( 'NONE', #90139, 1000.000000000000000 ) ;
#62908 = CARTESIAN_POINT ( 'NONE',  ( 0.000000000000000000, 36.75000000000000000, -2.500000000000000000 ) ) ;
#62909 = CARTESIAN_POINT ( 'NONE',  ( 13.79529636645031943, 45.34541550158062506, -14.16423886937409904 ) ) ;
#62910 = CARTESIAN_POINT ( 'NONE',  ( 12.63842701281683034, 12.46726448433411782, 9.846743663894596210 ) ) ;
#62911 = CARTESIAN_POINT ( 'NONE',  ( 17.20831665107776587, 4.133931151000785675, -7.208316651077762316 ) ) ;
#62912 = CARTESIAN_POINT ( 'NONE',  ( 10.58981376305282041, -0.03417435944610275333, 9.535111140613782510 ) ) ;
#62913 = CIRCLE ( 'NONE', #5482, 0.2999999999999999334 ) ;
#62914 = CARTESIAN_POINT ( 'NONE',  ( -4.164238869374099039, 46.80374883491397497, 8.674139862899312516E-16 ) ) ;
#62915 = CARTESIAN_POINT ( 'NONE',  ( 1.472469842513823179, 65.59226448433412315, -4.923371831947296329 ) ) ;
#62916 = EDGE_CURVE ( 'NONE', #1898, #79199, #15340, .T. ) ;
#62917 = CARTESIAN_POINT ( 'NONE',  ( 17.08211943468705840, 60.13708216824729647, -12.26659068614894466 ) ) ;
#62918 = CARTESIAN_POINT ( 'NONE',  ( 22.26659068614894466, 28.88708216824730357, 7.082119434687054849 ) ) ;
#62919 = CARTESIAN_POINT ( 'NONE',  ( 20.36894250292379738, 34.92874883491396076, -10.36894250292379027 ) ) ;
#62920 = LINE ( 'NONE', #10911, #69148 ) ;
#62922 = CARTESIAN_POINT ( 'NONE',  ( 10.00000000000000178, 62.25893115100078745, 9.846743663894594434 ) ) ;
#62921 = CARTESIAN_POINT ( 'NONE',  ( 4.323026924237980850, -6.401461444700509595, 2.500000000000000000 ) ) ;
#62923 = ORIENTED_EDGE ( 'NONE', *, *, #91320, .T. ) ;
#62924 = CARTESIAN_POINT ( 'NONE',  ( 2.035157376598822676, 32.43868534415483396, -7.964842623401177768 ) ) ;
#62925 = CARTESIAN_POINT ( 'NONE',  ( 10.93781366033349833, 14.49999999999999112, -10.26470809774071569 ) ) ;
#62926 = CARTESIAN_POINT ( 'NONE',  ( 20.00000000000000711, 92.98956734510680633, -4.826711382686650786 ) ) ;
#62927 = CARTESIAN_POINT ( 'NONE',  ( 5.076628168052703671, 36.84226448433412315, 8.527530157486179263 ) ) ;
#62928 = CARTESIAN_POINT ( 'NONE',  ( -2.816281873526471635, 63.91530133659708923, -3.434112377981056508 ) ) ;
#62929 = CARTESIAN_POINT ( 'NONE',  ( 3.469446951953614189E-15, -1.946251165086031243, 14.16423886937410259 ) ) ;
#62930 = CARTESIAN_POINT ( 'NONE',  ( 0.1532563361054083140, 46.00893115100079456, 1.131784320476157264E-15 ) ) ;
#62931 = CARTESIAN_POINT ( 'NONE',  ( 15.99538290524656503, -0.03417435944610275333, 0.1584996864329874799 ) ) ;
#62932 = VERTEX_POINT ( 'NONE', #8311 ) ;
#62933 = CARTESIAN_POINT ( 'NONE',  ( 10.00000000000000178, 8.053748834913967869, 14.16423886937410082 ) ) ;
#62934 = FACE_OUTER_BOUND ( 'NONE', #95091, .T. ) ;
#62936 = DIRECTION ( 'NONE',  ( 0.000000000000000000, 0.000000000000000000, -1.000000000000000000 ) ) ;
#62935 = PLANE ( 'NONE',  #33848 ) ;
#62937 = CARTESIAN_POINT ( 'NONE',  ( 7.084665262690076126, 9.105352010821503583, 10.88017736071109987 ) ) ;
#62938 = CARTESIAN_POINT ( 'NONE',  ( 3.591859063236761518, 29.95696800326375708, 11.09922568453594849 ) ) ;
#62939 = CARTESIAN_POINT ( 'NONE',  ( 20.24186590665278018, 2.616331881023272299, -6.114288769123028544 ) ) ;
#62940 = CARTESIAN_POINT ( 'NONE',  ( 4.559911319644449179, 63.89701867748817676, 9.422509992056141925 ) ) ;
#62941 = PRESENTATION_STYLE_ASSIGNMENT (( #70957 ) ) ;
#62942 = CARTESIAN_POINT ( 'NONE',  ( -46.93999999999942219, 101.0602049476338777, -8.583117191026476078 ) ) ;
#62943 = CARTESIAN_POINT ( 'NONE',  ( 24.16423886937409904, 64.09541550158064638, 3.795296366450317205 ) ) ;
#62944 = CARTESIAN_POINT ( 'NONE',  ( 6.564124673094354101, -0.5742864948665229452, 3.000000000000000000 ) ) ;
#62945 = CARTESIAN_POINT ( 'NONE',  ( 0.5774900079438590739, 27.64701867748817676, -5.440088680355550821 ) ) ;
#62946 = CARTESIAN_POINT ( 'NONE',  ( 20.88017736071110875, 40.77201867748818387, -2.915334737309920765 ) ) ;
#62947 = CARTESIAN_POINT ( 'NONE',  ( 22.81628187352647785, 1.415301336597087012, 3.434112377981063169 ) ) ;
#62948 = CARTESIAN_POINT ( 'NONE',  ( 19.84674366389459266, 48.71726448433413026, -2.638427012816827677 ) ) ;
#62949 = CARTESIAN_POINT ( 'NONE',  ( -2.816281873526473856, 64.12363466993042493, 9.499525473075851096E-16 ) ) ;
#62950 = CARTESIAN_POINT ( 'NONE',  ( 2.603489959281588995, 55.43575266056826933, -6.500000000000003553 ) ) ;
#62951 = ORIENTED_EDGE ( 'NONE', *, *, #51145, .T. ) ;
#62952 = CARTESIAN_POINT ( 'NONE',  ( 19.42250999205614548, 30.98035201082150536, -5.440088680355545492 ) ) ;
#62953 = CARTESIAN_POINT ( 'NONE',  ( 21.09922568453594849, 36.20696800326375353, 6.408140936763242479 ) ) ;
#62954 = DIRECTION ( 'NONE',  ( 0.000000000000000000, 0.000000000000000000, 1.000000000000000000 ) ) ;
#62955 = CARTESIAN_POINT ( 'NONE',  ( 18.52753015748618282, 58.92559781766745886, -4.923371831947291888 ) ) ;
#62956 = CARTESIAN_POINT ( 'NONE',  ( 20.88017736071110164, 55.35535201082149825, 2.915334737309930979 ) ) ;
#62957 = CARTESIAN_POINT ( 'NONE',  ( 1.472469842513823179, 6.425597817667451750, 4.923371831947296329 ) ) ;
#62958 = CARTESIAN_POINT ( 'NONE',  ( 16.40814093676323893, 35.79030133659708923, 11.09922568453595026 ) ) ;
#62960 = CYLINDRICAL_SURFACE ( 'NONE', #28806, 15.00000000000000000 ) ;
#62959 = CARTESIAN_POINT ( 'NONE',  ( 7.084665262690076126, 59.10535201082150536, 10.88017736071109987 ) ) ;
#62961 = LINE ( 'NONE', #78464, #83279 ) ;
#62962 = CARTESIAN_POINT ( 'NONE',  ( -1.099225684535947600, 58.70696800326375353, -6.408140936763238038 ) ) ;
#62963 = EDGE_LOOP ( 'NONE', ( #11228, #69054, #98750, #78034, #36303, #26840 ) ) ;
#62964 = CARTESIAN_POINT ( 'NONE',  ( 3.881785064875176605, 2.337810934421868936E-16, 14.10213074188657778 ) ) ;
#62965 = CARTESIAN_POINT ( 'NONE',  ( 1.932340009482144794, 16.49127512925449324, -6.500000000000007105 ) ) ;
#62966 = CARTESIAN_POINT ( 'NONE',  ( 7.084665262690076126, 4.105352010821503583, 10.88017736071109987 ) ) ;
#62968 = CARTESIAN_POINT ( 'NONE',  ( 2.917880565312948704, 17.63708216824730357, 12.26659068614894643 ) ) ;
#62967 = CARTESIAN_POINT ( 'NONE',  ( 21.09922568453594849, 41.20696800326375353, 6.408140936763242479 ) ) ;
#62969 = CARTESIAN_POINT ( 'NONE',  ( 12.63842701281683034, 12.46726448433411782, 9.846743663894596210 ) ) ;
#62970 = CARTESIAN_POINT ( 'NONE',  ( 20.88017736071110519, 5.563685344154837509, 2.639326808657452039E-16 ) ) ;
#62971 = CARTESIAN_POINT ( 'NONE',  ( 1.472469842513823179, 16.42559781766745175, 4.923371831947296329 ) ) ;
#62972 = CARTESIAN_POINT ( 'NONE',  ( -4.164238869374098151, 51.59541550158063217, -3.795296366450310543 ) ) ;
#62973 = ORIENTED_EDGE ( 'NONE', *, *, #60374, .T. ) ;
#62974 = SURFACE_SIDE_STYLE ('',( #55490 ) ) ;
#62975 = EDGE_CURVE ( 'NONE', #46169, #35983, #35286, .T. ) ;
#62976 = CARTESIAN_POINT ( 'NONE',  ( 19.42250999205614548, 20.98035201082150891, -5.440088680355545492 ) ) ;
#62977 = CARTESIAN_POINT ( 'NONE',  ( 13.99999999999999822, 11.00000000000000000, -5.000000000000000000 ) ) ;
#62978 = EDGE_LOOP ( 'NONE', ( #44666, #37291, #70875, #70049 ) ) ;
#62979 = CARTESIAN_POINT ( 'NONE',  ( 15.44008868035555793, 16.39701867748817321, -9.422509992056140149 ) ) ;
#62980 = CARTESIAN_POINT ( 'NONE',  ( 12.91533473730992121, 9.522018677488171434, 10.88017736071110164 ) ) ;
#62981 = CARTESIAN_POINT ( 'NONE',  ( 10.00000000000000178, 52.25893115100078745, 9.846743663894594434 ) ) ;
#62982 = CARTESIAN_POINT ( 'NONE',  ( -1.099225684535947600, 49.54030133659708923, 6.408140936763237150 ) ) ;
#62985 = CARTESIAN_POINT ( 'NONE',  ( 20.36894250292379382, 18.67874883491397142, 10.36894250292379205 ) ) ;
#62984 = CARTESIAN_POINT ( 'NONE',  ( 18.04007052943773459, 64.00257860105350005, -5.767676674365834089 ) ) ;
#62983 = AXIS2_PLACEMENT_3D ( 'NONE', #80498, #3042, #64485 ) ;
#62986 = CARTESIAN_POINT ( 'NONE',  ( 0.5774900079438607392, 23.48035201082150536, 5.440088680355550821 ) ) ;
#62987 = CARTESIAN_POINT ( 'NONE',  ( 12.91533473730992121, 9.522018677488171434, 10.88017736071110164 ) ) ;
#62988 = CARTESIAN_POINT ( 'NONE',  ( 7.361572987183170547, 52.05059781766745175, 9.846743663894590881 ) ) ;
#62989 = VECTOR ( 'NONE', #61946, 1000.000000000000000 ) ;
#62990 = CARTESIAN_POINT ( 'NONE',  ( -14.02068044289371684, 14.49999999999999822, -5.331089937175857330 ) ) ;
#62991 = CARTESIAN_POINT ( 'NONE',  ( 18.52753015748618282, 33.92559781766745886, -4.923371831947291888 ) ) ;
#62992 = CIRCLE ( 'NONE', #37459, 15.00000000000000000 ) ;
#62993 = CARTESIAN_POINT ( 'NONE',  ( 0.2751277870542967463, 70.00000000000000000, 6.000000000000000000 ) ) ;
#62994 = CARTESIAN_POINT ( 'NONE',  ( 12.63842701281683922, 4.550597817667451750, -9.846743663894590881 ) ) ;
#62995 = CARTESIAN_POINT ( 'NONE',  ( 3.469446951953614189E-15, 32.25893115100078745, 9.846743663894594434 ) ) ;
#62996 = ORIENTED_EDGE ( 'NONE', *, *, #95536, .T. ) ;
#62997 = DIRECTION ( 'NONE',  ( 0.9961946980917453232, -0.08715574274766037244, 0.000000000000000000 ) ) ;
#62998 = CARTESIAN_POINT ( 'NONE',  ( 4.559911319644449179, 63.89701867748817676, 9.422509992056141925 ) ) ;
#62999 = CARTESIAN_POINT ( 'NONE',  ( -1.099225684535947600, 4.540301336597087456, 6.408140936763237150 ) ) ;
#63001 = CARTESIAN_POINT ( 'NONE',  ( 0.5774900079438590739, 47.64701867748817676, -5.440088680355550821 ) ) ;
#63000 = CARTESIAN_POINT ( 'NONE',  ( 2.035157376598824452, 48.68868534415483396, 7.964842623401179544 ) ) ;
#63003 = CARTESIAN_POINT ( 'NONE',  ( 13.43411237798105340, 40.58196800326375353, 12.81628187352647963 ) ) ;
#63002 = CARTESIAN_POINT ( 'NONE',  ( 0.5774900079438607392, 8.480352010821505360, 5.440088680355550821 ) ) ;
#63004 = CARTESIAN_POINT ( 'NONE',  ( 22.26659068614895176, 24.72041550158063572, -7.082119434687042414 ) ) ;
#63005 = EDGE_CURVE ( 'NONE', #9752, #63527, #4976, .T. ) ;
#63006 = AXIS2_PLACEMENT_3D ( 'NONE', #89380, #67370, #20893 ) ;
#63007 = CARTESIAN_POINT ( 'NONE',  ( -2.816281873526473856, 39.33196800326374643, 3.434112377981055619 ) ) ;
#63008 = ORIENTED_EDGE ( 'NONE', *, *, #77763, .T. ) ;
#63009 = CARTESIAN_POINT ( 'NONE',  ( 0.1532563361054083140, 56.00893115100078745, 1.131784320476157264E-15 ) ) ;
#63010 = EDGE_CURVE ( 'NONE', #50375, #50944, #10167, .T. ) ;
#63011 = CARTESIAN_POINT ( 'NONE',  ( -0.8801773607111008646, 18.27201867748817321, 2.915334737309923430 ) ) ;
#63012 = ORIENTED_EDGE ( 'NONE', *, *, #24182, .T. ) ;
#63013 = CARTESIAN_POINT ( 'NONE',  ( 2.791683348922237240, 0.3839311510007847872, -7.208316651077763204 ) ) ;
#63014 =( NAMED_UNIT ( * ) SI_UNIT ( $, .STERADIAN. ) SOLID_ANGLE_UNIT ( ) );
#63015 = CARTESIAN_POINT ( 'NONE',  ( -2.799999999999999378, 22.11937003968011695, 3.429011037612589769E-16 ) ) ;
#63016 = CARTESIAN_POINT ( 'NONE',  ( 0.1532563361054082862, 11.21726448433411605, 2.638427012816831674 ) ) ;
#63017 = CARTESIAN_POINT ( 'NONE',  ( 0.1532563361054082862, 1.217264484334117824, 2.638427012816831674 ) ) ;
#63018 = CARTESIAN_POINT ( 'NONE',  ( -5.795997163829992083, 15.00000000000000000, -13.01802277140713926 ) ) ;
#63019 = AXIS2_PLACEMENT_3D ( 'NONE', #77624, #70637, #63118 ) ;
#63021 = DIRECTION ( 'NONE',  ( -0.000000000000000000, 1.000000000000000000, -0.000000000000000000 ) ) ;
#63020 = CARTESIAN_POINT ( 'NONE',  ( 12.91533473730993009, 56.60535201082151247, -10.88017736071109987 ) ) ;
#63022 = CARTESIAN_POINT ( 'NONE',  ( 0.5774900079438590739, 57.64701867748817676, -5.440088680355550821 ) ) ;
#63024 = ORIENTED_EDGE ( 'NONE', *, *, #24016, .T. ) ;
#63023 = CARTESIAN_POINT ( 'NONE',  ( 1.472469842513823179, 6.425597817667451750, 4.923371831947296329 ) ) ;
#63025 = CARTESIAN_POINT ( 'NONE',  ( -2.602060718268784267, 0.000000000000000000, -4.792399674598892823 ) ) ;
#63026 = CARTESIAN_POINT ( 'NONE',  ( 2.791683348922240793, 56.63393115100078035, 7.208316651077764092 ) ) ;
#63027 = VERTEX_POINT ( 'NONE', #7828 ) ;
#63028 = ORIENTED_EDGE ( 'NONE', *, *, #44760, .F. ) ;
#63029 = DIRECTION ( 'NONE',  ( 0.000000000000000000, 0.000000000000000000, -1.000000000000000000 ) ) ;
#63030 = CARTESIAN_POINT ( 'NONE',  ( 24.16423886937410614, 9.512082168247301794, -3.795296366450302550 ) ) ;
#63031 = CARTESIAN_POINT ( 'NONE',  ( -1.099225684535947600, 59.54030133659708923, 6.408140936763237150 ) ) ;
#63032 = CARTESIAN_POINT ( 'NONE',  ( 20.36894250292379738, 4.928748834913967869, -10.36894250292379027 ) ) ;
#63033 = CARTESIAN_POINT ( 'NONE',  ( 20.36894250292379382, 23.67874883491397142, 10.36894250292379205 ) ) ;
#63034 = DIRECTION ( 'NONE',  ( 0.9099612708765483227, 0.000000000000000000, -0.4146932426562279228 ) ) ;
#63035 = DIRECTION ( 'NONE',  ( 1.000000000000000000, -0.000000000000000000, 0.000000000000000000 ) ) ;
#63036 = CARTESIAN_POINT ( 'NONE',  ( -0.8801773607111009756, 18.06368534415484106, 1.068504757029289695E-15 ) ) ;
#63037 =( NAMED_UNIT ( * ) SI_UNIT ( $, .STERADIAN. ) SOLID_ANGLE_UNIT ( ) );
#63038 = ORIENTED_EDGE ( 'NONE', *, *, #59238, .F. ) ;
#63039 = CARTESIAN_POINT ( 'NONE',  ( 0.1532563361054100626, 0.8005978176674514168, -2.638427012816831230 ) ) ;
#63040 = VECTOR ( 'NONE', #79434, 1000.000000000000000 ) ;
#63041 = CARTESIAN_POINT ( 'NONE',  ( 1.472469842513823179, 21.42559781766745175, 4.923371831947296329 ) ) ;
#63042 = CARTESIAN_POINT ( 'NONE',  ( -1.099225684535947600, 34.54030133659708923, 6.408140936763237150 ) ) ;
#63044 = ADVANCED_FACE ( 'NONE', ( #98352 ), #84832, .T. ) ;
#63043 = CARTESIAN_POINT ( 'NONE',  ( 7.361572987183170547, 37.05059781766744464, 9.846743663894590881 ) ) ;
#63045 = CARTESIAN_POINT ( 'NONE',  ( 17.39651004071841101, 57.93575266056827644, 6.500000000000005329 ) ) ;
#63046 = CARTESIAN_POINT ( 'NONE',  ( 3.591859063236761518, 14.95696800326375531, 11.09922568453594849 ) ) ;
#63047 = CARTESIAN_POINT ( 'NONE',  ( 0.3093388210927670023, 14.63595249122790598, 14.99680997725066867 ) ) ;
#63048 = CARTESIAN_POINT ( 'NONE',  ( 5.076628168052703671, 21.84226448433411960, 8.527530157486179263 ) ) ;
#63049 = CARTESIAN_POINT ( 'NONE',  ( 7.361572987183169658, 9.967264484334119601, -9.846743663894592657 ) ) ;
#63050 = VERTEX_POINT ( 'NONE', #75813 ) ;
#63051 = TOROIDAL_SURFACE ( 'NONE', #55121, 14.49999999999999822, 0.5000000000000000000 ) ;
#63052 = CARTESIAN_POINT ( 'NONE',  ( 7.084665262690076126, 39.10535201082150536, 10.88017736071109987 ) ) ;
#63053 = CARTESIAN_POINT ( 'NONE',  ( 13.79529636645030344, 28.26208216824729647, 14.16423886937410614 ) ) ;
#63054 = CARTESIAN_POINT ( 'NONE',  ( 1.472469842513823179, 36.42559781766745175, 4.923371831947296329 ) ) ;
#63055 = CARTESIAN_POINT ( 'NONE',  ( 19.84674366389459266, 18.30059781766745175, 2.638427012816836559 ) ) ;
#63057 = CARTESIAN_POINT ( 'NONE',  ( -8.118176716543592519, 86.25458391402874270, 4.292297935673070164 ) ) ;
#63056 = CARTESIAN_POINT ( 'NONE',  ( 19.38216949554541557, 47.24863466993041783, -9.382169495545420901 ) ) ;
#63058 = CARTESIAN_POINT ( 'NONE',  ( 2.035157376598822676, 32.43868534415483396, -7.964842623401177768 ) ) ;
#63059 = CARTESIAN_POINT ( 'NONE',  ( -2.816281873526471635, 23.91530133659708568, -3.434112377981056508 ) ) ;
#63060 = CARTESIAN_POINT ( 'NONE',  ( 1.472469842513823179, 40.59226448433411605, -4.923371831947296329 ) ) ;
#63061 = CARTESIAN_POINT ( 'NONE',  ( 2.915334737309928315, 4.522018677488174099, 10.88017736071109987 ) ) ;
#63062 = CARTESIAN_POINT ( 'NONE',  ( 3.591859063236763294, 48.29030133659708923, -11.09922568453595026 ) ) ;
#63064 = DIRECTION ( 'NONE',  ( 0.6246950475544238435, 0.7808688094430307203, 0.000000000000000000 ) ) ;
#63063 = CARTESIAN_POINT ( 'NONE',  ( 0.5774900079438590739, 47.64701867748817676, -5.440088680355550821 ) ) ;
#63065 = DIRECTION ( 'NONE',  ( -4.205390244792255888E-16, 1.000000000000000000, 0.000000000000000000 ) ) ;
#63066 = CYLINDRICAL_SURFACE ( 'NONE', #9758, 11.92686044187656513 ) ;
#63067 = CARTESIAN_POINT ( 'NONE',  ( 12.91533473730992121, 49.52201867748817676, 10.88017736071110164 ) ) ;
#63068 = CARTESIAN_POINT ( 'NONE',  ( 4.559911319644449179, 52.23035201082151247, -9.422509992056141925 ) ) ;
#63069 = CARTESIAN_POINT ( 'NONE',  ( 8.629999999999995453, 40.74999999999999289, 4.250000000000000000 ) ) ;
#63070 = SURFACE_SIDE_STYLE ('',( #32573 ) ) ;
#63071 = CARTESIAN_POINT ( 'NONE',  ( 19.42250999205614548, 10.98035201082150536, -5.440088680355545492 ) ) ;
#63072 = CARTESIAN_POINT ( 'NONE',  ( 7.361572987183169658, 59.96726448433410894, -9.846743663894592657 ) ) ;
#63074 = PLANE ( 'NONE',  #4845 ) ;
#63073 = CARTESIAN_POINT ( 'NONE',  ( 19.42250999205614548, 20.98035201082150891, -5.440088680355545492 ) ) ;
#63075 = SURFACE_STYLE_USAGE ( .BOTH. , #22766 ) ;
#63076 = CARTESIAN_POINT ( 'NONE',  ( 6.565887622018943937, 25.16530133659708213, 12.81628187352647430 ) ) ;
#63077 = ORIENTED_EDGE ( 'NONE', *, *, #27881, .T. ) ;
#63078 = CARTESIAN_POINT ( 'NONE',  ( 2.035157376598824452, 48.68868534415483396, 7.964842623401179544 ) ) ;
#63079 = CARTESIAN_POINT ( 'NONE',  ( 18.52753015748617571, 33.09226448433411605, 4.923371831947298993 ) ) ;
#63081 = CARTESIAN_POINT ( 'NONE',  ( 19.72487221294571569, 47.80223176428831522, -6.499999999999982236 ) ) ;
#63080 = CARTESIAN_POINT ( 'NONE',  ( 22.81628187352647785, 1.623634669930420271, 6.195893100308588602E-16 ) ) ;
#63082 = CARTESIAN_POINT ( 'NONE',  ( 10.00000000000000178, 19.31368534415484106, 10.88017736071110342 ) ) ;
#63083 = CARTESIAN_POINT ( 'NONE',  ( 0.5774900079438607392, 38.48035201082150536, 5.440088680355550821 ) ) ;
#63084 = CARTESIAN_POINT ( 'NONE',  ( -4.164238869374099927, 57.01208216824731068, 3.795296366450308767 ) ) ;
#63085 = CARTESIAN_POINT ( 'NONE',  ( 14.92337183194729988, 39.34226448433412315, -8.527530157486177487 ) ) ;
#63086 = CARTESIAN_POINT ( 'NONE',  ( 19.42250999205614193, 55.14701867748817676, 5.440088680355555262 ) ) ;
#63087 = PRESENTATION_STYLE_ASSIGNMENT (( #32592 ) ) ;
#63088 = CARTESIAN_POINT ( 'NONE',  ( 20.36894250292379738, 14.92874883491396432, -10.36894250292379027 ) ) ;
#63089 = AXIS2_PLACEMENT_3D ( 'NONE', #21363, #43846, #13864 ) ;
#63090 = EDGE_CURVE ( 'NONE', #26110, #65168, #22830, .T. ) ;
#63091 = DIRECTION ( 'NONE',  ( -0.000000000000000000, -1.000000000000000000, -0.000000000000000000 ) ) ;
#63092 = CARTESIAN_POINT ( 'NONE',  ( 1.274849032794324932, 22.55509018479936145, -6.500000000000021316 ) ) ;
#63093 = EDGE_LOOP ( 'NONE', ( #48241, #26025, #58971, #5208, #34096, #4963 ) ) ;
#63094 = ORIENTED_EDGE ( 'NONE', *, *, #83639, .F. ) ;
#63095 = CARTESIAN_POINT ( 'NONE',  ( 24.16423886937410614, 29.30374883491396787, 8.672049930838204340E-16 ) ) ;
#63096 = CARTESIAN_POINT ( 'NONE',  ( 6.204703633549690345, 40.76208216824731778, -14.16423886937410259 ) ) ;
#63097 = CARTESIAN_POINT ( 'NONE',  ( 19.84674366389459266, 8.300597817667451750, 2.638427012816836559 ) ) ;
#63098 = CARTESIAN_POINT ( 'NONE',  ( 7.361572987183170547, 62.05059781766745886, 9.846743663894590881 ) ) ;
#63099 = CARTESIAN_POINT ( 'NONE',  ( 0.2751277870542967463, 0.000000000000000000, 6.500000000000000888 ) ) ;
#63101 = CARTESIAN_POINT ( 'NONE',  ( 22.81628187352648496, 26.83196800326374998, -3.434112377981050290 ) ) ;
#63100 = CARTESIAN_POINT ( 'NONE',  ( 20.88017736071110519, 65.56368534415483396, 2.639326808657452039E-16 ) ) ;
#63102 = CARTESIAN_POINT ( 'NONE',  ( 20.36894250292379382, 33.67874883491396076, 10.36894250292379205 ) ) ;
#63103 = CARTESIAN_POINT ( 'NONE',  ( -0.8801773607111008646, 28.27201867748817321, 2.915334737309923430 ) ) ;
#63104 = CARTESIAN_POINT ( 'NONE',  ( 12.07856007377828078, 4.686601975994315497E-16, -8.022367888854837759 ) ) ;
#63105 = CARTESIAN_POINT ( 'NONE',  ( 2.035157376598822676, 67.43868534415484817, -7.964842623401177768 ) ) ;
#63106 = CARTESIAN_POINT ( 'NONE',  ( -4.923371831947302546, -14.82440218233254470, -8.527530157486173934 ) ) ;
#63107 = EDGE_LOOP ( 'NONE', ( #84311, #87117, #31132, #96334 ) ) ;
#63108 = COLOUR_RGB ( '', 0.72549020, 0.75294118, 0.79215686) ;
#63109 = DIRECTION ( 'NONE',  ( 0.000000000000000000, 0.000000000000000000, -1.000000000000000000 ) ) ;
#63110 = EDGE_CURVE ( 'NONE', #54543, #58661, #16308, .T. ) ;
#63111 = DIRECTION ( 'NONE',  ( 0.000000000000000000, -0.7071067811865492381, -0.7071067811865457964 ) ) ;
#63112 = ORIENTED_EDGE ( 'NONE', *, *, #29295, .F. ) ;
#63113 =( NAMED_UNIT ( * ) PLANE_ANGLE_UNIT ( ) SI_UNIT ( $, .RADIAN. ) );
#63115 = CARTESIAN_POINT ( 'NONE',  ( 19.42250999205614548, 5.980352010821504471, -5.440088680355545492 ) ) ;
#63114 = CARTESIAN_POINT ( 'NONE',  ( -2.266590686148945544, 66.38708216824730357, -7.082119434687050408 ) ) ;
#63117 = CARTESIAN_POINT ( 'NONE',  ( 3.591859063236761518, 9.956968003263753531, 11.09922568453594849 ) ) ;
#63116 = CARTESIAN_POINT ( 'NONE',  ( 17.20831665107776587, 42.88393115100077324, 7.208316651077764980 ) ) ;
#63118 = DIRECTION ( 'NONE',  ( 0.000000000000000000, -1.000000000000000000, 0.000000000000000000 ) ) ;
#63119 = LINE ( 'NONE', #41135, #81417 ) ;
#63120 = EDGE_CURVE ( 'NONE', #55896, #75803, #63801, .T. ) ;
#63122 = CARTESIAN_POINT ( 'NONE',  ( 19.38216949554541557, 7.248634669930421381, -9.382169495545420901 ) ) ;
#63121 = STYLED_ITEM ( 'NONE', ( #51839 ), #84999 ) ;
#63123 = VERTEX_POINT ( 'NONE', #66638 ) ;
#63124 = CARTESIAN_POINT ( 'NONE',  ( 17.08211943468705130, 48.47041550158063927, 12.26659068614894998 ) ) ;
#63125 = ORIENTED_EDGE ( 'NONE', *, *, #87724, .F. ) ;
#63126 = EDGE_CURVE ( 'NONE', #74503, #84500, #82622, .T. ) ;
#63127 = CARTESIAN_POINT ( 'NONE',  ( 10.00000000000000000, 50.55374883491396787, -14.16423886937410082 ) ) ;
#63128 = ORIENTED_EDGE ( 'NONE', *, *, #13914, .F. ) ;
#63129 = CARTESIAN_POINT ( 'NONE',  ( -0.8801773607111009756, 33.06368534415484106, 1.068504757029289695E-15 ) ) ;
#63130 = CARTESIAN_POINT ( 'NONE',  ( 20.88017736071110164, 40.35535201082150536, 2.915334737309930979 ) ) ;
#63131 = CARTESIAN_POINT ( 'NONE',  ( 7.361572987183170547, 67.05059781766746596, 9.846743663894590881 ) ) ;
#63132 = CARTESIAN_POINT ( 'NONE',  ( 4.559911319644449179, 42.23035201082151247, -9.422509992056141925 ) ) ;
#63133 = CARTESIAN_POINT ( 'NONE',  ( 0.5774900079438590739, 67.64701867748817676, -5.440088680355550821 ) ) ;
#63134 = CARTESIAN_POINT ( 'NONE',  ( 4.559911319644449179, 23.89701867748817321, 9.422509992056141925 ) ) ;
#63135 = CARTESIAN_POINT ( 'NONE',  ( 0.3093388210927642268, 0.5000000000000004441, -14.99680997725065978 ) ) ;
#63136 = TOROIDAL_SURFACE ( 'NONE', #18401, 2.500000000000000888, 0.5000000000000000000 ) ;
#63137 = CARTESIAN_POINT ( 'NONE',  ( 0.1532563361054083140, 11.00893115100078568, 1.131784320476157264E-15 ) ) ;
#63138 = CARTESIAN_POINT ( 'NONE',  ( -3.500000000000000444, 1.019547802438453887, 2.499999999999999556 ) ) ;
#63139 = VERTEX_POINT ( 'NONE', #59618 ) ;
#63140 = CARTESIAN_POINT ( 'NONE',  ( 17.20831665107776587, 49.13393115100078745, -7.208316651077762316 ) ) ;
#63141 = FACE_OUTER_BOUND ( 'NONE', #31114, .T. ) ;
#63142 = CARTESIAN_POINT ( 'NONE',  ( 22.81628187352647785, 46.41530133659708213, 3.434112377981063169 ) ) ;
#63143 =( LENGTH_UNIT ( ) NAMED_UNIT ( * ) SI_UNIT ( .MILLI., .METRE. ) );
#63144 = CARTESIAN_POINT ( 'NONE',  ( -46.94000000000001194, 93.00000000000000000, 5.000000000000000000 ) ) ;
#63145 = EDGE_CURVE ( 'NONE', #78251, #34327, #23292, .T. ) ;
#63146 = CARTESIAN_POINT ( 'NONE',  ( -1.780824192092290481, 0.3640475087720979608, -14.89391369643516860 ) ) ;
#63147 = CARTESIAN_POINT ( 'NONE',  ( 17.20831665107776587, 52.88393115100078035, 7.208316651077764980 ) ) ;
#63148 = CARTESIAN_POINT ( 'NONE',  ( 24.16423886937410614, 49.51208216824730357, -3.795296366450302550 ) ) ;
#63149 = CARTESIAN_POINT ( 'NONE',  ( 17.20831665107776587, 54.13393115100079456, -7.208316651077762316 ) ) ;
#63150 = VERTEX_POINT ( 'NONE', #89628 ) ;
#63151 = CARTESIAN_POINT ( 'NONE',  ( 7.361572987183169658, 19.96726448433411960, -9.846743663894592657 ) ) ;
#63152 = CARTESIAN_POINT ( 'NONE',  ( 21.09922568453595559, 57.04030133659708923, -6.408140936763230044 ) ) ;
#63153 = CARTESIAN_POINT ( 'NONE',  ( 5.076628168052703671, 56.84226448433412315, 8.527530157486179263 ) ) ;
#63155 = EDGE_CURVE ( 'NONE', #71998, #26702, #88030, .T. ) ;
#63154 = CARTESIAN_POINT ( 'NONE',  ( 1.472469842513823179, 1.425597817667451528, 4.923371831947296329 ) ) ;
#63156 = ORIENTED_EDGE ( 'NONE', *, *, #63417, .T. ) ;
#63157 = CARTESIAN_POINT ( 'NONE',  ( -4.164238869374099927, 57.01208216824731068, 3.795296366450308767 ) ) ;
#63158 =( NAMED_UNIT ( * ) PLANE_ANGLE_UNIT ( ) SI_UNIT ( $, .RADIAN. ) );
#63159 = CARTESIAN_POINT ( 'NONE',  ( -0.8801773607111009756, 43.06368534415484106, 1.068504757029289695E-15 ) ) ;
#63161 = CARTESIAN_POINT ( 'NONE',  ( 17.96484262340118221, 51.18868534415483396, -7.964842623401177768 ) ) ;
#63160 = CARTESIAN_POINT ( 'NONE',  ( 22.81628187352647785, 11.41530133659708390, 3.434112377981063169 ) ) ;
#63162 = CARTESIAN_POINT ( 'NONE',  ( 14.16722289976690163, 14.49999999999999112, -4.928467845925561974 ) ) ;
#63163 = EDGE_CURVE ( 'NONE', #25279, #48910, #35642, .T. ) ;
#63164 = CARTESIAN_POINT ( 'NONE',  ( 64.56412365047462742, 13.99999999999999467, 10.00000000000000000 ) ) ;
#63165 = FACE_OUTER_BOUND ( 'NONE', #45075, .T. ) ;
#63166 = CARTESIAN_POINT ( 'NONE',  ( 5.076628168052704559, 50.17559781766745886, -8.527530157486179263 ) ) ;
#63167 = CARTESIAN_POINT ( 'NONE',  ( 1.472469842513823179, 0.5922644843341181575, -4.923371831947296329 ) ) ;
#63168 = CARTESIAN_POINT ( 'NONE',  ( -3.795296366450300773, 32.84541550158063217, 14.16423886937410437 ) ) ;
#63169 = CARTESIAN_POINT ( 'NONE',  ( -1.099225684535947600, 9.540301336597087456, 6.408140936763237150 ) ) ;
#63171 = DIRECTION ( 'NONE',  ( -0.5547001962252290364, -0.8320502943378437211, 0.000000000000000000 ) ) ;
#63170 = CARTESIAN_POINT ( 'NONE',  ( 4.559911319644449179, 12.23035201082150714, -9.422509992056141925 ) ) ;
#63172 =( NAMED_UNIT ( * ) SI_UNIT ( $, .STERADIAN. ) SOLID_ANGLE_UNIT ( ) );
#63173 = CARTESIAN_POINT ( 'NONE',  ( 20.36894250292379738, 34.92874883491396076, -10.36894250292379027 ) ) ;
#63174 = CARTESIAN_POINT ( 'NONE',  ( 6.204703633549690345, 27.84541550158063217, 14.16423886937410082 ) ) ;
#63175 = CARTESIAN_POINT ( 'NONE',  ( 2.917880565312948704, 67.63708216824730357, 12.26659068614894643 ) ) ;
#63176 = CARTESIAN_POINT ( 'NONE',  ( -2.816281873526473856, 39.12363466993041783, 9.499525473075851096E-16 ) ) ;
#63177 = CARTESIAN_POINT ( 'NONE',  ( 17.96484262340118221, 14.93868534415483751, 7.964842623401181321 ) ) ;
#63178 = AXIS2_PLACEMENT_3D ( 'NONE', #34316, #78363, #87820 ) ;
#63179 = VECTOR ( 'NONE', #88375, 1000.000000000000227 ) ;
#63180 = VERTEX_POINT ( 'NONE', #20647 ) ;
#63181 = CARTESIAN_POINT ( 'NONE',  ( 7.361572987183169658, 34.96726448433411605, -9.846743663894592657 ) ) ;
#63182 = CARTESIAN_POINT ( 'NONE',  ( 2.035157376598824452, 38.68868534415483396, 7.964842623401179544 ) ) ;
#63183 = CARTESIAN_POINT ( 'NONE',  ( 19.84674366389459266, 63.30059781766745886, 2.638427012816836559 ) ) ;
#63185 = CARTESIAN_POINT ( 'NONE',  ( 0.1532563361054083140, 61.00893115100078745, 1.131784320476157264E-15 ) ) ;
#63184 = CARTESIAN_POINT ( 'NONE',  ( 17.08211943468705840, 25.13708216824730357, -12.26659068614894466 ) ) ;
#63186 = DIRECTION ( 'NONE',  ( 0.8526401643540917341, 0.000000000000000000, -0.5224985647159496871 ) ) ;
#63187 =( GEOMETRIC_REPRESENTATION_CONTEXT ( 3 ) GLOBAL_UNCERTAINTY_ASSIGNED_CONTEXT ( ( #60451 ) ) GLOBAL_UNIT_ASSIGNED_CONTEXT ( ( #45703, #76205, #15224 ) ) REPRESENTATION_CONTEXT ( 'NONE', 'WORKASPACE' ) );
#63188 = UNCERTAINTY_MEASURE_WITH_UNIT (LENGTH_MEASURE( 1.000000000000000082E-05 ), #49725, 'distance_accuracy_value', 'NONE');
#63189 = CARTESIAN_POINT ( 'NONE',  ( 17.20831665107776587, 29.13393115100078390, -7.208316651077762316 ) ) ;
#63190 = CARTESIAN_POINT ( 'NONE',  ( 13.43411237798105340, 55.58196800326374643, 12.81628187352647963 ) ) ;
#63191 = CARTESIAN_POINT ( 'NONE',  ( 10.00000000000000000, 54.75893115100078745, -9.846743663894594434 ) ) ;
#63192 = ORIENTED_EDGE ( 'NONE', *, *, #82650, .T. ) ;
#63193 = CARTESIAN_POINT ( 'NONE',  ( 0.000000000000000000, 0.5000000000000004441, 0.000000000000000000 ) ) ;
#63194 = CARTESIAN_POINT ( 'NONE',  ( -0.8801773607111008646, 3.272018677488171434, 2.915334737309923430 ) ) ;
#63195 = CARTESIAN_POINT ( 'NONE',  ( 12.91533473730993009, 51.60535201082149825, -10.88017736071109987 ) ) ;
#63196 = CARTESIAN_POINT ( 'NONE',  ( -4.164238869374099039, 11.80374883491396965, 8.674139862899312516E-16 ) ) ;
#63197 = CARTESIAN_POINT ( 'NONE',  ( 2.035157376598822676, 67.43868534415484817, -7.964842623401177768 ) ) ;
#63198 = CARTESIAN_POINT ( 'NONE',  ( 0.1532563361054082862, 56.21726448433411605, 2.638427012816831674 ) ) ;
#63199 = CARTESIAN_POINT ( 'NONE',  ( 4.559911319644449179, 22.23035201082150536, -9.422509992056141925 ) ) ;
#63200 = DIRECTION ( 'NONE',  ( -0.000000000000000000, 0.000000000000000000, 1.000000000000000000 ) ) ;
#63201 = CARTESIAN_POINT ( 'NONE',  ( 18.52753015748617571, 58.09226448433411605, 4.923371831947298993 ) ) ;
#63202 = EDGE_CURVE ( 'NONE', #82102, #8279, #46501, .T. ) ;
#63203 = CARTESIAN_POINT ( 'NONE',  ( 0.1532563361054083140, 1.008931151000784787, 1.131784320476157264E-15 ) ) ;
#63204 = UNCERTAINTY_MEASURE_WITH_UNIT (LENGTH_MEASURE( 1.000000000000000082E-05 ), #38628, 'distance_accuracy_value', 'NONE');
#63205 = CARTESIAN_POINT ( 'NONE',  ( 19.38216949554541202, 60.99863466993042493, 9.382169495545424454 ) ) ;
#63206 = VERTEX_POINT ( 'NONE', #65635 ) ;
#63207 = VERTEX_POINT ( 'NONE', #34641 ) ;
#63208 = DIRECTION ( 'NONE',  ( -0.000000000000000000, 1.000000000000000000, -0.000000000000000000 ) ) ;
#63209 = CARTESIAN_POINT ( 'NONE',  ( 5.810202895580461657, 14.95077488074853456, -13.56051778013764242 ) ) ;
#63210 = CARTESIAN_POINT ( 'NONE',  ( 24.16423886937409904, 44.09541550158063927, 3.795296366450317205 ) ) ;
#63211 = CARTESIAN_POINT ( 'NONE',  ( 0.1532563361054083140, 61.00893115100078745, 1.131784320476157264E-15 ) ) ;
#63212 = CARTESIAN_POINT ( 'NONE',  ( 1.472469842513823179, 15.59226448433411960, -4.923371831947296329 ) ) ;
#63213 = CARTESIAN_POINT ( 'NONE',  ( 3.836325488036175457, 14.49999999999999112, -14.50112432709429378 ) ) ;
#63215 = CARTESIAN_POINT ( 'NONE',  ( 19.84674366389459266, 58.71726448433411605, -2.638427012816827677 ) ) ;
#63214 = CARTESIAN_POINT ( 'NONE',  ( 20.88017736071110875, 25.77201867748816966, -2.915334737309920765 ) ) ;
#63216 = DIRECTION ( 'NONE',  ( 0.000000000000000000, 1.000000000000000000, 0.000000000000000000 ) ) ;
#63217 = EDGE_CURVE ( 'NONE', #94289, #27691, #41744, .T. ) ;
#63218 = CARTESIAN_POINT ( 'NONE',  ( 2.917880565312950480, 35.97041550158063217, -12.26659068614894821 ) ) ;
#63219 = CARTESIAN_POINT ( 'NONE',  ( -4.164238869374099927, 62.01208216824728936, 3.795296366450308767 ) ) ;
#63220 = CARTESIAN_POINT ( 'NONE',  ( 10.00000000000000000, 64.75893115100078035, -9.846743663894594434 ) ) ;
#63221 = CARTESIAN_POINT ( 'NONE',  ( 1.274849032794280523, 68.57228050351031357, 6.499999999999960032 ) ) ;
#63222 = CARTESIAN_POINT ( 'NONE',  ( 0.5774900079438590739, 62.64701867748817676, -5.440088680355550821 ) ) ;
#63223 = CARTESIAN_POINT ( 'NONE',  ( 17.20831665107776587, 14.13393115100078568, -7.208316651077762316 ) ) ;
#63224 = CARTESIAN_POINT ( 'NONE',  ( -7.037696230105376927, -86.26312365675100580, 3.750000000000000000 ) ) ;
#63225 = ORIENTED_EDGE ( 'NONE', *, *, #29842, .F. ) ;
#63226 = DIRECTION ( 'NONE',  ( 0.01646788341559294114, 0.9998643952135761737, 0.000000000000000000 ) ) ;
#63227 = ORIENTED_EDGE ( 'NONE', *, *, #64993, .F. ) ;
#63228 = EDGE_CURVE ( 'NONE', #16048, #44176, #65138, .T. ) ;
#63229 = CARTESIAN_POINT ( 'NONE',  ( 12.63842701281683922, 29.55059781766745175, -9.846743663894590881 ) ) ;
#63230 = ORIENTED_EDGE ( 'NONE', *, *, #95160, .F. ) ;
#63231 = VECTOR ( 'NONE', #41582, 1000.000000000000000 ) ;
#63232 = CARTESIAN_POINT ( 'NONE',  ( 22.26659068614894466, 28.88708216824730357, 7.082119434687054849 ) ) ;
#63233 = CARTESIAN_POINT ( 'NONE',  ( 1.472469842513823179, 35.59226448433412315, -4.923371831947296329 ) ) ;
#63234 = CARTESIAN_POINT ( 'NONE',  ( -0.8801773607111009756, 43.06368534415484106, 1.068504757029289695E-15 ) ) ;
#63235 = CARTESIAN_POINT ( 'NONE',  ( 14.26139399674455710, 4.125707382711286748E-16, 2.619664342929903356 ) ) ;
#63236 = VERTEX_POINT ( 'NONE', #80656 ) ;
#63237 = CARTESIAN_POINT ( 'NONE',  ( 4.559911319644449179, 42.23035201082151247, -9.422509992056141925 ) ) ;
#63238 = ADVANCED_FACE ( 'NONE', ( #21139 ), #51640, .T. ) ;
#63239 = CARTESIAN_POINT ( 'NONE',  ( 3.434112377981054287, -2.334698663402912100, -12.81628187352647608 ) ) ;
#63240 = ORIENTED_EDGE ( 'NONE', *, *, #35159, .T. ) ;
#63241 = CARTESIAN_POINT ( 'NONE',  ( 13.79529636645031943, 5.345415501580634832, -14.16423886937409904 ) ) ;
#63242 = EDGE_CURVE ( 'NONE', #22706, #52000, #31573, .T. ) ;
#63243 = VERTEX_POINT ( 'NONE', #44113 ) ;
#63244 = CARTESIAN_POINT ( 'NONE',  ( 13.43411237798105340, 35.58196800326375353, 12.81628187352647963 ) ) ;
#63245 = CARTESIAN_POINT ( 'NONE',  ( 19.84674366389459621, 23.50893115100078390, 7.409399052514197653E-17 ) ) ;
#63246 = LINE ( 'NONE', #16784, #25631 ) ;
#63247 = CARTESIAN_POINT ( 'NONE',  ( 0.1532563361054100626, 30.80059781766744820, -2.638427012816831230 ) ) ;
#63248 = COLOUR_RGB ( '', 0.66274510, 0.83137255, 0.94901961) ;
#63249 = CIRCLE ( 'NONE', #75971, 15.00000000000000000 ) ;
#63250 = ORIENTED_EDGE ( 'NONE', *, *, #41239, .F. ) ;
#63251 = CARTESIAN_POINT ( 'NONE',  ( 20.88017736071110519, 50.56368534415484106, 2.639326808657452039E-16 ) ) ;
#63252 = CARTESIAN_POINT ( 'NONE',  ( 2.393480905993088381, 14.49999999999999112, 14.80781041047758784 ) ) ;
#63253 = AXIS2_PLACEMENT_3D ( 'NONE', #38199, #62142, #94622 ) ;
#63254 = CARTESIAN_POINT ( 'NONE',  ( 0.4195498155886317471, 0.5000000000000013323, 9.500000000000000000 ) ) ;
#63255 = CARTESIAN_POINT ( 'NONE',  ( 1.472469842513823179, 5.592264484334118713, -4.923371831947296329 ) ) ;
#63256 = CARTESIAN_POINT ( 'NONE',  ( 21.09922568453595559, 12.04030133659708746, -6.408140936763230044 ) ) ;
#63257 = CARTESIAN_POINT ( 'NONE',  ( -6.138934250732154041, -0.03417435944610275333, 14.77128574976603481 ) ) ;
#63258 = CARTESIAN_POINT ( 'NONE',  ( 12.63842701281683034, 47.46726448433412315, 9.846743663894596210 ) ) ;
#63259 = CARTESIAN_POINT ( 'NONE',  ( -2.816281873526473856, 64.12363466993042493, 9.499525473075851096E-16 ) ) ;
#63260 = CARTESIAN_POINT ( 'NONE',  ( -4.164238869374099039, 11.80374883491396965, 8.674139862899312516E-16 ) ) ;
#63261 = CARTESIAN_POINT ( 'NONE',  ( 18.52753015748618282, 13.92559781766745175, -4.923371831947291888 ) ) ;
#63262 = CARTESIAN_POINT ( 'NONE',  ( 22.81628187352648496, 36.83196800326376064, -3.434112377981050290 ) ) ;
#63264 = LINE ( 'NONE', #45826, #97710 ) ;
#63263 = DIRECTION ( 'NONE',  ( -1.000000000000000000, -0.000000000000000000, -0.000000000000000000 ) ) ;
#63265 = CARTESIAN_POINT ( 'NONE',  ( 12.91533473730992121, 54.52201867748816255, 10.88017736071110164 ) ) ;
#63266 = CARTESIAN_POINT ( 'NONE',  ( 6.565887622018943937, 10.16530133659708746, 12.81628187352647430 ) ) ;
#63267 = CARTESIAN_POINT ( 'NONE',  ( 9.779999999999990479, 18.09999999999999787, 0.000000000000000000 ) ) ;
#63268 = CARTESIAN_POINT ( 'NONE',  ( 19.84674366389459266, 23.30059781766745530, 2.638427012816836559 ) ) ;
#63270 = EDGE_CURVE ( 'NONE', #65600, #63150, #36948, .T. ) ;
#63269 = CARTESIAN_POINT ( 'NONE',  ( 4.559911319644449179, 32.23035201082150536, -9.422509992056141925 ) ) ;
#63271 = CARTESIAN_POINT ( 'NONE',  ( -2.816281873526473856, 34.33196800326376064, 3.434112377981055619 ) ) ;
#63272 = AXIS2_PLACEMENT_3D ( 'NONE', #56174, #78673, #93168 ) ;
#63273 = CARTESIAN_POINT ( 'NONE',  ( 0.1532563361054083140, 26.00893115100078745, 1.131784320476157264E-15 ) ) ;
#63274 = VECTOR ( 'NONE', #30430, 999.9999999999998863 ) ;
#63275 = FILL_AREA_STYLE ('',( #86290 ) ) ;
#63276 = CARTESIAN_POINT ( 'NONE',  ( 17.85158348494333680, 44.73726573380442773, -6.500000000000027534 ) ) ;
#63277 = VECTOR ( 'NONE', #66103, 1000.000000000000114 ) ;
#63278 = CARTESIAN_POINT ( 'NONE',  ( 15.44008868035555793, 16.39701867748817321, -9.422509992056140149 ) ) ;
#63279 = CARTESIAN_POINT ( 'NONE',  ( 17.96484262340118221, 56.18868534415484817, -7.964842623401177768 ) ) ;
#63280 = DIRECTION ( 'NONE',  ( -0.5075383629607084224, 0.000000000000000000, 0.8616291604415231564 ) ) ;
#63282 = CARTESIAN_POINT ( 'NONE',  ( -0.8801773607110991993, 22.85535201082150181, -2.915334737309923874 ) ) ;
#63281 = CARTESIAN_POINT ( 'NONE',  ( 10.00000000000000000, 39.75893115100078745, -9.846743663894594434 ) ) ;
#63283 = DIRECTION ( 'NONE',  ( 6.608470384673550777E-17, 1.000000000000000000, -0.000000000000000000 ) ) ;
#63284 = CARTESIAN_POINT ( 'NONE',  ( 2.035157376598822676, 42.43868534415483396, -7.964842623401177768 ) ) ;
#63285 = CARTESIAN_POINT ( 'NONE',  ( 15.44008868035555260, 9.730352010821505360, 9.422509992056143702 ) ) ;
#63286 = CARTESIAN_POINT ( 'NONE',  ( 10.00000000000000178, 17.25893115100078745, 9.846743663894594434 ) ) ;
#63287 = CARTESIAN_POINT ( 'NONE',  ( 12.63842701281683922, 39.55059781766744464, -9.846743663894590881 ) ) ;
#63288 = LINE ( 'NONE', #40318, #88003 ) ;
#63289 = SURFACE_STYLE_USAGE ( .BOTH. , #71791 ) ;
#63290 = CARTESIAN_POINT ( 'NONE',  ( 17.08211943468705840, 25.13708216824730357, -12.26659068614894466 ) ) ;
#63291 = CARTESIAN_POINT ( 'NONE',  ( 5.076628168052704559, 40.17559781766745175, -8.527530157486179263 ) ) ;
#63292 = FACE_OUTER_BOUND ( 'NONE', #97027, .T. ) ;
#63293 = EDGE_LOOP ( 'NONE', ( #42821, #82196, #54532, #76396 ) ) ;
#63294 = CARTESIAN_POINT ( 'NONE',  ( 20.88017736071110875, 5.772018677488170546, -2.915334737309920765 ) ) ;
#63295 = CARTESIAN_POINT ( 'NONE',  ( 2.791683348922240793, 26.63393115100078745, 7.208316651077764092 ) ) ;
#63297 = CARTESIAN_POINT ( 'NONE',  ( -7.754961693898215991, 84.52280956283338753, -4.000000000000000000 ) ) ;
#63296 = CARTESIAN_POINT ( 'NONE',  ( 0.000000000000000000, 0.5000000000000004441, 0.000000000000000000 ) ) ;
#63298 = CARTESIAN_POINT ( 'NONE',  ( 7.084665262690076126, 44.10535201082151247, 10.88017736071109987 ) ) ;
#63299 = CARTESIAN_POINT ( 'NONE',  ( 5.240416992896709480, 14.95077488074852390, 13.79072622793305136 ) ) ;
#63300 = VECTOR ( 'NONE', #3970, 1000.000000000000000 ) ;
#63301 = CARTESIAN_POINT ( 'NONE',  ( 7.084665262690076126, 12.02201867748817143, -10.88017736071110164 ) ) ;
#63302 = CARTESIAN_POINT ( 'NONE',  ( -1.099225684535947600, 43.70696800326375353, -6.408140936763238038 ) ) ;
#63303 = CARTESIAN_POINT ( 'NONE',  ( -2.816281873526473856, 14.33196800326375531, 3.434112377981055619 ) ) ;
#63304 = CARTESIAN_POINT ( 'NONE',  ( 2.791683348922240793, 16.63393115100078745, 7.208316651077764092 ) ) ;
#63305 = VERTEX_POINT ( 'NONE', #35134 ) ;
#63306 = CARTESIAN_POINT ( 'NONE',  ( -13.78891971893217239, 14.49999999999999112, 5.904717858191482094 ) ) ;
#63307 = CARTESIAN_POINT ( 'NONE',  ( 6.204703633549690345, 47.84541550158064638, 14.16423886937410082 ) ) ;
#63308 = CARTESIAN_POINT ( 'NONE',  ( 2.917880565312948704, 27.63708216824730357, 12.26659068614894643 ) ) ;
#63309 = CARTESIAN_POINT ( 'NONE',  ( 12.91533473730993009, 16.60535201082150891, -10.88017736071109987 ) ) ;
#63311 = DIRECTION ( 'NONE',  ( 0.000000000000000000, 0.000000000000000000, -1.000000000000000000 ) ) ;
#63310 = CARTESIAN_POINT ( 'NONE',  ( 12.91533473730993009, 51.60535201082149825, -10.88017736071109987 ) ) ;
#63312 = FACE_OUTER_BOUND ( 'NONE', #14597, .T. ) ;
#63313 = CARTESIAN_POINT ( 'NONE',  ( 18.04007052943771683, 48.01528370094807485, 5.767676674365856293 ) ) ;
#63314 = CARTESIAN_POINT ( 'NONE',  ( 2.791683348922237240, 10.38393115100078390, -7.208316651077763204 ) ) ;
#63315 = CARTESIAN_POINT ( 'NONE',  ( 0.000000000000000000, 15.00000000000000000, 0.000000000000000000 ) ) ;
#63316 = CARTESIAN_POINT ( 'NONE',  ( 7.361572987183170547, 22.05059781766745530, 9.846743663894590881 ) ) ;
#63317 = CARTESIAN_POINT ( 'NONE',  ( 5.076628168052704559, 0.1755978176674514724, -8.527530157486179263 ) ) ;
#63318 = CARTESIAN_POINT ( 'NONE',  ( 17.20831665107776587, 24.13393115100078035, -7.208316651077762316 ) ) ;
#63319 = CARTESIAN_POINT ( 'NONE',  ( 5.076628168052703671, 46.84226448433412315, 8.527530157486179263 ) ) ;
#63320 = ADVANCED_FACE ( 'NONE', ( #29115 ), #51135, .T. ) ;
#63321 = VECTOR ( 'NONE', #22860, 1000.000000000000000 ) ;
#63322 = CARTESIAN_POINT ( 'NONE',  ( 15.44008868035555260, 14.73035201082150536, 9.422509992056143702 ) ) ;
#63323 = AXIS2_PLACEMENT_3D ( 'NONE', #12748, #50247, #13748 ) ;
#63324 = UNCERTAINTY_MEASURE_WITH_UNIT (LENGTH_MEASURE( 1.000000000000000082E-05 ), #52443, 'distance_accuracy_value', 'NONE');
#63325 = CARTESIAN_POINT ( 'NONE',  ( 13.43411237798105340, 35.58196800326375353, 12.81628187352647963 ) ) ;
#63326 = CARTESIAN_POINT ( 'NONE',  ( 20.88017736071110164, 55.35535201082149825, 2.915334737309930979 ) ) ;
#63327 = CARTESIAN_POINT ( 'NONE',  ( 19.84674366389459266, 28.30059781766745886, 2.638427012816836559 ) ) ;
#63329 = CARTESIAN_POINT ( 'NONE',  ( 19.84674366389459621, 23.50893115100078390, 7.409399052514197653E-17 ) ) ;
#63328 = CARTESIAN_POINT ( 'NONE',  ( 6.204703633549690345, 40.76208216824731778, -14.16423886937410259 ) ) ;
#63331 = ADVANCED_FACE ( 'NONE', ( #8113 ), #92581, .F. ) ;
#63330 = CARTESIAN_POINT ( 'NONE',  ( 18.72515096720571037, 55.05509018479936145, 6.499999999999982236 ) ) ;
#63332 = CIRCLE ( 'NONE', #69693, 3.000000000000002665 ) ;
#63333 = EDGE_CURVE ( 'NONE', #29027, #53769, #76912, .T. ) ;
#63334 = CARTESIAN_POINT ( 'NONE',  ( 12.63842701281683034, 47.46726448433412315, 9.846743663894596210 ) ) ;
#63336 = CARTESIAN_POINT ( 'NONE',  ( 10.00000000000000000, 15.55374883491396787, -14.16423886937410082 ) ) ;
#63335 = CARTESIAN_POINT ( 'NONE',  ( 14.92337183194729633, 37.67559781766745175, 8.527530157486181039 ) ) ;
#63337 = CARTESIAN_POINT ( 'NONE',  ( 17.08211943468705130, 23.47041550158063572, 12.26659068614894998 ) ) ;
#63338 = CARTESIAN_POINT ( 'NONE',  ( 18.52753015748618282, 28.92559781766745175, -4.923371831947291888 ) ) ;
#63339 = CARTESIAN_POINT ( 'NONE',  ( 2.035157376598824452, 48.68868534415483396, 7.964842623401179544 ) ) ;
#63340 = CARTESIAN_POINT ( 'NONE',  ( 17.96484262340118221, 26.18868534415483396, -7.964842623401177768 ) ) ;
#63341 = CARTESIAN_POINT ( 'NONE',  ( 19.42250999205614548, 45.98035201082150536, -5.440088680355545492 ) ) ;
#63342 = CARTESIAN_POINT ( 'NONE',  ( -0.8801773607111008646, 28.27201867748817321, 2.915334737309923430 ) ) ;
#63343 = VERTEX_POINT ( 'NONE', #54575 ) ;
#63344 = CARTESIAN_POINT ( 'NONE',  ( 20.88017736071110519, 55.56368534415484817, 2.639326808657452039E-16 ) ) ;
#63345 = VERTEX_POINT ( 'NONE', #30099 ) ;
#63346 = CARTESIAN_POINT ( 'NONE',  ( -1.099225684535947600, 53.70696800326376064, -6.408140936763238038 ) ) ;
#63347 = VECTOR ( 'NONE', #67980, 1000.000000000000000 ) ;
#63348 = CARTESIAN_POINT ( 'NONE',  ( 10.00000000000000178, 59.31368534415484106, 10.88017736071110342 ) ) ;
#63349 = ORIENTED_EDGE ( 'NONE', *, *, #17550, .T. ) ;
#63350 = VECTOR ( 'NONE', #8135, 1000.000000000000000 ) ;
#63351 = LINE ( 'NONE', #93855, #31723 ) ;
#63352 = AXIS2_PLACEMENT_3D ( 'NONE', #10057, #10542, #64013 ) ;
#63353 = CARTESIAN_POINT ( 'NONE',  ( 20.15039907845753930, 70.00000000000000000, -6.262539305110068177 ) ) ;
#63354 = LINE ( 'NONE', #25386, #40866 ) ;
#63355 = CARTESIAN_POINT ( 'NONE',  ( 22.26659068614895176, 54.72041550158063217, -7.082119434687042414 ) ) ;
#63356 = CARTESIAN_POINT ( 'NONE',  ( 0.1532563361054082862, 6.217264484334118713, 2.638427012816831674 ) ) ;
#63357 = ADVANCED_FACE ( 'NONE', ( #44622 ), #75117, .F. ) ;
#63358 = CARTESIAN_POINT ( 'NONE',  ( 24.16423886937409904, 4.095415501580634832, 3.795296366450317205 ) ) ;
#63359 = CARTESIAN_POINT ( 'NONE',  ( 0.1532563361054083140, 1.008931151000784787, 1.131784320476157264E-15 ) ) ;
#63360 = CARTESIAN_POINT ( 'NONE',  ( 19.42250999205614548, 10.98035201082150358, -5.440088680355545492 ) ) ;
#63361 = CARTESIAN_POINT ( 'NONE',  ( 0.1532563361054100626, 45.80059781766745886, -2.638427012816831230 ) ) ;
#63362 = EDGE_LOOP ( 'NONE', ( #92984, #97322, #80614 ) ) ;
#63363 = ADVANCED_FACE ( 'NONE', ( #15627 ), #48133, .F. ) ;
#63364 = CARTESIAN_POINT ( 'NONE',  ( 5.076628168052704559, 50.17559781766745886, -8.527530157486179263 ) ) ;
#63365 = ORIENTED_EDGE ( 'NONE', *, *, #29563, .F. ) ;
#63366 = DIRECTION ( 'NONE',  ( -1.000000000000000000, 0.000000000000000000, 0.000000000000000000 ) ) ;
#63367 = CARTESIAN_POINT ( 'NONE',  ( -0.8801773607110991993, 37.85535201082151247, -2.915334737309923874 ) ) ;
#63368 = CARTESIAN_POINT ( 'NONE',  ( 7.361572987183170547, 52.05059781766745175, 9.846743663894590881 ) ) ;
#63369 = CARTESIAN_POINT ( 'NONE',  ( -13.61912076658552095, 7.098136097991034869E-16, 5.334594295380809648 ) ) ;
#63370 = CARTESIAN_POINT ( 'NONE',  ( -0.8801773607110991993, 57.85535201082149825, -2.915334737309923874 ) ) ;
#63371 = CARTESIAN_POINT ( 'NONE',  ( 10.00000000000000000, 11.81368534415483751, -10.88017736071110342 ) ) ;
#63372 = CARTESIAN_POINT ( 'NONE',  ( 13.43411237798106583, 47.66530133659709634, -12.81628187352647252 ) ) ;
#63373 = CARTESIAN_POINT ( 'NONE',  ( 24.35999999999999233, 44.49999999999997868, -9.500000000000000000 ) ) ;
#63374 = ORIENTED_EDGE ( 'NONE', *, *, #3351, .F. ) ;
#63375 = CARTESIAN_POINT ( 'NONE',  ( -1.099225684535947600, 34.54030133659708923, 6.408140936763237150 ) ) ;
#63376 = CARTESIAN_POINT ( 'NONE',  ( 12.91533473730993009, 31.60535201082150891, -10.88017736071109987 ) ) ;
#63377 = VECTOR ( 'NONE', #60516, 1000.000000000000000 ) ;
#63378 =( BOUNDED_SURFACE ( )  B_SPLINE_SURFACE ( 1, 2, ( 
 ( #56844, #86371, #77869, #33342, #9885, #9380, #48355, #56366, #70884, #32858, #87343, #64329, #71379, #39883, #63836, #2892, #24401, #63358, #10373, #94350, #78861, #18858, #79355, #8884, #71850, #39401, #85380, #40874, #25869, #86859, #47371, #62870, #93366, #93861, #41383, #55379, #47860, #18365, #85879, #25389, #94841, #69894, #48844, #26343, #49338, #17391, #55872, #3360, #33824, #78366, #1414, #31867, #40385, #62366, #54869, #16893, #87823, #3859, #89315, #27323, #13313, #79838, #19343, #50315, #11343, #42343, #72818, #43313, #35317, #28315, #4358, #65314, #58302, #34824, #65810, #81796, #95840, #35818, #66304, #57821, #80829, #73318, #81320, #49826, #42834, #95336, #80336, #20331, #88818, #41863, #11835, #12814, #88329, #19827, #72326, #20823, #50826, #12329, #34319, #4841, #73807, #96343, #5337, #27817, #96840, #58807, #51313, #64817, #26835, #57329, #26658, #33654, #40195, #26176, #64149, #55182, #63663, #71678, #94667, #48668, #49643, #41685, #70208, #34145, #1727, #47694, #41198, #79169, #87156, #9699, #32681, #63174, #25699, #72155, #86193, #10198, #56668, #70702, #86683, #57153, #32182, #11166, #87651, #11661, #78687, #56189, #3188, #18187, #40692, #18681, #10684, #93682, #49167, #33170, #71193, #2221, #24711, #19164, #2716, #62684, #93185, #25215, #94168, #85699, #55696, #17705, #79669, #3683, #64639, #48175, #95147, #80150, #17216, #78186, #83177, #45174, #30653, #695, #31148, #9147, #54147, #39166, #46172, #60664, #39664, #45673, #61159, #14702, #8176, #70156, #52676, #83676, #47133, #75675, #69172, #61639, #62131, #7188, #84656, #46648, #8653, #62625, #92639, #16164, #98710, #1673, #32126, #54634, #15191, #23683, #85152, #77144, #92160, #53663, #69655, #1181, #31639, #24163, #53170, #93130, #37691, #16658, #68190, #91164, #77630, #91668, #30161, #23187, #22691, #38670, #76171, #7691, #15686, #84179, #38188, #68675, #202, #76655, #65077, #24657, #63127, #18142, #55126, #17653, #48123, #41635, #3138, #57099, #78638, #40640, #26128, #10145, #33600, #10631, #11116, #55639, #72101, #71138, #56137, #41143, #79615, #93629, #79118, #9647, #25164, #18623, #87108, #42120, #86139, #3628, #2666, #33117, #34583, #87595, #64097, #25644, #72586, #2171, #71628, #4120, #49114, #49585, #63611, #94117, #94613, #86632, #48614, #32628, #56619, #85642, #26602, #34095, #64586, #95094, #19105, #80098, #11603, #17161, #47641, #78137, #40144, #70648, #88087, #97108, #43086, #52078, #44565, #74067, #65576, #21085, #96603, #96103, #36078, #44063, #58578, #89080, #75063, #82571, #59070, #27587, #51583, #89574, #80600, #20594, #28579 ),
 ( #35587, #82069, #51080, #58077, #13579, #6570, #81571, #73571, #74570, #28080, #50095, #57590, #88581, #20089, #50593, #73079, #29062, #6084, #4615, #21587, #36586, #13079, #66581, #67073, #81085, #5096, #43574, #5599, #97601, #59570, #12586, #12098, #90063, #19600, #27087, #14085, #66075, #37082, #95601, #42601, #35076, #47023, #53542, #15085, #54037, #94, #22084, #29548, #37578, #98598, #91047, #45053, #1061, #69053, #75563, #92523, #77037, #38071, #38558, #68563, #30541, #91554, #24050, #98090, #90555, #54520, #7076, #589, #53046, #68071, #69544, #61532, #14584, #52559, #76543, #23569, #85036, #16548, #77514, #30048, #31527, #76053, #39049, #60054, #83063, #45556, #15575, #46056, #9031, #31032, #84548, #61041, #60556, #67581, #22575, #7583, #83565, #23073, #84055, #8061, #92041, #62022, #16047, #46536, #8550, #50333, #1560, #72835, #34838, #95859, #50842, #80846, #4373, #85528, #96361, #27834, #42849, #2051, #11852, #73333, #42362, #80354, #41880, #65333, #27343, #57836, #19843, #40026, #88838, #20346, #12343, #62511, #78022, #4860, #49356, #58320, #65829, #18874, #11361, #35336, #81334, #72343, #39548, #70528, #93016, #70037, #88345, #79858, #32008, #24553, #3876, #55010, #17040, #9525, #32514, #64349, #47519, #94857, #26359, #56859, #87360, #34339, #64834, #95353, #26852, #57349, #87842, #19361, #49845, #35835, #37828, #51333, #44804, #97346, #81815, #14834, #6820, #58823, #96858, #21835, #67826, #98837, #68318, #60795, #74312, #45309, #21336, #83311, #43331, #5356, #89815, #59806, #90300, #30293, #14331, #98343, #6321, #20841, #91295, #5839, #51826, #73823, #67322, #22818, #12831, #43817, #7325, #66322, #29310, #52318, #22330, #28333, #75309, #37336, #29801, #53298, #52804, #60310, #89331, #13333, #36329, #75805, #66824, #82811, #28817, #90803, #59316, #13834, #82313, #44315, #74816, #36830, #97845, #32756, #63251, #55267, #7819, #23320, #62765, #92289, #2299, #9778, #61778, #54274, #24791, #40276, #16299, #17290, #84313, #38314, #85780, #77768, #23812, #25289, #69795, #24302, #1804, #46299, #84790, #46780, #8784, #32261, #62265, #69299, #343, #77274, #76302, #15331, #39303, #1321, #16791, #31772, #53802, #9281, #93760, #92773, #31278, #54764, #68810, #45814, #15813, #76786, #8303, #61290, #47766, #85283, #91799, #70783, #93267, #47266, #39789, #70289, #78264, #83806, #30785, #38802, #822, #80727, #94243, #87725, #41277, #25772, #57717, #49720, #2795, #40769, #64715, #11735, #42732, #12221, #4741, #18264, #88218, #64227, #27219, #86266, #48253, #33727, #3761, #34217, #73210, #57226, #42245, #49242, #63740 ) ),
 .UNSPECIFIED., .F., .F., .F. ) 
 B_SPLINE_SURFACE_WITH_KNOTS ( ( 2, 2 ),
 ( 3, 2, 2, 2, 2, 2, 2, 2, 2, 2, 2, 2, 2, 2, 2, 2, 2, 2, 2, 2, 2, 2, 2, 2, 2, 2, 2, 2, 2, 2, 2, 2, 2, 2, 2, 2, 2, 2, 2, 2, 2, 2, 2, 2, 2, 2, 2, 2, 2, 2, 2, 2, 2, 2, 2, 2, 2, 2, 2, 2, 2, 2, 2, 2, 2, 2, 2, 2, 2, 2, 2, 2, 2, 2, 2, 2, 2, 2, 2, 2, 2, 2, 2, 2, 2, 2, 2, 2, 2, 2, 2, 2, 2, 2, 2, 2, 2, 2, 2, 2, 2, 2, 2, 2, 2, 2, 2, 2, 2, 2, 2, 2, 2, 2, 2, 2, 2, 2, 2, 2, 2, 2, 2, 2, 2, 2, 2, 2, 2, 2, 2, 2, 2, 2, 2, 2, 2, 2, 2, 2, 2, 2, 2, 2, 2, 2, 2, 2, 2, 2, 2, 2, 2, 2, 2, 2, 2, 2, 2, 2, 2, 2, 3 ),
 ( 0.000000000000000000, 1.000000000000000000 ),
 ( 0.000000000000000000, 0.005952380952380952051, 0.01190476190476190410, 0.01785714285714285615, 0.02380952380952380820, 0.02976190476190476025, 0.03571428571428571230, 0.04166666666666666435, 0.04761904761904761640, 0.05357142857142856845, 0.05952380952380952051, 0.06547619047619047949, 0.07142857142857142461, 0.07738095238095238360, 0.08333333333333332871, 0.08928571428571428770, 0.09523809523809523281, 0.1011904761904761918, 0.1071428571428571369, 0.1130952380952380959, 0.1190476190476190410, 0.1250000000000000000, 0.1309523809523809590, 0.1369047619047619180, 0.1428571428571428492, 0.1488095238095238082, 0.1547619047619047672, 0.1607142857142857262, 0.1666666666666666574, 0.1726190476190476164, 0.1785714285714285754, 0.1845238095238095344, 0.1904761904761904656, 0.1964285714285714246, 0.2023809523809523836, 0.2083333333333333426, 0.2142857142857142738, 0.2202380952380952328, 0.2261904761904761918, 0.2321428571428571508, 0.2380952380952380820, 0.2440476190476190410, 0.2500000000000000000, 0.2559523809523809312, 0.2619047619047619180, 0.2678571428571428492, 0.2738095238095238360, 0.2797619047619047672, 0.2857142857142856984, 0.2916666666666666852, 0.2976190476190476164, 0.3035714285714285476, 0.3095238095238095344, 0.3154761904761904656, 0.3214285714285714524, 0.3273809523809523836, 0.3333333333333333148, 0.3392857142857143016, 0.3452380952380952328, 0.3511904761904761640, 0.3571428571428571508, 0.3630952380952380820, 0.3690476190476190688, 0.3750000000000000000, 0.3809523809523809312, 0.3869047619047619180, 0.3928571428571428492, 0.3988095238095238360, 0.4047619047619047672, 0.4107142857142856984, 0.4166666666666666852, 0.4226190476190476164, 0.4285714285714285476, 0.4345238095238095344, 0.4404761904761904656, 0.4464285714285714524, 0.4523809523809523836, 0.4583333333333333148, 0.4642857142857143016, 0.4702380952380952328, 0.4761904761904761640, 0.4821428571428571508, 0.4880952380952380820, 0.4940476190476190688, 0.5000000000000000000, 0.5059523809523809312, 0.5119047619047618625, 0.5178571428571429047, 0.5238095238095238360, 0.5297619047619047672, 0.5357142857142856984, 0.5416666666666666297, 0.5476190476190476719, 0.5535714285714286031, 0.5595238095238095344, 0.5654761904761904656, 0.5714285714285713969, 0.5773809523809523281, 0.5833333333333333703, 0.5892857142857143016, 0.5952380952380952328, 0.6011904761904761640, 0.6071428571428570953, 0.6130952380952381375, 0.6190476190476190688, 0.6250000000000000000, 0.6309523809523809312, 0.6369047619047618625, 0.6428571428571429047, 0.6488095238095238360, 0.6547619047619047672, 0.6607142857142856984, 0.6666666666666666297, 0.6726190476190476719, 0.6785714285714286031, 0.6845238095238095344, 0.6904761904761904656, 0.6964285714285713969, 0.7023809523809523281, 0.7083333333333333703, 0.7142857142857143016, 0.7202380952380952328, 0.7261904761904761640, 0.7321428571428570953, 0.7380952380952381375, 0.7440476190476190688, 0.7500000000000000000, 0.7559523809523809312, 0.7619047619047618625, 0.7678571428571429047, 0.7738095238095238360, 0.7797619047619047672, 0.7857142857142856984, 0.7916666666666666297, 0.7976190476190476719, 0.8035714285714286031, 0.8095238095238095344, 0.8154761904761904656, 0.8214285714285713969, 0.8273809523809523281, 0.8333333333333333703, 0.8392857142857143016, 0.8452380952380952328, 0.8511904761904761640, 0.8571428571428570953, 0.8630952380952381375, 0.8690476190476190688, 0.8750000000000000000, 0.8809523809523809312, 0.8869047619047618625, 0.8928571428571429047, 0.8988095238095238360, 0.9047619047619047672, 0.9107142857142856984, 0.9166666666666666297, 0.9226190476190476719, 0.9285714285714286031, 0.9345238095238095344, 0.9404761904761904656, 0.9464285714285713969, 0.9523809523809523281, 0.9583333333333333703, 0.9642857142857143016 ),
 .UNSPECIFIED. ) 
 GEOMETRIC_REPRESENTATION_ITEM ( )  RATIONAL_B_SPLINE_SURFACE ( (
 ( 1.000000000000000000, 0.9659258262890683122, 1.000000000000000000, 0.9659258262890683122, 1.000000000000000000, 0.9659258262890683122, 1.000000000000000000, 0.9659258262890683122, 1.000000000000000000, 0.9659258262890683122, 1.000000000000000000, 0.9659258262890683122, 1.000000000000000000, 0.9659258262890683122, 1.000000000000000000, 0.9659258262890683122, 1.000000000000000000, 0.9659258262890683122, 1.000000000000000000, 0.9659258262890683122, 1.000000000000000000, 0.9659258262890683122, 1.000000000000000000, 0.9659258262890683122, 1.000000000000000000, 0.9659258262890683122, 1.000000000000000000, 0.9659258262890683122, 1.000000000000000000, 0.9659258262890683122, 1.000000000000000000, 0.9659258262890683122, 1.000000000000000000, 0.9659258262890683122, 1.000000000000000000, 0.9659258262890683122, 1.000000000000000000, 0.9659258262890683122, 1.000000000000000000, 0.9659258262890683122, 1.000000000000000000, 0.9659258262890683122, 1.000000000000000000, 0.9659258262890683122, 1.000000000000000000, 0.9659258262890683122, 1.000000000000000000, 0.9659258262890683122, 1.000000000000000000, 0.9659258262890683122, 1.000000000000000000, 0.9659258262890683122, 1.000000000000000000, 0.9659258262890683122, 1.000000000000000000, 0.9659258262890683122, 1.000000000000000000, 0.9659258262890683122, 1.000000000000000000, 0.9659258262890683122, 1.000000000000000000, 0.9659258262890683122, 1.000000000000000000, 0.9659258262890683122, 1.000000000000000000, 0.9659258262890683122, 1.000000000000000000, 0.9659258262890683122, 1.000000000000000000, 0.9659258262890683122, 1.000000000000000000, 0.9659258262890683122, 1.000000000000000000, 0.9659258262890683122, 1.000000000000000000, 0.9659258262890683122, 1.000000000000000000, 0.9659258262890683122, 1.000000000000000000, 0.9659258262890683122, 1.000000000000000000, 0.9659258262890683122, 1.000000000000000000, 0.9659258262890683122, 1.000000000000000000, 0.9659258262890683122, 1.000000000000000000, 0.9659258262890683122, 1.000000000000000000, 0.9659258262890683122, 1.000000000000000000, 0.9659258262890683122, 1.000000000000000000, 0.9659258262890683122, 1.000000000000000000, 0.9659258262890683122, 1.000000000000000000, 0.9659258262890683122, 1.000000000000000000, 0.9659258262890683122, 1.000000000000000000, 0.9659258262890683122, 1.000000000000000000, 0.9659258262890683122, 1.000000000000000000, 0.9659258262890683122, 1.000000000000000000, 0.9659258262890683122, 1.000000000000000000, 0.9659258262890683122, 1.000000000000000000, 0.9659258262890683122, 1.000000000000000000, 0.9659258262890683122, 1.000000000000000000, 0.9659258262890683122, 1.000000000000000000, 0.9659258262890683122, 1.000000000000000000, 0.9659258262890683122, 1.000000000000000000, 0.9659258262890683122, 1.000000000000000000, 0.9659258262890683122, 1.000000000000000000, 0.9659258262890683122, 1.000000000000000000, 0.9659258262890683122, 1.000000000000000000, 0.9659258262890683122, 1.000000000000000000, 0.9659258262890683122, 1.000000000000000000, 0.9659258262890683122, 1.000000000000000000, 0.9659258262890683122, 1.000000000000000000, 0.9659258262890683122, 1.000000000000000000, 0.9659258262890683122, 1.000000000000000000, 0.9659258262890683122, 1.000000000000000000, 0.9659258262890683122, 1.000000000000000000, 0.9659258262890683122, 1.000000000000000000, 0.9659258262890683122, 1.000000000000000000, 0.9659258262890683122, 1.000000000000000000, 0.9659258262890683122, 1.000000000000000000, 0.9659258262890683122, 1.000000000000000000, 0.9659258262890683122, 1.000000000000000000, 0.9659258262890683122, 1.000000000000000000, 0.9659258262890683122, 1.000000000000000000, 0.9659258262890683122, 1.000000000000000000, 0.9659258262890683122, 1.000000000000000000, 0.9659258262890683122, 1.000000000000000000, 0.9659258262890683122, 1.000000000000000000, 0.9659258262890683122, 1.000000000000000000, 0.9659258262890683122, 1.000000000000000000, 0.9659258262890683122, 1.000000000000000000, 0.9659258262890683122, 1.000000000000000000, 0.9659258262890683122, 1.000000000000000000, 0.9659258262890683122, 1.000000000000000000, 0.9659258262890683122, 1.000000000000000000, 0.9659258262890683122, 1.000000000000000000, 0.9659258262890683122, 1.000000000000000000, 0.9659258262890683122, 1.000000000000000000, 0.9659258262890683122, 1.000000000000000000, 0.9659258262890683122, 1.000000000000000000, 0.9659258262890683122, 1.000000000000000000, 0.9659258262890683122, 1.000000000000000000, 0.9659258262890683122, 1.000000000000000000, 0.9659258262890683122, 1.000000000000000000, 0.9659258262890683122, 1.000000000000000000, 0.9659258262890683122, 1.000000000000000000, 0.9659258262890683122, 1.000000000000000000, 0.9659258262890683122, 1.000000000000000000, 0.9659258262890683122, 1.000000000000000000, 0.9659258262890683122, 1.000000000000000000, 0.9659258262890683122, 1.000000000000000000, 0.9659258262890683122, 1.000000000000000000, 0.9659258262890683122, 1.000000000000000000, 0.9659258262890683122, 1.000000000000000000, 0.9659258262890683122, 1.000000000000000000, 0.9659258262890683122, 1.000000000000000000, 0.9659258262890683122, 1.000000000000000000, 0.9659258262890683122, 1.000000000000000000, 0.9659258262890683122, 1.000000000000000000, 0.9659258262890683122, 1.000000000000000000, 0.9659258262890683122, 1.000000000000000000, 0.9659258262890683122, 1.000000000000000000, 0.9659258262890683122, 1.000000000000000000, 0.9659258262890683122, 1.000000000000000000, 0.9659258262890683122, 1.000000000000000000, 0.9659258262890683122, 1.000000000000000000, 0.9659258262890683122, 1.000000000000000000, 0.9659258262890683122, 1.000000000000000000, 0.9659258262890683122, 1.000000000000000000, 0.9659258262890683122, 1.000000000000000000, 0.9659258262890683122, 1.000000000000000000, 0.9659258262890683122, 1.000000000000000000, 0.9659258262890683122, 1.000000000000000000, 0.9659258262890683122, 1.000000000000000000, 0.9659258262890683122, 1.000000000000000000, 0.9659258262890683122, 1.000000000000000000, 0.9659258262890683122, 1.000000000000000000, 0.9659258262890683122, 1.000000000000000000, 0.9659258262890683122, 1.000000000000000000, 0.9659258262890683122, 1.000000000000000000, 0.9659258262890683122, 1.000000000000000000, 0.9659258262890683122, 1.000000000000000000, 0.9659258262890683122, 1.000000000000000000, 0.9659258262890683122, 1.000000000000000000, 0.9659258262890683122, 1.000000000000000000, 0.9659258262890683122, 1.000000000000000000, 0.9659258262890683122, 1.000000000000000000, 0.9659258262890683122, 1.000000000000000000, 0.9659258262890683122, 1.000000000000000000, 0.9659258262890683122, 1.000000000000000000, 0.9659258262890683122, 1.000000000000000000, 0.9659258262890683122, 1.000000000000000000, 0.9659258262890683122, 1.000000000000000000, 0.9659258262890683122, 1.000000000000000000, 0.9659258262890683122, 1.000000000000000000, 0.9659258262890683122, 1.000000000000000000, 0.9659258262890683122, 1.000000000000000000, 0.9659258262890683122, 1.000000000000000000, 0.9659258262890683122, 1.000000000000000000, 0.9659258262890683122, 1.000000000000000000, 0.9659258262890683122, 1.000000000000000000, 0.9659258262890683122, 1.000000000000000000, 0.9659258262890683122, 1.000000000000000000, 0.9659258262890683122, 1.000000000000000000, 0.9659258262890683122, 1.000000000000000000, 0.9659258262890683122, 1.000000000000000000),
 ( 1.000000000000000000, 0.9659258262890683122, 1.000000000000000000, 0.9659258262890683122, 1.000000000000000000, 0.9659258262890683122, 1.000000000000000000, 0.9659258262890683122, 1.000000000000000000, 0.9659258262890683122, 1.000000000000000000, 0.9659258262890683122, 1.000000000000000000, 0.9659258262890683122, 1.000000000000000000, 0.9659258262890683122, 1.000000000000000000, 0.9659258262890683122, 1.000000000000000000, 0.9659258262890683122, 1.000000000000000000, 0.9659258262890683122, 1.000000000000000000, 0.9659258262890683122, 1.000000000000000000, 0.9659258262890683122, 1.000000000000000000, 0.9659258262890683122, 1.000000000000000000, 0.9659258262890683122, 1.000000000000000000, 0.9659258262890683122, 1.000000000000000000, 0.9659258262890683122, 1.000000000000000000, 0.9659258262890683122, 1.000000000000000000, 0.9659258262890683122, 1.000000000000000000, 0.9659258262890683122, 1.000000000000000000, 0.9659258262890683122, 1.000000000000000000, 0.9659258262890683122, 1.000000000000000000, 0.9659258262890683122, 1.000000000000000000, 0.9659258262890683122, 1.000000000000000000, 0.9659258262890683122, 1.000000000000000000, 0.9659258262890683122, 1.000000000000000000, 0.9659258262890683122, 1.000000000000000000, 0.9659258262890683122, 1.000000000000000000, 0.9659258262890683122, 1.000000000000000000, 0.9659258262890683122, 1.000000000000000000, 0.9659258262890683122, 1.000000000000000000, 0.9659258262890683122, 1.000000000000000000, 0.9659258262890683122, 1.000000000000000000, 0.9659258262890683122, 1.000000000000000000, 0.9659258262890683122, 1.000000000000000000, 0.9659258262890683122, 1.000000000000000000, 0.9659258262890683122, 1.000000000000000000, 0.9659258262890683122, 1.000000000000000000, 0.9659258262890683122, 1.000000000000000000, 0.9659258262890683122, 1.000000000000000000, 0.9659258262890683122, 1.000000000000000000, 0.9659258262890683122, 1.000000000000000000, 0.9659258262890683122, 1.000000000000000000, 0.9659258262890683122, 1.000000000000000000, 0.9659258262890683122, 1.000000000000000000, 0.9659258262890683122, 1.000000000000000000, 0.9659258262890683122, 1.000000000000000000, 0.9659258262890683122, 1.000000000000000000, 0.9659258262890683122, 1.000000000000000000, 0.9659258262890683122, 1.000000000000000000, 0.9659258262890683122, 1.000000000000000000, 0.9659258262890683122, 1.000000000000000000, 0.9659258262890683122, 1.000000000000000000, 0.9659258262890683122, 1.000000000000000000, 0.9659258262890683122, 1.000000000000000000, 0.9659258262890683122, 1.000000000000000000, 0.9659258262890683122, 1.000000000000000000, 0.9659258262890683122, 1.000000000000000000, 0.9659258262890683122, 1.000000000000000000, 0.9659258262890683122, 1.000000000000000000, 0.9659258262890683122, 1.000000000000000000, 0.9659258262890683122, 1.000000000000000000, 0.9659258262890683122, 1.000000000000000000, 0.9659258262890683122, 1.000000000000000000, 0.9659258262890683122, 1.000000000000000000, 0.9659258262890683122, 1.000000000000000000, 0.9659258262890683122, 1.000000000000000000, 0.9659258262890683122, 1.000000000000000000, 0.9659258262890683122, 1.000000000000000000, 0.9659258262890683122, 1.000000000000000000, 0.9659258262890683122, 1.000000000000000000, 0.9659258262890683122, 1.000000000000000000, 0.9659258262890683122, 1.000000000000000000, 0.9659258262890683122, 1.000000000000000000, 0.9659258262890683122, 1.000000000000000000, 0.9659258262890683122, 1.000000000000000000, 0.9659258262890683122, 1.000000000000000000, 0.9659258262890683122, 1.000000000000000000, 0.9659258262890683122, 1.000000000000000000, 0.9659258262890683122, 1.000000000000000000, 0.9659258262890683122, 1.000000000000000000, 0.9659258262890683122, 1.000000000000000000, 0.9659258262890683122, 1.000000000000000000, 0.9659258262890683122, 1.000000000000000000, 0.9659258262890683122, 1.000000000000000000, 0.9659258262890683122, 1.000000000000000000, 0.9659258262890683122, 1.000000000000000000, 0.9659258262890683122, 1.000000000000000000, 0.9659258262890683122, 1.000000000000000000, 0.9659258262890683122, 1.000000000000000000, 0.9659258262890683122, 1.000000000000000000, 0.9659258262890683122, 1.000000000000000000, 0.9659258262890683122, 1.000000000000000000, 0.9659258262890683122, 1.000000000000000000, 0.9659258262890683122, 1.000000000000000000, 0.9659258262890683122, 1.000000000000000000, 0.9659258262890683122, 1.000000000000000000, 0.9659258262890683122, 1.000000000000000000, 0.9659258262890683122, 1.000000000000000000, 0.9659258262890683122, 1.000000000000000000, 0.9659258262890683122, 1.000000000000000000, 0.9659258262890683122, 1.000000000000000000, 0.9659258262890683122, 1.000000000000000000, 0.9659258262890683122, 1.000000000000000000, 0.9659258262890683122, 1.000000000000000000, 0.9659258262890683122, 1.000000000000000000, 0.9659258262890683122, 1.000000000000000000, 0.9659258262890683122, 1.000000000000000000, 0.9659258262890683122, 1.000000000000000000, 0.9659258262890683122, 1.000000000000000000, 0.9659258262890683122, 1.000000000000000000, 0.9659258262890683122, 1.000000000000000000, 0.9659258262890683122, 1.000000000000000000, 0.9659258262890683122, 1.000000000000000000, 0.9659258262890683122, 1.000000000000000000, 0.9659258262890683122, 1.000000000000000000, 0.9659258262890683122, 1.000000000000000000, 0.9659258262890683122, 1.000000000000000000, 0.9659258262890683122, 1.000000000000000000, 0.9659258262890683122, 1.000000000000000000, 0.9659258262890683122, 1.000000000000000000, 0.9659258262890683122, 1.000000000000000000, 0.9659258262890683122, 1.000000000000000000, 0.9659258262890683122, 1.000000000000000000, 0.9659258262890683122, 1.000000000000000000, 0.9659258262890683122, 1.000000000000000000, 0.9659258262890683122, 1.000000000000000000, 0.9659258262890683122, 1.000000000000000000, 0.9659258262890683122, 1.000000000000000000, 0.9659258262890683122, 1.000000000000000000, 0.9659258262890683122, 1.000000000000000000, 0.9659258262890683122, 1.000000000000000000, 0.9659258262890683122, 1.000000000000000000, 0.9659258262890683122, 1.000000000000000000, 0.9659258262890683122, 1.000000000000000000, 0.9659258262890683122, 1.000000000000000000, 0.9659258262890683122, 1.000000000000000000, 0.9659258262890683122, 1.000000000000000000, 0.9659258262890683122, 1.000000000000000000, 0.9659258262890683122, 1.000000000000000000, 0.9659258262890683122, 1.000000000000000000, 0.9659258262890683122, 1.000000000000000000, 0.9659258262890683122, 1.000000000000000000, 0.9659258262890683122, 1.000000000000000000, 0.9659258262890683122, 1.000000000000000000, 0.9659258262890683122, 1.000000000000000000, 0.9659258262890683122, 1.000000000000000000, 0.9659258262890683122, 1.000000000000000000, 0.9659258262890683122, 1.000000000000000000, 0.9659258262890683122, 1.000000000000000000, 0.9659258262890683122, 1.000000000000000000, 0.9659258262890683122, 1.000000000000000000, 0.9659258262890683122, 1.000000000000000000, 0.9659258262890683122, 1.000000000000000000, 0.9659258262890683122, 1.000000000000000000, 0.9659258262890683122, 1.000000000000000000, 0.9659258262890683122, 1.000000000000000000, 0.9659258262890683122, 1.000000000000000000, 0.9659258262890683122, 1.000000000000000000, 0.9659258262890683122, 1.000000000000000000, 0.9659258262890683122, 1.000000000000000000, 0.9659258262890683122, 1.000000000000000000) ) ) 
 REPRESENTATION_ITEM ( '' )  SURFACE ( )  );
#63379 = VERTEX_POINT ( 'NONE', #98142 ) ;
#63380 = CARTESIAN_POINT ( 'NONE',  ( 3.192513988408024694, -3.228466078459764559E-15, 14.27292421863752914 ) ) ;
#63381 = CARTESIAN_POINT ( 'NONE',  ( 17.20831665107776587, 4.133931151000785675, -7.208316651077762316 ) ) ;
#63382 = CARTESIAN_POINT ( 'NONE',  ( 0.1532563361054100626, 50.80059781766745175, -2.638427012816831230 ) ) ;
#63384 = CARTESIAN_POINT ( 'NONE',  ( 10.00000000000000178, 32.25893115100078745, 9.846743663894594434 ) ) ;
#63383 = CARTESIAN_POINT ( 'NONE',  ( 19.84674366389459266, 8.300597817667451750, 2.638427012816836559 ) ) ;
#63385 = CARTESIAN_POINT ( 'NONE',  ( -0.1042174387088615761, 28.10736173766202128, 6.337391062633417782 ) ) ;
#63386 = CARTESIAN_POINT ( 'NONE',  ( -13.75543905097459429, 0.04962897369418823451, -5.333404663735767492 ) ) ;
#63387 = CARTESIAN_POINT ( 'NONE',  ( 18.52753015748617571, 23.09226448433411960, 4.923371831947298993 ) ) ;
#63388 = CARTESIAN_POINT ( 'NONE',  ( -0.1049300847420622101, 52.21697413083879979, -6.336235997365760930 ) ) ;
#63389 = LINE ( 'NONE', #64363, #53487 ) ;
#63391 = CARTESIAN_POINT ( 'NONE',  ( -0.1503990784575247319, 22.22266099184918886, -6.262539305110083276 ) ) ;
#63390 = CARTESIAN_POINT ( 'NONE',  ( 2.791683348922240793, 21.63393115100078745, 7.208316651077764092 ) ) ;
#63392 = CARTESIAN_POINT ( 'NONE',  ( 17.99999999999999645, 99.99999999999998579, 8.000000000000000000 ) ) ;
#63394 = ORIENTED_EDGE ( 'NONE', *, *, #80326, .F. ) ;
#63393 = CARTESIAN_POINT ( 'NONE',  ( 12.63842701281683034, 52.46726448433413026, 9.846743663894596210 ) ) ;
#63395 = CARTESIAN_POINT ( 'NONE',  ( 13.40508947812165097, 15.00000000000000000, -5.527528931046084004 ) ) ;
#63396 = CARTESIAN_POINT ( 'NONE',  ( 22.81628187352647785, 26.41530133659708923, 3.434112377981063169 ) ) ;
#63397 = CARTESIAN_POINT ( 'NONE',  ( 17.20831665107776587, 49.13393115100078745, -7.208316651077762316 ) ) ;
#63398 = DIRECTION ( 'NONE',  ( 1.000000000000000000, -0.000000000000000000, -0.000000000000000000 ) ) ;
#63399 = CARTESIAN_POINT ( 'NONE',  ( -4.164238869374099039, 41.80374883491397497, 8.674139862899312516E-16 ) ) ;
#63400 = CARTESIAN_POINT ( 'NONE',  ( 1.472469842513823179, 16.42559781766745175, 4.923371831947296329 ) ) ;
#63401 = ORIENTED_EDGE ( 'NONE', *, *, #33837, .F. ) ;
#63402 = CARTESIAN_POINT ( 'NONE',  ( 0.1532563361054100626, 5.800597817667452638, -2.638427012816831230 ) ) ;
#63403 = CARTESIAN_POINT ( 'NONE',  ( 19.67370888310408716, 90.62786186788183329, 5.438836974231068488 ) ) ;
#63404 = CARTESIAN_POINT ( 'NONE',  ( 20.36894250292379738, 49.92874883491396787, -10.36894250292379027 ) ) ;
#63405 = CARTESIAN_POINT ( 'NONE',  ( 17.20831665107776587, 59.13393115100078745, -7.208316651077762316 ) ) ;
#63406 = CARTESIAN_POINT ( 'NONE',  ( 2.035157376598822676, 12.43868534415483751, -7.964842623401177768 ) ) ;
#63408 = VECTOR ( 'NONE', #22583, 1000.000000000000114 ) ;
#63407 = CARTESIAN_POINT ( 'NONE',  ( 20.36894250292379738, 24.92874883491396787, -10.36894250292379027 ) ) ;
#63409 = CARTESIAN_POINT ( 'NONE',  ( 2.917880565312948704, 42.63708216824729647, 12.26659068614894643 ) ) ;
#63410 = DIRECTION ( 'NONE',  ( 0.000000000000000000, 0.000000000000000000, -1.000000000000000000 ) ) ;
#63412 = CARTESIAN_POINT ( 'NONE',  ( 0.1532563361054083140, 51.00893115100078745, 1.131784320476157264E-15 ) ) ;
#63411 = CARTESIAN_POINT ( 'NONE',  ( 6.905507196109046397, -69.44000359832128311, 2.750000000000000000 ) ) ;
#63413 = CIRCLE ( 'NONE', #45885, 14.49999999999999822 ) ;
#63414 = ORIENTED_EDGE ( 'NONE', *, *, #98491, .F. ) ;
#63415 = CARTESIAN_POINT ( 'NONE',  ( 15.44008868035555260, 34.73035201082151247, 9.422509992056143702 ) ) ;
#63416 = CARTESIAN_POINT ( 'NONE',  ( 20.15039907845753220, 22.62777174578612716, -6.262539305110077947 ) ) ;
#63417 = EDGE_CURVE ( 'NONE', #88425, #21334, #61585, .T. ) ;
#63418 = FACE_OUTER_BOUND ( 'NONE', #24148, .T. ) ;
#63419 = CARTESIAN_POINT ( 'NONE',  ( 19.84674366389459621, 43.50893115100078745, 7.409399052514197653E-17 ) ) ;
#63421 = CARTESIAN_POINT ( 'NONE',  ( 0.6178305044545838731, 64.74863466993043914, 9.382169495545420901 ) ) ;
#63420 = AXIS2_PLACEMENT_3D ( 'NONE', #1467, #18418, #24948 ) ;
#63422 = CARTESIAN_POINT ( 'NONE',  ( 14.16423886937410259, 4.303748834913974086, -2.602085213965210642E-15 ) ) ;
#63423 = CARTESIAN_POINT ( 'NONE',  ( 2.791683348922240793, 51.63393115100078745, 7.208316651077764092 ) ) ;
#63424 = CARTESIAN_POINT ( 'NONE',  ( 10.00000000000000178, 67.25893115100079456, 9.846743663894594434 ) ) ;
#63425 = ORIENTED_EDGE ( 'NONE', *, *, #58296, .T. ) ;
#63426 = CARTESIAN_POINT ( 'NONE',  ( 22.26659068614894466, 23.88708216824730357, 7.082119434687054849 ) ) ;
#63427 = CARTESIAN_POINT ( 'NONE',  ( 19.67858290521088804, 89.00000000000000000, 5.461713021790605360 ) ) ;
#63428 = CARTESIAN_POINT ( 'NONE',  ( -10.82361996477964361, 14.95037106895822809, -10.02529603627149690 ) ) ;
#63429 = CARTESIAN_POINT ( 'NONE',  ( 20.88017736071110164, 5.355352010821503583, 2.915334737309930979 ) ) ;
#63430 = CARTESIAN_POINT ( 'NONE',  ( -1.099225684535947600, 28.70696800326375353, -6.408140936763238038 ) ) ;
#63431 = DIRECTION ( 'NONE',  ( 1.000000000000000000, 0.000000000000000000, 0.000000000000000000 ) ) ;
#63432 = CARTESIAN_POINT ( 'NONE',  ( 4.559911319644449179, 67.23035201082150536, -9.422509992056141925 ) ) ;
#63433 = CARTESIAN_POINT ( 'NONE',  ( -46.94000000000000483, 100.4746355719282320, -9.260812147861324561 ) ) ;
#63434 = DIRECTION ( 'NONE',  ( -0.000000000000000000, -1.000000000000000000, -0.000000000000000000 ) ) ;
#63435 = CARTESIAN_POINT ( 'NONE',  ( -0.8801773607111008646, 3.272018677488171434, 2.915334737309923430 ) ) ;
#63436 = CARTESIAN_POINT ( 'NONE',  ( -0.1049300847420659155, 42.21697413083878558, -6.336235997365754713 ) ) ;
#63437 = CARTESIAN_POINT ( 'NONE',  ( 20.88017736071110164, 30.35535201082151247, 2.915334737309930979 ) ) ;
#63438 = CARTESIAN_POINT ( 'NONE',  ( 2.035157376598824452, 38.68868534415483396, 7.964842623401179544 ) ) ;
#63439 = CARTESIAN_POINT ( 'NONE',  ( -2.816281873526471635, -1.084698663402913210, -3.434112377981056508 ) ) ;
#63440 = PLANE ( 'NONE',  #53902 ) ;
#63441 = CARTESIAN_POINT ( 'NONE',  ( -1.099225684535947600, 63.70696800326376774, -6.408140936763238038 ) ) ;
#63442 = CARTESIAN_POINT ( 'NONE',  ( 0.1532563361054100626, 10.80059781766745175, -2.638427012816831230 ) ) ;
#63443 = EDGE_CURVE ( 'NONE', #92229, #81201, #76900, .T. ) ;
#63444 = ORIENTED_EDGE ( 'NONE', *, *, #13330, .T. ) ;
#63445 = CARTESIAN_POINT ( 'NONE',  ( 7.084665262690076126, 32.02201867748816966, -10.88017736071110164 ) ) ;
#63446 = CARTESIAN_POINT ( 'NONE',  ( -2.816281873526471635, 28.91530133659708213, -3.434112377981056508 ) ) ;
#63447 = UNCERTAINTY_MEASURE_WITH_UNIT (LENGTH_MEASURE( 1.000000000000000082E-05 ), #16511, 'distance_accuracy_value', 'NONE');
#63448 = EDGE_CURVE ( 'NONE', #63645, #82054, #14644, .T. ) ;
#63449 = CARTESIAN_POINT ( 'NONE',  ( 19.84674366389459621, 58.50893115100078745, 7.409399052514197653E-17 ) ) ;
#63450 = B_SPLINE_CURVE_WITH_KNOTS ( 'NONE', 3,
 ( #26654, #57150, #87647, #19161, #13629, #91100 ),
 .UNSPECIFIED., .F., .F.,
 ( 4, 2, 4 ),
 ( 0.0002800020636817285172, 0.0006862073132860471540, 0.001092412562890365899 ),
 .UNSPECIFIED. ) ;
#63451 = CARTESIAN_POINT ( 'NONE',  ( 12.91533473730993009, 51.60535201082149825, -10.88017736071109987 ) ) ;
#63452 = EDGE_CURVE ( 'NONE', #12785, #62370, #75328, .T. ) ;
#63453 = CARTESIAN_POINT ( 'NONE',  ( 5.076628168052704559, 10.17559781766745175, -8.527530157486179263 ) ) ;
#63454 = VECTOR ( 'NONE', #43398, 1000.000000000000000 ) ;
#63455 = CARTESIAN_POINT ( 'NONE',  ( 22.81628187352648496, 41.83196800326375353, -3.434112377981050290 ) ) ;
#63456 = CARTESIAN_POINT ( 'NONE',  ( 10.00000000000000000, 56.81368534415484106, -10.88017736071110342 ) ) ;
#63457 = CARTESIAN_POINT ( 'NONE',  ( 17.39651004071838614, 52.93575266056826933, 6.500000000000032863 ) ) ;
#63458 = CARTESIAN_POINT ( 'NONE',  ( 16.40814093676323893, 60.79030133659709634, 11.09922568453595026 ) ) ;
#63459 = EDGE_LOOP ( 'NONE', ( #42702, #30267, #28305, #2438 ) ) ;
#63460 =( NAMED_UNIT ( * ) SI_UNIT ( $, .STERADIAN. ) SOLID_ANGLE_UNIT ( ) );
#63461 = DIRECTION ( 'NONE',  ( 1.000000000000000000, 2.569960705150826877E-16, -0.000000000000000000 ) ) ;
#63462 = CARTESIAN_POINT ( 'NONE',  ( 20.88017736071110875, 5.772018677488170546, -2.915334737309920765 ) ) ;
#63464 = CARTESIAN_POINT ( 'NONE',  ( 13.79529636645030344, 23.26208216824730002, 14.16423886937410614 ) ) ;
#63463 = CARTESIAN_POINT ( 'NONE',  ( -2.816281873526471635, 43.91530133659708923, -3.434112377981056508 ) ) ;
#63465 = CARTESIAN_POINT ( 'NONE',  ( 0.1532563361054083140, 11.00893115100078568, 1.131784320476157264E-15 ) ) ;
#63466 = CARTESIAN_POINT ( 'NONE',  ( -0.8801773607111008646, 8.272018677488171434, 2.915334737309923430 ) ) ;
#63467 = CARTESIAN_POINT ( 'NONE',  ( 7.361572987183170547, 22.05059781766745530, 9.846743663894590881 ) ) ;
#63468 = CARTESIAN_POINT ( 'NONE',  ( -0.3689425029237881626, 57.42874883491397497, 10.36894250292379027 ) ) ;
#63469 = ORIENTED_EDGE ( 'NONE', *, *, #72914, .T. ) ;
#63470 = CARTESIAN_POINT ( 'NONE',  ( 19.42250999205614548, 5.980352010821504471, -5.440088680355545492 ) ) ;
#63471 =( GEOMETRIC_REPRESENTATION_CONTEXT ( 3 ) GLOBAL_UNCERTAINTY_ASSIGNED_CONTEXT ( ( #54350 ) ) GLOBAL_UNIT_ASSIGNED_CONTEXT ( ( #21620, #83093, #53574 ) ) REPRESENTATION_CONTEXT ( 'NONE', 'WORKASPACE' ) );
#63472 = CARTESIAN_POINT ( 'NONE',  ( 19.42250999205614193, 15.14701867748817143, 5.440088680355555262 ) ) ;
#63473 = CARTESIAN_POINT ( 'NONE',  ( 1.383448333479232462, 32.37718327197428181, -6.499999999999977796 ) ) ;
#63474 = AXIS2_PLACEMENT_3D ( 'NONE', #22272, #89269, #60737 ) ;
#63475 = ORIENTED_EDGE ( 'NONE', *, *, #38200, .F. ) ;
#63476 = ORIENTED_EDGE ( 'NONE', *, *, #32507, .T. ) ;
#63477 = CARTESIAN_POINT ( 'NONE',  ( 7.084665262690076126, 14.10535201082150358, 10.88017736071109987 ) ) ;
#63478 = CARTESIAN_POINT ( 'NONE',  ( 1.472469842513823179, 55.59226448433412315, -4.923371831947296329 ) ) ;
#63479 = CARTESIAN_POINT ( 'NONE',  ( 13.78891971893204271, 0.5000000000000004441, 5.904717858191622426 ) ) ;
#63481 = CARTESIAN_POINT ( 'NONE',  ( 20.36894250292379738, 14.92874883491396432, -10.36894250292379027 ) ) ;
#63480 = CARTESIAN_POINT ( 'NONE',  ( 0.000000000000000000, 81.99999999999992895, 5.000000000000000000 ) ) ;
#63482 = CARTESIAN_POINT ( 'NONE',  ( 4.559911319644449179, 33.89701867748817676, 9.422509992056141925 ) ) ;
#63483 = CARTESIAN_POINT ( 'NONE',  ( 19.42250999205614548, 20.98035201082150891, -5.440088680355545492 ) ) ;
#63484 = CARTESIAN_POINT ( 'NONE',  ( 18.52753015748618282, 58.92559781766745886, -4.923371831947291888 ) ) ;
#63485 = CARTESIAN_POINT ( 'NONE',  ( -10.07524202709548611, -32.17782673090250256, -3.750000000000000444 ) ) ;
#63486 = CARTESIAN_POINT ( 'NONE',  ( 17.20831665107776587, 34.13393115100078745, -7.208316651077762316 ) ) ;
#63487 = EDGE_CURVE ( 'NONE', #96588, #30635, #82944, .T. ) ;
#63488 = CARTESIAN_POINT ( 'NONE',  ( 0.1532563361054100626, 10.80059781766745175, -2.638427012816831230 ) ) ;
#63489 = CARTESIAN_POINT ( 'NONE',  ( -7.208316651077756099, 26.63393115100079811, 7.208316651077766757 ) ) ;
#63490 = ORIENTED_EDGE ( 'NONE', *, *, #36022, .T. ) ;
#63491 = CARTESIAN_POINT ( 'NONE',  ( 19.42250999205614548, 5.980352010821504471, -5.440088680355545492 ) ) ;
#63492 = CARTESIAN_POINT ( 'NONE',  ( 12.63842701281683922, 9.550597817667449974, -9.846743663894590881 ) ) ;
#63494 = CARTESIAN_POINT ( 'NONE',  ( 1.472469842513823179, 65.59226448433412315, -4.923371831947296329 ) ) ;
#63493 = AXIS2_PLACEMENT_3D ( 'NONE', #62304, #83352, #52844 ) ;
#63495 = CARTESIAN_POINT ( 'NONE',  ( -0.8801773607111009756, 48.06368534415484817, 1.068504757029289695E-15 ) ) ;
#63497 = CARTESIAN_POINT ( 'NONE',  ( 0.6178305044545838731, 39.74863466993041072, 9.382169495545420901 ) ) ;
#63496 = CARTESIAN_POINT ( 'NONE',  ( 2.035157376598824452, 8.688685344154839285, 7.964842623401179544 ) ) ;
#63498 = CARTESIAN_POINT ( 'NONE',  ( -2.266590686148945544, 26.38708216824730357, -7.082119434687050408 ) ) ;
#63499 = AXIS2_PLACEMENT_3D ( 'NONE', #92204, #69700, #75719 ) ;
#63500 = CARTESIAN_POINT ( 'NONE',  ( 0.000000000000000000, 0.5000000000000004441, 0.000000000000000000 ) ) ;
#63501 = VECTOR ( 'NONE', #1523, 1000.000000000000114 ) ;
#63502 = CARTESIAN_POINT ( 'NONE',  ( 6.565887622018943937, 55.16530133659709634, 12.81628187352647430 ) ) ;
#63503 = ORIENTED_EDGE ( 'NONE', *, *, #93485, .F. ) ;
#63504 = CARTESIAN_POINT ( 'NONE',  ( 14.92337183194729633, 62.67559781766745886, 8.527530157486181039 ) ) ;
#63505 = CARTESIAN_POINT ( 'NONE',  ( 20.88017736071110164, 25.35535201082150891, 2.915334737309930979 ) ) ;
#63506 = ORIENTED_EDGE ( 'NONE', *, *, #27201, .T. ) ;
#63507 = CARTESIAN_POINT ( 'NONE',  ( -0.8801773607111009756, 68.06368534415484817, 1.068504757029289695E-15 ) ) ;
#63508 = CARTESIAN_POINT ( 'NONE',  ( 7.361572987183169658, 14.96726448433411960, -9.846743663894592657 ) ) ;
#63509 = CARTESIAN_POINT ( 'NONE',  ( 19.84674366389459621, 3.508931151000785231, 7.409399052514197653E-17 ) ) ;
#63511 = FACE_OUTER_BOUND ( 'NONE', #41446, .T. ) ;
#63510 = CARTESIAN_POINT ( 'NONE',  ( 19.42250999205614548, 50.98035201082151247, -5.440088680355545492 ) ) ;
#63512 = CARTESIAN_POINT ( 'NONE',  ( 4.559911319644449179, 58.89701867748817676, 9.422509992056141925 ) ) ;
#63514 = ORIENTED_EDGE ( 'NONE', *, *, #9622, .T. ) ;
#63513 = CARTESIAN_POINT ( 'NONE',  ( 0.1532563361054100626, 0.8005978176674514168, -2.638427012816831230 ) ) ;
#63515 = CARTESIAN_POINT ( 'NONE',  ( 12.60589901313228189, 14.49999999999999112, -8.129656208642064286 ) ) ;
#63516 = CARTESIAN_POINT ( 'NONE',  ( 5.076628168052704559, 55.17559781766745175, -8.527530157486179263 ) ) ;
#63517 = ORIENTED_EDGE ( 'NONE', *, *, #82866, .T. ) ;
#63518 = ORIENTED_EDGE ( 'NONE', *, *, #5361, .T. ) ;
#63519 = CARTESIAN_POINT ( 'NONE',  ( 4.219999999999999751, 10.00000000000000000, -2.750000000000000000 ) ) ;
#63520 = CARTESIAN_POINT ( 'NONE',  ( -2.266590686148945544, 6.387082168247300906, -7.082119434687050408 ) ) ;
#63521 = CARTESIAN_POINT ( 'NONE',  ( 10.00000000000000178, 55.37363466993042493, 12.81628187352647608 ) ) ;
#63522 = CARTESIAN_POINT ( 'NONE',  ( 17.08211943468705130, 3.470415501580634388, 12.26659068614894998 ) ) ;
#63523 = CARTESIAN_POINT ( 'NONE',  ( 24.16423886937410614, 29.51208216824729647, -3.795296366450302550 ) ) ;
#63524 = CARTESIAN_POINT ( 'NONE',  ( -14.24131928502211863, -0.03417435944610275333, 0.4973178280104966764 ) ) ;
#63525 = CARTESIAN_POINT ( 'NONE',  ( 2.035157376598824452, 23.68868534415484461, 7.964842623401179544 ) ) ;
#63526 = DIRECTION ( 'NONE',  ( 1.000000000000000000, -0.000000000000000000, -0.000000000000000000 ) ) ;
#63527 = VERTEX_POINT ( 'NONE', #52614 ) ;
#63528 = CARTESIAN_POINT ( 'NONE',  ( 1.472469842513823179, 11.42559781766745175, 4.923371831947296329 ) ) ;
#63529 = CARTESIAN_POINT ( 'NONE',  ( 21.09922568453595559, 37.04030133659708923, -6.408140936763230044 ) ) ;
#63530 = CARTESIAN_POINT ( 'NONE',  ( 2.791683348922237240, 35.38393115100079456, -7.208316651077763204 ) ) ;
#63531 = EDGE_CURVE ( 'NONE', #55250, #55876, #83114, .T. ) ;
#63532 = CARTESIAN_POINT ( 'NONE',  ( -2.816281873526473856, 34.12363466993042493, 9.499525473075851096E-16 ) ) ;
#63533 = DIRECTION ( 'NONE',  ( 1.000000000000000000, 0.000000000000000000, 0.000000000000000000 ) ) ;
#63534 =( GEOMETRIC_REPRESENTATION_CONTEXT ( 3 ) GLOBAL_UNCERTAINTY_ASSIGNED_CONTEXT ( ( #85222 ) ) GLOBAL_UNIT_ASSIGNED_CONTEXT ( ( #75035, #60027, #91016 ) ) REPRESENTATION_CONTEXT ( 'NONE', 'WORKASPACE' ) );
#63535 = CARTESIAN_POINT ( 'NONE',  ( 10.00000000000000178, 22.25893115100078745, 9.846743663894594434 ) ) ;
#63536 = CARTESIAN_POINT ( 'NONE',  ( -2.266590686148945544, 16.38708216824730357, -7.082119434687050408 ) ) ;
#63537 = CARTESIAN_POINT ( 'NONE',  ( 7.084665262690076126, 34.10535201082151247, 10.88017736071109987 ) ) ;
#63538 = CARTESIAN_POINT ( 'NONE',  ( 24.16423886937409904, 34.09541550158064638, 3.795296366450317205 ) ) ;
#63539 = CARTESIAN_POINT ( 'NONE',  ( 17.20831665107776587, 57.88393115100078745, 7.208316651077764980 ) ) ;
#63540 = CARTESIAN_POINT ( 'NONE',  ( 18.52753015748618282, 13.92559781766745175, -4.923371831947291888 ) ) ;
#63542 = CARTESIAN_POINT ( 'NONE',  ( 9.065164099344530158, 0.5000000000000004441, -11.95084933600767307 ) ) ;
#63541 = CARTESIAN_POINT ( 'NONE',  ( 10.00000000000000178, 55.37363466993042493, 12.81628187352647608 ) ) ;
#63543 = CARTESIAN_POINT ( 'NONE',  ( 2.035157376598824452, 23.68868534415484461, 7.964842623401179544 ) ) ;
#63544 = DIRECTION ( 'NONE',  ( 1.000000000000000000, -0.000000000000000000, -0.000000000000000000 ) ) ;
#63545 = AXIS2_PLACEMENT_3D ( 'NONE', #73096, #88596, #29082 ) ;
#63546 = CARTESIAN_POINT ( 'NONE',  ( 16.40814093676324603, 17.45696800326375353, -11.09922568453594671 ) ) ;
#63547 = CARTESIAN_POINT ( 'NONE',  ( 5.076628168052704559, 40.17559781766745175, -8.527530157486179263 ) ) ;
#63548 = CARTESIAN_POINT ( 'NONE',  ( -5.204170427930421283E-15, 6.813685344154843726, -10.88017736071110342 ) ) ;
#63549 = CARTESIAN_POINT ( 'NONE',  ( 19.72487221294570858, 12.80223176428831167, -6.500000000000000888 ) ) ;
#63551 = CARTESIAN_POINT ( 'NONE',  ( 13.99999999999999822, 61.00000000000000711, -5.000000000000000000 ) ) ;
#63550 = CARTESIAN_POINT ( 'NONE',  ( 20.88017736071110164, 65.35535201082150536, 2.915334737309930979 ) ) ;
#63552 = VECTOR ( 'NONE', #67779, 1000.000000000000000 ) ;
#63553 = DIRECTION ( 'NONE',  ( -0.000000000000000000, -1.000000000000000000, -0.000000000000000000 ) ) ;
#63554 = AXIS2_PLACEMENT_3D ( 'NONE', #10241, #92743, #54732 ) ;
#63555 = CARTESIAN_POINT ( 'NONE',  ( 17.96484262340118221, 49.93868534415484106, 7.964842623401181321 ) ) ;
#63556 = CARTESIAN_POINT ( 'NONE',  ( 19.42250999205614193, 55.14701867748817676, 5.440088680355555262 ) ) ;
#63557 = DIRECTION ( 'NONE',  ( -0.000000000000000000, 1.000000000000000000, -0.000000000000000000 ) ) ;
#63558 = ADVANCED_FACE ( 'NONE', ( #45106 ), #30593, .F. ) ;
#63559 = FILL_AREA_STYLE_COLOUR ( '', #47650 ) ;
#63560 = CARTESIAN_POINT ( 'NONE',  ( -0.8801773607110991993, 7.855352010821506248, -2.915334737309923874 ) ) ;
#63561 = EDGE_CURVE ( 'NONE', #72221, #13031, #76597, .T. ) ;
#63562 = CARTESIAN_POINT ( 'NONE',  ( 16.40814093676323893, 0.7903013365970867898, 11.09922568453595026 ) ) ;
#63564 = CARTESIAN_POINT ( 'NONE',  ( -3.499999999999998668, 1.019547802438465434, -3.750000000000000000 ) ) ;
#63563 = CARTESIAN_POINT ( 'NONE',  ( -0.8801773607110991993, 27.85535201082150181, -2.915334737309923874 ) ) ;
#63565 = FACE_OUTER_BOUND ( 'NONE', #86063, .T. ) ;
#63566 = CARTESIAN_POINT ( 'NONE',  ( 6.565887622018943937, 20.16530133659708213, 12.81628187352647430 ) ) ;
#63567 = ORIENTED_EDGE ( 'NONE', *, *, #8602, .T. ) ;
#63568 = CARTESIAN_POINT ( 'NONE',  ( 2.035157376598824452, 53.68868534415484817, 7.964842623401179544 ) ) ;
#63569 = CARTESIAN_POINT ( 'NONE',  ( 0.1532563361054083140, 41.00893115100078745, 1.131784320476157264E-15 ) ) ;
#63571 = CARTESIAN_POINT ( 'NONE',  ( -2.283843307429720415, 13.12729635533385597, 10.00000000000000000 ) ) ;
#63570 = CARTESIAN_POINT ( 'NONE',  ( 19.38216949554541202, 0.9986346699304200492, 9.382169495545424454 ) ) ;
#63572 = CARTESIAN_POINT ( 'NONE',  ( 10.00000000000000000, 31.81368534415483751, -10.88017736071110342 ) ) ;
#63573 = CARTESIAN_POINT ( 'NONE',  ( 20.88017736071110164, 40.35535201082150536, 2.915334737309930979 ) ) ;
#63574 = CARTESIAN_POINT ( 'NONE',  ( 20.36894250292379738, 49.92874883491396787, -10.36894250292379027 ) ) ;
#63575 = CARTESIAN_POINT ( 'NONE',  ( 12.63842701281683922, 34.55059781766745886, -9.846743663894590881 ) ) ;
#63576 = CARTESIAN_POINT ( 'NONE',  ( 0.5774900079438590739, 57.64701867748817676, -5.440088680355550821 ) ) ;
#63577 = DIRECTION ( 'NONE',  ( -0.000000000000000000, -1.000000000000000000, -0.000000000000000000 ) ) ;
#63578 = CARTESIAN_POINT ( 'NONE',  ( 22.26659068614894466, 18.88708216824730002, 7.082119434687054849 ) ) ;
#63579 = CARTESIAN_POINT ( 'NONE',  ( -9.240973841163681257, 4.382479893023984083E-16, 11.17382667070366331 ) ) ;
#63580 = FACE_OUTER_BOUND ( 'NONE', #21624, .T. ) ;
#63581 = ORIENTED_EDGE ( 'NONE', *, *, #53955, .T. ) ;
#63582 = CARTESIAN_POINT ( 'NONE',  ( 13.79529636645031943, 45.34541550158062506, -14.16423886937409904 ) ) ;
#63583 = CARTESIAN_POINT ( 'NONE',  ( 10.00000000000000178, 43.05374883491397497, 14.16423886937410082 ) ) ;
#63584 = CARTESIAN_POINT ( 'NONE',  ( 19.84674366389459621, 18.50893115100078745, 7.409399052514197653E-17 ) ) ;
#63585 = CARTESIAN_POINT ( 'NONE',  ( 22.81628187352647785, 21.62363466993041783, 6.195893100308588602E-16 ) ) ;
#63586 = CARTESIAN_POINT ( 'NONE',  ( -14.82269085861176983, 14.49999999999999112, 2.299529454046846499 ) ) ;
#63587 = FACE_OUTER_BOUND ( 'NONE', #50091, .T. ) ;
#63589 = CARTESIAN_POINT ( 'NONE',  ( -2.816281873526473856, 29.12363466993041783, 9.499525473075851096E-16 ) ) ;
#63588 = CARTESIAN_POINT ( 'NONE',  ( 4.559911319644449179, 62.23035201082150536, -9.422509992056141925 ) ) ;
#63590 = EDGE_CURVE ( 'NONE', #49705, #1795, #86488, .T. ) ;
#63591 = CARTESIAN_POINT ( 'NONE',  ( 2.917880565312948704, 42.63708216824729647, 12.26659068614894643 ) ) ;
#63592 = ADVANCED_FACE ( 'NONE', ( #10568 ), #56075, .T. ) ;
#63593 = CARTESIAN_POINT ( 'NONE',  ( 20.15039907845753930, 0.07447313448805115144, -6.262539305110068177 ) ) ;
#63594 = CARTESIAN_POINT ( 'NONE',  ( 20.88017736071110519, 65.56368534415483396, 2.639326808657452039E-16 ) ) ;
#63595 = CARTESIAN_POINT ( 'NONE',  ( 8.527530157486175710, -16.07440218233254470, -4.923371831947298993 ) ) ;
#63596 = VERTEX_POINT ( 'NONE', #85089 ) ;
#63597 = SURFACE_STYLE_FILL_AREA ( #80583 ) ;
#63598 = CARTESIAN_POINT ( 'NONE',  ( 20.15039907845753930, 70.00000000000000000, -6.262539305110068177 ) ) ;
#63599 = ORIENTED_EDGE ( 'NONE', *, *, #6932, .F. ) ;
#63600 = CARTESIAN_POINT ( 'NONE',  ( -2.266590686148945544, 2.220415501580634388, 7.082119434687048631 ) ) ;
#63602 = CARTESIAN_POINT ( 'NONE',  ( 0.5774900079438590739, 7.647018677488171434, -5.440088680355550821 ) ) ;
#63601 = CARTESIAN_POINT ( 'NONE',  ( 17.96484262340118221, 6.188685344154837509, -7.964842623401177768 ) ) ;
#63604 = CARTESIAN_POINT ( 'NONE',  ( 22.81628187352648496, 1.831968003263753753, -3.434112377981050290 ) ) ;
#63603 = CARTESIAN_POINT ( 'NONE',  ( 17.20831665107776587, 37.88393115100078745, 7.208316651077764980 ) ) ;
#63605 = PLANE ( 'NONE',  #96596 ) ;
#63606 = CARTESIAN_POINT ( 'NONE',  ( 4.219999999999999751, 10.25000000000000000, 4.000000000000000000 ) ) ;
#63607 = CARTESIAN_POINT ( 'NONE',  ( -2.816281873526471635, 18.91530133659708213, -3.434112377981056508 ) ) ;
#63608 = ORIENTED_EDGE ( 'NONE', *, *, #52821, .T. ) ;
#63609 = CARTESIAN_POINT ( 'NONE',  ( -4.164238869374098151, 51.59541550158063217, -3.795296366450310543 ) ) ;
#63610 = EDGE_LOOP ( 'NONE', ( #8450, #34594, #96762 ) ) ;
#63611 = CARTESIAN_POINT ( 'NONE',  ( 24.16423886937410614, 59.30374883491397497, 8.672049930838204340E-16 ) ) ;
#63612 = VERTEX_POINT ( 'NONE', #41577 ) ;
#63613 = CARTESIAN_POINT ( 'NONE',  ( -0.8801773607110991993, 32.85535201082151247, -2.915334737309923874 ) ) ;
#63614 = CARTESIAN_POINT ( 'NONE',  ( 15.44008868035555793, 36.39701867748816966, -9.422509992056140149 ) ) ;
#63615 = CARTESIAN_POINT ( 'NONE',  ( 2.035157376598824452, 33.68868534415484106, 7.964842623401179544 ) ) ;
#63616 = CARTESIAN_POINT ( 'NONE',  ( 12.91533473730992121, 64.52201867748817676, 10.88017736071110164 ) ) ;
#63617 = CARTESIAN_POINT ( 'NONE',  ( 4.559911319644449179, 27.23035201082150536, -9.422509992056141925 ) ) ;
#63618 = AXIS2_PLACEMENT_3D ( 'NONE', #5796, #57792, #80802 ) ;
#63619 = AXIS2_PLACEMENT_3D ( 'NONE', #48592, #4593, #4100 ) ;
#63620 = DIRECTION ( 'NONE',  ( 0.4924235601034769316, 0.000000000000000000, -0.8703556959398941473 ) ) ;
#63621 = CARTESIAN_POINT ( 'NONE',  ( 10.00000000000000178, 17.25893115100078745, 9.846743663894594434 ) ) ;
#63622 = CARTESIAN_POINT ( 'NONE',  ( 0.000000000000000000, 14.49999999999999822, 0.000000000000000000 ) ) ;
#63623 = ORIENTED_EDGE ( 'NONE', *, *, #22411, .F. ) ;
#63624 = CARTESIAN_POINT ( 'NONE',  ( 11.10658183845692015, -52.67641232763506309, 4.000000000000000888 ) ) ;
#63625 = CARTESIAN_POINT ( 'NONE',  ( 18.52753015748618282, 48.92559781766745886, -4.923371831947291888 ) ) ;
#63626 = DIRECTION ( 'NONE',  ( -0.000000000000000000, -1.000000000000000000, -0.000000000000000000 ) ) ;
#63627 = CARTESIAN_POINT ( 'NONE',  ( -1.099225684535947600, 44.54030133659708923, 6.408140936763237150 ) ) ;
#63628 = CARTESIAN_POINT ( 'NONE',  ( 1.350000000000004086, 98.50000000000000000, -8.000000000000000000 ) ) ;
#63629 = DIRECTION ( 'NONE',  ( -1.000000000000000000, 0.000000000000000000, 0.000000000000000000 ) ) ;
#63630 = CARTESIAN_POINT ( 'NONE',  ( 8.209432707284774366, 0.5000000000000004441, 12.55409154915492032 ) ) ;
#63631 = CARTESIAN_POINT ( 'NONE',  ( 10.00000000000000178, 67.25893115100079456, 9.846743663894594434 ) ) ;
#63632 = CARTESIAN_POINT ( 'NONE',  ( 20.36894250292379738, 44.92874883491396787, -10.36894250292379027 ) ) ;
#63633 = CARTESIAN_POINT ( 'NONE',  ( 12.03768810259479594, 15.00000000000000533, 8.306778944023417210 ) ) ;
#63634 = VERTEX_POINT ( 'NONE', #25583 ) ;
#63635 = CARTESIAN_POINT ( 'NONE',  ( 14.26328062697241705, 14.95037112300443560, 3.770429249334884325 ) ) ;
#63636 = CARTESIAN_POINT ( 'NONE',  ( 1.472469842513823179, 16.42559781766745175, 4.923371831947296329 ) ) ;
#63637 = SURFACE_SIDE_STYLE ('',( #58099 ) ) ;
#63638 = CARTESIAN_POINT ( 'NONE',  ( 0.1532563361054082862, 66.21726448433413736, 2.638427012816831674 ) ) ;
#63639 = CARTESIAN_POINT ( 'NONE',  ( 17.20831665107776587, 2.883931151000785231, 7.208316651077764980 ) ) ;
#63640 = EDGE_CURVE ( 'NONE', #46092, #54024, #36365, .T. ) ;
#63641 = CARTESIAN_POINT ( 'NONE',  ( 32.06412365047463453, 22.49999999999998934, -9.500000000000000000 ) ) ;
#63642 = CARTESIAN_POINT ( 'NONE',  ( 1.472469842513823179, 60.59226448433412315, -4.923371831947296329 ) ) ;
#63643 =( BOUNDED_SURFACE ( )  B_SPLINE_SURFACE ( 3, 2, ( 
 ( #47304, #94662, #46820 ),
 ( #45852, #76342, #68851 ),
 ( #77804, #9319, #92813 ),
 ( #26171, #24343, #56662 ),
 ( #15853, #3183, #30832 ),
 ( #37869, #7859, #384 ),
 ( #87151, #45346, #62305 ),
 ( #69336, #46338, #38846 ),
 ( #33649, #64145, #75850 ),
 ( #8340, #60839, #31809 ),
 ( #23359, #7370, #53842 ),
 ( #91338, #16337, #54316 ),
 ( #84353, #84830, #8825 ),
 ( #68365, #39340, #98882 ),
 ( #22865, #41193, #1358 ),
 ( #71673, #53336, #66124 ),
 ( #43133, #42650, #73126 ),
 ( #28132, #4668, #27637 ),
 ( #49162, #50643, #3678 ),
 ( #73625, #58632, #89131 ),
 ( #65629, #5148, #34140 ),
 ( #34634, #95654, #58122 ),
 ( #20642, #97160, #42171 ),
 ( #36123, #51131, #43627 ),
 ( #81621, #19159, #41681 ),
 ( #12634, #57642, #59115 ),
 ( #88630, #35638, #80146 ),
 ( #50142, #72634, #13130 ) ),
 .UNSPECIFIED., .F., .F., .F. ) 
 B_SPLINE_SURFACE_WITH_KNOTS ( ( 4, 2, 2, 2, 2, 2, 2, 2, 2, 2, 2, 2, 2, 4 ),
 ( 3, 3 ),
 ( 0.000000000000000000, 0.003117204018079801700, 0.006234408036159603400, 0.01246881607231920680, 0.02493763214463841360, 0.03740644821695762040, 0.04987526428927682720, 0.06234408036159603400, 0.07481289643391524080, 0.08728171250623445454, 0.09351612054239405447, 0.09663332456047385444, 0.09819192656951375442, 0.09975052857855365440 ),
 ( 0.000000000000000000, 1.000000000000000000 ),
 .UNSPECIFIED. ) 
 GEOMETRIC_REPRESENTATION_ITEM ( )  RATIONAL_B_SPLINE_SURFACE ( (
 ( 1.000000000000000000, 0.7071067811865475727, 1.000000000000000000),
 ( 1.000000000000000000, 0.7071067811865475727, 1.000000000000000000),
 ( 1.000000000000000000, 0.7071067811865475727, 1.000000000000000000),
 ( 1.000000000000000000, 0.7071067811865475727, 1.000000000000000000),
 ( 1.000000000000000000, 0.7071067811865475727, 1.000000000000000000),
 ( 1.000000000000000000, 0.7071067811865475727, 1.000000000000000000),
 ( 1.000000000000000000, 0.7071067811865475727, 1.000000000000000000),
 ( 1.000000000000000000, 0.7071067811865475727, 1.000000000000000000),
 ( 1.000000000000000000, 0.7071067811865471286, 1.000000000000000000),
 ( 1.000000000000000000, 0.7071067811865471286, 1.000000000000000000),
 ( 1.000000000000000000, 0.7071067811865475727, 1.000000000000000000),
 ( 1.000000000000000000, 0.7071067811865475727, 1.000000000000000000),
 ( 1.000000000000000000, 0.7071067811865482389, 1.000000000000000000),
 ( 1.000000000000000000, 0.7071067811865482389, 1.000000000000000000),
 ( 1.000000000000000000, 0.7071067811865473507, 1.000000000000000000),
 ( 1.000000000000000000, 0.7071067811865473507, 1.000000000000000000),
 ( 1.000000000000000000, 0.7071067811865475727, 1.000000000000000000),
 ( 1.000000000000000000, 0.7071067811865475727, 1.000000000000000000),
 ( 1.000000000000000000, 0.7071067811865475727, 1.000000000000000000),
 ( 1.000000000000000000, 0.7071067811865475727, 1.000000000000000000),
 ( 1.000000000000000000, 0.7071067811865475727, 1.000000000000000000),
 ( 1.000000000000000000, 0.7071067811865475727, 1.000000000000000000),
 ( 1.000000000000000000, 0.7071067811865475727, 1.000000000000000000),
 ( 1.000000000000000000, 0.7071067811865475727, 1.000000000000000000),
 ( 1.000000000000000000, 0.7071067811865520136, 1.000000000000000000),
 ( 1.000000000000000000, 0.7071067811865520136, 1.000000000000000000),
 ( 1.000000000000000000, 0.7071067811865445751, 1.000000000000000000),
 ( 1.000000000000000000, 0.7071067811865445751, 1.000000000000000000) ) ) 
 REPRESENTATION_ITEM ( '' )  SURFACE ( )  );
#63644 = CARTESIAN_POINT ( 'NONE',  ( 18.72515096720568550, 20.05509018479935790, 6.500000000000015099 ) ) ;
#63645 = VERTEX_POINT ( 'NONE', #56557 ) ;
#63646 = CARTESIAN_POINT ( 'NONE',  ( -4.164238869374098151, 61.59541550158063217, -3.795296366450310543 ) ) ;
#63647 = CARTESIAN_POINT ( 'NONE',  ( -27.43587634952537968, 22.49999999999998934, 9.500000000000000000 ) ) ;
#63648 = CARTESIAN_POINT ( 'NONE',  ( 10.00000000000000178, 44.31368534415484106, 10.88017736071110342 ) ) ;
#63650 = DIRECTION ( 'NONE',  ( 0.000000000000000000, 0.000000000000000000, -1.000000000000000000 ) ) ;
#63649 = CARTESIAN_POINT ( 'NONE',  ( 22.81628187352648496, 11.83196800326375531, -3.434112377981050290 ) ) ;
#63651 = CARTESIAN_POINT ( 'NONE',  ( -8.470640952597646489, -3.255147616298275020E-15, 11.92295067084760696 ) ) ;
#63652 = CARTESIAN_POINT ( 'NONE',  ( 6.879999999999995453, 43.00000000000000000, -6.500000000000000888 ) ) ;
#63653 = CARTESIAN_POINT ( 'NONE',  ( 0.1916775849787265285, 62.25868815902069286, -6.499999999999991118 ) ) ;
#63654 = AXIS2_PLACEMENT_3D ( 'NONE', #59132, #52139, #98666 ) ;
#63655 = CARTESIAN_POINT ( 'NONE',  ( 0.1532563361054100626, 55.80059781766745175, -2.638427012816831230 ) ) ;
#63656 = SURFACE_SIDE_STYLE ('',( #56182 ) ) ;
#63657 = CARTESIAN_POINT ( 'NONE',  ( -5.204170427930421283E-15, -38.18631465584515183, -10.88017736071110342 ) ) ;
#63658 = CARTESIAN_POINT ( 'NONE',  ( 6.565887622018943937, 13.08196800326374998, -12.81628187352647608 ) ) ;
#63660 =( NAMED_UNIT ( * ) PLANE_ANGLE_UNIT ( ) SI_UNIT ( $, .RADIAN. ) );
#63659 = CARTESIAN_POINT ( 'NONE',  ( 15.44008868035555260, 9.730352010821505360, 9.422509992056143702 ) ) ;
#63661 = FACE_OUTER_BOUND ( 'NONE', #54484, .T. ) ;
#63662 = CARTESIAN_POINT ( 'NONE',  ( -4.164238869374099927, 37.01208216824731068, 3.795296366450308767 ) ) ;
#63663 = CARTESIAN_POINT ( 'NONE',  ( 22.26659068614895176, 24.72041550158063572, -7.082119434687042414 ) ) ;
#63664 = CARTESIAN_POINT ( 'NONE',  ( 2.035157376598824452, 3.688685344154837953, 7.964842623401179544 ) ) ;
#63665 = CARTESIAN_POINT ( 'NONE',  ( 14.92337183194729633, 37.67559781766745175, 8.527530157486181039 ) ) ;
#63666 = CARTESIAN_POINT ( 'NONE',  ( 10.00000000000000178, 35.37363466993042493, 12.81628187352647608 ) ) ;
#63667 = CARTESIAN_POINT ( 'NONE',  ( 2.035157376598822676, 12.43868534415483751, -7.964842623401177768 ) ) ;
#63668 = EDGE_LOOP ( 'NONE', ( #37311, #34434, #94830, #67543 ) ) ;
#63669 = CARTESIAN_POINT ( 'NONE',  ( 12.63842701281683034, 32.46726448433412315, 9.846743663894596210 ) ) ;
#63670 = EDGE_CURVE ( 'NONE', #63050, #18880, #54252, .T. ) ;
#63671 = CARTESIAN_POINT ( 'NONE',  ( 0.5774900079438590739, 37.64701867748817676, -5.440088680355550821 ) ) ;
#63672 = CARTESIAN_POINT ( 'NONE',  ( 16.40814093676324603, 2.456968003263753531, -11.09922568453594671 ) ) ;
#63674 = CARTESIAN_POINT ( 'NONE',  ( -0.1503990784575359729, 18.10158574516642460, 6.262539305110062848 ) ) ;
#63673 = CARTESIAN_POINT ( 'NONE',  ( 20.36894250292379382, 18.67874883491397142, 10.36894250292379205 ) ) ;
#63675 = CARTESIAN_POINT ( 'NONE',  ( 1.274849032794292736, 37.55509018479936145, -6.499999999999977796 ) ) ;
#63676 = CARTESIAN_POINT ( 'NONE',  ( 14.92337183194729988, 24.34226448433411960, -8.527530157486177487 ) ) ;
#63677 = CARTESIAN_POINT ( 'NONE',  ( 10.00000000000000178, 55.37363466993042493, 12.81628187352647608 ) ) ;
#63678 = CARTESIAN_POINT ( 'NONE',  ( 19.84674366389459621, 48.50893115100078745, 7.409399052514197653E-17 ) ) ;
#63679 = EDGE_LOOP ( 'NONE', ( #93356, #97468, #24911, #87080 ) ) ;
#63680 = PLANE ( 'NONE',  #39781 ) ;
#63681 = SURFACE_SIDE_STYLE ('',( #57659 ) ) ;
#63682 = CARTESIAN_POINT ( 'NONE',  ( 24.16423886937410614, 64.30374883491396076, 8.672049930838204340E-16 ) ) ;
#63683 = CARTESIAN_POINT ( 'NONE',  ( 20.88017736071110875, 60.77201867748817676, -2.915334737309920765 ) ) ;
#63684 = CARTESIAN_POINT ( 'NONE',  ( 10.00000000000000000, 10.55374883491396787, -14.16423886937410082 ) ) ;
#63685 = CARTESIAN_POINT ( 'NONE',  ( 10.00000000000000178, 2.258931151000784787, 9.846743663894594434 ) ) ;
#63686 = CARTESIAN_POINT ( 'NONE',  ( 0.1532563361054082862, 46.21726448433411605, 2.638427012816831674 ) ) ;
#63687 = CARTESIAN_POINT ( 'NONE',  ( 4.559911319644449179, 13.89701867748817143, 9.422509992056141925 ) ) ;
#63688 = PLANE ( 'NONE',  #38384 ) ;
#63689 = CARTESIAN_POINT ( 'NONE',  ( 7.361572987183170547, 67.05059781766746596, 9.846743663894590881 ) ) ;
#63690 = CIRCLE ( 'NONE', #60494, 0.2500000000000002220 ) ;
#63691 =( NAMED_UNIT ( * ) PLANE_ANGLE_UNIT ( ) SI_UNIT ( $, .RADIAN. ) );
#63692 = CIRCLE ( 'NONE', #78055, 0.2000000000000000944 ) ;
#63693 = CARTESIAN_POINT ( 'NONE',  ( 8.209432707284781472, 14.63595249122790598, 12.55409154915492387 ) ) ;
#63694 = ORIENTED_EDGE ( 'NONE', *, *, #45398, .F. ) ;
#63695 = ORIENTED_EDGE ( 'NONE', *, *, #59750, .F. ) ;
#63696 = FACE_OUTER_BOUND ( 'NONE', #47849, .T. ) ;
#63697 = CARTESIAN_POINT ( 'NONE',  ( 10.00000000000000000, 5.553748834913967869, -14.16423886937410082 ) ) ;
#63698 = CARTESIAN_POINT ( 'NONE',  ( -2.266590686148945544, 1.387082168247301128, -7.082119434687050408 ) ) ;
#63699 = CARTESIAN_POINT ( 'NONE',  ( -2.266590686148945544, 42.22041550158063217, 7.082119434687048631 ) ) ;
#63700 = CARTESIAN_POINT ( 'NONE',  ( 18.52753015748617571, 58.09226448433411605, 4.923371831947298993 ) ) ;
#63701 = CARTESIAN_POINT ( 'NONE',  ( 0.1532563361054100626, 20.80059781766744464, -2.638427012816831230 ) ) ;
#63702 =( LENGTH_UNIT ( ) NAMED_UNIT ( * ) SI_UNIT ( .MILLI., .METRE. ) );
#63704 = CARTESIAN_POINT ( 'NONE',  ( 5.076628168052704559, 60.17559781766745175, -8.527530157486179263 ) ) ;
#63703 = CARTESIAN_POINT ( 'NONE',  ( 20.88017736071110875, 20.77201867748816611, -2.915334737309920765 ) ) ;
#63705 = CARTESIAN_POINT ( 'NONE',  ( 10.97324858046202323, 2.151463686025922861E-16, -9.670892530813203436 ) ) ;
#63706 = CARTESIAN_POINT ( 'NONE',  ( -2.266590686148945544, 37.22041550158063217, 7.082119434687048631 ) ) ;
#63707 = CARTESIAN_POINT ( 'NONE',  ( -0.8801773607110991993, 2.855352010821504471, -2.915334737309923874 ) ) ;
#63708 = FACE_OUTER_BOUND ( 'NONE', #68547, .T. ) ;
#63709 = CARTESIAN_POINT ( 'NONE',  ( 18.00000000000000000, 78.20644475923570837, 3.828778322547196300 ) ) ;
#63710 = CARTESIAN_POINT ( 'NONE',  ( 0.5774900079438607392, 63.48035201082149825, 5.440088680355550821 ) ) ;
#63711 = CARTESIAN_POINT ( 'NONE',  ( 10.00000000000000178, 12.25893115100078568, 9.846743663894594434 ) ) ;
#63712 = CARTESIAN_POINT ( 'NONE',  ( -3.772435417270453506, -6.430908609835228162, 3.750000000000806466 ) ) ;
#63713 = EDGE_CURVE ( 'NONE', #27622, #25275, #33541, .T. ) ;
#63714 = ORIENTED_EDGE ( 'NONE', *, *, #60997, .T. ) ;
#63715 = FACE_OUTER_BOUND ( 'NONE', #94021, .T. ) ;
#63716 = EDGE_LOOP ( 'NONE', ( #82718, #12322, #41520, #48513, #80569, #5183, #71487, #15300 ) ) ;
#63717 = CARTESIAN_POINT ( 'NONE',  ( 5.076628168052704559, 30.17559781766745175, -8.527530157486179263 ) ) ;
#63718 = EDGE_LOOP ( 'NONE', ( #20427, #53401, #49847, #42522 ) ) ;
#63719 = CARTESIAN_POINT ( 'NONE',  ( 10.00000000000000178, 33.05374883491396787, 14.16423886937410082 ) ) ;
#63720 = CARTESIAN_POINT ( 'NONE',  ( 18.52753015748617571, 28.09226448433411960, 4.923371831947298993 ) ) ;
#63721 = CARTESIAN_POINT ( 'NONE',  ( 0.5774900079438607392, 43.48035201082151247, 5.440088680355550821 ) ) ;
#63722 = ADVANCED_FACE ( 'NONE', ( #40081 ), #94549, .T. ) ;
#63723 = CIRCLE ( 'NONE', #54156, 14.49999999999999822 ) ;
#63724 =( LENGTH_UNIT ( ) NAMED_UNIT ( * ) SI_UNIT ( .MILLI., .METRE. ) );
#63725 = CARTESIAN_POINT ( 'NONE',  ( 17.96484262340118221, 34.93868534415482685, 7.964842623401181321 ) ) ;
#63726 = CARTESIAN_POINT ( 'NONE',  ( 3.434112377981054287, -7.334698663402913432, -12.81628187352647608 ) ) ;
#63727 = ORIENTED_EDGE ( 'NONE', *, *, #29511, .F. ) ;
#63728 = CARTESIAN_POINT ( 'NONE',  ( 15.44008868035555260, 44.73035201082151247, 9.422509992056143702 ) ) ;
#63729 = CARTESIAN_POINT ( 'NONE',  ( 24.16423886937409904, 4.095415501580634832, 3.795296366450317205 ) ) ;
#63730 = VERTEX_POINT ( 'NONE', #64527 ) ;
#63731 = VERTEX_POINT ( 'NONE', #9088 ) ;
#63732 = CARTESIAN_POINT ( 'NONE',  ( 0.1532563361054100626, 0.8005978176674514168, -2.638427012816831230 ) ) ;
#63733 = CARTESIAN_POINT ( 'NONE',  ( -2.816281873526471635, 28.91530133659708213, -3.434112377981056508 ) ) ;
#63734 = AXIS2_PLACEMENT_3D ( 'NONE', #79410, #3910, #41918 ) ;
#63735 = CARTESIAN_POINT ( 'NONE',  ( 1.472469842513823179, 21.42559781766745175, 4.923371831947296329 ) ) ;
#63736 = CARTESIAN_POINT ( 'NONE',  ( 4.559911319644449179, 2.230352010821504471, -9.422509992056141925 ) ) ;
#63737 = DIRECTION ( 'NONE',  ( -1.000000000000000000, -0.000000000000000000, -0.000000000000000000 ) ) ;
#63738 = CARTESIAN_POINT ( 'NONE',  ( 1.472469842513823179, 35.59226448433412315, -4.923371831947296329 ) ) ;
#63739 = CARTESIAN_POINT ( 'NONE',  ( 19.42250999205614193, 60.14701867748817676, 5.440088680355555262 ) ) ;
#63740 = CARTESIAN_POINT ( 'NONE',  ( 10.00000000000000178, 69.31368534415484817, 10.88017736071110342 ) ) ;
#63741 = CARTESIAN_POINT ( 'NONE',  ( -14.94699059465108881, 14.49999999999999112, 1.259949270174695268 ) ) ;
#63742 = CARTESIAN_POINT ( 'NONE',  ( -1.099225684535947600, 64.54030133659709634, 6.408140936763237150 ) ) ;
#63743 = CARTESIAN_POINT ( 'NONE',  ( 2.791683348922237240, 10.38393115100078390, -7.208316651077763204 ) ) ;
#63744 = CARTESIAN_POINT ( 'NONE',  ( 13.43411237798105340, 15.58196800326374998, 12.81628187352647963 ) ) ;
#63745 = CARTESIAN_POINT ( 'NONE',  ( -0.1503990784575328643, 70.00000000000000000, 6.262539305110068177 ) ) ;
#63746 = CARTESIAN_POINT ( 'NONE',  ( 5.076628168052703671, 46.84226448433412315, 8.527530157486179263 ) ) ;
#63747 = CARTESIAN_POINT ( 'NONE',  ( 20.88017736071110164, 35.35535201082150536, 2.915334737309930979 ) ) ;
#63748 = CARTESIAN_POINT ( 'NONE',  ( 24.16423886937409904, 4.095415501580634832, 3.795296366450317205 ) ) ;
#63749 = CARTESIAN_POINT ( 'NONE',  ( 19.84674366389459266, 33.30059781766744464, 2.638427012816836559 ) ) ;
#63750 = CARTESIAN_POINT ( 'NONE',  ( -2.816281873526471635, 33.91530133659708213, -3.434112377981056508 ) ) ;
#63752 = CARTESIAN_POINT ( 'NONE',  ( 7.674335239599196612, 0.2306972965111885598, 12.81961907869222372 ) ) ;
#63751 =( LENGTH_UNIT ( ) NAMED_UNIT ( * ) SI_UNIT ( .MILLI., .METRE. ) );
#63753 = CARTESIAN_POINT ( 'NONE',  ( 19.42250999205614193, 45.14701867748817676, 5.440088680355555262 ) ) ;
#63754 = CARTESIAN_POINT ( 'NONE',  ( -2.816281873526473856, 9.123634669930421381, 9.499525473075851096E-16 ) ) ;
#63755 = CARTESIAN_POINT ( 'NONE',  ( 0.1532563361054083140, 41.00893115100078745, 1.131784320476157264E-15 ) ) ;
#63756 = CARTESIAN_POINT ( 'NONE',  ( 0.1532563361054083140, 26.00893115100078745, 1.131784320476157264E-15 ) ) ;
#63757 = CARTESIAN_POINT ( 'NONE',  ( 10.00000000000000000, 21.81368534415484106, -10.88017736071110342 ) ) ;
#63758 = EDGE_CURVE ( 'NONE', #72571, #40524, #41801, .T. ) ;
#63759 = CARTESIAN_POINT ( 'NONE',  ( 13.43411237798105340, 30.58196800326374998, 12.81628187352647963 ) ) ;
#63760 = CARTESIAN_POINT ( 'NONE',  ( 19.84674366389459266, 18.30059781766745175, 2.638427012816836559 ) ) ;
#63761 = CARTESIAN_POINT ( 'NONE',  ( -6.382347221874291598, 14.49999999999999112, -13.57444820018240783 ) ) ;
#63762 = CARTESIAN_POINT ( 'NONE',  ( 19.42250999205614193, 15.14701867748817143, 5.440088680355555262 ) ) ;
#63763 = CARTESIAN_POINT ( 'NONE',  ( 4.559911319644449179, 58.89701867748817676, 9.422509992056141925 ) ) ;
#63764 = CARTESIAN_POINT ( 'NONE',  ( 2.035157376598824452, 8.688685344154839285, 7.964842623401179544 ) ) ;
#63766 = CARTESIAN_POINT ( 'NONE',  ( 15.44008868035555793, 36.39701867748816966, -9.422509992056140149 ) ) ;
#63765 = CARTESIAN_POINT ( 'NONE',  ( 2.791683348922240793, 46.63393115100077324, 7.208316651077764092 ) ) ;
#63767 = CARTESIAN_POINT ( 'NONE',  ( 19.42250999205614193, 40.14701867748817676, 5.440088680355555262 ) ) ;
#63768 = CARTESIAN_POINT ( 'NONE',  ( -0.8801773607111008646, 18.27201867748817321, 2.915334737309923430 ) ) ;
#63769 = CARTESIAN_POINT ( 'NONE',  ( 20.32896413005680358, 54.74545670184114243, 5.963430220938287007 ) ) ;
#63770 = CARTESIAN_POINT ( 'NONE',  ( 0.1532563361054083140, 36.00893115100078745, 1.131784320476157264E-15 ) ) ;
#63772 = CARTESIAN_POINT ( 'NONE',  ( -5.817157072110619609, 0.3640475087720984049, -13.82608706751095085 ) ) ;
#63771 = CARTESIAN_POINT ( 'NONE',  ( -0.3689425029237881626, 37.42874883491396787, 10.36894250292379027 ) ) ;
#63773 = DIRECTION ( 'NONE',  ( 0.000000000000000000, 1.000000000000000000, 0.000000000000000000 ) ) ;
#63774 = CARTESIAN_POINT ( 'NONE',  ( 22.81628187352647785, 6.623634669930420493, 6.195893100308588602E-16 ) ) ;
#63775 = CIRCLE ( 'NONE', #68593, 14.49999999999999822 ) ;
#63776 = CARTESIAN_POINT ( 'NONE',  ( -18.00000000000000355, 75.73428692542562146, 3.000000000000000000 ) ) ;
#63777 = CARTESIAN_POINT ( 'NONE',  ( 17.08211943468705130, 28.47041550158063572, 12.26659068614894998 ) ) ;
#63778 = DIRECTION ( 'NONE',  ( 0.3338068592337714025, 0.000000000000000000, 0.9426414910921783186 ) ) ;
#63779 = ORIENTED_EDGE ( 'NONE', *, *, #22369, .T. ) ;
#63780 = EDGE_CURVE ( 'NONE', #58411, #40169, #6680, .T. ) ;
#63781 = CARTESIAN_POINT ( 'NONE',  ( -4.164238869374099039, 61.80374883491397497, 8.674139862899312516E-16 ) ) ;
#63782 = CARTESIAN_POINT ( 'NONE',  ( 19.84674366389459266, 18.71726448433411960, -2.638427012816827677 ) ) ;
#63783 = FACE_OUTER_BOUND ( 'NONE', #66381, .T. ) ;
#63784 = CARTESIAN_POINT ( 'NONE',  ( 15.44008868035555793, 61.39701867748817676, -9.422509992056140149 ) ) ;
#63785 = DIRECTION ( 'NONE',  ( 0.4771587602596153999, 0.000000000000000000, -0.8788171126619616080 ) ) ;
#63786 = CARTESIAN_POINT ( 'NONE',  ( 17.96484262340118221, 24.93868534415484461, 7.964842623401181321 ) ) ;
#63787 = DIRECTION ( 'NONE',  ( 0.000000000000000000, -1.000000000000000000, 0.000000000000000000 ) ) ;
#63788 = CARTESIAN_POINT ( 'NONE',  ( 10.00000000000000178, 5.373634669930420493, 12.81628187352647608 ) ) ;
#63789 = CARTESIAN_POINT ( 'NONE',  ( 14.92337183194729633, 12.67559781766745353, 8.527530157486181039 ) ) ;
#63791 = EDGE_LOOP ( 'NONE', ( #15086, #69880, #96710, #71370, #55037, #5097 ) ) ;
#63790 = EDGE_CURVE ( 'NONE', #1898, #79104, #24253, .T. ) ;
#63792 = CARTESIAN_POINT ( 'NONE',  ( 2.791683348922237240, 0.3839311510007847872, -7.208316651077763204 ) ) ;
#63793 = CARTESIAN_POINT ( 'NONE',  ( -3.927832320392065313, 15.00000000000000000, -13.69797916712109398 ) ) ;
#63794 = CARTESIAN_POINT ( 'NONE',  ( 13.79529636645030344, 58.26208216824728936, 14.16423886937410614 ) ) ;
#63795 = CARTESIAN_POINT ( 'NONE',  ( 24.16423886937410614, 24.30374883491396787, 8.672049930838204340E-16 ) ) ;
#63796 = CARTESIAN_POINT ( 'NONE',  ( -0.8801773607111008646, 28.27201867748817321, 2.915334737309923430 ) ) ;
#63797 = CARTESIAN_POINT ( 'NONE',  ( -0.8801773607111008646, 48.27201867748816966, 2.915334737309923430 ) ) ;
#63798 = DIRECTION ( 'NONE',  ( 1.000000000000000000, 0.000000000000000000, -0.000000000000000000 ) ) ;
#63799 = VECTOR ( 'NONE', #56775, 1000.000000000000000 ) ;
#63800 = CARTESIAN_POINT ( 'NONE',  ( 19.84674366389459266, 48.71726448433412315, -2.638427012816827677 ) ) ;
#63801 = B_SPLINE_CURVE_WITH_KNOTS ( 'NONE', 3,
 ( #90308, #22338, #77283, #52325, #90810, #69804, #14338, #37344, #1327, #31779, #67834, #351, #52126, #88142, #36128, #20143, #72639, #19654 ),
 .UNSPECIFIED., .F., .F.,
 ( 4, 2, 2, 2, 2, 2, 2, 2, 4 ),
 ( 2.168404344971008868E-18, 0.002783576088282441099, 0.005567152176564879595, 0.01113430435312975572, 0.02226860870625951144, 0.04453721741251901595, 0.06680582611877852739, 0.07794013047190828658, 0.08907443482503803189 ),
 .UNSPECIFIED. ) ;
#63802 = CARTESIAN_POINT ( 'NONE',  ( 18.52753015748618282, 3.925597817667451306, -4.923371831947291888 ) ) ;
#63803 = DIRECTION ( 'NONE',  ( 0.000000000000000000, 0.000000000000000000, -1.000000000000000000 ) ) ;
#63804 = CARTESIAN_POINT ( 'NONE',  ( 0.1532563361054100626, 20.80059781766744464, -2.638427012816831230 ) ) ;
#63805 = CARTESIAN_POINT ( 'NONE',  ( 0.1532563361054083140, 26.00893115100078745, 1.131784320476157264E-15 ) ) ;
#63806 = CARTESIAN_POINT ( 'NONE',  ( 17.20831665107776587, 52.88393115100078035, 7.208316651077764980 ) ) ;
#63807 = CARTESIAN_POINT ( 'NONE',  ( 19.42250999205614548, 20.98035201082150891, -5.440088680355545492 ) ) ;
#63808 = B_SPLINE_CURVE_WITH_KNOTS ( 'NONE', 3,
 ( #60715, #91212, #45726, #82730, #22740, #83725 ),
 .UNSPECIFIED., .F., .F.,
 ( 4, 2, 4 ),
 ( 0.000000000000000000, 0.0002701661927229334929, 0.0005403323854458669858 ),
 .UNSPECIFIED. ) ;
#63809 = CARTESIAN_POINT ( 'NONE',  ( 3.591859063236761518, 34.95696800326375353, 11.09922568453594849 ) ) ;
#63810 = CARTESIAN_POINT ( 'NONE',  ( 4.559911319644449179, 58.89701867748817676, 9.422509992056141925 ) ) ;
#63811 = CARTESIAN_POINT ( 'NONE',  ( 5.076628168052704559, 30.17559781766745175, -8.527530157486179263 ) ) ;
#63813 = CARTESIAN_POINT ( 'NONE',  ( 1.472469842513823179, 20.59226448433411960, -4.923371831947296329 ) ) ;
#63812 = CARTESIAN_POINT ( 'NONE',  ( -2.266590686148945544, 46.38708216824730357, -7.082119434687050408 ) ) ;
#63814 = CARTESIAN_POINT ( 'NONE',  ( -9.024359497401759356, 75.07164295747612925, 3.000000000000000000 ) ) ;
#63815 = CARTESIAN_POINT ( 'NONE',  ( 10.00000000000000000, 54.75893115100078745, -9.846743663894594434 ) ) ;
#63817 = CARTESIAN_POINT ( 'NONE',  ( 20.36894250292379382, 8.678748834913967869, 10.36894250292379205 ) ) ;
#63816 = CARTESIAN_POINT ( 'NONE',  ( 0.1532563361054083140, 51.00893115100078745, 1.131784320476157264E-15 ) ) ;
#63818 = CARTESIAN_POINT ( 'NONE',  ( -0.3689425029237881626, 32.42874883491395366, 10.36894250292379027 ) ) ;
#63819 = CARTESIAN_POINT ( 'NONE',  ( 0.1532563361054083140, 31.00893115100078390, 1.131784320476157264E-15 ) ) ;
#63820 = CARTESIAN_POINT ( 'NONE',  ( 20.88017736071110519, 25.56368534415483751, 2.639326808657452039E-16 ) ) ;
#63821 = CARTESIAN_POINT ( 'NONE',  ( -0.8801773607111008646, 43.27201867748817676, 2.915334737309923430 ) ) ;
#63822 = CARTESIAN_POINT ( 'NONE',  ( -0.8801773607111009756, 48.06368534415484817, 1.068504757029289695E-15 ) ) ;
#63823 = ORIENTED_EDGE ( 'NONE', *, *, #33865, .F. ) ;
#63824 = CARTESIAN_POINT ( 'NONE',  ( 13.43411237798106583, 32.66530133659708213, -12.81628187352647252 ) ) ;
#63825 = CARTESIAN_POINT ( 'NONE',  ( 12.91533473730993009, 56.60535201082151247, -10.88017736071109987 ) ) ;
#63826 = ORIENTED_EDGE ( 'NONE', *, *, #4812, .T. ) ;
#63827 = CARTESIAN_POINT ( 'NONE',  ( 7.361572987183169658, -0.03273551566588185635, -9.846743663894592657 ) ) ;
#63828 = ADVANCED_FACE ( 'NONE', ( #12528 ), #29496, .T. ) ;
#63829 = CARTESIAN_POINT ( 'NONE',  ( 0.5774900079438607392, 58.48035201082151247, 5.440088680355550821 ) ) ;
#63830 = ORIENTED_EDGE ( 'NONE', *, *, #45259, .F. ) ;
#63831 = CARTESIAN_POINT ( 'NONE',  ( 0.5774900079438590739, 57.64701867748817676, -5.440088680355550821 ) ) ;
#63832 = DIRECTION ( 'NONE',  ( 0.000000000000000000, 0.000000000000000000, -1.000000000000000000 ) ) ;
#63833 = CARTESIAN_POINT ( 'NONE',  ( 0.000000000000000000, 91.25000000000000000, 8.000000000000000000 ) ) ;
#63834 = CARTESIAN_POINT ( 'NONE',  ( 10.00000000000000000, 11.81368534415483751, -10.88017736071110342 ) ) ;
#63835 = CARTESIAN_POINT ( 'NONE',  ( 17.20831665107776587, 9.133931151000787452, -7.208316651077762316 ) ) ;
#63836 = CARTESIAN_POINT ( 'NONE',  ( 17.08211943468705130, 3.470415501580634388, 12.26659068614894998 ) ) ;
#63837 = CARTESIAN_POINT ( 'NONE',  ( 19.84674366389459266, 8.300597817667451750, 2.638427012816836559 ) ) ;
#63838 = CARTESIAN_POINT ( 'NONE',  ( 0.5774900079438607392, 8.480352010821505360, 5.440088680355550821 ) ) ;
#63839 = CARTESIAN_POINT ( 'NONE',  ( 19.84674366389459266, 48.71726448433413026, -2.638427012816827677 ) ) ;
#63840 = ORIENTED_EDGE ( 'NONE', *, *, #55676, .F. ) ;
#63841 = CIRCLE ( 'NONE', #38321, 6.499999999999995559 ) ;
#63842 = CARTESIAN_POINT ( 'NONE',  ( 18.52753015748618282, 48.92559781766745886, -4.923371831947291888 ) ) ;
#63843 = ORIENTED_EDGE ( 'NONE', *, *, #7710, .F. ) ;
#63844 = CARTESIAN_POINT ( 'NONE',  ( 17.96484262340118221, 56.18868534415484817, -7.964842623401177768 ) ) ;
#63845 = CARTESIAN_POINT ( 'NONE',  ( 2.791683348922237240, 45.38393115100079456, -7.208316651077763204 ) ) ;
#63847 = DIRECTION ( 'NONE',  ( 0.06975647374412534407, 0.9975640502598241977, 0.000000000000000000 ) ) ;
#63846 = DIRECTION ( 'NONE',  ( 0.000000000000000000, 0.000000000000000000, 1.000000000000000000 ) ) ;
#63848 = CARTESIAN_POINT ( 'NONE',  ( 20.88017736071110164, 60.35535201082151957, 2.915334737309930979 ) ) ;
#63849 = CIRCLE ( 'NONE', #76640, 3.940000000000000835 ) ;
#63850 = CARTESIAN_POINT ( 'NONE',  ( 19.42250999205614548, 10.98035201082150536, -5.440088680355545492 ) ) ;
#63851 = VECTOR ( 'NONE', #83394, 1000.000000000000114 ) ;
#63852 = CARTESIAN_POINT ( 'NONE',  ( -1.099225684535947600, 43.70696800326375353, -6.408140936763238038 ) ) ;
#63853 = CYLINDRICAL_SURFACE ( 'NONE', #27553, 15.00000000000000000 ) ;
#63854 = ORIENTED_EDGE ( 'NONE', *, *, #25686, .F. ) ;
#63855 = CARTESIAN_POINT ( 'NONE',  ( -1.099225684535947600, 29.54030133659708923, 6.408140936763237150 ) ) ;
#63856 = CARTESIAN_POINT ( 'NONE',  ( 2.035157376598824452, 28.68868534415484106, 7.964842623401179544 ) ) ;
#63857 = ADVANCED_FACE ( 'NONE', ( #61001 ), #61983, .T. ) ;
#63858 = VERTEX_POINT ( 'NONE', #22534 ) ;
#63859 = CARTESIAN_POINT ( 'NONE',  ( 7.361572987183170547, 57.05059781766744464, 9.846743663894590881 ) ) ;
#63861 = CARTESIAN_POINT ( 'NONE',  ( 0.1532563361054082862, 56.21726448433411605, 2.638427012816831674 ) ) ;
#63860 = CARTESIAN_POINT ( 'NONE',  ( 2.791683348922240793, 6.633931151000785675, 7.208316651077764092 ) ) ;
#63862 = CARTESIAN_POINT ( 'NONE',  ( 0.1089645850228758012, 28.16234555792570049, 6.479102184480775684 ) ) ;
#63863 = CARTESIAN_POINT ( 'NONE',  ( -27.43587634952537968, 22.49999999999998934, 10.00000000000000000 ) ) ;
#63864 = CARTESIAN_POINT ( 'NONE',  ( 14.92337183194729988, 34.34226448433411605, -8.527530157486177487 ) ) ;
#63865 = CARTESIAN_POINT ( 'NONE',  ( -15.00000000000004974, 91.25000000000000000, -7.750000000000000000 ) ) ;
#63866 = CARTESIAN_POINT ( 'NONE',  ( 1.821158202401482962, 61.16688879859522388, 6.499999999999917399 ) ) ;
#63868 =( NAMED_UNIT ( * ) PLANE_ANGLE_UNIT ( ) SI_UNIT ( $, .RADIAN. ) );
#63867 = CARTESIAN_POINT ( 'NONE',  ( 18.52753015748617571, 28.09226448433411960, 4.923371831947298993 ) ) ;
#63869 = CARTESIAN_POINT ( 'NONE',  ( 0.000000000000000000, 14.49999999999999822, 0.000000000000000000 ) ) ;
#63870 = EDGE_CURVE ( 'NONE', #70565, #11027, #67534, .T. ) ;
#63872 = VERTEX_POINT ( 'NONE', #84011 ) ;
#63871 = CARTESIAN_POINT ( 'NONE',  ( 17.20831665107776587, 54.13393115100079456, -7.208316651077762316 ) ) ;
#63873 = CARTESIAN_POINT ( 'NONE',  ( -0.8801773607110990882, 7.855352010821506248, -2.915334737309924318 ) ) ;
#63874 = CARTESIAN_POINT ( 'NONE',  ( 19.38216949554541202, 20.99863466993042138, 9.382169495545424454 ) ) ;
#63875 = CARTESIAN_POINT ( 'NONE',  ( 18.52753015748618282, 48.92559781766745886, -4.923371831947291888 ) ) ;
#63876 = EDGE_CURVE ( 'NONE', #74806, #34483, #52, .T. ) ;
#63877 = CARTESIAN_POINT ( 'NONE',  ( -0.03932841506543179738, 8.121614419605014845, 6.397827110478955248 ) ) ;
#63879 = EDGE_CURVE ( 'NONE', #37066, #38896, #3479, .T. ) ;
#63878 = CARTESIAN_POINT ( 'NONE',  ( 17.08211943468705840, 50.13708216824730357, -12.26659068614894466 ) ) ;
#63880 = CARTESIAN_POINT ( 'NONE',  ( 17.20831665107776587, 19.13393115100078035, -7.208316651077762316 ) ) ;
#63881 = LINE ( 'NONE', #8928, #2992 ) ;
#63882 = CARTESIAN_POINT ( 'NONE',  ( 8.470897558477602729, 15.00000000000000711, -11.92401951126078963 ) ) ;
#63883 = CARTESIAN_POINT ( 'NONE',  ( -2.266590686148945544, 46.38708216824730357, -7.082119434687050408 ) ) ;
#63884 = CARTESIAN_POINT ( 'NONE',  ( 7.361572987183169658, 54.96726448433413026, -9.846743663894592657 ) ) ;
#63885 = CARTESIAN_POINT ( 'NONE',  ( 0.5774900079438590739, 2.647018677488171434, -5.440088680355550821 ) ) ;
#63886 = CARTESIAN_POINT ( 'NONE',  ( 22.26659068614895176, 19.72041550158063572, -7.082119434687042414 ) ) ;
#63887 = CARTESIAN_POINT ( 'NONE',  ( 24.16423886937410614, 39.30374883491396787, 8.672049930838204340E-16 ) ) ;
#63888 = SURFACE_SIDE_STYLE ('',( #33390 ) ) ;
#63890 = CARTESIAN_POINT ( 'NONE',  ( 18.52753015748617571, 53.09226448433412315, 4.923371831947298993 ) ) ;
#63889 = CARTESIAN_POINT ( 'NONE',  ( -0.8801773607111009756, 28.06368534415484106, 1.068504757029289695E-15 ) ) ;
#63891 = ORIENTED_EDGE ( 'NONE', *, *, #14836, .T. ) ;
#63892 = CARTESIAN_POINT ( 'NONE',  ( 0.5774900079438607392, 33.48035201082150536, 5.440088680355550821 ) ) ;
#63893 = DIRECTION ( 'NONE',  ( 0.000000000000000000, 0.000000000000000000, 1.000000000000000000 ) ) ;
#63894 = CARTESIAN_POINT ( 'NONE',  ( -7.750000000000000000, 40.99999999999999289, 4.250000000000000000 ) ) ;
#63895 = CARTESIAN_POINT ( 'NONE',  ( 17.20831665107776587, 49.13393115100078745, -7.208316651077762316 ) ) ;
#63896 = CARTESIAN_POINT ( 'NONE',  ( -27.43587634952537968, 22.49999999999998934, 10.00000000000000000 ) ) ;
#63897 = CARTESIAN_POINT ( 'NONE',  ( -14.16423886937410437, 6.595415501580630391, -3.795296366450299885 ) ) ;
#63898 = CARTESIAN_POINT ( 'NONE',  ( 17.20831665107776587, 57.88393115100078745, 7.208316651077764980 ) ) ;
#63899 = CARTESIAN_POINT ( 'NONE',  ( 14.92337183194729633, 62.67559781766745886, 8.527530157486181039 ) ) ;
#63900 = CIRCLE ( 'NONE', #46370, 0.5000000000000004441 ) ;
#63902 = EDGE_CURVE ( 'NONE', #95826, #70674, #17814, .T. ) ;
#63901 = ORIENTED_EDGE ( 'NONE', *, *, #72820, .T. ) ;
#63903 = CARTESIAN_POINT ( 'NONE',  ( 13.79529636645031943, 30.34541550158063927, -14.16423886937409904 ) ) ;
#63904 = CARTESIAN_POINT ( 'NONE',  ( 11.10000000000000142, 98.49999999999998579, -8.525133428036873795 ) ) ;
#63905 = CARTESIAN_POINT ( 'NONE',  ( -4.535014064424438551, -17.52590857052339146, -2.499999999999193534 ) ) ;
#63906 = CARTESIAN_POINT ( 'NONE',  ( 4.559911319644449179, 2.230352010821504916, -9.422509992056141925 ) ) ;
#63907 = CARTESIAN_POINT ( 'NONE',  ( -2.816281873526473856, 19.12363466993042138, 9.499525473075851096E-16 ) ) ;
#63908 = FACE_OUTER_BOUND ( 'NONE', #67814, .T. ) ;
#63909 = CARTESIAN_POINT ( 'NONE',  ( 14.92337183194729988, 9.342264484334119601, -8.527530157486177487 ) ) ;
#63910 = AXIS2_PLACEMENT_3D ( 'NONE', #40955, #96422, #3447 ) ;
#63911 = EDGE_CURVE ( 'NONE', #37674, #32127, #13019, .T. ) ;
#63912 = CARTESIAN_POINT ( 'NONE',  ( 4.823529266124356063, -6.402884419280910677, -4.000000000000000000 ) ) ;
#63913 = CARTESIAN_POINT ( 'NONE',  ( 1.959929470562269183, 20.51528370094808196, -5.767676674365832312 ) ) ;
#63914 = CARTESIAN_POINT ( 'NONE',  ( -0.8801773607111008646, 8.272018677488171434, 2.915334737309923430 ) ) ;
#63915 = DIRECTION ( 'NONE',  ( -0.1993679344171901680, 0.000000000000000000, -0.9799247046208311440 ) ) ;
#63916 = CARTESIAN_POINT ( 'NONE',  ( 12.91533473730992121, 34.52201867748817676, 10.88017736071110164 ) ) ;
#63917 = CARTESIAN_POINT ( 'NONE',  ( 4.559911319644449179, 43.89701867748816966, 9.422509992056141925 ) ) ;
#63918 = CARTESIAN_POINT ( 'NONE',  ( 19.84674366389459621, 63.50893115100078745, 7.409399052514197653E-17 ) ) ;
#63919 = CARTESIAN_POINT ( 'NONE',  ( 7.361572987183169658, 64.96726448433412315, -9.846743663894592657 ) ) ;
#63920 = CARTESIAN_POINT ( 'NONE',  ( -0.7375392941516176748, 0.5000000000000004441, -14.98185688723471820 ) ) ;
#63921 = CARTESIAN_POINT ( 'NONE',  ( 12.63842701281683922, 14.55059781766744997, -9.846743663894590881 ) ) ;
#63922 = ORIENTED_EDGE ( 'NONE', *, *, #82010, .F. ) ;
#63923 = CARTESIAN_POINT ( 'NONE',  ( 19.42250999205614193, 30.14701867748817321, 5.440088680355555262 ) ) ;
#63924 = CARTESIAN_POINT ( 'NONE',  ( 19.38216949554541202, 35.99863466993041072, 9.382169495545424454 ) ) ;
#63925 = CARTESIAN_POINT ( 'NONE',  ( 7.361572987183169658, 64.96726448433412315, -9.846743663894592657 ) ) ;
#63926 = CARTESIAN_POINT ( 'NONE',  ( 0.5774900079438607392, 58.48035201082151247, 5.440088680355550821 ) ) ;
#63927 = CARTESIAN_POINT ( 'NONE',  ( 10.00000000000000178, 12.25893115100078568, 9.846743663894594434 ) ) ;
#63928 = CARTESIAN_POINT ( 'NONE',  ( 22.81628187352648496, 36.83196800326376064, -3.434112377981050290 ) ) ;
#63930 = CARTESIAN_POINT ( 'NONE',  ( -2.614810775378867191, 35.00346125376525919, -10.00000000000000000 ) ) ;
#63929 = CARTESIAN_POINT ( 'NONE',  ( 19.42250999205614548, 65.98035201082151957, -5.440088680355545492 ) ) ;
#63931 = ORIENTED_EDGE ( 'NONE', *, *, #25409, .T. ) ;
#63932 = FACE_OUTER_BOUND ( 'NONE', #52776, .T. ) ;
#63933 =( NAMED_UNIT ( * ) PLANE_ANGLE_UNIT ( ) SI_UNIT ( $, .RADIAN. ) );
#63934 = CARTESIAN_POINT ( 'NONE',  ( 2.035157376598822676, 12.43868534415483751, -7.964842623401177768 ) ) ;
#63936 = CARTESIAN_POINT ( 'NONE',  ( -4.164238869374098151, 26.59541550158063217, -3.795296366450310543 ) ) ;
#63935 = CARTESIAN_POINT ( 'NONE',  ( 21.09922568453595559, 57.04030133659708923, -6.408140936763230044 ) ) ;
#63937 = CARTESIAN_POINT ( 'NONE',  ( 1.472469842513823179, 11.42559781766745175, 4.923371831947296329 ) ) ;
#63938 = VECTOR ( 'NONE', #65135, 1000.000000000000000 ) ;
#63939 = CARTESIAN_POINT ( 'NONE',  ( 14.92337183194729988, 14.34226448433411782, -8.527530157486177487 ) ) ;
#63940 = CARTESIAN_POINT ( 'NONE',  ( 10.00000000000000000, 55.55374883491396787, -14.16423886937410082 ) ) ;
#63941 = ORIENTED_EDGE ( 'NONE', *, *, #8542, .F. ) ;
#63942 = CARTESIAN_POINT ( 'NONE',  ( -0.8801773607111009756, 18.06368534415484106, 1.068504757029289695E-15 ) ) ;
#63943 = EDGE_CURVE ( 'NONE', #85865, #51000, #46016, .T. ) ;
#63944 = CARTESIAN_POINT ( 'NONE',  ( 17.96484262340118221, 21.18868534415483396, -7.964842623401177768 ) ) ;
#63945 = CARTESIAN_POINT ( 'NONE',  ( 19.50000000000000711, 98.59912998021083297, 4.500000000000000888 ) ) ;
#63946 = ORIENTED_EDGE ( 'NONE', *, *, #47541, .F. ) ;
#63947 = DIRECTION ( 'NONE',  ( -0.000000000000000000, 1.000000000000000000, 0.000000000000000000 ) ) ;
#63948 = CARTESIAN_POINT ( 'NONE',  ( 12.91533473730992121, 19.52201867748816611, 10.88017736071110164 ) ) ;
#63949 = CARTESIAN_POINT ( 'NONE',  ( 1.472469842513823179, 50.59226448433411605, -4.923371831947296329 ) ) ;
#63950 = AXIS2_PLACEMENT_3D ( 'NONE', #28102, #11139, #41658 ) ;
#63951 = B_SPLINE_CURVE_WITH_KNOTS ( 'NONE', 3,
 ( #45241, #92222, #37761, #77212 ),
 .UNSPECIFIED., .F., .F.,
 ( 4, 4 ),
 ( 0.000000000000000000, 0.002657014572711323321 ),
 .UNSPECIFIED. ) ;
#63952 = DIRECTION ( 'NONE',  ( -0.000000000000000000, -1.000000000000000000, -0.000000000000000000 ) ) ;
#63953 = DIRECTION ( 'NONE',  ( 0.000000000000000000, 0.000000000000000000, -1.000000000000000000 ) ) ;
#63954 = CARTESIAN_POINT ( 'NONE',  ( 2.917880565312948704, 22.63708216824730002, 12.26659068614894643 ) ) ;
#63955 = CARTESIAN_POINT ( 'NONE',  ( 15.44008868035555793, 41.39701867748817676, -9.422509992056140149 ) ) ;
#63956 = CARTESIAN_POINT ( 'NONE',  ( -0.8801773607111008646, 13.27201867748817321, 2.915334737309923430 ) ) ;
#63957 = CARTESIAN_POINT ( 'NONE',  ( 19.84674366389459621, 58.50893115100078745, 7.409399052514197653E-17 ) ) ;
#63958 = CARTESIAN_POINT ( 'NONE',  ( -11.60530215607347948, -82.03068034365578853, -3.750000000000000000 ) ) ;
#63959 = CARTESIAN_POINT ( 'NONE',  ( 14.92337183194729988, 39.34226448433412315, -8.527530157486177487 ) ) ;
#63960 = CARTESIAN_POINT ( 'NONE',  ( 5.378451019861591575, 0.000000000000000000, 0.9000440264802798129 ) ) ;
#63961 = CARTESIAN_POINT ( 'NONE',  ( 19.84674366389459266, 13.30059781766745353, 2.638427012816836559 ) ) ;
#63962 = CARTESIAN_POINT ( 'NONE',  ( -3.434112377981067610, -36.91803199673623936, -12.81628187352647252 ) ) ;
#63963 = ORIENTED_EDGE ( 'NONE', *, *, #2981, .T. ) ;
#63964 = CARTESIAN_POINT ( 'NONE',  ( 20.88017736071110164, 15.35535201082150358, 2.915334737309930979 ) ) ;
#63965 = CARTESIAN_POINT ( 'NONE',  ( 18.52753015748617571, 13.09226448433411960, 4.923371831947298993 ) ) ;
#63966 = CARTESIAN_POINT ( 'NONE',  ( 5.076628168052704559, 65.17559781766745175, -8.527530157486179263 ) ) ;
#63968 = CARTESIAN_POINT ( 'NONE',  ( 15.44008868035555793, 46.39701867748817676, -9.422509992056140149 ) ) ;
#63967 = CARTESIAN_POINT ( 'NONE',  ( 20.88017736071110875, 40.77201867748818387, -2.915334737309920765 ) ) ;
#63970 = CARTESIAN_POINT ( 'NONE',  ( 0.6178305044545838731, 49.74863466993041072, 9.382169495545420901 ) ) ;
#63969 = CARTESIAN_POINT ( 'NONE',  ( 19.42250999205614548, 15.98035201082150714, -5.440088680355545492 ) ) ;
#63971 = CARTESIAN_POINT ( 'NONE',  ( 24.16423886937409904, 34.09541550158064638, 3.795296366450317205 ) ) ;
#63972 = CARTESIAN_POINT ( 'NONE',  ( 20.24186590665275531, 12.61633188102327630, -6.114288769123077394 ) ) ;
#63973 = CARTESIAN_POINT ( 'NONE',  ( 22.81628187352647785, 61.62363466993041783, 6.195893100308588602E-16 ) ) ;
#63974 = VERTEX_POINT ( 'NONE', #60013 ) ;
#63975 = CARTESIAN_POINT ( 'NONE',  ( 2.791683348922240793, 51.63393115100078745, 7.208316651077764092 ) ) ;
#63976 = CARTESIAN_POINT ( 'NONE',  ( 19.42250999205614193, 40.14701867748817676, 5.440088680355555262 ) ) ;
#63977 = CIRCLE ( 'NONE', #70429, 0.5000000000000004441 ) ;
#63978 = EDGE_LOOP ( 'NONE', ( #25760, #32529, #75481, #94413 ) ) ;
#63980 = CARTESIAN_POINT ( 'NONE',  ( 14.48718990079890112, 15.00000000000000000, -0.6093675230840328583 ) ) ;
#63979 = CARTESIAN_POINT ( 'NONE',  ( 19.84674366389459621, 3.508931151000785231, 7.409399052514197653E-17 ) ) ;
#63981 = AXIS2_PLACEMENT_3D ( 'NONE', #76496, #45500, #19439 ) ;
#63982 = CARTESIAN_POINT ( 'NONE',  ( 1.274849032794278747, 42.55509018479936856, -6.499999999999960032 ) ) ;
#63983 = CARTESIAN_POINT ( 'NONE',  ( 1.472469842513823179, 16.42559781766745175, 4.923371831947296329 ) ) ;
#63984 = CARTESIAN_POINT ( 'NONE',  ( 19.84674366389459266, 23.30059781766745530, 2.638427012816836559 ) ) ;
#63985 = ADVANCED_FACE ( 'NONE', ( #46494 ), #56961, .T. ) ;
#63986 = CARTESIAN_POINT ( 'NONE',  ( 2.791683348922237240, 15.38393115100078212, -7.208316651077763204 ) ) ;
#63987 = CARTESIAN_POINT ( 'NONE',  ( 0.1532563361054083140, 6.008931151000784787, 1.131784320476157264E-15 ) ) ;
#63989 = CARTESIAN_POINT ( 'NONE',  ( -38.69000000000001194, 93.50000000000000000, 9.500000000000000000 ) ) ;
#63988 = CARTESIAN_POINT ( 'NONE',  ( 4.559911319644449179, 62.23035201082150536, -9.422509992056141925 ) ) ;
#63990 = CARTESIAN_POINT ( 'NONE',  ( 17.96484262340118221, 56.18868534415484817, -7.964842623401177768 ) ) ;
#63992 = VERTEX_POINT ( 'NONE', #87949 ) ;
#63991 = CARTESIAN_POINT ( 'NONE',  ( 17.20831665107776587, 19.13393115100078035, -7.208316651077762316 ) ) ;
#63993 = ADVANCED_FACE ( 'NONE', ( #34942 ), #44418, .F. ) ;
#63994 = CARTESIAN_POINT ( 'NONE',  ( 0.8952175423695086787, 63.52576239577081907, 5.990408912944362285 ) ) ;
#63995 = CARTESIAN_POINT ( 'NONE',  ( 5.076628168052704559, 50.17559781766745886, -8.527530157486179263 ) ) ;
#63996 = ORIENTED_EDGE ( 'NONE', *, *, #44473, .F. ) ;
#63997 = VERTEX_POINT ( 'NONE', #13432 ) ;
#63998 = DIRECTION ( 'NONE',  ( 0.000000000000000000, 1.000000000000000000, -0.000000000000000000 ) ) ;
#63999 = ADVANCED_FACE ( 'NONE', ( #5461 ), #42954, .F. ) ;
#64000 = CARTESIAN_POINT ( 'NONE',  ( 19.38216949554541202, 55.99863466993041072, 9.382169495545424454 ) ) ;
#64001 =( LENGTH_UNIT ( ) NAMED_UNIT ( * ) SI_UNIT ( .MILLI., .METRE. ) );
#64002 = CARTESIAN_POINT ( 'NONE',  ( 2.917880565312948704, 37.63708216824731068, 12.26659068614894643 ) ) ;
#64003 =( NAMED_UNIT ( * ) SI_UNIT ( $, .STERADIAN. ) SOLID_ANGLE_UNIT ( ) );
#64004 = CARTESIAN_POINT ( 'NONE',  ( -0.3689425029237898834, 6.178748834913968757, -10.36894250292378850 ) ) ;
#64005 = CARTESIAN_POINT ( 'NONE',  ( 20.88017736071110875, 30.77201867748816966, -2.915334737309920765 ) ) ;
#64006 = ORIENTED_EDGE ( 'NONE', *, *, #34653, .F. ) ;
#64007 = CARTESIAN_POINT ( 'NONE',  ( 19.84674366389459266, 13.71726448433411782, -2.638427012816827677 ) ) ;
#64009 = CARTESIAN_POINT ( 'NONE',  ( 7.361572987183170547, 12.05059781766744997, 9.846743663894590881 ) ) ;
#64008 = CARTESIAN_POINT ( 'NONE',  ( 19.42250999205614193, 55.14701867748817676, 5.440088680355555262 ) ) ;
#64010 = AXIS2_PLACEMENT_3D ( 'NONE', #19045, #25087, #3075 ) ;
#64011 = CARTESIAN_POINT ( 'NONE',  ( 22.81628187352647785, 41.62363466993042493, 6.195893100308588602E-16 ) ) ;
#64012 = CARTESIAN_POINT ( 'NONE',  ( 0.1532563361054082862, 36.21726448433410894, 2.638427012816831674 ) ) ;
#64013 = DIRECTION ( 'NONE',  ( 0.000000000000000000, 0.000000000000000000, 1.000000000000000000 ) ) ;
#64014 = CARTESIAN_POINT ( 'NONE',  ( 4.559911319644449179, 58.89701867748817676, 9.422509992056141925 ) ) ;
#64015 = CARTESIAN_POINT ( 'NONE',  ( 10.00000000000000000, 22.87363466993042138, -12.81628187352647608 ) ) ;
#64016 = CARTESIAN_POINT ( 'NONE',  ( -14.16423886937410082, -38.19625116508603213, 4.336808689942017736E-15 ) ) ;
#64017 = CARTESIAN_POINT ( 'NONE',  ( 0.1532563361054100626, 20.80059781766744464, -2.638427012816831230 ) ) ;
#64018 = PRESENTATION_LAYER_ASSIGNMENT (  '', '', ( #8169 ) ) ;
#64019 = CARTESIAN_POINT ( 'NONE',  ( -0.3689425029237898834, 16.17874883491396076, -10.36894250292378850 ) ) ;
#64020 = ORIENTED_EDGE ( 'NONE', *, *, #63270, .T. ) ;
#64021 = CARTESIAN_POINT ( 'NONE',  ( 12.91533473730993009, 36.60535201082151247, -10.88017736071109987 ) ) ;
#64022 = CARTESIAN_POINT ( 'NONE',  ( -2.266590686148945544, 37.22041550158063217, 7.082119434687048631 ) ) ;
#64023 = CARTESIAN_POINT ( 'NONE',  ( 19.84674366389459266, 53.71726448433411605, -2.638427012816827677 ) ) ;
#64024 = CARTESIAN_POINT ( 'NONE',  ( 12.63842701281683034, 12.46726448433411782, 9.846743663894596210 ) ) ;
#64026 = CARTESIAN_POINT ( 'NONE',  ( 10.00000000000000178, 70.00000000000000000, 0.000000000000000000 ) ) ;
#64025 = CARTESIAN_POINT ( 'NONE',  ( 16.40814093676324603, 52.45696800326375353, -11.09922568453594671 ) ) ;
#64027 = CARTESIAN_POINT ( 'NONE',  ( 4.559911319644449179, 43.89701867748816966, 9.422509992056141925 ) ) ;
#64028 = EDGE_CURVE ( 'NONE', #14809, #97109, #78549, .T. ) ;
#64029 = CARTESIAN_POINT ( 'NONE',  ( 7.361080431567760485, -0.6440110890646428832, 3.000000000000000000 ) ) ;
#64030 = CARTESIAN_POINT ( 'NONE',  ( 13.43411237798106583, 22.66530133659708923, -12.81628187352647252 ) ) ;
#64031 = CARTESIAN_POINT ( 'NONE',  ( 14.92337183194729988, 59.34226448433412315, -8.527530157486177487 ) ) ;
#64032 = CARTESIAN_POINT ( 'NONE',  ( 10.88017736071110519, 10.56368534415484639, -2.602085213965210642E-15 ) ) ;
#64034 = CARTESIAN_POINT ( 'NONE',  ( -13.48255862861931043, 15.00000000000000000, 5.335786055104065895 ) ) ;
#64033 = CARTESIAN_POINT ( 'NONE',  ( -0.1042174387088687926, 13.10736173766201240, 6.337391062633409788 ) ) ;
#64035 = CARTESIAN_POINT ( 'NONE',  ( 14.99847009497944406, 15.00000000000000000, 0.2142307401081381124 ) ) ;
#64037 = EDGE_CURVE ( 'NONE', #98896, #16073, #91315, .T. ) ;
#64036 = CARTESIAN_POINT ( 'NONE',  ( 66.56412365047464164, 26.99999999999998224, 9.500000000000000000 ) ) ;
#64038 = CARTESIAN_POINT ( 'NONE',  ( 7.084665262690076126, 52.02201867748816255, -10.88017736071110164 ) ) ;
#64039 = VECTOR ( 'NONE', #38324, 1000.000000000000000 ) ;
#64040 = CARTESIAN_POINT ( 'NONE',  ( 12.91533473730993009, 51.60535201082149825, -10.88017736071109987 ) ) ;
#64041 = CARTESIAN_POINT ( 'NONE',  ( -0.1688089201193209155, 79.91181047996344944, 9.500000000000000000 ) ) ;
#64042 = DIRECTION ( 'NONE',  ( -0.000000000000000000, -1.000000000000000000, -0.000000000000000000 ) ) ;
#64043 = CARTESIAN_POINT ( 'NONE',  ( 19.84674366389459621, 23.50893115100078390, 7.409399052514197653E-17 ) ) ;
#64044 = CARTESIAN_POINT ( 'NONE',  ( 2.035157376598824452, 18.68868534415484106, 7.964842623401179544 ) ) ;
#64045 = CARTESIAN_POINT ( 'NONE',  ( 5.076628168052703671, 66.84226448433412315, 8.527530157486179263 ) ) ;
#64047 = CARTESIAN_POINT ( 'NONE',  ( -3.521924875522737253, -0.8399941893316781316, -3.750000000000001332 ) ) ;
#64046 = CARTESIAN_POINT ( 'NONE',  ( 4.559911319644449179, 23.89701867748817321, 9.422509992056141925 ) ) ;
#64048 = CARTESIAN_POINT ( 'NONE',  ( 20.32896413005680714, 52.60497603579417358, -5.963430220938276349 ) ) ;
#64049 = CIRCLE ( 'NONE', #28936, 15.00000000000000000 ) ;
#64050 = CARTESIAN_POINT ( 'NONE',  ( 6.565887622018943937, 23.08196800326375708, -12.81628187352647608 ) ) ;
#64051 = ORIENTED_EDGE ( 'NONE', *, *, #90552, .T. ) ;
#64052 = CARTESIAN_POINT ( 'NONE',  ( 0.5774900079438607392, 53.48035201082151247, 5.440088680355550821 ) ) ;
#64053 = CARTESIAN_POINT ( 'NONE',  ( 2.791683348922240793, 46.63393115100077324, 7.208316651077764092 ) ) ;
#64054 = CARTESIAN_POINT ( 'NONE',  ( 19.38216949554541202, 25.99863466993042138, 9.382169495545424454 ) ) ;
#64055 = CARTESIAN_POINT ( 'NONE',  ( -0.8801773607110991993, 32.85535201082151247, -2.915334737309923874 ) ) ;
#64056 = CARTESIAN_POINT ( 'NONE',  ( -0.3689425029237898834, 46.17874883491397497, -10.36894250292378850 ) ) ;
#64057 = CARTESIAN_POINT ( 'NONE',  ( 5.076628168052703671, 36.84226448433412315, 8.527530157486179263 ) ) ;
#64058 = CARTESIAN_POINT ( 'NONE',  ( 2.035157376598822676, 67.43868534415484817, -7.964842623401177768 ) ) ;
#64059 = CARTESIAN_POINT ( 'NONE',  ( -0.8801773607111008646, 48.27201867748816966, 2.915334737309923430 ) ) ;
#64060 = CARTESIAN_POINT ( 'NONE',  ( -8.564643372776465924, 14.49999999999999112, -12.31449893000758955 ) ) ;
#64061 = CARTESIAN_POINT ( 'NONE',  ( 24.16423886937409904, 19.09541550158063927, 3.795296366450317205 ) ) ;
#64062 = CARTESIAN_POINT ( 'NONE',  ( 1.711636803080548441, 21.84492782695770430, -6.499999999999988454 ) ) ;
#64063 = ORIENTED_EDGE ( 'NONE', *, *, #98651, .T. ) ;
#64064 = ORIENTED_EDGE ( 'NONE', *, *, #52539, .F. ) ;
#64065 = CARTESIAN_POINT ( 'NONE',  ( 17.08211943468705840, 50.13708216824730357, -12.26659068614894466 ) ) ;
#64066 = CARTESIAN_POINT ( 'NONE',  ( 20.36894250292379738, 54.92874883491396076, -10.36894250292379027 ) ) ;
#64067 = CARTESIAN_POINT ( 'NONE',  ( 7.361572987183170547, 17.05059781766745530, 9.846743663894590881 ) ) ;
#64068 = CARTESIAN_POINT ( 'NONE',  ( 16.40814093676323893, 15.79030133659708746, 11.09922568453595026 ) ) ;
#64069 = CARTESIAN_POINT ( 'NONE',  ( 7.771322705631394712, 15.00000000000000000, 12.24159072199921283 ) ) ;
#64070 = CARTESIAN_POINT ( 'NONE',  ( 0.9940297508536876103, 0.000000000000000000, 14.21528771620250353 ) ) ;
#64072 = CARTESIAN_POINT ( 'NONE',  ( 3.591859063236761518, 34.95696800326375353, 11.09922568453594849 ) ) ;
#64071 = CARTESIAN_POINT ( 'NONE',  ( 2.035157376598822676, 67.43868534415484817, -7.964842623401177768 ) ) ;
#64073 = CARTESIAN_POINT ( 'NONE',  ( -2.266590686148945544, 47.22041550158063927, 7.082119434687048631 ) ) ;
#64074 = SURFACE_STYLE_USAGE ( .BOTH. , #41121 ) ;
#64075 = PRESENTATION_STYLE_ASSIGNMENT (( #33581 ) ) ;
#64076 = CARTESIAN_POINT ( 'NONE',  ( 7.208316651077762316, -0.8660688489992137695, -7.208316651077764980 ) ) ;
#64077 = EDGE_CURVE ( 'NONE', #52255, #81670, #75247, .T. ) ;
#64078 = VERTEX_POINT ( 'NONE', #49956 ) ;
#64079 = PLANE ( 'NONE',  #49210 ) ;
#64080 = CARTESIAN_POINT ( 'NONE',  ( 19.84674366389459266, 18.71726448433411960, -2.638427012816827677 ) ) ;
#64081 = CARTESIAN_POINT ( 'NONE',  ( 8.880000000000000782, 1.019547802438458550, -3.750000000000000000 ) ) ;
#64082 = VERTEX_POINT ( 'NONE', #12938 ) ;
#64083 = CARTESIAN_POINT ( 'NONE',  ( 24.16423886937410614, 14.30374883491396787, 8.672049930838204340E-16 ) ) ;
#64085 = CARTESIAN_POINT ( 'NONE',  ( 17.96484262340118221, 16.18868534415483396, -7.964842623401177768 ) ) ;
#64084 = CARTESIAN_POINT ( 'NONE',  ( -0.8801773607110991993, 12.85535201082150358, -2.915334737309923874 ) ) ;
#64087 = CARTESIAN_POINT ( 'NONE',  ( 10.00000000000000000, 7.873634669930421381, -12.81628187352647608 ) ) ;
#64086 = CARTESIAN_POINT ( 'NONE',  ( 14.92337183194729988, 44.34226448433412315, -8.527530157486177487 ) ) ;
#64088 = CARTESIAN_POINT ( 'NONE',  ( -3.166711953933234014, 0.000000000000000000, 4.439566422914446697 ) ) ;
#64089 = VECTOR ( 'NONE', #91839, 1000.000000000000000 ) ;
#64090 = EDGE_CURVE ( 'NONE', #9878, #21520, #45504, .T. ) ;
#64091 = CARTESIAN_POINT ( 'NONE',  ( -14.09394518620605297, 15.00000000000000000, -3.407449058785551710 ) ) ;
#64092 = STYLED_ITEM ( 'NONE', ( #95907 ), #80374 ) ;
#64093 = CARTESIAN_POINT ( 'NONE',  ( 6.565887622018943937, 23.08196800326375708, -12.81628187352647608 ) ) ;
#64094 = ORIENTED_EDGE ( 'NONE', *, *, #19983, .F. ) ;
#64095 = CARTESIAN_POINT ( 'NONE',  ( 24.16423886937409904, 54.09541550158063217, 3.795296366450317205 ) ) ;
#64096 = ORIENTED_EDGE ( 'NONE', *, *, #46564, .T. ) ;
#64097 = CARTESIAN_POINT ( 'NONE',  ( 2.917880565312948704, 57.63708216824731068, 12.26659068614894643 ) ) ;
#64098 = ORIENTED_EDGE ( 'NONE', *, *, #22288, .F. ) ;
#64099 = CARTESIAN_POINT ( 'NONE',  ( 7.084665262690076126, 37.02201867748817676, -10.88017736071110164 ) ) ;
#64100 = CARTESIAN_POINT ( 'NONE',  ( 17.96484262340118221, 41.18868534415484106, -7.964842623401177768 ) ) ;
#64101 = CARTESIAN_POINT ( 'NONE',  ( 4.559911319644449179, 68.89701867748817676, 9.422509992056141925 ) ) ;
#64102 = CARTESIAN_POINT ( 'NONE',  ( 2.035157376598822676, 32.43868534415483396, -7.964842623401177768 ) ) ;
#64104 = AXIS2_PLACEMENT_3D ( 'NONE', #37929, #37435, #76402 ) ;
#64103 = CARTESIAN_POINT ( 'NONE',  ( -13.21236992757665973, 15.00000000000000000, -5.338143956176898186 ) ) ;
#64105 = ADVANCED_FACE ( 'NONE', ( #20947 ), #30573, .T. ) ;
#64106 = CIRCLE ( 'NONE', #41802, 0.2500000000000000000 ) ;
#64107 = CARTESIAN_POINT ( 'NONE',  ( 19.84674366389459621, 13.50893115100078568, 7.409399052514197653E-17 ) ) ;
#64108 = CARTESIAN_POINT ( 'NONE',  ( -4.000000000000000000, 10.25000000000000000, -2.750000000000000000 ) ) ;
#64109 = EDGE_LOOP ( 'NONE', ( #2781, #13562, #8712, #61900 ) ) ;
#64110 = CARTESIAN_POINT ( 'NONE',  ( 8.959592931194404031, -9.312622102008740299, 4.000000000000000000 ) ) ;
#64111 = CARTESIAN_POINT ( 'NONE',  ( 18.52753015748617571, 38.09226448433412315, 4.923371831947298993 ) ) ;
#64113 = EDGE_CURVE ( 'NONE', #43512, #32737, #74416, .T. ) ;
#64112 = CYLINDRICAL_SURFACE ( 'NONE', #54768, 11.92686044187656513 ) ;
#64114 =( GEOMETRIC_REPRESENTATION_CONTEXT ( 3 ) GLOBAL_UNCERTAINTY_ASSIGNED_CONTEXT ( ( #42310 ) ) GLOBAL_UNIT_ASSIGNED_CONTEXT ( ( #60788, #84306, #68803 ) ) REPRESENTATION_CONTEXT ( 'NONE', 'WORKASPACE' ) );
#64115 = CARTESIAN_POINT ( 'NONE',  ( -3.711005778769052021, -5.293034685380286319, 2.750000000000000000 ) ) ;
#64116 = DIRECTION ( 'NONE',  ( 0.9799247046208269252, 0.000000000000000000, 0.1993679344172108736 ) ) ;
#64117 = CARTESIAN_POINT ( 'NONE',  ( -0.1503990784575328643, 65.12777174578613426, 6.262539305110068177 ) ) ;
#64118 = CARTESIAN_POINT ( 'NONE',  ( 17.20831665107776587, 62.88393115100078745, 7.208316651077764980 ) ) ;
#64119 = CARTESIAN_POINT ( 'NONE',  ( 2.917880565312948704, 47.63708216824730357, 12.26659068614894643 ) ) ;
#64120 = DIRECTION ( 'NONE',  ( -0.000000000000000000, -0.000000000000000000, 1.000000000000000000 ) ) ;
#64121 = VERTEX_POINT ( 'NONE', #42465 ) ;
#64123 = CIRCLE ( 'NONE', #76914, 0.2500000000000002220 ) ;
#64122 = DIRECTION ( 'NONE',  ( 0.000000000000000000, 0.000000000000000000, 1.000000000000000000 ) ) ;
#64124 = CARTESIAN_POINT ( 'NONE',  ( 14.92337183194729988, 34.34226448433411605, -8.527530157486177487 ) ) ;
#64125 = CARTESIAN_POINT ( 'NONE',  ( 6.565887622018943937, 10.16530133659708746, 12.81628187352647430 ) ) ;
#64126 = CARTESIAN_POINT ( 'NONE',  ( 18.52753015748617571, 3.092264484334118269, 4.923371831947298993 ) ) ;
#64127 =( NAMED_UNIT ( * ) SI_UNIT ( $, .STERADIAN. ) SOLID_ANGLE_UNIT ( ) );
#64128 = CARTESIAN_POINT ( 'NONE',  ( 7.361572987183169658, 59.96726448433410894, -9.846743663894592657 ) ) ;
#64129 = CARTESIAN_POINT ( 'NONE',  ( 31.00000000000000355, 44.99999999999999289, 7.000000000000000000 ) ) ;
#64130 = ADVANCED_FACE ( 'NONE', ( #72946 ), #25809, .T. ) ;
#64131 = EDGE_LOOP ( 'NONE', ( #27919, #52293, #59101, #94532 ) ) ;
#64132 = CARTESIAN_POINT ( 'NONE',  ( 7.084665262690076126, 2.022018677488171434, -10.88017736071110164 ) ) ;
#64133 = DIRECTION ( 'NONE',  ( 0.000000000000000000, 1.000000000000000000, 0.000000000000000000 ) ) ;
#64134 = CARTESIAN_POINT ( 'NONE',  ( 7.084665262690076126, 37.02201867748817676, -10.88017736071110164 ) ) ;
#64136 = LINE ( 'NONE', #5638, #52912 ) ;
#64135 = CARTESIAN_POINT ( 'NONE',  ( 10.00000000000000178, 15.37363466993042138, 12.81628187352647608 ) ) ;
#64137 = CARTESIAN_POINT ( 'NONE',  ( 10.82361996477978217, 0.04962893104176950565, -10.02529603627134236 ) ) ;
#64138 = EDGE_CURVE ( 'NONE', #46976, #1757, #30395, .T. ) ;
#64139 = CARTESIAN_POINT ( 'NONE',  ( 6.579634127946654587, -87.99828267815715321, 3.250000000000000888 ) ) ;
#64140 = CARTESIAN_POINT ( 'NONE',  ( 18.29284471827484637, 35.40189080397292543, -6.500000000000014211 ) ) ;
#64141 = CARTESIAN_POINT ( 'NONE',  ( 14.92337183194729988, 54.34226448433412315, -8.527530157486177487 ) ) ;
#64142 = B_SPLINE_CURVE_WITH_KNOTS ( 'NONE', 3,
 ( #11241, #70784, #9282, #24303, #94742, #63741 ),
 .UNSPECIFIED., .F., .F.,
 ( 4, 2, 4 ),
 ( 0.0002800098398967154449, 0.0006862151655623427004, 0.001092420491227969956 ),
 .UNSPECIFIED. ) ;
#64143 = CARTESIAN_POINT ( 'NONE',  ( -3.795296366450322534, 30.76208216824731423, -14.16423886937409904 ) ) ;
#64144 = CARTESIAN_POINT ( 'NONE',  ( 16.40814093676324603, 7.456968003263754419, -11.09922568453594671 ) ) ;
#64145 = CARTESIAN_POINT ( 'NONE',  ( -9.206646936938154724, -19.70874149522700591, -4.000000000000000888 ) ) ;
#64147 = CARTESIAN_POINT ( 'NONE',  ( 6.000000000000000000, 61.50000000000000711, 6.500000000000000888 ) ) ;
#64146 = CARTESIAN_POINT ( 'NONE',  ( 15.44008868035555260, 29.73035201082150891, 9.422509992056143702 ) ) ;
#64148 = CARTESIAN_POINT ( 'NONE',  ( 22.26659068614894466, 33.88708216824730357, 7.082119434687054849 ) ) ;
#64149 = CARTESIAN_POINT ( 'NONE',  ( 24.16423886937410614, 24.30374883491396787, 8.672049930838204340E-16 ) ) ;
#64150 = CARTESIAN_POINT ( 'NONE',  ( 17.96484262340118221, 16.18868534415483396, -7.964842623401177768 ) ) ;
#64151 = CARTESIAN_POINT ( 'NONE',  ( 5.076628168052703671, 36.84226448433412315, 8.527530157486179263 ) ) ;
#64152 = CARTESIAN_POINT ( 'NONE',  ( -2.816281873526473856, 34.33196800326376064, 3.434112377981055619 ) ) ;
#64153 = CARTESIAN_POINT ( 'NONE',  ( 17.96484262340118221, 16.18868534415483396, -7.964842623401177768 ) ) ;
#64154 =( GEOMETRIC_REPRESENTATION_CONTEXT ( 3 ) GLOBAL_UNCERTAINTY_ASSIGNED_CONTEXT ( ( #45448 ) ) GLOBAL_UNIT_ASSIGNED_CONTEXT ( ( #4806, #54226, #59758 ) ) REPRESENTATION_CONTEXT ( 'NONE', 'WORKASPACE' ) );
#64155 = CARTESIAN_POINT ( 'NONE',  ( 7.361572987183170547, 42.05059781766745886, 9.846743663894590881 ) ) ;
#64156 = CARTESIAN_POINT ( 'NONE',  ( 4.559911319644449179, 37.23035201082150536, -9.422509992056141925 ) ) ;
#64157 = CARTESIAN_POINT ( 'NONE',  ( 10.00000000000000178, 0.3736346699304200492, 12.81628187352647608 ) ) ;
#64159 = CARTESIAN_POINT ( 'NONE',  ( 0.1532563361054082862, 61.21726448433412315, 2.638427012816831674 ) ) ;
#64158 = CARTESIAN_POINT ( 'NONE',  ( 13.79529636645031943, 25.34541550158063572, -14.16423886937409904 ) ) ;
#64160 = CARTESIAN_POINT ( 'NONE',  ( 8.879999999999995453, 40.99999999999999289, -3.750000000000000000 ) ) ;
#64161 = UNCERTAINTY_MEASURE_WITH_UNIT (LENGTH_MEASURE( 1.000000000000000082E-05 ), #36300, 'distance_accuracy_value', 'NONE');
#64162 = CARTESIAN_POINT ( 'NONE',  ( 5.076628168052704559, 20.17559781766745175, -8.527530157486179263 ) ) ;
#64163 = CARTESIAN_POINT ( 'NONE',  ( 22.81628187352648496, 51.83196800326376064, -3.434112377981050290 ) ) ;
#64164 = CARTESIAN_POINT ( 'NONE',  ( 14.92337183194729988, 59.34226448433412315, -8.527530157486177487 ) ) ;
#64165 = EDGE_LOOP ( 'NONE', ( #66660, #35479, #87209, #18216 ) ) ;
#64166 = DIRECTION ( 'NONE',  ( -6.608470384673550777E-17, -1.000000000000000000, -0.000000000000000000 ) ) ;
#64167 = DIRECTION ( 'NONE',  ( -0.000000000000000000, -0.000000000000000000, -1.000000000000000000 ) ) ;
#64168 = CARTESIAN_POINT ( 'NONE',  ( 13.79529636645030344, 63.26208216824730357, 14.16423886937410614 ) ) ;
#64169 = CARTESIAN_POINT ( 'NONE',  ( -2.266590686148945544, 11.38708216824730179, -7.082119434687050408 ) ) ;
#64170 = CARTESIAN_POINT ( 'NONE',  ( 15.44008868035555793, 66.39701867748817676, -9.422509992056140149 ) ) ;
#64171 = CARTESIAN_POINT ( 'NONE',  ( 1.472469842513823179, 46.42559781766745175, 4.923371831947296329 ) ) ;
#64172 = CARTESIAN_POINT ( 'NONE',  ( 17.96484262340118221, 14.93868534415483751, 7.964842623401181321 ) ) ;
#64173 = CARTESIAN_POINT ( 'NONE',  ( 9.779999999999990479, 20.99999999999999645, 3.000000000000000000 ) ) ;
#64174 = CARTESIAN_POINT ( 'NONE',  ( 1.472469842513823179, 66.42559781766745175, 4.923371831947296329 ) ) ;
#64175 = ORIENTED_EDGE ( 'NONE', *, *, #31140, .T. ) ;
#64176 = UNCERTAINTY_MEASURE_WITH_UNIT (LENGTH_MEASURE( 1.000000000000000082E-05 ), #83414, 'distance_accuracy_value', 'NONE');
#64177 = VECTOR ( 'NONE', #75689, 999.9999999999998863 ) ;
#64178 = CARTESIAN_POINT ( 'NONE',  ( -4.856044144387521300, 2.253107639696438902E-16, -13.79699902221167918 ) ) ;
#64179 = ORIENTED_EDGE ( 'NONE', *, *, #95864, .F. ) ;
#64180 = VERTEX_POINT ( 'NONE', #91398 ) ;
#64181 = CARTESIAN_POINT ( 'NONE',  ( 12.24319267753454099, 54.01141590572476048, -2.899999999999999467 ) ) ;
#64182 = CARTESIAN_POINT ( 'NONE',  ( -0.3689425029237881626, 7.428748834913967869, 10.36894250292379027 ) ) ;
#64183 = CARTESIAN_POINT ( 'NONE',  ( -0.3689425029237881626, 2.428748834913967869, 10.36894250292379027 ) ) ;
#64184 = B_SPLINE_CURVE_WITH_KNOTS ( 'NONE', 3,
 ( #87355, #56855, #42356, #4369, #96356, #18869, #34834, #72831 ),
 .UNSPECIFIED., .F., .F.,
 ( 4, 2, 2, 4 ),
 ( 2.665285624635612776E-17, 0.003056699928650253879, 0.004585049892975365422, 0.006113399857300476532 ),
 .UNSPECIFIED. ) ;
#64185 = CARTESIAN_POINT ( 'NONE',  ( 10.00000000000000000, 54.75893115100078745, -9.846743663894594434 ) ) ;
#64186 = CARTESIAN_POINT ( 'NONE',  ( 2.791683348922237240, 30.38393115100078390, -7.208316651077763204 ) ) ;
#64187 = SURFACE_SIDE_STYLE ('',( #40727 ) ) ;
#64189 = CARTESIAN_POINT ( 'NONE',  ( 0.1532563361054082862, 56.21726448433411605, 2.638427012816831674 ) ) ;
#64188 = CARTESIAN_POINT ( 'NONE',  ( 0.5774900079438590739, 27.64701867748817676, -5.440088680355550821 ) ) ;
#64190 = SURFACE_STYLE_FILL_AREA ( #94208 ) ;
#64191 = CARTESIAN_POINT ( 'NONE',  ( 24.16423886937409904, 44.09541550158063927, 3.795296366450317205 ) ) ;
#64192 = CARTESIAN_POINT ( 'NONE',  ( 6.204703633549690345, 65.76208216824731778, -14.16423886937410259 ) ) ;
#64193 = CARTESIAN_POINT ( 'NONE',  ( 7.361572987183169658, 64.96726448433412315, -9.846743663894592657 ) ) ;
#64194 = AXIS2_PLACEMENT_3D ( 'NONE', #93042, #91069, #40051 ) ;
#64195 = CARTESIAN_POINT ( 'NONE',  ( 0.8649609010933267950, 15.00000000000000178, -14.60103384664011195 ) ) ;
#64196 = CARTESIAN_POINT ( 'NONE',  ( 12.91533473730992121, 64.52201867748817676, 10.88017736071110164 ) ) ;
#64197 = CIRCLE ( 'NONE', #21101, 11.25000000000000178 ) ;
#64198 = CARTESIAN_POINT ( 'NONE',  ( 1.472469842513823179, 35.59226448433412315, -4.923371831947296329 ) ) ;
#64199 = CARTESIAN_POINT ( 'NONE',  ( -4.262581423003701353, -13.85606188143274231, 3.749999999999193090 ) ) ;
#64200 = ORIENTED_EDGE ( 'NONE', *, *, #73608, .T. ) ;
#64201 = DIRECTION ( 'NONE',  ( 0.000000000000000000, 0.000000000000000000, -1.000000000000000000 ) ) ;
#64202 = AXIS2_PLACEMENT_3D ( 'NONE', #27882, #37383, #66876 ) ;
#64203 = ORIENTED_EDGE ( 'NONE', *, *, #33404, .T. ) ;
#64204 = CARTESIAN_POINT ( 'NONE',  ( 19.84674366389459266, 18.71726448433411960, -2.638427012816827677 ) ) ;
#64205 = ORIENTED_EDGE ( 'NONE', *, *, #69556, .T. ) ;
#64206 = CARTESIAN_POINT ( 'NONE',  ( 17.08211943468705840, 35.13708216824730357, -12.26659068614894466 ) ) ;
#64207 = CARTESIAN_POINT ( 'NONE',  ( 5.076628168052703671, 31.84226448433412315, 8.527530157486179263 ) ) ;
#64208 = CARTESIAN_POINT ( 'NONE',  ( 2.035157376598822676, 57.43868534415484106, -7.964842623401177768 ) ) ;
#64209 = EDGE_CURVE ( 'NONE', #55079, #10597, #37204, .T. ) ;
#64210 = CARTESIAN_POINT ( 'NONE',  ( 2.035157376598822676, 42.43868534415483396, -7.964842623401177768 ) ) ;
#64211 = CARTESIAN_POINT ( 'NONE',  ( 18.52753015748618282, 43.92559781766745175, -4.923371831947291888 ) ) ;
#64212 = CARTESIAN_POINT ( 'NONE',  ( -3.434112377981067610, -6.918031996736242917, -12.81628187352647252 ) ) ;
#64213 = EDGE_LOOP ( 'NONE', ( #81686, #50914, #58365, #71157 ) ) ;
#64214 = CARTESIAN_POINT ( 'NONE',  ( -2.266590686148945544, 12.22041550158063394, 7.082119434687048631 ) ) ;
#64215 = ORIENTED_EDGE ( 'NONE', *, *, #62079, .T. ) ;
#64216 = ORIENTED_EDGE ( 'NONE', *, *, #11405, .T. ) ;
#64217 = CARTESIAN_POINT ( 'NONE',  ( 19.38216949554541202, 25.99863466993042138, 9.382169495545424454 ) ) ;
#64218 = FILL_AREA_STYLE ('',( #79239 ) ) ;
#64219 = CARTESIAN_POINT ( 'NONE',  ( 0.1532563361054082862, 26.21726448433411605, 2.638427012816831674 ) ) ;
#64220 = FILL_AREA_STYLE ('',( #33721 ) ) ;
#64221 = CARTESIAN_POINT ( 'NONE',  ( -2.816281873526471635, 43.91530133659708923, -3.434112377981056508 ) ) ;
#64222 = CYLINDRICAL_SURFACE ( 'NONE', #70304, 1.500000000000001332 ) ;
#64223 = CARTESIAN_POINT ( 'NONE',  ( 2.791683348922240793, 31.63393115100078745, 7.208316651077764092 ) ) ;
#64224 = CARTESIAN_POINT ( 'NONE',  ( 10.00000000000000178, 64.31368534415483396, 10.88017736071110342 ) ) ;
#64225 = CIRCLE ( 'NONE', #21141, 0.5000000000000000000 ) ;
#64226 = ADVANCED_FACE ( 'NONE', ( #84409 ), #8399, .T. ) ;
#64227 = CARTESIAN_POINT ( 'NONE',  ( 7.084665262690076126, 67.02201867748817676, -10.88017736071110164 ) ) ;
#64228 = CARTESIAN_POINT ( 'NONE',  ( -45.12679085540637658, 105.3517674277019012, 4.910439065983985607 ) ) ;
#64229 = CYLINDRICAL_SURFACE ( 'NONE', #62054, 11.92686044187656513 ) ;
#64230 = CARTESIAN_POINT ( 'NONE',  ( 18.52753015748618282, 3.925597817667451306, -4.923371831947291888 ) ) ;
#64231 = EDGE_CURVE ( 'NONE', #58660, #78529, #89591, .T. ) ;
#64232 = DIRECTION ( 'NONE',  ( -1.000000000000000000, 0.000000000000000000, -0.000000000000000000 ) ) ;
#64233 = CARTESIAN_POINT ( 'NONE',  ( 10.00000000000000178, 47.25893115100078745, 9.846743663894594434 ) ) ;
#64234 = CARTESIAN_POINT ( 'NONE',  ( 8.008672916919360803E-16, 22.29452073070357088, 0.000000000000000000 ) ) ;
#64235 = CARTESIAN_POINT ( 'NONE',  ( -0.3689425029237881626, 7.428748834913967869, 10.36894250292379027 ) ) ;
#64236 = CARTESIAN_POINT ( 'NONE',  ( 0.1532563361054083140, 36.00893115100078745, 1.131784320476157264E-15 ) ) ;
#64237 = CARTESIAN_POINT ( 'NONE',  ( -2.816281873526473856, 29.12363466993041783, 9.499525473075851096E-16 ) ) ;
#64239 = CARTESIAN_POINT ( 'NONE',  ( -18.89999999999999147, 91.25000000000000000, 8.000000000000000000 ) ) ;
#64238 = FACE_OUTER_BOUND ( 'NONE', #51439, .T. ) ;
#64240 = CARTESIAN_POINT ( 'NONE',  ( 15.44008868035555793, 66.39701867748817676, -9.422509992056140149 ) ) ;
#64241 = CARTESIAN_POINT ( 'NONE',  ( 22.81628187352648496, 1.831968003263753753, -3.434112377981050290 ) ) ;
#64242 = LINE ( 'NONE', #18279, #8813 ) ;
#64243 = CARTESIAN_POINT ( 'NONE',  ( 17.20831665107776587, 22.88393115100078745, 7.208316651077764980 ) ) ;
#64244 = CARTESIAN_POINT ( 'NONE',  ( 10.00000000000000000, 26.81368534415484106, -10.88017736071110342 ) ) ;
#64245 = CARTESIAN_POINT ( 'NONE',  ( 22.81628187352647785, 26.62363466993042138, 6.195893100308588602E-16 ) ) ;
#64246 =( GEOMETRIC_REPRESENTATION_CONTEXT ( 3 ) GLOBAL_UNCERTAINTY_ASSIGNED_CONTEXT ( ( #37288 ) ) GLOBAL_UNIT_ASSIGNED_CONTEXT ( ( #30566, #8086, #77062 ) ) REPRESENTATION_CONTEXT ( 'NONE', 'WORKASPACE' ) );
#64247 = CARTESIAN_POINT ( 'NONE',  ( 2.791683348922240793, 26.63393115100078745, 7.208316651077764092 ) ) ;
#64248 = CARTESIAN_POINT ( 'NONE',  ( -8.636324037029986300, 86.94567068113131825, 4.522730969307667159 ) ) ;
#64249 = CARTESIAN_POINT ( 'NONE',  ( 12.91533473730992121, 39.52201867748817676, 10.88017736071110164 ) ) ;
#64250 = AXIS2_PLACEMENT_3D ( 'NONE', #2306, #8791, #77773 ) ;
#64251 = ORIENTED_EDGE ( 'NONE', *, *, #18631, .F. ) ;
#64252 =( GEOMETRIC_REPRESENTATION_CONTEXT ( 3 ) GLOBAL_UNCERTAINTY_ASSIGNED_CONTEXT ( ( #20298 ) ) GLOBAL_UNIT_ASSIGNED_CONTEXT ( ( #64498, #72498, #63037 ) ) REPRESENTATION_CONTEXT ( 'NONE', 'WORKASPACE' ) );
#64253 = CARTESIAN_POINT ( 'NONE',  ( 7.084665262690076126, 57.02201867748817676, -10.88017736071110164 ) ) ;
#64254 = CARTESIAN_POINT ( 'NONE',  ( 4.559911319644449179, 3.897018677488170990, 9.422509992056141925 ) ) ;
#64256 = CARTESIAN_POINT ( 'NONE',  ( 4.559911319644449179, 27.23035201082150536, -9.422509992056141925 ) ) ;
#64255 = CARTESIAN_POINT ( 'NONE',  ( 12.63842701281683034, 47.46726448433412315, 9.846743663894596210 ) ) ;
#64257 =( LENGTH_UNIT ( ) NAMED_UNIT ( * ) SI_UNIT ( .MILLI., .METRE. ) );
#64258 = CIRCLE ( 'NONE', #21184, 0.2499999999999999445 ) ;
#64259 = CARTESIAN_POINT ( 'NONE',  ( 10.00000000000000000, 46.81368534415484106, -10.88017736071110342 ) ) ;
#64260 = CARTESIAN_POINT ( 'NONE',  ( -0.8801773607111009756, 8.063685344154837509, 1.068504757029289695E-15 ) ) ;
#64261 = DIRECTION ( 'NONE',  ( -1.000000000000000000, 0.000000000000000000, 0.000000000000000000 ) ) ;
#64262 = VECTOR ( 'NONE', #5286, 999.9999999999998863 ) ;
#64263 = CARTESIAN_POINT ( 'NONE',  ( 10.00000000000000178, 42.25893115100078745, 9.846743663894594434 ) ) ;
#64265 = CARTESIAN_POINT ( 'NONE',  ( 20.24186590665278018, 19.73410085661204150, 6.114288769123035649 ) ) ;
#64264 = CARTESIAN_POINT ( 'NONE',  ( 20.36894250292379738, 54.92874883491396076, -10.36894250292379027 ) ) ;
#64266 = CARTESIAN_POINT ( 'NONE',  ( 8.979999999999991545, 21.00000000000000000, 2.900000000000000355 ) ) ;
#64267 = EDGE_CURVE ( 'NONE', #52153, #71557, #35502, .T. ) ;
#64268 =( LENGTH_UNIT ( ) NAMED_UNIT ( * ) SI_UNIT ( .MILLI., .METRE. ) );
#64270 = STYLED_ITEM ( 'NONE', ( #56217 ), #73599 ) ;
#64269 = CARTESIAN_POINT ( 'NONE',  ( 10.00000000000000178, 23.05374883491397142, 14.16423886937410082 ) ) ;
#64271 = CARTESIAN_POINT ( 'NONE',  ( -3.771300335753330568, -6.411622728200643273, 2.749999999999999556 ) ) ;
#64272 = CARTESIAN_POINT ( 'NONE',  ( -0.8801773607111008646, 3.272018677488171434, 2.915334737309923430 ) ) ;
#64273 = CARTESIAN_POINT ( 'NONE',  ( 5.076628168052704559, 40.17559781766745175, -8.527530157486179263 ) ) ;
#64275 = DIRECTION ( 'NONE',  ( 1.000000000000000000, 0.000000000000000000, 0.000000000000000000 ) ) ;
#64274 = CARTESIAN_POINT ( 'NONE',  ( 13.55255535720591986, 0.000000000000000000, 4.403492169843056914 ) ) ;
#64276 = CARTESIAN_POINT ( 'NONE',  ( 0.5774900079438607392, 58.48035201082151247, 5.440088680355550821 ) ) ;
#64277 = CARTESIAN_POINT ( 'NONE',  ( -2.816281873526473856, 64.12363466993042493, 9.499525473075851096E-16 ) ) ;
#64278 = CARTESIAN_POINT ( 'NONE',  ( 12.91533473730992121, 34.52201867748817676, 10.88017736071110164 ) ) ;
#64279 = CARTESIAN_POINT ( 'NONE',  ( 19.38216949554541202, 60.99863466993042493, 9.382169495545424454 ) ) ;
#64280 = CARTESIAN_POINT ( 'NONE',  ( 10.00000000000000000, 7.873634669930421381, -12.81628187352647608 ) ) ;
#64281 = CARTESIAN_POINT ( 'NONE',  ( 14.92337183194729988, 9.342264484334119601, -8.527530157486177487 ) ) ;
#64282 = EDGE_LOOP ( 'NONE', ( #25886, #36916, #8059, #46387 ) ) ;
#64283 = LINE ( 'NONE', #86324, #78166 ) ;
#64284 = CARTESIAN_POINT ( 'NONE',  ( 4.559911319644449179, 7.230352010821505360, -9.422509992056141925 ) ) ;
#64285 = VECTOR ( 'NONE', #44452, 1000.000000000000000 ) ;
#64286 = CARTESIAN_POINT ( 'NONE',  ( 13.79529636645031943, 30.34541550158063927, -14.16423886937409904 ) ) ;
#64287 = CARTESIAN_POINT ( 'NONE',  ( 10.00000000000000178, 34.31368534415484106, 10.88017736071110342 ) ) ;
#64288 = CARTESIAN_POINT ( 'NONE',  ( -0.8801773607110991993, 47.85535201082150536, -2.915334737309923874 ) ) ;
#64289 = PLANE ( 'NONE',  #89480 ) ;
#64290 = FACE_OUTER_BOUND ( 'NONE', #3750, .T. ) ;
#64291 = CARTESIAN_POINT ( 'NONE',  ( 19.84674366389459266, 3.717264484334118713, -2.638427012816827677 ) ) ;
#64292 = CARTESIAN_POINT ( 'NONE',  ( -14.09394518620614711, 4.304378373471060795E-16, 3.407449058785263940 ) ) ;
#64293 = CARTESIAN_POINT ( 'NONE',  ( 12.63842701281683034, 22.46726448433411605, 9.846743663894596210 ) ) ;
#64294 = CARTESIAN_POINT ( 'NONE',  ( -14.52941021839284907, 15.00000000000000888, 1.683622718072942170 ) ) ;
#64295 = DIRECTION ( 'NONE',  ( 0.000000000000000000, 1.000000000000000000, -0.000000000000000000 ) ) ;
#64296 = CARTESIAN_POINT ( 'NONE',  ( 5.076628168052704559, 25.17559781766745175, -8.527530157486179263 ) ) ;
#64297 = CARTESIAN_POINT ( 'NONE',  ( 10.00000000000000000, 49.75893115100078745, -9.846743663894594434 ) ) ;
#64298 = CARTESIAN_POINT ( 'NONE',  ( 2.035157376598822676, 27.43868534415483396, -7.964842623401177768 ) ) ;
#64299 = UNCERTAINTY_MEASURE_WITH_UNIT (LENGTH_MEASURE( 1.000000000000000082E-05 ), #77680, 'distance_accuracy_value', 'NONE');
#64300 = CIRCLE ( 'NONE', #48395, 15.00000000000000000 ) ;
#64301 = CARTESIAN_POINT ( 'NONE',  ( 13.43411237798106583, 47.66530133659709634, -12.81628187352647252 ) ) ;
#64302 = CARTESIAN_POINT ( 'NONE',  ( 2.035157376598822676, 67.43868534415484817, -7.964842623401177768 ) ) ;
#64303 = CARTESIAN_POINT ( 'NONE',  ( 2.791683348922240793, 31.63393115100078745, 7.208316651077764092 ) ) ;
#64305 = CARTESIAN_POINT ( 'NONE',  ( 10.00000000000000178, 17.25893115100078745, 9.846743663894594434 ) ) ;
#64304 = CARTESIAN_POINT ( 'NONE',  ( 17.08211943468705840, 45.13708216824730357, -12.26659068614894466 ) ) ;
#64306 = CARTESIAN_POINT ( 'NONE',  ( 0.1143410931637246358, 60.21691075486303646, 6.480892540919863443 ) ) ;
#64307 = CARTESIAN_POINT ( 'NONE',  ( 5.076628168052704559, 60.17559781766745175, -8.527530157486179263 ) ) ;
#64308 = CARTESIAN_POINT ( 'NONE',  ( -0.3689425029237881626, 12.42874883491396609, 10.36894250292379027 ) ) ;
#64309 = CARTESIAN_POINT ( 'NONE',  ( 10.00000000000000178, 28.05374883491396787, 14.16423886937410082 ) ) ;
#64310 = CARTESIAN_POINT ( 'NONE',  ( 10.00000000000000178, 27.25893115100078390, 9.846743663894594434 ) ) ;
#64311 = CARTESIAN_POINT ( 'NONE',  ( 0.4400000000000020006, 1.019547802438468986, 2.500000000000000000 ) ) ;
#64312 = CARTESIAN_POINT ( 'NONE',  ( 7.084665262690076126, 19.10535201082150181, 10.88017736071109987 ) ) ;
#64313 = CARTESIAN_POINT ( 'NONE',  ( 20.88017736071110164, 60.35535201082151957, 2.915334737309930979 ) ) ;
#64314 = CARTESIAN_POINT ( 'NONE',  ( 7.084665262690076126, 47.02201867748818387, -10.88017736071110164 ) ) ;
#64315 = ORIENTED_EDGE ( 'NONE', *, *, #6442, .F. ) ;
#64316 = CARTESIAN_POINT ( 'NONE',  ( 0.6178305044545838731, 39.74863466993041072, 9.382169495545420901 ) ) ;
#64317 = CARTESIAN_POINT ( 'NONE',  ( 19.42250999205614193, 55.14701867748817676, 5.440088680355555262 ) ) ;
#64318 = ORIENTED_EDGE ( 'NONE', *, *, #85385, .T. ) ;
#64319 = CARTESIAN_POINT ( 'NONE',  ( 13.34989199099680413, 14.95037102702803544, -6.279943681065447869 ) ) ;
#64320 = EDGE_CURVE ( 'NONE', #55254, #23929, #24322, .T. ) ;
#64321 = CARTESIAN_POINT ( 'NONE',  ( -19.64999999999999858, 92.00000000000000000, -7.750000000000000000 ) ) ;
#64322 = EDGE_LOOP ( 'NONE', ( #12571, #20545, #30290, #53554 ) ) ;
#64323 = CARTESIAN_POINT ( 'NONE',  ( 15.44008868035555793, 66.39701867748817676, -9.422509992056140149 ) ) ;
#64324 = CARTESIAN_POINT ( 'NONE',  ( 20.88017736071110519, 5.563685344154837509, 2.639326808657452039E-16 ) ) ;
#64325 = CARTESIAN_POINT ( 'NONE',  ( 14.43063482171895373, -2.066760391300490855E-16, -2.386446184883025179 ) ) ;
#64326 = DIRECTION ( 'NONE',  ( -0.000000000000000000, -1.000000000000000000, -0.000000000000000000 ) ) ;
#64327 = CARTESIAN_POINT ( 'NONE',  ( 0.5774900079438590739, 12.64701867748817321, -5.440088680355550821 ) ) ;
#64328 = CARTESIAN_POINT ( 'NONE',  ( 12.63842701281683922, 14.55059781766744997, -9.846743663894590881 ) ) ;
#64329 = CARTESIAN_POINT ( 'NONE',  ( 6.204703633549690345, 2.845415501580634388, 14.16423886937410082 ) ) ;
#64330 = AXIS2_PLACEMENT_3D ( 'NONE', #60686, #74709, #21725 ) ;
#64331 = CARTESIAN_POINT ( 'NONE',  ( 18.52753015748618282, 3.925597817667451306, -4.923371831947291888 ) ) ;
#64332 = VECTOR ( 'NONE', #95899, 1000.000000000000000 ) ;
#64333 = CARTESIAN_POINT ( 'NONE',  ( 15.44008868035555793, 11.39701867748817143, -9.422509992056140149 ) ) ;
#64334 = CARTESIAN_POINT ( 'NONE',  ( 0.1532563361054082862, 51.21726448433412315, 2.638427012816831674 ) ) ;
#64335 = STYLED_ITEM ( 'NONE', ( #89019 ), #93070 ) ;
#64336 = CARTESIAN_POINT ( 'NONE',  ( 10.00000000000000000, 44.75893115100078745, -9.846743663894594434 ) ) ;
#64337 = ORIENTED_EDGE ( 'NONE', *, *, #73815, .T. ) ;
#64338 = CARTESIAN_POINT ( 'NONE',  ( 18.72515096720568195, 31.07228050351032422, -6.500000000000018652 ) ) ;
#64339 = CARTESIAN_POINT ( 'NONE',  ( 2.035157376598824452, 53.68868534415484817, 7.964842623401179544 ) ) ;
#64340 = CARTESIAN_POINT ( 'NONE',  ( 0.1532563361054100626, 50.80059781766745175, -2.638427012816831230 ) ) ;
#64341 = CARTESIAN_POINT ( 'NONE',  ( -1.099225684535947600, 29.54030133659708923, 6.408140936763237150 ) ) ;
#64343 = CARTESIAN_POINT ( 'NONE',  ( -6.000000000000000000, 78.07179676972447169, 6.500000000000000888 ) ) ;
#64342 = PRESENTATION_STYLE_ASSIGNMENT (( #1424 ) ) ;
#64344 = CARTESIAN_POINT ( 'NONE',  ( 7.084665262690076126, 57.02201867748817676, -10.88017736071110164 ) ) ;
#64345 = CARTESIAN_POINT ( 'NONE',  ( -4.164238869374099927, 67.01208216824728936, 3.795296366450308767 ) ) ;
#64346 = B_SPLINE_CURVE_WITH_KNOTS ( 'NONE', 3,
 ( #49722, #75692, #7708, #76188 ),
 .UNSPECIFIED., .F., .F.,
 ( 4, 4 ),
 ( 6.505213034913026604E-19, 0.001036303429213372230 ),
 .UNSPECIFIED. ) ;
#64347 = EDGE_CURVE ( 'NONE', #81215, #91503, #77390, .T. ) ;
#64348 = CARTESIAN_POINT ( 'NONE',  ( 21.09922568453594849, 36.20696800326375353, 6.408140936763242479 ) ) ;
#64349 = CARTESIAN_POINT ( 'NONE',  ( 7.084665262690076126, 34.10535201082151247, 10.88017736071109987 ) ) ;
#64350 = FACE_OUTER_BOUND ( 'NONE', #77033, .T. ) ;
#64351 = ORIENTED_EDGE ( 'NONE', *, *, #57701, .T. ) ;
#64352 = CARTESIAN_POINT ( 'NONE',  ( 6.565887622018943937, 45.16530133659708923, 12.81628187352647430 ) ) ;
#64353 = CARTESIAN_POINT ( 'NONE',  ( 20.88017736071110519, 30.56368534415484106, 2.639326808657452039E-16 ) ) ;
#64354 = EDGE_CURVE ( 'NONE', #92170, #55079, #61878, .T. ) ;
#64355 = ORIENTED_EDGE ( 'NONE', *, *, #21603, .T. ) ;
#64356 = CARTESIAN_POINT ( 'NONE',  ( 17.20831665107776587, 7.883931151000784787, 7.208316651077764980 ) ) ;
#64357 = CARTESIAN_POINT ( 'NONE',  ( 19.84674366389459266, 58.30059781766745886, 2.638427012816836559 ) ) ;
#64359 = CARTESIAN_POINT ( 'NONE',  ( 18.52753015748618282, 53.92559781766745175, -4.923371831947291888 ) ) ;
#64358 = CARTESIAN_POINT ( 'NONE',  ( 19.84674366389459266, 18.30059781766745175, 2.638427012816836559 ) ) ;
#64360 = CARTESIAN_POINT ( 'NONE',  ( -11.07412464642555250, -96.03934428903617970, 3.750000000000000888 ) ) ;
#64361 = FILL_AREA_STYLE ('',( #94377 ) ) ;
#64362 = CARTESIAN_POINT ( 'NONE',  ( -4.326345305608602310, 0.000000000000000000, -3.319721512309643074 ) ) ;
#64363 = CARTESIAN_POINT ( 'NONE',  ( -8.000000000000000000, 75.73428692542562146, 3.000000000000000000 ) ) ;
#64364 = AXIS2_PLACEMENT_3D ( 'NONE', #74116, #11659, #57644 ) ;
#64366 = CARTESIAN_POINT ( 'NONE',  ( -6.000000000000009770, 40.74999999999999289, -4.000000000000000000 ) ) ;
#64365 = CARTESIAN_POINT ( 'NONE',  ( 0.1532563361054082862, 31.21726448433412315, 2.638427012816831674 ) ) ;
#64367 = DIRECTION ( 'NONE',  ( 0.000000000000000000, 0.000000000000000000, 1.000000000000000000 ) ) ;
#64369 = ORIENTED_EDGE ( 'NONE', *, *, #34526, .T. ) ;
#64368 = CARTESIAN_POINT ( 'NONE',  ( 14.92337183194729633, 57.67559781766745886, 8.527530157486181039 ) ) ;
#64370 = AXIS2_PLACEMENT_3D ( 'NONE', #9161, #32641, #19977 ) ;
#64371 = LINE ( 'NONE', #17429, #66108 ) ;
#64372 = CARTESIAN_POINT ( 'NONE',  ( 21.09922568453594849, 26.20696800326375353, 6.408140936763242479 ) ) ;
#64373 = CARTESIAN_POINT ( 'NONE',  ( 14.92337183194729988, 44.34226448433412315, -8.527530157486177487 ) ) ;
#64374 = LINE ( 'NONE', #2443, #88813 ) ;
#64375 = CARTESIAN_POINT ( 'NONE',  ( -4.164238869374099927, 57.01208216824731068, 3.795296366450308767 ) ) ;
#64376 = CARTESIAN_POINT ( 'NONE',  ( 18.52753015748617571, 18.09226448433411960, 4.923371831947298993 ) ) ;
#64377 = CARTESIAN_POINT ( 'NONE',  ( 19.65571488900285502, 85.77913566376845722, 5.360955758210749877 ) ) ;
#64378 = CARTESIAN_POINT ( 'NONE',  ( -0.3689425029237881626, 52.42874883491396076, 10.36894250292379027 ) ) ;
#64379 = CARTESIAN_POINT ( 'NONE',  ( 12.63842701281683034, 57.46726448433411605, 9.846743663894596210 ) ) ;
#64380 = CARTESIAN_POINT ( 'NONE',  ( -2.266590686148945544, 66.38708216824730357, -7.082119434687050408 ) ) ;
#64381 = CARTESIAN_POINT ( 'NONE',  ( -0.3689425029237881626, 32.42874883491395366, 10.36894250292379027 ) ) ;
#64382 = CARTESIAN_POINT ( 'NONE',  ( -2.266590686148945544, 42.22041550158063217, 7.082119434687048631 ) ) ;
#64383 = DIRECTION ( 'NONE',  ( -0.000000000000000000, -0.000000000000000000, 1.000000000000000000 ) ) ;
#64385 = CARTESIAN_POINT ( 'NONE',  ( 5.076628168052704559, 50.17559781766745886, -8.527530157486179263 ) ) ;
#64384 = LINE ( 'NONE', #87396, #16612 ) ;
#64386 = CARTESIAN_POINT ( 'NONE',  ( 0.5774900079438590739, 32.64701867748816966, -5.440088680355550821 ) ) ;
#64387 = CARTESIAN_POINT ( 'NONE',  ( 11.35674369515838933, -65.10150209588266534, 3.750000000000001332 ) ) ;
#64388 = EDGE_CURVE ( 'NONE', #50974, #8774, #73750, .T. ) ;
#64389 = CARTESIAN_POINT ( 'NONE',  ( 19.84674366389459266, 53.30059781766744464, 2.638427012816836559 ) ) ;
#64390 = CARTESIAN_POINT ( 'NONE',  ( 17.41414817163570916, 33.99863903001854482, -9.761180582272329431 ) ) ;
#64391 = CARTESIAN_POINT ( 'NONE',  ( 3.469446951953614189E-15, 8.053748834913978527, 14.16423886937410259 ) ) ;
#64392 = CARTESIAN_POINT ( 'NONE',  ( 14.92337183194729988, 54.34226448433412315, -8.527530157486177487 ) ) ;
#64393 = CARTESIAN_POINT ( 'NONE',  ( 18.52753015748617571, 63.09226448433412315, 4.923371831947298993 ) ) ;
#64394 = ORIENTED_EDGE ( 'NONE', *, *, #27801, .T. ) ;
#64395 = TOROIDAL_SURFACE ( 'NONE', #90172, 2.799999999999999822, 0.2000000000000000111 ) ;
#64396 = CARTESIAN_POINT ( 'NONE',  ( 2.917880565312950480, 30.97041550158063572, -12.26659068614894821 ) ) ;
#64397 = CARTESIAN_POINT ( 'NONE',  ( -14.48718990079890290, 15.00000000000000000, 0.6093675230839377122 ) ) ;
#64399 = CARTESIAN_POINT ( 'NONE',  ( -10.76445796112971109, 15.00000000000000711, -9.901260316209995693 ) ) ;
#64398 = CARTESIAN_POINT ( 'NONE',  ( -3.770608837273494274, -6.399801140528821541, -2.500000000000403677 ) ) ;
#64401 = AXIS2_PLACEMENT_3D ( 'NONE', #9404, #70903, #74707 ) ;
#64400 = CARTESIAN_POINT ( 'NONE',  ( -0.8801773607111008646, 23.27201867748817676, 2.915334737309923430 ) ) ;
#64402 = CARTESIAN_POINT ( 'NONE',  ( 0.6178305044545818747, 18.49863466993041428, -9.382169495545419124 ) ) ;
#64403 = FACE_OUTER_BOUND ( 'NONE', #50709, .T. ) ;
#64404 = CARTESIAN_POINT ( 'NONE',  ( 2.791683348922237240, 10.38393115100078390, -7.208316651077763204 ) ) ;
#64405 = AXIS2_PLACEMENT_3D ( 'NONE', #70483, #55479, #32956 ) ;
#64406 = CARTESIAN_POINT ( 'NONE',  ( 6.905642986259637794, -69.45547628558860254, -3.750000000000000000 ) ) ;
#64407 = EDGE_CURVE ( 'NONE', #84535, #21097, #62130, .T. ) ;
#64408 = CARTESIAN_POINT ( 'NONE',  ( 20.36894250292379382, 28.67874883491396787, 10.36894250292379205 ) ) ;
#64409 = CARTESIAN_POINT ( 'NONE',  ( 20.15039907845753930, 0.07447313448805115144, -6.262539305110068177 ) ) ;
#64410 = FILL_AREA_STYLE ('',( #43391 ) ) ;
#64411 = CARTESIAN_POINT ( 'NONE',  ( -0.8801773607111009756, 8.063685344154837509, 1.068504757029289695E-15 ) ) ;
#64412 = DIRECTION ( 'NONE',  ( -3.286260152890462729E-14, 0.000000000000000000, 1.000000000000000000 ) ) ;
#64413 = CARTESIAN_POINT ( 'NONE',  ( 10.00000000000000000, 41.81368534415484106, -10.88017736071110342 ) ) ;
#64414 = CARTESIAN_POINT ( 'NONE',  ( 10.00000000000000178, 34.31368534415484106, 10.88017736071110342 ) ) ;
#64415 = CARTESIAN_POINT ( 'NONE',  ( 3.591859063236761518, -0.04303199673624671928, 11.09922568453594849 ) ) ;
#64416 = CARTESIAN_POINT ( 'NONE',  ( 1.472469842513823179, 65.59226448433412315, -4.923371831947296329 ) ) ;
#64417 = CARTESIAN_POINT ( 'NONE',  ( 10.00000000000000000, 4.758931151000784787, -9.846743663894594434 ) ) ;
#64418 = ORIENTED_EDGE ( 'NONE', *, *, #65634, .T. ) ;
#64419 = DIRECTION ( 'NONE',  ( 0.000000000000000000, 0.000000000000000000, -1.000000000000000000 ) ) ;
#64420 = CARTESIAN_POINT ( 'NONE',  ( 15.44008868035555260, 44.73035201082151247, 9.422509992056143702 ) ) ;
#64421 = UNCERTAINTY_MEASURE_WITH_UNIT (LENGTH_MEASURE( 1.000000000000000082E-05 ), #90700, 'distance_accuracy_value', 'NONE');
#64422 = CARTESIAN_POINT ( 'NONE',  ( 22.81628187352647785, 11.62363466993042138, 6.195893100308588602E-16 ) ) ;
#64423 = CARTESIAN_POINT ( 'NONE',  ( 7.084665262690076126, 57.02201867748817676, -10.88017736071110164 ) ) ;
#64424 = CARTESIAN_POINT ( 'NONE',  ( 1.472469842513823179, 25.59226448433412315, -4.923371831947296329 ) ) ;
#64425 = CARTESIAN_POINT ( 'NONE',  ( -2.816281873526473856, 39.12363466993041783, 9.499525473075851096E-16 ) ) ;
#64426 = CARTESIAN_POINT ( 'NONE',  ( 2.791683348922237240, 5.383931151000785675, -7.208316651077763204 ) ) ;
#64427 = ORIENTED_EDGE ( 'NONE', *, *, #96753, .T. ) ;
#64428 = B_SPLINE_CURVE_WITH_KNOTS ( 'NONE', 3,
 ( #50792, #10829, #81283, #35781, #86826, #94311 ),
 .UNSPECIFIED., .F., .F.,
 ( 4, 2, 4 ),
 ( 0.0002800086601589242097, 0.0006862139742844824888, 0.001092419288410040931 ),
 .UNSPECIFIED. ) ;
#64429 = DIRECTION ( 'NONE',  ( 1.000000000000000000, 0.000000000000000000, 0.000000000000000000 ) ) ;
#64430 = CARTESIAN_POINT ( 'NONE',  ( -10.29975640502598289, 43.93058911311638326, -2.900000000000000799 ) ) ;
#64431 = CARTESIAN_POINT ( 'NONE',  ( -0.8801773607110991993, 7.855352010821504471, -2.915334737309923874 ) ) ;
#64432 = CARTESIAN_POINT ( 'NONE',  ( 21.09922568453595559, 62.04030133659709634, -6.408140936763230044 ) ) ;
#64433 = CARTESIAN_POINT ( 'NONE',  ( 1.472469842513823179, 20.59226448433411960, -4.923371831947296329 ) ) ;
#64434 = CARTESIAN_POINT ( 'NONE',  ( -0.8801773607110991993, 2.855352010821504471, -2.915334737309923874 ) ) ;
#64435 = CARTESIAN_POINT ( 'NONE',  ( 10.00000000000000178, 9.313685344154839285, 10.88017736071110342 ) ) ;
#64436 = VERTEX_POINT ( 'NONE', #60407 ) ;
#64437 = CARTESIAN_POINT ( 'NONE',  ( -0.8801773607111008646, 8.272018677488171434, 2.915334737309923430 ) ) ;
#64438 = ADVANCED_FACE ( 'NONE', ( #14436 ), #63378, .T. ) ;
#64439 = CARTESIAN_POINT ( 'NONE',  ( 17.96484262340118221, 16.18868534415483396, -7.964842623401177768 ) ) ;
#64440 = FACE_OUTER_BOUND ( 'NONE', #31902, .T. ) ;
#64441 = ORIENTED_EDGE ( 'NONE', *, *, #734, .F. ) ;
#64442 = CARTESIAN_POINT ( 'NONE',  ( 14.92337183194729988, 64.34226448433412315, -8.527530157486177487 ) ) ;
#64443 = CARTESIAN_POINT ( 'NONE',  ( 0.5774900079438590739, 22.64701867748817321, -5.440088680355550821 ) ) ;
#64444 = CARTESIAN_POINT ( 'NONE',  ( 0.1532563361054082862, 61.21726448433412315, 2.638427012816831674 ) ) ;
#64445 = DIRECTION ( 'NONE',  ( 0.000000000000000000, -1.000000000000000000, 0.000000000000000000 ) ) ;
#64446 = CARTESIAN_POINT ( 'NONE',  ( 16.40814093676323893, 50.79030133659708923, 11.09922568453595026 ) ) ;
#64447 = CARTESIAN_POINT ( 'NONE',  ( -0.1503990784575323369, 4.248846992468888750, -6.262539305110070842 ) ) ;
#64448 = CARTESIAN_POINT ( 'NONE',  ( 20.36894250292379382, 28.67874883491396787, 10.36894250292379205 ) ) ;
#64449 = CARTESIAN_POINT ( 'NONE',  ( 17.96484262340118221, 44.93868534415483396, 7.964842623401181321 ) ) ;
#64450 = CARTESIAN_POINT ( 'NONE',  ( 20.88017736071110519, 20.56368534415484106, 2.639326808657452039E-16 ) ) ;
#64451 = EDGE_CURVE ( 'NONE', #36584, #49358, #72182, .T. ) ;
#64452 = CARTESIAN_POINT ( 'NONE',  ( 12.63842701281683922, 59.55059781766744464, -9.846743663894590881 ) ) ;
#64453 = CARTESIAN_POINT ( 'NONE',  ( -3.927832320392065313, 15.00000000000000000, -13.69797916712109398 ) ) ;
#64454 = CARTESIAN_POINT ( 'NONE',  ( 2.791683348922240793, 51.63393115100078745, 7.208316651077764092 ) ) ;
#64455 = CARTESIAN_POINT ( 'NONE',  ( 7.361572987183170547, 2.050597817667451750, 9.846743663894590881 ) ) ;
#64456 = CARTESIAN_POINT ( 'NONE',  ( 11.09922568453595026, -28.79303199673624292, 6.408140936763232709 ) ) ;
#64457 = ORIENTED_EDGE ( 'NONE', *, *, #2547, .T. ) ;
#64458 = B_SPLINE_CURVE_WITH_KNOTS ( 'NONE', 3,
 ( #32898, #78402, #9921, #85919, #57369, #63395 ),
 .UNSPECIFIED., .F., .F.,
 ( 4, 2, 4 ),
 ( 3.409110551475976050E-05, 0.0004400426677365986252, 0.0008459942299584374695 ),
 .UNSPECIFIED. ) ;
#64459 = CARTESIAN_POINT ( 'NONE',  ( 0.5774900079438607392, 18.48035201082150536, 5.440088680355550821 ) ) ;
#64460 = CARTESIAN_POINT ( 'NONE',  ( 19.84674366389459266, 13.71726448433411782, -2.638427012816827677 ) ) ;
#64461 = ADVANCED_FACE ( 'NONE', ( #87236 ), #75400, .T. ) ;
#64462 = CARTESIAN_POINT ( 'NONE',  ( 6.565887622018943937, -1.918031996736246692, -12.81628187352647608 ) ) ;
#64463 = CARTESIAN_POINT ( 'NONE',  ( 17.96484262340118221, 51.18868534415483396, -7.964842623401177768 ) ) ;
#64465 = CARTESIAN_POINT ( 'NONE',  ( 21.09922568453594849, 46.20696800326376064, 6.408140936763242479 ) ) ;
#64464 = CARTESIAN_POINT ( 'NONE',  ( 17.96484262340118221, 26.18868534415483396, -7.964842623401177768 ) ) ;
#64466 = CARTESIAN_POINT ( 'NONE',  ( 10.00000000000000178, 38.05374883491396787, 14.16423886937410082 ) ) ;
#64467 = CARTESIAN_POINT ( 'NONE',  ( -14.97687855664607781, 0.3640475087720984604, -0.8325315005902566012 ) ) ;
#64468 = VECTOR ( 'NONE', #63208, 1000.000000000000000 ) ;
#64469 = CARTESIAN_POINT ( 'NONE',  ( 13.43411237798105340, 55.58196800326374643, 12.81628187352647963 ) ) ;
#64470 = ORIENTED_EDGE ( 'NONE', *, *, #79044, .F. ) ;
#64471 = CARTESIAN_POINT ( 'NONE',  ( 19.84674366389459266, 53.30059781766744464, 2.638427012816836559 ) ) ;
#64472 = CARTESIAN_POINT ( 'NONE',  ( 19.42250999205614193, 35.14701867748816966, 5.440088680355555262 ) ) ;
#64473 = EDGE_CURVE ( 'NONE', #65586, #27193, #17777, .T. ) ;
#64474 = ORIENTED_EDGE ( 'NONE', *, *, #44628, .F. ) ;
#64476 = CARTESIAN_POINT ( 'NONE',  ( -4.285591316845102305, -17.54293119412275104, 2.499999999999998668 ) ) ;
#64475 = CARTESIAN_POINT ( 'NONE',  ( 1.472469842513823179, 6.425597817667451750, 4.923371831947296329 ) ) ;
#64477 = CARTESIAN_POINT ( 'NONE',  ( 2.791683348922240793, 26.63393115100078745, 7.208316651077764092 ) ) ;
#64478 = CARTESIAN_POINT ( 'NONE',  ( 1.472469842513823179, 5.592264484334118713, -4.923371831947296329 ) ) ;
#64479 = CARTESIAN_POINT ( 'NONE',  ( 14.92337183194729988, 4.342264484334117824, -8.527530157486177487 ) ) ;
#64481 =( NAMED_UNIT ( * ) PLANE_ANGLE_UNIT ( ) SI_UNIT ( $, .RADIAN. ) );
#64480 = CARTESIAN_POINT ( 'NONE',  ( 0.5774900079438607392, 63.48035201082149825, 5.440088680355550821 ) ) ;
#64482 = CARTESIAN_POINT ( 'NONE',  ( 19.42250999205614193, 60.14701867748817676, 5.440088680355555262 ) ) ;
#64484 = EDGE_LOOP ( 'NONE', ( #77749, #2663, #55762, #55751 ) ) ;
#64483 = CARTESIAN_POINT ( 'NONE',  ( 5.076628168052704559, 20.17559781766745175, -8.527530157486179263 ) ) ;
#64485 = DIRECTION ( 'NONE',  ( 0.000000000000000000, 0.000000000000000000, 1.000000000000000000 ) ) ;
#64486 = CARTESIAN_POINT ( 'NONE',  ( 7.361572987183169658, 54.96726448433413026, -9.846743663894592657 ) ) ;
#64487 = ORIENTED_EDGE ( 'NONE', *, *, #4236, .F. ) ;
#64488 = EDGE_LOOP ( 'NONE', ( #51306, #24487, #38543, #35287 ) ) ;
#64489 = CYLINDRICAL_SURFACE ( 'NONE', #95326, 0.5000000000000004441 ) ;
#64490 = CARTESIAN_POINT ( 'NONE',  ( -2.266590686148945544, 1.387082168247301128, -7.082119434687050408 ) ) ;
#64491 = UNCERTAINTY_MEASURE_WITH_UNIT (LENGTH_MEASURE( 1.000000000000000082E-05 ), #85888, 'distance_accuracy_value', 'NONE');
#64492 = DIRECTION ( 'NONE',  ( -0.000000000000000000, -0.000000000000000000, 1.000000000000000000 ) ) ;
#64493 = CARTESIAN_POINT ( 'NONE',  ( -0.3689425029237898834, 11.17874883491396787, -10.36894250292378850 ) ) ;
#64494 = CARTESIAN_POINT ( 'NONE',  ( -4.164238869374099927, 32.01208216824730357, 3.795296366450308767 ) ) ;
#64495 = CARTESIAN_POINT ( 'NONE',  ( 10.00000000000000178, 3.053748834913967425, 14.16423886937410082 ) ) ;
#64496 = CARTESIAN_POINT ( 'NONE',  ( 10.00000000000000000, 0.5537488349139675359, -14.16423886937410082 ) ) ;
#64497 = CARTESIAN_POINT ( 'NONE',  ( 19.42250999205614193, 35.14701867748816966, 5.440088680355555262 ) ) ;
#64498 =( LENGTH_UNIT ( ) NAMED_UNIT ( * ) SI_UNIT ( .MILLI., .METRE. ) );
#64499 = ORIENTED_EDGE ( 'NONE', *, *, #7243, .T. ) ;
#64500 = CARTESIAN_POINT ( 'NONE',  ( 18.52753015748618282, 13.92559781766745175, -4.923371831947291888 ) ) ;
#64502 = CARTESIAN_POINT ( 'NONE',  ( 10.00000000000000000, 19.75893115100078390, -9.846743663894594434 ) ) ;
#64501 = CARTESIAN_POINT ( 'NONE',  ( 20.88017736071110519, 50.56368534415484106, 2.639326808657452039E-16 ) ) ;
#64503 = CARTESIAN_POINT ( 'NONE',  ( 16.40814093676324603, 47.45696800326375353, -11.09922568453594671 ) ) ;
#64504 = CARTESIAN_POINT ( 'NONE',  ( 2.791683348922237240, 40.38393115100078035, -7.208316651077763204 ) ) ;
#64505 = CARTESIAN_POINT ( 'NONE',  ( 11.48952521350024192, 4.570664323179305100E-16, -8.845383562533745803 ) ) ;
#64506 = ADVANCED_FACE ( 'NONE', ( #72712 ), #26734, .F. ) ;
#64507 = CARTESIAN_POINT ( 'NONE',  ( 15.44008868035555793, 61.39701867748817676, -9.422509992056140149 ) ) ;
#64508 = CARTESIAN_POINT ( 'NONE',  ( 21.09922568453594849, 31.20696800326375353, 6.408140936763242479 ) ) ;
#64509 = CARTESIAN_POINT ( 'NONE',  ( -12.26659068614895354, -38.61291783175269643, -7.082119434687038861 ) ) ;
#64510 = CARTESIAN_POINT ( 'NONE',  ( 19.84674366389459266, 28.71726448433411960, -2.638427012816827677 ) ) ;
#64511 = CARTESIAN_POINT ( 'NONE',  ( 17.08211943468705840, 15.13708216824730179, -12.26659068614894466 ) ) ;
#64512 = EDGE_LOOP ( 'NONE', ( #2280, #66813, #12889, #57478 ) ) ;
#64513 = CARTESIAN_POINT ( 'NONE',  ( 17.96484262340118221, 41.18868534415484106, -7.964842623401177768 ) ) ;
#64514 = CARTESIAN_POINT ( 'NONE',  ( 19.42250999205614193, 50.14701867748817676, 5.440088680355555262 ) ) ;
#64515 = CARTESIAN_POINT ( 'NONE',  ( 10.00000000000000178, 43.05374883491397497, 14.16423886937410082 ) ) ;
#64516 = CARTESIAN_POINT ( 'NONE',  ( 18.52753015748617571, 53.09226448433412315, 4.923371831947298993 ) ) ;
#64517 = CARTESIAN_POINT ( 'NONE',  ( 14.92337183194729633, 7.675597817667451750, 8.527530157486181039 ) ) ;
#64519 = DIRECTION ( 'NONE',  ( 0.000000000000000000, 0.000000000000000000, -1.000000000000000000 ) ) ;
#64518 = DIRECTION ( 'NONE',  ( -0.04361938736532633420, 0.000000000000000000, -0.9990482215818581313 ) ) ;
#64520 = CARTESIAN_POINT ( 'NONE',  ( 15.44008868035555793, 46.39701867748817676, -9.422509992056140149 ) ) ;
#64521 = CARTESIAN_POINT ( 'NONE',  ( 0.5600000000000083800, 105.0000000000000000, 5.000000000000000000 ) ) ;
#64522 = CARTESIAN_POINT ( 'NONE',  ( 6.565887622018943937, 23.08196800326375708, -12.81628187352647608 ) ) ;
#64523 = CARTESIAN_POINT ( 'NONE',  ( 16.40814093676324603, 22.45696800326375353, -11.09922568453594671 ) ) ;
#64524 = CARTESIAN_POINT ( 'NONE',  ( 18.52753015748617571, 53.09226448433412315, 4.923371831947298993 ) ) ;
#64525 = CARTESIAN_POINT ( 'NONE',  ( 7.964842623401181321, 14.93868534415484106, 7.964842623401174215 ) ) ;
#64526 = CARTESIAN_POINT ( 'NONE',  ( 0.5774900079438590739, 67.64701867748817676, -5.440088680355550821 ) ) ;
#64527 = CARTESIAN_POINT ( 'NONE',  ( 19.72487221294570858, 21.86607318730131411, 6.500000000000000888 ) ) ;
#64528 = CARTESIAN_POINT ( 'NONE',  ( 0.000000000000000000, 14.49999999999999822, 0.000000000000000000 ) ) ;
#64529 = CARTESIAN_POINT ( 'NONE',  ( 0.5774900079438590739, 62.64701867748817676, -5.440088680355550821 ) ) ;
#64530 = CARTESIAN_POINT ( 'NONE',  ( 10.00000000000000000, -0.2410688489992152128, -9.846743663894594434 ) ) ;
#64531 = CARTESIAN_POINT ( 'NONE',  ( 18.00000000000000000, 78.50170875364489120, -3.769097879698134257 ) ) ;
#64532 = TOROIDAL_SURFACE ( 'NONE', #93309, 2.899999999999999911, 0.1000000000000000056 ) ;
#64533 = CARTESIAN_POINT ( 'NONE',  ( 12.63842701281683034, 37.46726448433411605, 9.846743663894596210 ) ) ;
#64534 = CARTESIAN_POINT ( 'NONE',  ( 10.00000000000000178, 24.31368534415484106, 10.88017736071110342 ) ) ;
#64535 = CARTESIAN_POINT ( 'NONE',  ( -1.099225684535947600, -0.4596986634029132657, 6.408140936763237150 ) ) ;
#64537 = CARTESIAN_POINT ( 'NONE',  ( -8.838651438279397254, 14.95077488074853456, -11.81204219878349804 ) ) ;
#64536 = CARTESIAN_POINT ( 'NONE',  ( 10.00000000000000000, 31.81368534415483751, -10.88017736071110342 ) ) ;
#64538 =( NAMED_UNIT ( * ) SI_UNIT ( $, .STERADIAN. ) SOLID_ANGLE_UNIT ( ) );
#64539 = CARTESIAN_POINT ( 'NONE',  ( 3.591859063236761518, 44.95696800326376064, 11.09922568453594849 ) ) ;
#64540 = ORIENTED_EDGE ( 'NONE', *, *, #28646, .F. ) ;
#64541 = CARTESIAN_POINT ( 'NONE',  ( 2.035157376598822676, 52.43868534415483396, -7.964842623401177768 ) ) ;
#64542 = VECTOR ( 'NONE', #39954, 1000.000000000000000 ) ;
#64543 = CARTESIAN_POINT ( 'NONE',  ( 21.09922568453594849, 21.20696800326375353, 6.408140936763242479 ) ) ;
#64544 = CARTESIAN_POINT ( 'NONE',  ( 7.084665262690076126, 24.10535201082150181, 10.88017736071109987 ) ) ;
#64545 = CARTESIAN_POINT ( 'NONE',  ( -4.164238869374098151, 51.59541550158063217, -3.795296366450310543 ) ) ;
#64546 = CARTESIAN_POINT ( 'NONE',  ( 7.361572987183169658, 39.96726448433411605, -9.846743663894592657 ) ) ;
#64547 = CARTESIAN_POINT ( 'NONE',  ( 4.559911319644449179, 67.23035201082150536, -9.422509992056141925 ) ) ;
#64548 = CARTESIAN_POINT ( 'NONE',  ( 10.00000000000000000, -0.2410688489992152128, -9.846743663894594434 ) ) ;
#64549 = DIRECTION ( 'NONE',  ( 0.000000000000000000, 1.000000000000000000, 0.000000000000000000 ) ) ;
#64550 = CARTESIAN_POINT ( 'NONE',  ( 13.79529636645030344, 33.26208216824730357, 14.16423886937410614 ) ) ;
#64551 = DIRECTION ( 'NONE',  ( 0.000000000000000000, 0.000000000000000000, 1.000000000000000000 ) ) ;
#64552 = CARTESIAN_POINT ( 'NONE',  ( -14.47650479471822393, 14.49999999999999112, -3.928206833722243108 ) ) ;
#64554 = EDGE_LOOP ( 'NONE', ( #93730, #75834, #24133, #15204, #4233, #41387 ) ) ;
#64553 = EDGE_CURVE ( 'NONE', #67870, #55759, #6747, .T. ) ;
#64555 = ORIENTED_EDGE ( 'NONE', *, *, #47389, .T. ) ;
#64556 = CARTESIAN_POINT ( 'NONE',  ( 20.36894250292379382, 53.67874883491397497, 10.36894250292379205 ) ) ;
#64557 = CARTESIAN_POINT ( 'NONE',  ( -4.164238869374098151, 46.59541550158063927, -3.795296366450310543 ) ) ;
#64558 = CARTESIAN_POINT ( 'NONE',  ( 0.1532563361054082862, 11.21726448433411605, 2.638427012816831674 ) ) ;
#64559 = CARTESIAN_POINT ( 'NONE',  ( 3.591859063236761518, 14.95696800326375531, 11.09922568453594849 ) ) ;
#64560 = PLANE ( 'NONE',  #31559 ) ;
#64561 = DIRECTION ( 'NONE',  ( -0.9961946980917453232, 0.08715574274766037244, 0.000000000000000000 ) ) ;
#64562 = CARTESIAN_POINT ( 'NONE',  ( 19.38216949554541202, 35.99863466993041072, 9.382169495545424454 ) ) ;
#64563 = CARTESIAN_POINT ( 'NONE',  ( 13.79529636645030344, 48.26208216824728936, 14.16423886937410614 ) ) ;
#64564 = EDGE_CURVE ( 'NONE', #41967, #23012, #17887, .T. ) ;
#64565 = EDGE_CURVE ( 'NONE', #77740, #43585, #96236, .T. ) ;
#64566 = CARTESIAN_POINT ( 'NONE',  ( -13.21236992757677164, -0.03417435944610275333, 5.338143956176621074 ) ) ;
#64567 = SURFACE_STYLE_FILL_AREA ( #71119 ) ;
#64568 = CARTESIAN_POINT ( 'NONE',  ( -9.846743663894594434, 6.008931151000790116, 3.469446951953614189E-15 ) ) ;
#64569 = ORIENTED_EDGE ( 'NONE', *, *, #60822, .T. ) ;
#64570 = CARTESIAN_POINT ( 'NONE',  ( 19.84674366389459621, 13.50893115100078568, 7.409399052514197653E-17 ) ) ;
#64571 = DIRECTION ( 'NONE',  ( -0.000000000000000000, 0.000000000000000000, 1.000000000000000000 ) ) ;
#64572 = ORIENTED_EDGE ( 'NONE', *, *, #24511, .T. ) ;
#64573 = CARTESIAN_POINT ( 'NONE',  ( 13.79529636645031943, 15.34541550158063750, -14.16423886937409904 ) ) ;
#64575 = CARTESIAN_POINT ( 'NONE',  ( 17.96484262340118221, 6.188685344154837509, -7.964842623401177768 ) ) ;
#64574 = CARTESIAN_POINT ( 'NONE',  ( 20.88017736071110875, 10.77201867748817143, -2.915334737309920765 ) ) ;
#64577 = CARTESIAN_POINT ( 'NONE',  ( -2.816281873526473856, -0.8763653300695799508, 9.499525473075851096E-16 ) ) ;
#64576 = CARTESIAN_POINT ( 'NONE',  ( 19.84674366389459621, 53.50893115100078745, 7.409399052514197653E-17 ) ) ;
#64578 = EDGE_CURVE ( 'NONE', #71601, #36015, #95736, .T. ) ;
#64579 = DIRECTION ( 'NONE',  ( -0.000000000000000000, -1.000000000000000000, -0.000000000000000000 ) ) ;
#64580 = VECTOR ( 'NONE', #54354, 1000.000000000000000 ) ;
#64581 = CARTESIAN_POINT ( 'NONE',  ( 16.40814093676324603, 12.45696800326375353, -11.09922568453594671 ) ) ;
#64582 = ORIENTED_EDGE ( 'NONE', *, *, #94836, .T. ) ;
#64583 = CARTESIAN_POINT ( 'NONE',  ( 10.00000000000000000, 60.55374883491397497, -14.16423886937410082 ) ) ;
#64584 = EDGE_LOOP ( 'NONE', ( #75791, #44738, #43454, #56529 ) ) ;
#64585 = EDGE_CURVE ( 'NONE', #33221, #90159, #50214, .T. ) ;
#64586 = CARTESIAN_POINT ( 'NONE',  ( -2.266590686148945544, 61.38708216824730357, -7.082119434687050408 ) ) ;
#64587 = EDGE_LOOP ( 'NONE', ( #18661, #201, #54260, #21260, #85716 ) ) ;
#64588 = CARTESIAN_POINT ( 'NONE',  ( 10.00000000000000000, 36.81368534415484106, -10.88017736071110342 ) ) ;
#64589 = CARTESIAN_POINT ( 'NONE',  ( 2.035157376598824452, 48.68868534415483396, 7.964842623401179544 ) ) ;
#64590 = CARTESIAN_POINT ( 'NONE',  ( -0.8801773607111009756, 38.06368534415484106, 1.068504757029289695E-15 ) ) ;
#64591 = CARTESIAN_POINT ( 'NONE',  ( 13.64884605730314426, 15.00000000000000000, -8.341846182955777067 ) ) ;
#64592 = CARTESIAN_POINT ( 'NONE',  ( 19.42250999205614548, 45.98035201082150536, -5.440088680355545492 ) ) ;
#64593 = DIRECTION ( 'NONE',  ( -1.000000000000000000, 0.000000000000000000, 0.000000000000000000 ) ) ;
#64594 = CARTESIAN_POINT ( 'NONE',  ( 7.361572987183169658, 14.96726448433411960, -9.846743663894592657 ) ) ;
#64595 = EDGE_LOOP ( 'NONE', ( #3250, #95881, #40096, #84643 ) ) ;
#64596 = DIRECTION ( 'NONE',  ( 0.9999509640662961329, 0.009903002720634834083, 0.000000000000000000 ) ) ;
#64597 = CARTESIAN_POINT ( 'NONE',  ( 0.1532563361054083140, 51.00893115100078745, 1.131784320476157264E-15 ) ) ;
#64598 = CIRCLE ( 'NONE', #59832, 14.49999999999999822 ) ;
#64599 = DIRECTION ( 'NONE',  ( 0.000000000000000000, -1.000000000000000000, 0.000000000000000000 ) ) ;
#64600 = CARTESIAN_POINT ( 'NONE',  ( 16.40814093676324603, 52.45696800326375353, -11.09922568453594671 ) ) ;
#64601 = CIRCLE ( 'NONE', #21536, 15.00000000000000000 ) ;
#64602 = LINE ( 'NONE', #87613, #1219 ) ;
#64603 = ORIENTED_EDGE ( 'NONE', *, *, #84233, .T. ) ;
#64604 = CARTESIAN_POINT ( 'NONE',  ( -46.30928139467843607, 104.0823827281712255, 5.529860068218146019 ) ) ;
#64605 = CARTESIAN_POINT ( 'NONE',  ( -7.079946287805722882, -69.52844923516938991, 3.749999999999999112 ) ) ;
#64606 = SURFACE_STYLE_FILL_AREA ( #34114 ) ;
#64607 = CARTESIAN_POINT ( 'NONE',  ( 13.79529636645031943, 65.34541550158063217, -14.16423886937409904 ) ) ;
#64608 = DIRECTION ( 'NONE',  ( 0.000000000000000000, 1.000000000000000000, 0.000000000000000000 ) ) ;
#64609 = EDGE_LOOP ( 'NONE', ( #50309, #39455, #62811, #62864, #58358, #23581 ) ) ;
#64610 = DIRECTION ( 'NONE',  ( -0.000000000000000000, -1.000000000000000000, -0.000000000000000000 ) ) ;
#64611 = CARTESIAN_POINT ( 'NONE',  ( 19.84674366389459266, 38.71726448433412315, -2.638427012816827677 ) ) ;
#64612 = CARTESIAN_POINT ( 'NONE',  ( 22.81628187352647785, 61.41530133659709634, 3.434112377981063169 ) ) ;
#64613 = CARTESIAN_POINT ( 'NONE',  ( 19.38216949554541202, 10.99863466993042138, 9.382169495545424454 ) ) ;
#64614 = CARTESIAN_POINT ( 'NONE',  ( 17.96484262340118221, 64.93868534415483396, 7.964842623401181321 ) ) ;
#64615 = CARTESIAN_POINT ( 'NONE',  ( 19.84674366389459266, 13.71726448433411782, -2.638427012816827677 ) ) ;
#64616 = CARTESIAN_POINT ( 'NONE',  ( 17.20831665107776587, 59.13393115100078745, -7.208316651077762316 ) ) ;
#64617 = DIRECTION ( 'NONE',  ( -0.000000000000000000, -0.000000000000000000, -1.000000000000000000 ) ) ;
#64618 = STYLED_ITEM ( 'NONE', ( #21384 ), #6645 ) ;
#64619 = ORIENTED_EDGE ( 'NONE', *, *, #83673, .T. ) ;
#64620 = CARTESIAN_POINT ( 'NONE',  ( -0.8801773607111009756, 3.063685344154838397, 1.068504757029289695E-15 ) ) ;
#64621 = DIRECTION ( 'NONE',  ( 1.000000000000000000, 0.000000000000000000, 0.000000000000000000 ) ) ;
#64622 = CARTESIAN_POINT ( 'NONE',  ( 2.035157376598822676, 37.43868534415484106, -7.964842623401177768 ) ) ;
#64624 = CARTESIAN_POINT ( 'NONE',  ( 7.084665262690076126, 67.02201867748817676, -10.88017736071110164 ) ) ;
#64623 = CARTESIAN_POINT ( 'NONE',  ( -2.816281873526473856, 29.33196800326376064, 3.434112377981055619 ) ) ;
#64625 = CARTESIAN_POINT ( 'NONE',  ( -14.82269085861172364, 14.49999999999999112, -2.299529454047143595 ) ) ;
#64626 = PLANE ( 'NONE',  #42163 ) ;
#64627 = DIRECTION ( 'NONE',  ( -1.000000000000000000, 0.000000000000000000, 0.000000000000000000 ) ) ;
#64628 = CARTESIAN_POINT ( 'NONE',  ( 19.84674366389459266, 53.71726448433411605, -2.638427012816827677 ) ) ;
#64629 = CARTESIAN_POINT ( 'NONE',  ( 0.1532563361054100626, 20.80059781766744464, -2.638427012816831230 ) ) ;
#64630 = CARTESIAN_POINT ( 'NONE',  ( 2.915334737309921209, -18.39464798917849109, -10.88017736071110164 ) ) ;
#64631 = CARTESIAN_POINT ( 'NONE',  ( 13.43411237798105340, 20.58196800326374643, 12.81628187352647963 ) ) ;
#64632 = DIRECTION ( 'NONE',  ( 1.000000000000000000, 0.000000000000000000, 0.000000000000000000 ) ) ;
#64634 = CARTESIAN_POINT ( 'NONE',  ( 8.439016546559821919, 3.791394052158136007E-16, 11.79122553964979048 ) ) ;
#64633 = CARTESIAN_POINT ( 'NONE',  ( 19.42250999205614548, 30.98035201082150536, -5.440088680355545492 ) ) ;
#64635 = CARTESIAN_POINT ( 'NONE',  ( -6.767445849361066301, 0.5000000000000004441, -13.38662304974505801 ) ) ;
#64637 = EDGE_CURVE ( 'NONE', #2203, #70379, #78763, .T. ) ;
#64636 = AXIS2_PLACEMENT_3D ( 'NONE', #56612, #65070, #12581 ) ;
#64638 = CARTESIAN_POINT ( 'NONE',  ( 17.08211943468705840, 50.13708216824730357, -12.26659068614894466 ) ) ;
#64639 = CARTESIAN_POINT ( 'NONE',  ( 10.00000000000000000, 35.55374883491396787, -14.16423886937410082 ) ) ;
#64640 = CARTESIAN_POINT ( 'NONE',  ( 10.00000000000000000, 39.75893115100078745, -9.846743663894594434 ) ) ;
#64641 = CARTESIAN_POINT ( 'NONE',  ( -2.816281873526471635, 33.91530133659708213, -3.434112377981056508 ) ) ;
#64642 = CARTESIAN_POINT ( 'NONE',  ( 0.5774900079438590739, 22.64701867748817321, -5.440088680355550821 ) ) ;
#64643 = CARTESIAN_POINT ( 'NONE',  ( 19.84674366389459266, 53.30059781766744464, 2.638427012816836559 ) ) ;
#64644 = CARTESIAN_POINT ( 'NONE',  ( 15.44008868035555793, 36.39701867748816966, -9.422509992056140149 ) ) ;
#64645 = CARTESIAN_POINT ( 'NONE',  ( -1.099225684535947600, 4.540301336597087456, 6.408140936763237150 ) ) ;
#64646 = CARTESIAN_POINT ( 'NONE',  ( -0.3689425029237898834, 16.17874883491396076, -10.36894250292378850 ) ) ;
#64647 = CARTESIAN_POINT ( 'NONE',  ( -14.94699059465099822, 14.49999999999999822, -1.259949270175015013 ) ) ;
#64648 = CARTESIAN_POINT ( 'NONE',  ( 2.791683348922237240, 30.38393115100078390, -7.208316651077763204 ) ) ;
#64649 = CARTESIAN_POINT ( 'NONE',  ( 10.00000000000000000, 1.813685344154837731, -10.88017736071110342 ) ) ;
#64650 = CARTESIAN_POINT ( 'NONE',  ( 0.6178305044545838731, 4.748634669930420493, 9.382169495545420901 ) ) ;
#64651 = EDGE_LOOP ( 'NONE', ( #40274, #61775, #55666, #83309 ) ) ;
#64652 = CARTESIAN_POINT ( 'NONE',  ( 0.2751277870542967463, 0.000000000000000000, 6.500000000000000888 ) ) ;
#64653 = CARTESIAN_POINT ( 'NONE',  ( 4.380000000000000782, 1.019547802438464545, 2.750000000000000000 ) ) ;
#64654 = CARTESIAN_POINT ( 'NONE',  ( -0.3689425029237898834, 61.17874883491396076, -10.36894250292378850 ) ) ;
#64655 = CARTESIAN_POINT ( 'NONE',  ( 13.79529636645031943, 5.345415501580634832, -14.16423886937409904 ) ) ;
#64656 = CARTESIAN_POINT ( 'NONE',  ( 1.472469842513823179, 6.425597817667451750, 4.923371831947296329 ) ) ;
#64657 = CARTESIAN_POINT ( 'NONE',  ( 0.1532563361054100626, 45.80059781766745886, -2.638427012816831230 ) ) ;
#64658 = CARTESIAN_POINT ( 'NONE',  ( -0.8801773607111008646, 38.27201867748816255, 2.915334737309923430 ) ) ;
#64659 = CARTESIAN_POINT ( 'NONE',  ( 24.35999999999999233, 44.99999999999997158, 9.500000000000000000 ) ) ;
#64660 = CARTESIAN_POINT ( 'NONE',  ( 2.791683348922237240, 65.38393115100078035, -7.208316651077763204 ) ) ;
#64661 = ADVANCED_FACE ( 'NONE', ( #79744 ), #88166, .T. ) ;
#64662 = ORIENTED_EDGE ( 'NONE', *, *, #81605, .F. ) ;
#64663 = CARTESIAN_POINT ( 'NONE',  ( -4.850115630859501259, 0.04922511925147174394, -13.93278430610814844 ) ) ;
#64665 = VERTEX_POINT ( 'NONE', #58709 ) ;
#64664 = EDGE_CURVE ( 'NONE', #71742, #11450, #74703, .T. ) ;
#64666 = ORIENTED_EDGE ( 'NONE', *, *, #92728, .F. ) ;
#64667 = CARTESIAN_POINT ( 'NONE',  ( -6.000000000000014211, 80.07179676972448590, 6.250000000000000000 ) ) ;
#64668 = CARTESIAN_POINT ( 'NONE',  ( -4.164238869374099927, 2.012082168247300906, 3.795296366450308767 ) ) ;
#64669 = CARTESIAN_POINT ( 'NONE',  ( 24.16423886937410614, 9.303748834913967869, 8.672049930838204340E-16 ) ) ;
#64670 = AXIS2_PLACEMENT_3D ( 'NONE', #53318, #76807, #89233 ) ;
#64671 = CARTESIAN_POINT ( 'NONE',  ( 13.79529636645030344, 53.26208216824730357, 14.16423886937410614 ) ) ;
#64672 = CARTESIAN_POINT ( 'NONE',  ( 2.791683348922240793, 56.63393115100078035, 7.208316651077764092 ) ) ;
#64673 = CARTESIAN_POINT ( 'NONE',  ( 2.791683348922237240, 35.38393115100079456, -7.208316651077763204 ) ) ;
#64674 = DIRECTION ( 'NONE',  ( -6.938893903907222067E-15, 0.000000000000000000, -1.000000000000000000 ) ) ;
#64676 = CARTESIAN_POINT ( 'NONE',  ( 19.84674366389459266, 63.30059781766745886, 2.638427012816836559 ) ) ;
#64675 = CARTESIAN_POINT ( 'NONE',  ( 19.42250999205614193, 35.14701867748816966, 5.440088680355555262 ) ) ;
#64677 = CARTESIAN_POINT ( 'NONE',  ( 6.204703633549690345, 7.845415501580634832, 14.16423886937410082 ) ) ;
#64678 = CARTESIAN_POINT ( 'NONE',  ( 2.917880565312948704, 57.63708216824731068, 12.26659068614894643 ) ) ;
#64679 = VECTOR ( 'NONE', #17306, 1000.000000000000000 ) ;
#64680 = EDGE_CURVE ( 'NONE', #93630, #80446, #16814, .T. ) ;
#64681 = CARTESIAN_POINT ( 'NONE',  ( 4.559911319644449179, 2.230352010821504916, -9.422509992056141925 ) ) ;
#64682 = CARTESIAN_POINT ( 'NONE',  ( 5.000000000000000000, -2.909297654740273256E-16, -7.000000000000000000 ) ) ;
#64683 = CARTESIAN_POINT ( 'NONE',  ( 4.559911319644449179, 67.23035201082150536, -9.422509992056141925 ) ) ;
#64684 = CARTESIAN_POINT ( 'NONE',  ( 12.63842701281683922, 34.55059781766745886, -9.846743663894590881 ) ) ;
#64685 = CARTESIAN_POINT ( 'NONE',  ( -8.527530157486173934, -33.57440218233254114, 4.923371831947302546 ) ) ;
#64686 = ORIENTED_EDGE ( 'NONE', *, *, #16941, .F. ) ;
#64687 = FILL_AREA_STYLE_COLOUR ( '', #82685 ) ;
#64688 = ORIENTED_EDGE ( 'NONE', *, *, #46498, .T. ) ;
#64689 = CARTESIAN_POINT ( 'NONE',  ( 17.20831665107776587, 17.88393115100078745, 7.208316651077764980 ) ) ;
#64690 = ORIENTED_EDGE ( 'NONE', *, *, #73384, .T. ) ;
#64691 = CARTESIAN_POINT ( 'NONE',  ( -0.3689425029237898834, 36.17874883491396787, -10.36894250292378850 ) ) ;
#64692 = CARTESIAN_POINT ( 'NONE',  ( 17.20831665107776587, 37.88393115100078745, 7.208316651077764980 ) ) ;
#64693 = CARTESIAN_POINT ( 'NONE',  ( 12.91533473730992121, 54.52201867748816255, 10.88017736071110164 ) ) ;
#64694 = CARTESIAN_POINT ( 'NONE',  ( 15.44008868035555793, 51.39701867748816966, -9.422509992056140149 ) ) ;
#64695 = CARTESIAN_POINT ( 'NONE',  ( 7.361572987183169658, 44.96726448433412315, -9.846743663894592657 ) ) ;
#64696 = CARTESIAN_POINT ( 'NONE',  ( 22.81628187352647785, 61.62363466993041783, 6.195893100308588602E-16 ) ) ;
#64697 = CARTESIAN_POINT ( 'NONE',  ( -9.382169495545413795, 14.74863466993041961, 9.382169495545428006 ) ) ;
#64698 = ORIENTED_EDGE ( 'NONE', *, *, #54443, .F. ) ;
#64699 = CARTESIAN_POINT ( 'NONE',  ( 0.5774900079438607392, 48.48035201082150536, 5.440088680355550821 ) ) ;
#64700 = CARTESIAN_POINT ( 'NONE',  ( -4.164238869374099039, 26.80374883491397142, 8.674139862899312516E-16 ) ) ;
#64701 = VERTEX_POINT ( 'NONE', #21719 ) ;
#64702 = EDGE_CURVE ( 'NONE', #86853, #27481, #81216, .T. ) ;
#64703 = VERTEX_POINT ( 'NONE', #28704 ) ;
#64704 = CARTESIAN_POINT ( 'NONE',  ( 0.6178305044545838731, 24.74863466993042493, 9.382169495545420901 ) ) ;
#64705 = DIRECTION ( 'NONE',  ( 1.000000000000000000, 0.000000000000000000, 0.000000000000000000 ) ) ;
#64706 = CARTESIAN_POINT ( 'NONE',  ( 12.63842701281683034, 17.46726448433411250, 9.846743663894596210 ) ) ;
#64707 = CARTESIAN_POINT ( 'NONE',  ( 19.42250999205614193, 5.147018677488171434, 5.440088680355555262 ) ) ;
#64708 = DIRECTION ( 'NONE',  ( -0.000000000000000000, 0.000000000000000000, 1.000000000000000000 ) ) ;
#64709 = CARTESIAN_POINT ( 'NONE',  ( 19.84674366389459266, 33.71726448433410894, -2.638427012816827677 ) ) ;
#64710 = COLOUR_RGB ( '', 0.08235294, 0.09019608, 0.10196078) ;
#64711 = ADVANCED_FACE ( 'NONE', ( #97236 ), #81699, .F. ) ;
#64712 = CARTESIAN_POINT ( 'NONE',  ( 4.559911319644449179, 67.23035201082150536, -9.422509992056141925 ) ) ;
#64713 = STYLED_ITEM ( 'NONE', ( #59248 ), #49810 ) ;
#64714 = LINE ( 'NONE', #41276, #47874 ) ;
#64715 = CARTESIAN_POINT ( 'NONE',  ( 20.88017736071110519, 65.56368534415483396, 2.639326808657452039E-16 ) ) ;
#64716 = CARTESIAN_POINT ( 'NONE',  ( 19.05914839598885280, 29.96693863883976050, 6.499999999999962697 ) ) ;
#64717 = FACE_OUTER_BOUND ( 'NONE', #24187, .T. ) ;
#64718 = CARTESIAN_POINT ( 'NONE',  ( 12.63842701281683922, 4.550597817667451750, -9.846743663894590881 ) ) ;
#64719 = CARTESIAN_POINT ( 'NONE',  ( 3.591859063236763294, 28.29030133659708568, -11.09922568453595026 ) ) ;
#64720 = CYLINDRICAL_SURFACE ( 'NONE', #83485, 15.00000000000000000 ) ;
#64721 = CARTESIAN_POINT ( 'NONE',  ( 19.84674366389459266, 38.71726448433412315, -2.638427012816827677 ) ) ;
#64722 = CARTESIAN_POINT ( 'NONE',  ( 3.591859063236761518, 64.95696800326376774, 11.09922568453594849 ) ) ;
#64723 = CARTESIAN_POINT ( 'NONE',  ( -4.164238869374099039, 26.80374883491397142, 8.674139862899312516E-16 ) ) ;
#64724 = CARTESIAN_POINT ( 'NONE',  ( 1.472469842513823179, 26.42559781766745175, 4.923371831947296329 ) ) ;
#64725 = CARTESIAN_POINT ( 'NONE',  ( 22.81628187352648496, 26.83196800326374998, -3.434112377981050290 ) ) ;
#64727 = DIRECTION ( 'NONE',  ( 0.000000000000000000, -1.000000000000000000, 0.000000000000000000 ) ) ;
#64726 = FACE_OUTER_BOUND ( 'NONE', #66934, .T. ) ;
#64728 = CARTESIAN_POINT ( 'NONE',  ( -0.8801773607111008646, 58.27201867748816966, 2.915334737309923430 ) ) ;
#64729 = CARTESIAN_POINT ( 'NONE',  ( 0.6178305044545838731, 4.748634669930420493, 9.382169495545420901 ) ) ;
#64730 = CARTESIAN_POINT ( 'NONE',  ( 9.159723438033129383, -0.03417435944610275333, 10.91613331444548507 ) ) ;
#64731 = CARTESIAN_POINT ( 'NONE',  ( 2.791683348922237240, 35.38393115100079456, -7.208316651077763204 ) ) ;
#64732 = CARTESIAN_POINT ( 'NONE',  ( 0.5774900079438607392, 23.48035201082150536, 5.440088680355550821 ) ) ;
#64733 = CARTESIAN_POINT ( 'NONE',  ( 22.81628187352647785, 26.41530133659708923, 3.434112377981063169 ) ) ;
#64734 =( GEOMETRIC_REPRESENTATION_CONTEXT ( 3 ) GLOBAL_UNCERTAINTY_ASSIGNED_CONTEXT ( ( #91109 ) ) GLOBAL_UNIT_ASSIGNED_CONTEXT ( ( #88551, #96070, #87566 ) ) REPRESENTATION_CONTEXT ( 'NONE', 'WORKASPACE' ) );
#64735 = CARTESIAN_POINT ( 'NONE',  ( 10.00000000000000178, 22.25893115100078745, 9.846743663894594434 ) ) ;
#64736 =( BOUNDED_SURFACE ( )  B_SPLINE_SURFACE ( 3, 2, ( 
 ( #13546, #58542, #80567 ),
 ( #57069, #19078, #49553 ),
 ( #66546, #12557, #12062 ),
 ( #72553, #4582, #43539 ),
 ( #35552, #66041, #4084 ),
 ( #27550, #58044, #50556 ),
 ( #74035, #5565, #34549 ),
 ( #97074, #89543, #54005 ),
 ( #75028, #60519, #22541 ),
 ( #37044, #53013, #91010 ),
 ( #83032, #67542, #554 ),
 ( #90516, #29513, #98056 ),
 ( #16011, #38524, #60021 ),
 ( #22050, #52041, #44532 ),
 ( #15541, #82531, #30014 ),
 ( #38038, #69022, #83527 ),
 ( #84515, #52525, #14548 ),
 ( #45019, #15046, #77000 ),
 ( #45518, #68035, #75524 ),
 ( #90029, #14049, #7039 ),
 ( #29026, #91520, #46025 ),
 ( #76018, #37544, #7548 ) ),
 .UNSPECIFIED., .F., .F., .F. ) 
 B_SPLINE_SURFACE_WITH_KNOTS ( ( 4, 2, 2, 2, 2, 2, 2, 2, 2, 2, 4 ),
 ( 3, 3 ),
 ( 0.000000000000000000, 0.002789288213736775251, 0.005578576427473550502, 0.01115715285494710100, 0.02231430570989420201, 0.03347145856484130128, 0.04462861141978840401, 0.06694291712968260255, 0.07810006998462970529, 0.08367864641210326360, 0.08925722283957680803 ),
 ( 0.000000000000000000, 1.000000000000000000 ),
 .UNSPECIFIED. ) 
 GEOMETRIC_REPRESENTATION_ITEM ( )  RATIONAL_B_SPLINE_SURFACE ( (
 ( 1.000000000000000000, 0.7071067811865482389, 1.000000000000000000),
 ( 1.000000000000000000, 0.7071067811865482389, 1.000000000000000000),
 ( 1.000000000000000000, 0.7071067811865482389, 1.000000000000000000),
 ( 1.000000000000000000, 0.7071067811865482389, 1.000000000000000000),
 ( 1.000000000000000000, 0.7071067811865475727, 1.000000000000000000),
 ( 1.000000000000000000, 0.7071067811865475727, 1.000000000000000000),
 ( 1.000000000000000000, 0.7071067811865463515, 1.000000000000000000),
 ( 1.000000000000000000, 0.7071067811865463515, 1.000000000000000000),
 ( 1.000000000000000000, 0.7071067811865477948, 1.000000000000000000),
 ( 1.000000000000000000, 0.7071067811865477948, 1.000000000000000000),
 ( 1.000000000000000000, 0.7071067811865475727, 1.000000000000000000),
 ( 1.000000000000000000, 0.7071067811865475727, 1.000000000000000000),
 ( 1.000000000000000000, 0.7071067811865475727, 1.000000000000000000),
 ( 1.000000000000000000, 0.7071067811865475727, 1.000000000000000000),
 ( 1.000000000000000000, 0.7071067811865487940, 1.000000000000000000),
 ( 1.000000000000000000, 0.7071067811865487940, 1.000000000000000000),
 ( 1.000000000000000000, 0.7071067811865456854, 1.000000000000000000),
 ( 1.000000000000000000, 0.7071067811865456854, 1.000000000000000000),
 ( 1.000000000000000000, 0.7071067811865475727, 1.000000000000000000),
 ( 1.000000000000000000, 0.7071067811865475727, 1.000000000000000000),
 ( 1.000000000000000000, 0.7071067811865475727, 1.000000000000000000),
 ( 1.000000000000000000, 0.7071067811865475727, 1.000000000000000000) ) ) 
 REPRESENTATION_ITEM ( '' )  SURFACE ( )  );
#64737 = DIRECTION ( 'NONE',  ( -0.8610351672809766210, 0.4339697742547264370, -0.2651201156810288340 ) ) ;
#64738 = CARTESIAN_POINT ( 'NONE',  ( -13.01808377376653247, 90.72591000949749684, 7.552080394870894331 ) ) ;
#64739 = CARTESIAN_POINT ( 'NONE',  ( 20.88017736071110519, 35.56368534415484106, 2.639326808657452039E-16 ) ) ;
#64740 = AXIS2_PLACEMENT_3D ( 'NONE', #36228, #27237, #35731 ) ;
#64741 = ORIENTED_EDGE ( 'NONE', *, *, #13305, .T. ) ;
#64742 = CARTESIAN_POINT ( 'NONE',  ( 15.44008868035555260, 59.73035201082151247, 9.422509992056143702 ) ) ;
#64743 =( NAMED_UNIT ( * ) PLANE_ANGLE_UNIT ( ) SI_UNIT ( $, .RADIAN. ) );
#64745 = CARTESIAN_POINT ( 'NONE',  ( 7.084665262690076126, 29.10535201082150181, 10.88017736071109987 ) ) ;
#64744 = CARTESIAN_POINT ( 'NONE',  ( 14.92337183194729988, 44.34226448433412315, -8.527530157486177487 ) ) ;
#64746 = DIRECTION ( 'NONE',  ( 0.000000000000000000, 0.000000000000000000, 1.000000000000000000 ) ) ;
#64747 = CARTESIAN_POINT ( 'NONE',  ( 10.00000000000000178, 49.31368534415484106, 10.88017736071110342 ) ) ;
#64749 = CARTESIAN_POINT ( 'NONE',  ( 20.00000000000000711, 84.99347556686142013, -4.825407044038334980 ) ) ;
#64748 = CARTESIAN_POINT ( 'NONE',  ( 19.42250999205614193, 10.14701867748816966, 5.440088680355555262 ) ) ;
#64750 = LINE ( 'NONE', #95262, #51520 ) ;
#64751 = SURFACE_STYLE_FILL_AREA ( #20262 ) ;
#64752 = CARTESIAN_POINT ( 'NONE',  ( 18.52753015748618282, 53.92559781766745175, -4.923371831947291888 ) ) ;
#64754 = SURFACE_STYLE_FILL_AREA ( #49760 ) ;
#64753 = CARTESIAN_POINT ( 'NONE',  ( -2.266590686148945544, 57.22041550158063217, 7.082119434687048631 ) ) ;
#64755 = CARTESIAN_POINT ( 'NONE',  ( 12.58848565468353797, 2.439454888092384977E-16, 7.447709424579961990 ) ) ;
#64756 = EDGE_CURVE ( 'NONE', #11943, #96670, #25882, .T. ) ;
#64757 = CARTESIAN_POINT ( 'NONE',  ( 2.241241388159942801E-47, 3.851859888774471706E-31, 7.000000000000000000 ) ) ;
#64758 = CARTESIAN_POINT ( 'NONE',  ( -2.266590686148945544, 36.38708216824730357, -7.082119434687050408 ) ) ;
#64759 = FACE_OUTER_BOUND ( 'NONE', #91795, .T. ) ;
#64760 = ORIENTED_EDGE ( 'NONE', *, *, #68889, .F. ) ;
#64761 = CIRCLE ( 'NONE', #85565, 15.00000000000000000 ) ;
#64762 = CARTESIAN_POINT ( 'NONE',  ( 2.917880565312950480, 60.97041550158063927, -12.26659068614894821 ) ) ;
#64763 = CARTESIAN_POINT ( 'NONE',  ( 19.84674366389459266, 33.30059781766744464, 2.638427012816836559 ) ) ;
#64765 = CARTESIAN_POINT ( 'NONE',  ( -8.051923691749143686, 84.95650211105896688, -3.789018682291705797 ) ) ;
#64764 = DIRECTION ( 'NONE',  ( -0.000000000000000000, -1.000000000000000000, -0.000000000000000000 ) ) ;
#64766 = CARTESIAN_POINT ( 'NONE',  ( 15.44008868035555260, 64.73035201082151957, 9.422509992056143702 ) ) ;
#64767 = CARTESIAN_POINT ( 'NONE',  ( 6.565887622018943937, 65.16530133659709634, 12.81628187352647430 ) ) ;
#64768 = CARTESIAN_POINT ( 'NONE',  ( 19.42250999205614548, 30.98035201082150536, -5.440088680355545492 ) ) ;
#64769 = CARTESIAN_POINT ( 'NONE',  ( 0.6178305044545818747, 63.49863466993043204, -9.382169495545419124 ) ) ;
#64770 = CARTESIAN_POINT ( 'NONE',  ( 6.565887622018943937, 13.08196800326374998, -12.81628187352647608 ) ) ;
#64771 = CARTESIAN_POINT ( 'NONE',  ( 10.00000000000000178, 17.25893115100078745, 9.846743663894594434 ) ) ;
#64772 = EDGE_LOOP ( 'NONE', ( #84732, #47102, #82863, #43318 ) ) ;
#64773 = CARTESIAN_POINT ( 'NONE',  ( 20.36894250292379738, 64.92874883491397497, -10.36894250292379027 ) ) ;
#64774 = CARTESIAN_POINT ( 'NONE',  ( 2.917880565312948704, 32.63708216824730357, 12.26659068614894643 ) ) ;
#64775 = CARTESIAN_POINT ( 'NONE',  ( 2.035157376598822676, 27.43868534415483396, -7.964842623401177768 ) ) ;
#64776 = CARTESIAN_POINT ( 'NONE',  ( 2.035157376598824452, 53.68868534415484817, 7.964842623401179544 ) ) ;
#64777 = LINE ( 'NONE', #65773, #15978 ) ;
#64778 = DIRECTION ( 'NONE',  ( -0.7372773368101340763, -0.000000000000000000, 0.6755902076156493630 ) ) ;
#64779 = CARTESIAN_POINT ( 'NONE',  ( 5.076628168052703671, 6.842264484334118713, 8.527530157486179263 ) ) ;
#64780 =( LENGTH_UNIT ( ) NAMED_UNIT ( * ) SI_UNIT ( .MILLI., .METRE. ) );
#64781 = CARTESIAN_POINT ( 'NONE',  ( -46.61696533502858841, 101.4435428601134959, 8.298995519389800180 ) ) ;
#64782 = CARTESIAN_POINT ( 'NONE',  ( 14.92337183194729633, 27.67559781766745530, 8.527530157486181039 ) ) ;
#64783 = CARTESIAN_POINT ( 'NONE',  ( 1.472469842513823179, 51.42559781766745886, 4.923371831947296329 ) ) ;
#64784 = AXIS2_PLACEMENT_3D ( 'NONE', #96767, #65240, #95765 ) ;
#64785 = EDGE_CURVE ( 'NONE', #81069, #77887, #90189, .T. ) ;
#64786 = CARTESIAN_POINT ( 'NONE',  ( 22.81628187352647785, 46.62363466993041783, 6.195893100308588602E-16 ) ) ;
#64787 = FACE_OUTER_BOUND ( 'NONE', #2158, .T. ) ;
#64788 = CARTESIAN_POINT ( 'NONE',  ( 7.084665262690076126, 64.10535201082150536, 10.88017736071109987 ) ) ;
#64789 = CARTESIAN_POINT ( 'NONE',  ( 7.361572987183170547, 32.05059781766745175, 9.846743663894590881 ) ) ;
#64791 = CARTESIAN_POINT ( 'NONE',  ( 0.1532563361054100626, 25.80059781766744820, -2.638427012816831230 ) ) ;
#64790 = CARTESIAN_POINT ( 'NONE',  ( 13.79529636645030344, 58.26208216824728936, 14.16423886937410614 ) ) ;
#64792 = DIRECTION ( 'NONE',  ( -0.000000000000000000, -0.000000000000000000, 1.000000000000000000 ) ) ;
#64793 = CARTESIAN_POINT ( 'NONE',  ( 10.00000000000000000, 64.75893115100078035, -9.846743663894594434 ) ) ;
#64794 = CARTESIAN_POINT ( 'NONE',  ( -2.266590686148945544, 6.387082168247300906, -7.082119434687050408 ) ) ;
#64795 = EDGE_CURVE ( 'NONE', #39993, #18606, #98220, .T. ) ;
#64796 = CARTESIAN_POINT ( 'NONE',  ( 20.36894250292379382, 28.67874883491396787, 10.36894250292379205 ) ) ;
#64797 = CARTESIAN_POINT ( 'NONE',  ( 19.84674366389459621, 33.50893115100078745, 7.409399052514197653E-17 ) ) ;
#64798 = CARTESIAN_POINT ( 'NONE',  ( 18.28836319691945889, 9.344927826957706074, 6.499999999999995559 ) ) ;
#64799 = CARTESIAN_POINT ( 'NONE',  ( 2.035157376598822676, 27.43868534415483396, -7.964842623401177768 ) ) ;
#64800 = CARTESIAN_POINT ( 'NONE',  ( 17.96484262340118221, 59.93868534415484106, 7.964842623401181321 ) ) ;
#64801 = CARTESIAN_POINT ( 'NONE',  ( 19.10478245763052030, 50.10160829253887727, 5.990408912944319653 ) ) ;
#64802 = EDGE_LOOP ( 'NONE', ( #84039, #14081, #65575, #18029 ) ) ;
#64803 = CARTESIAN_POINT ( 'NONE',  ( -1.099225684535947600, 49.54030133659708923, 6.408140936763237150 ) ) ;
#64804 = CARTESIAN_POINT ( 'NONE',  ( -0.8801773607111008646, 48.27201867748816966, 2.915334737309923430 ) ) ;
#64805 = ORIENTED_EDGE ( 'NONE', *, *, #9691, .F. ) ;
#64806 = CYLINDRICAL_SURFACE ( 'NONE', #80917, 15.00000000000000000 ) ;
#64807 = CARTESIAN_POINT ( 'NONE',  ( 7.084665262690076126, 67.02201867748817676, -10.88017736071110164 ) ) ;
#64808 = AXIS2_PLACEMENT_3D ( 'NONE', #28424, #49444, #18966 ) ;
#64809 = ORIENTED_EDGE ( 'NONE', *, *, #90170, .F. ) ;
#64810 = CIRCLE ( 'NONE', #63178, 10.65000000000026326 ) ;
#64811 = CARTESIAN_POINT ( 'NONE',  ( 20.88017736071110519, 65.56368534415483396, 2.639326808657452039E-16 ) ) ;
#64812 = CARTESIAN_POINT ( 'NONE',  ( -0.8801773607110991993, 2.855352010821504471, -2.915334737309923874 ) ) ;
#64813 = CARTESIAN_POINT ( 'NONE',  ( 1.959929470562272291, 1.502578601053488283, 5.767676674365836753 ) ) ;
#64814 = CARTESIAN_POINT ( 'NONE',  ( 14.76044511231853207, 14.76984987354014400, -2.313329003772379266 ) ) ;
#64815 = CARTESIAN_POINT ( 'NONE',  ( 2.035157376598824452, 13.68868534415483751, 7.964842623401179544 ) ) ;
#64816 = CARTESIAN_POINT ( 'NONE',  ( 7.361572987183169658, 14.96726448433411960, -9.846743663894592657 ) ) ;
#64817 = CARTESIAN_POINT ( 'NONE',  ( 6.204703633549690345, 22.84541550158062861, 14.16423886937410082 ) ) ;
#64818 = VECTOR ( 'NONE', #51912, 1000.000000000000000 ) ;
#64819 =( BOUNDED_SURFACE ( )  B_SPLINE_SURFACE ( 1, 2, ( 
 ( #24515, #45517, #60518, #91519, #62477, #91009, #92003, #552, #1026, #69021, #83526, #54004, #54974, #31486, #38523, #30999, #61495, #76999, #39511, #23532, #24017, #53012, #84514, #70003, #98560, #8511, #16010, #23035, #46499, #54486, #68529, #76017, #92489, #46989, #39014, #30013, #69509, #53508, #92981, #85494, #61990, #7547, #85000, #8026, #38037, #16513, #77483, #1527, #31973, #17004, #47483, #7038, #58, #37543, #68034, #15045, #30505, #61008, #84019, #15540, #46024, #76510, #48956, #40987, #63472, #56471, #26447, #40496, #17504, #64439, #18965, #2999, #70496, #79465, #25498, #34431, #26943, #86957, #47969, #3477, #78965, #78478, #18471, #56948, #71483, #33449, #57444, #64924, #41486, #9994, #33934, #71955, #62976, #63944, #10962, #39991, #95452, #85992, #2017, #77984, #41971, #9490, #55491, #94946, #87449, #49443, #70991, #2515, #32967, #94455, #79948, #93974, #17984, #11452, #55984, #25973, #87934, #32480, #72435, #19450, #93480, #86486, #3963, #25006, #48468, #10476, #66917, #28903, #51921, #11947, #20934, #58414, #50430, #4462, #67412, #20439, #90391, #49943, #88436, #43420, #80449, #42939, #73422, #97439, #28423, #82405, #4946, #42451, #13931, #59406, #12925, #58921, #36922, #19936, #72933, #74910, #80938, #81422, #12431, #35427, #89911, #34930, #27432, #43907, #13422, #97941, #65922, #65427, #96450, #6410, #95951, #35921, #73922, #74407, #5449, #57927, #96952, #29398, #5932, #66419, #89421, #51422, #81912, #44407, #36424, #21425, #27922, #59899, #88929, #50927, #38404, #98436, #15899, #46390, #30884, #82908, #67914, #68905, #14926, #84400, #23410, #83404, #45393, #433, #53894, #75898, #61380, #29893, #14426, #91889, #15425, #7423, #76876, #98931, #22917, #7909, #60395, #37920, #68409, #90892, #21928, #52407, #22420, #52895, #30386, #6916, #75397, #53386, #60889, #44895, #83895, #91388, #37426, #45906, #76393, #33012, #63510, #79991, #56513, #95495, #40036, #11494, #26986, #80492, #48505, #94498, #42015, #94014, #4014, #56989, #19008, #72480, #2059, #11009, #79009, #40535, #93520, #57485, #10512, #70537, #32521, #78520, #33490, #63020, #25536, #56027, #87493, #18510, #34475, #86524, #25047, #64968, #49484, #3039, #48999, #87979, #10033, #55534, #19490, #71033, #71529, #2554, #18024, #49985, #86030, #17544, #33977, #3519, #48011, #41027, #63988, #26017, #87002, #79508, #41526, #71995, #64480, #94989, #26493, #58968, #29438, #5976, #43461, #73963, #66462, #81955, #44451, #35964, #28949, #27477, #28471, #74952, #4505, #13469, #5492, #96494, #89465, #11990, #6455, #42491, #88476, #43950, #20982, #59450, #50475 ),
 ( #80978, #42982, #35471, #19978, #36964, #74449, #12479, #96994, #59942, #89952, #90432, #21468, #51466, #12968, #72975, #34971, #65467, #67460, #73463, #36469, #27967, #4990, #13975, #66963, #57970, #95994, #97482, #51967, #97981, #21972, #52450, #65967, #82452, #58459, #88974, #20482, #50970, #81463, #16431, #69925, #60439, #38938, #8916, #31898, #77402, #44941, #53931, #91436, #75446, #38446, #1447, #62396, #83446, #45438, #84440, #53428, #46909, #30920, #14968, #15937, #76921, #69427, #92904, #68942, #22460, #92416, #473, #39432, #75940, #61419, #67957, #37962, #45946, #76435, #46427, #8431, #948, #31409, #61911, #7465, #24435, #82953, #54409, #6959, #52936, #23941, #22963, #14466, #37467, #60930, #83937, #84921, #98479, #15464, #29934, #68453, #90932, #98975, #30428, #7951, #91929, #23456, #94381, #71878, #17425, #63390, #86404, #9917, #26375, #79873, #24926, #85911, #78396, #32397, #87375, #56400, #62900, #40908, #3891, #3393, #34359, #33856, #2923, #55906, #85414, #16925, #77902, #11377, #93400, #86885, #40420, #55408, #56874, #48876, #1939, #39917, #63867, #10891, #41897, #72359, #64850, #54899, #17907, #70419, #41417, #48390, #78892, #93894, #18890, #95369, #47893, #64365, #47400, #9415, #49372, #70914, #25899, #25422, #2434, #10401, #32892, #71407, #33373, #18395, #79386, #94874, #91189, #75202, #27358, #60200, #22224, #83205, #38214, #82705, #65349, #37714, #14223, #60689, #57852, #44702, #11871, #80862, #90199, #21729, #98230, #52700, #29691, #90695, #7213, #88362, #76198, #7717, #98737, #49861, #95877, #68216, #35353, #45698, #53198, #4875, #96375, #30188, #83702, #59702, #22714, #19857, #80371, #15219, #14727, #65845, #68699, #6712, #67717, #45203, #50351, #29203, #52211, #12360, #26867, #57364, #42865, #42377, #37229, #19377, #87859, #75702, #72853, #4388, #34854, #73350, #93156, #78659, #85175, #24680, #40662, #39690, #2191, #61187, #16685, #92662, #55151, #62156, #76681, #47155, #17672, #85665, #31666, #24190, #54659, #70178, #32653, #77658, #17185, #15711, #9172, #63147, #91693, #1694, #32150, #84682, #62652, #47665, #61665, #38696, #78159, #40166, #9669, #23212, #70671, #46674, #55663, #48145, #93649, #69195, #25183, #1211, #720, #86162, #10164, #231, #30679, #53685, #84203, #46197, #31174, #8201, #92184, #23710, #54171, #16192, #77172, #8680, #39192, #69680, #71160, #35100, #2685, #48635, #42141, #80117, #88109, #10650, #33619, #64118, #26622, #73098, #26145, #94635, #56639, #12116, #87616, #27607, #33136, #42618, #58094, #12605, #79636, #57119, #4635, #87124, #65597, #19618, #50112, #96125, #63631 ) ),
 .UNSPECIFIED., .F., .F., .T. ) 
 B_SPLINE_SURFACE_WITH_KNOTS ( ( 2, 2 ),
 ( 3, 2, 2, 2, 2, 2, 2, 2, 2, 2, 2, 2, 2, 2, 2, 2, 2, 2, 2, 2, 2, 2, 2, 2, 2, 2, 2, 2, 2, 2, 2, 2, 2, 2, 2, 2, 2, 2, 2, 2, 2, 2, 2, 2, 2, 2, 2, 2, 2, 2, 2, 2, 2, 2, 2, 2, 2, 2, 2, 2, 2, 2, 2, 2, 2, 2, 2, 2, 2, 2, 2, 2, 2, 2, 2, 2, 2, 2, 2, 2, 2, 2, 2, 2, 2, 2, 2, 2, 2, 2, 2, 2, 2, 2, 2, 2, 2, 2, 2, 2, 2, 2, 2, 2, 2, 2, 2, 2, 2, 2, 2, 2, 2, 2, 2, 2, 2, 2, 2, 2, 2, 2, 2, 2, 2, 2, 2, 2, 2, 2, 2, 2, 2, 2, 2, 2, 2, 2, 2, 2, 2, 2, 2, 2, 2, 2, 2, 2, 2, 2, 2, 2, 2, 2, 2, 2, 2, 2, 2, 2, 2, 2, 3 ),
 ( 0.000000000000000000, 1.000000000000000000 ),
 ( 0.000000000000000000, 0.005952380952380952051, 0.01190476190476190410, 0.01785714285714285615, 0.02380952380952380820, 0.02976190476190476025, 0.03571428571428571230, 0.04166666666666666435, 0.04761904761904761640, 0.05357142857142856845, 0.05952380952380952051, 0.06547619047619047949, 0.07142857142857142461, 0.07738095238095238360, 0.08333333333333332871, 0.08928571428571428770, 0.09523809523809523281, 0.1011904761904761918, 0.1071428571428571369, 0.1130952380952380959, 0.1190476190476190410, 0.1250000000000000000, 0.1309523809523809590, 0.1369047619047619180, 0.1428571428571428492, 0.1488095238095238082, 0.1547619047619047672, 0.1607142857142857262, 0.1666666666666666574, 0.1726190476190476164, 0.1785714285714285754, 0.1845238095238095344, 0.1904761904761904656, 0.1964285714285714246, 0.2023809523809523836, 0.2083333333333333426, 0.2142857142857142738, 0.2202380952380952328, 0.2261904761904761918, 0.2321428571428571508, 0.2380952380952380820, 0.2440476190476190410, 0.2500000000000000000, 0.2559523809523809312, 0.2619047619047619180, 0.2678571428571428492, 0.2738095238095238360, 0.2797619047619047672, 0.2857142857142856984, 0.2916666666666666852, 0.2976190476190476164, 0.3035714285714285476, 0.3095238095238095344, 0.3154761904761904656, 0.3214285714285714524, 0.3273809523809523836, 0.3333333333333333148, 0.3392857142857143016, 0.3452380952380952328, 0.3511904761904761640, 0.3571428571428571508, 0.3630952380952380820, 0.3690476190476190688, 0.3750000000000000000, 0.3809523809523809312, 0.3869047619047619180, 0.3928571428571428492, 0.3988095238095238360, 0.4047619047619047672, 0.4107142857142856984, 0.4166666666666666852, 0.4226190476190476164, 0.4285714285714285476, 0.4345238095238095344, 0.4404761904761904656, 0.4464285714285714524, 0.4523809523809523836, 0.4583333333333333148, 0.4642857142857143016, 0.4702380952380952328, 0.4761904761904761640, 0.4821428571428571508, 0.4880952380952380820, 0.4940476190476190688, 0.5000000000000000000, 0.5059523809523809312, 0.5119047619047618625, 0.5178571428571429047, 0.5238095238095238360, 0.5297619047619047672, 0.5357142857142856984, 0.5416666666666666297, 0.5476190476190476719, 0.5535714285714286031, 0.5595238095238095344, 0.5654761904761904656, 0.5714285714285713969, 0.5773809523809523281, 0.5833333333333333703, 0.5892857142857143016, 0.5952380952380952328, 0.6011904761904761640, 0.6071428571428570953, 0.6130952380952381375, 0.6190476190476190688, 0.6250000000000000000, 0.6309523809523809312, 0.6369047619047618625, 0.6428571428571429047, 0.6488095238095238360, 0.6547619047619047672, 0.6607142857142856984, 0.6666666666666666297, 0.6726190476190476719, 0.6785714285714286031, 0.6845238095238095344, 0.6904761904761904656, 0.6964285714285713969, 0.7023809523809523281, 0.7083333333333333703, 0.7142857142857143016, 0.7202380952380952328, 0.7261904761904761640, 0.7321428571428570953, 0.7380952380952381375, 0.7440476190476190688, 0.7500000000000000000, 0.7559523809523809312, 0.7619047619047618625, 0.7678571428571429047, 0.7738095238095238360, 0.7797619047619047672, 0.7857142857142856984, 0.7916666666666666297, 0.7976190476190476719, 0.8035714285714286031, 0.8095238095238095344, 0.8154761904761904656, 0.8214285714285713969, 0.8273809523809523281, 0.8333333333333333703, 0.8392857142857143016, 0.8452380952380952328, 0.8511904761904761640, 0.8571428571428570953, 0.8630952380952381375, 0.8690476190476190688, 0.8750000000000000000, 0.8809523809523809312, 0.8869047619047618625, 0.8928571428571429047, 0.8988095238095238360, 0.9047619047619047672, 0.9107142857142856984, 0.9166666666666666297, 0.9226190476190476719, 0.9285714285714286031, 0.9345238095238095344, 0.9404761904761904656, 0.9464285714285713969, 0.9523809523809523281, 0.9583333333333333703, 0.9642857142857143016 ),
 .UNSPECIFIED. ) 
 GEOMETRIC_REPRESENTATION_ITEM ( )  RATIONAL_B_SPLINE_SURFACE ( (
 ( 1.000000000000000000, 0.9659258262890683122, 1.000000000000000000, 0.9659258262890683122, 1.000000000000000000, 0.9659258262890683122, 1.000000000000000000, 0.9659258262890683122, 1.000000000000000000, 0.9659258262890683122, 1.000000000000000000, 0.9659258262890683122, 1.000000000000000000, 0.9659258262890683122, 1.000000000000000000, 0.9659258262890683122, 1.000000000000000000, 0.9659258262890683122, 1.000000000000000000, 0.9659258262890683122, 1.000000000000000000, 0.9659258262890683122, 1.000000000000000000, 0.9659258262890683122, 1.000000000000000000, 0.9659258262890683122, 1.000000000000000000, 0.9659258262890683122, 1.000000000000000000, 0.9659258262890683122, 1.000000000000000000, 0.9659258262890683122, 1.000000000000000000, 0.9659258262890683122, 1.000000000000000000, 0.9659258262890683122, 1.000000000000000000, 0.9659258262890683122, 1.000000000000000000, 0.9659258262890683122, 1.000000000000000000, 0.9659258262890683122, 1.000000000000000000, 0.9659258262890683122, 1.000000000000000000, 0.9659258262890683122, 1.000000000000000000, 0.9659258262890683122, 1.000000000000000000, 0.9659258262890683122, 1.000000000000000000, 0.9659258262890683122, 1.000000000000000000, 0.9659258262890683122, 1.000000000000000000, 0.9659258262890683122, 1.000000000000000000, 0.9659258262890683122, 1.000000000000000000, 0.9659258262890683122, 1.000000000000000000, 0.9659258262890683122, 1.000000000000000000, 0.9659258262890683122, 1.000000000000000000, 0.9659258262890683122, 1.000000000000000000, 0.9659258262890683122, 1.000000000000000000, 0.9659258262890683122, 1.000000000000000000, 0.9659258262890683122, 1.000000000000000000, 0.9659258262890683122, 1.000000000000000000, 0.9659258262890683122, 1.000000000000000000, 0.9659258262890683122, 1.000000000000000000, 0.9659258262890683122, 1.000000000000000000, 0.9659258262890683122, 1.000000000000000000, 0.9659258262890683122, 1.000000000000000000, 0.9659258262890683122, 1.000000000000000000, 0.9659258262890683122, 1.000000000000000000, 0.9659258262890683122, 1.000000000000000000, 0.9659258262890683122, 1.000000000000000000, 0.9659258262890683122, 1.000000000000000000, 0.9659258262890683122, 1.000000000000000000, 0.9659258262890683122, 1.000000000000000000, 0.9659258262890683122, 1.000000000000000000, 0.9659258262890683122, 1.000000000000000000, 0.9659258262890683122, 1.000000000000000000, 0.9659258262890683122, 1.000000000000000000, 0.9659258262890683122, 1.000000000000000000, 0.9659258262890683122, 1.000000000000000000, 0.9659258262890683122, 1.000000000000000000, 0.9659258262890683122, 1.000000000000000000, 0.9659258262890683122, 1.000000000000000000, 0.9659258262890683122, 1.000000000000000000, 0.9659258262890683122, 1.000000000000000000, 0.9659258262890683122, 1.000000000000000000, 0.9659258262890683122, 1.000000000000000000, 0.9659258262890683122, 1.000000000000000000, 0.9659258262890683122, 1.000000000000000000, 0.9659258262890683122, 1.000000000000000000, 0.9659258262890683122, 1.000000000000000000, 0.9659258262890683122, 1.000000000000000000, 0.9659258262890683122, 1.000000000000000000, 0.9659258262890683122, 1.000000000000000000, 0.9659258262890683122, 1.000000000000000000, 0.9659258262890683122, 1.000000000000000000, 0.9659258262890683122, 1.000000000000000000, 0.9659258262890683122, 1.000000000000000000, 0.9659258262890683122, 1.000000000000000000, 0.9659258262890683122, 1.000000000000000000, 0.9659258262890683122, 1.000000000000000000, 0.9659258262890683122, 1.000000000000000000, 0.9659258262890683122, 1.000000000000000000, 0.9659258262890683122, 1.000000000000000000, 0.9659258262890683122, 1.000000000000000000, 0.9659258262890683122, 1.000000000000000000, 0.9659258262890683122, 1.000000000000000000, 0.9659258262890683122, 1.000000000000000000, 0.9659258262890683122, 1.000000000000000000, 0.9659258262890683122, 1.000000000000000000, 0.9659258262890683122, 1.000000000000000000, 0.9659258262890683122, 1.000000000000000000, 0.9659258262890683122, 1.000000000000000000, 0.9659258262890683122, 1.000000000000000000, 0.9659258262890683122, 1.000000000000000000, 0.9659258262890683122, 1.000000000000000000, 0.9659258262890683122, 1.000000000000000000, 0.9659258262890683122, 1.000000000000000000, 0.9659258262890683122, 1.000000000000000000, 0.9659258262890683122, 1.000000000000000000, 0.9659258262890683122, 1.000000000000000000, 0.9659258262890683122, 1.000000000000000000, 0.9659258262890683122, 1.000000000000000000, 0.9659258262890683122, 1.000000000000000000, 0.9659258262890683122, 1.000000000000000000, 0.9659258262890683122, 1.000000000000000000, 0.9659258262890683122, 1.000000000000000000, 0.9659258262890683122, 1.000000000000000000, 0.9659258262890683122, 1.000000000000000000, 0.9659258262890683122, 1.000000000000000000, 0.9659258262890683122, 1.000000000000000000, 0.9659258262890683122, 1.000000000000000000, 0.9659258262890683122, 1.000000000000000000, 0.9659258262890683122, 1.000000000000000000, 0.9659258262890683122, 1.000000000000000000, 0.9659258262890683122, 1.000000000000000000, 0.9659258262890683122, 1.000000000000000000, 0.9659258262890683122, 1.000000000000000000, 0.9659258262890683122, 1.000000000000000000, 0.9659258262890683122, 1.000000000000000000, 0.9659258262890683122, 1.000000000000000000, 0.9659258262890683122, 1.000000000000000000, 0.9659258262890683122, 1.000000000000000000, 0.9659258262890683122, 1.000000000000000000, 0.9659258262890683122, 1.000000000000000000, 0.9659258262890683122, 1.000000000000000000, 0.9659258262890683122, 1.000000000000000000, 0.9659258262890683122, 1.000000000000000000, 0.9659258262890683122, 1.000000000000000000, 0.9659258262890683122, 1.000000000000000000, 0.9659258262890683122, 1.000000000000000000, 0.9659258262890683122, 1.000000000000000000, 0.9659258262890683122, 1.000000000000000000, 0.9659258262890683122, 1.000000000000000000, 0.9659258262890683122, 1.000000000000000000, 0.9659258262890683122, 1.000000000000000000, 0.9659258262890683122, 1.000000000000000000, 0.9659258262890683122, 1.000000000000000000, 0.9659258262890683122, 1.000000000000000000, 0.9659258262890683122, 1.000000000000000000, 0.9659258262890683122, 1.000000000000000000, 0.9659258262890683122, 1.000000000000000000, 0.9659258262890683122, 1.000000000000000000, 0.9659258262890683122, 1.000000000000000000, 0.9659258262890683122, 1.000000000000000000, 0.9659258262890683122, 1.000000000000000000, 0.9659258262890683122, 1.000000000000000000, 0.9659258262890683122, 1.000000000000000000, 0.9659258262890683122, 1.000000000000000000, 0.9659258262890683122, 1.000000000000000000, 0.9659258262890683122, 1.000000000000000000, 0.9659258262890683122, 1.000000000000000000, 0.9659258262890683122, 1.000000000000000000, 0.9659258262890683122, 1.000000000000000000, 0.9659258262890683122, 1.000000000000000000, 0.9659258262890683122, 1.000000000000000000, 0.9659258262890683122, 1.000000000000000000, 0.9659258262890683122, 1.000000000000000000, 0.9659258262890683122, 1.000000000000000000, 0.9659258262890683122, 1.000000000000000000, 0.9659258262890683122, 1.000000000000000000, 0.9659258262890683122, 1.000000000000000000, 0.9659258262890683122, 1.000000000000000000, 0.9659258262890683122, 1.000000000000000000, 0.9659258262890683122, 1.000000000000000000, 0.9659258262890683122, 1.000000000000000000, 0.9659258262890683122, 1.000000000000000000),
 ( 1.000000000000000000, 0.9659258262890683122, 1.000000000000000000, 0.9659258262890683122, 1.000000000000000000, 0.9659258262890683122, 1.000000000000000000, 0.9659258262890683122, 1.000000000000000000, 0.9659258262890683122, 1.000000000000000000, 0.9659258262890683122, 1.000000000000000000, 0.9659258262890683122, 1.000000000000000000, 0.9659258262890683122, 1.000000000000000000, 0.9659258262890683122, 1.000000000000000000, 0.9659258262890683122, 1.000000000000000000, 0.9659258262890683122, 1.000000000000000000, 0.9659258262890683122, 1.000000000000000000, 0.9659258262890683122, 1.000000000000000000, 0.9659258262890683122, 1.000000000000000000, 0.9659258262890683122, 1.000000000000000000, 0.9659258262890683122, 1.000000000000000000, 0.9659258262890683122, 1.000000000000000000, 0.9659258262890683122, 1.000000000000000000, 0.9659258262890683122, 1.000000000000000000, 0.9659258262890683122, 1.000000000000000000, 0.9659258262890683122, 1.000000000000000000, 0.9659258262890683122, 1.000000000000000000, 0.9659258262890683122, 1.000000000000000000, 0.9659258262890683122, 1.000000000000000000, 0.9659258262890683122, 1.000000000000000000, 0.9659258262890683122, 1.000000000000000000, 0.9659258262890683122, 1.000000000000000000, 0.9659258262890683122, 1.000000000000000000, 0.9659258262890683122, 1.000000000000000000, 0.9659258262890683122, 1.000000000000000000, 0.9659258262890683122, 1.000000000000000000, 0.9659258262890683122, 1.000000000000000000, 0.9659258262890683122, 1.000000000000000000, 0.9659258262890683122, 1.000000000000000000, 0.9659258262890683122, 1.000000000000000000, 0.9659258262890683122, 1.000000000000000000, 0.9659258262890683122, 1.000000000000000000, 0.9659258262890683122, 1.000000000000000000, 0.9659258262890683122, 1.000000000000000000, 0.9659258262890683122, 1.000000000000000000, 0.9659258262890683122, 1.000000000000000000, 0.9659258262890683122, 1.000000000000000000, 0.9659258262890683122, 1.000000000000000000, 0.9659258262890683122, 1.000000000000000000, 0.9659258262890683122, 1.000000000000000000, 0.9659258262890683122, 1.000000000000000000, 0.9659258262890683122, 1.000000000000000000, 0.9659258262890683122, 1.000000000000000000, 0.9659258262890683122, 1.000000000000000000, 0.9659258262890683122, 1.000000000000000000, 0.9659258262890683122, 1.000000000000000000, 0.9659258262890683122, 1.000000000000000000, 0.9659258262890683122, 1.000000000000000000, 0.9659258262890683122, 1.000000000000000000, 0.9659258262890683122, 1.000000000000000000, 0.9659258262890683122, 1.000000000000000000, 0.9659258262890683122, 1.000000000000000000, 0.9659258262890683122, 1.000000000000000000, 0.9659258262890683122, 1.000000000000000000, 0.9659258262890683122, 1.000000000000000000, 0.9659258262890683122, 1.000000000000000000, 0.9659258262890683122, 1.000000000000000000, 0.9659258262890683122, 1.000000000000000000, 0.9659258262890683122, 1.000000000000000000, 0.9659258262890683122, 1.000000000000000000, 0.9659258262890683122, 1.000000000000000000, 0.9659258262890683122, 1.000000000000000000, 0.9659258262890683122, 1.000000000000000000, 0.9659258262890683122, 1.000000000000000000, 0.9659258262890683122, 1.000000000000000000, 0.9659258262890683122, 1.000000000000000000, 0.9659258262890683122, 1.000000000000000000, 0.9659258262890683122, 1.000000000000000000, 0.9659258262890683122, 1.000000000000000000, 0.9659258262890683122, 1.000000000000000000, 0.9659258262890683122, 1.000000000000000000, 0.9659258262890683122, 1.000000000000000000, 0.9659258262890683122, 1.000000000000000000, 0.9659258262890683122, 1.000000000000000000, 0.9659258262890683122, 1.000000000000000000, 0.9659258262890683122, 1.000000000000000000, 0.9659258262890683122, 1.000000000000000000, 0.9659258262890683122, 1.000000000000000000, 0.9659258262890683122, 1.000000000000000000, 0.9659258262890683122, 1.000000000000000000, 0.9659258262890683122, 1.000000000000000000, 0.9659258262890683122, 1.000000000000000000, 0.9659258262890683122, 1.000000000000000000, 0.9659258262890683122, 1.000000000000000000, 0.9659258262890683122, 1.000000000000000000, 0.9659258262890683122, 1.000000000000000000, 0.9659258262890683122, 1.000000000000000000, 0.9659258262890683122, 1.000000000000000000, 0.9659258262890683122, 1.000000000000000000, 0.9659258262890683122, 1.000000000000000000, 0.9659258262890683122, 1.000000000000000000, 0.9659258262890683122, 1.000000000000000000, 0.9659258262890683122, 1.000000000000000000, 0.9659258262890683122, 1.000000000000000000, 0.9659258262890683122, 1.000000000000000000, 0.9659258262890683122, 1.000000000000000000, 0.9659258262890683122, 1.000000000000000000, 0.9659258262890683122, 1.000000000000000000, 0.9659258262890683122, 1.000000000000000000, 0.9659258262890683122, 1.000000000000000000, 0.9659258262890683122, 1.000000000000000000, 0.9659258262890683122, 1.000000000000000000, 0.9659258262890683122, 1.000000000000000000, 0.9659258262890683122, 1.000000000000000000, 0.9659258262890683122, 1.000000000000000000, 0.9659258262890683122, 1.000000000000000000, 0.9659258262890683122, 1.000000000000000000, 0.9659258262890683122, 1.000000000000000000, 0.9659258262890683122, 1.000000000000000000, 0.9659258262890683122, 1.000000000000000000, 0.9659258262890683122, 1.000000000000000000, 0.9659258262890683122, 1.000000000000000000, 0.9659258262890683122, 1.000000000000000000, 0.9659258262890683122, 1.000000000000000000, 0.9659258262890683122, 1.000000000000000000, 0.9659258262890683122, 1.000000000000000000, 0.9659258262890683122, 1.000000000000000000, 0.9659258262890683122, 1.000000000000000000, 0.9659258262890683122, 1.000000000000000000, 0.9659258262890683122, 1.000000000000000000, 0.9659258262890683122, 1.000000000000000000, 0.9659258262890683122, 1.000000000000000000, 0.9659258262890683122, 1.000000000000000000, 0.9659258262890683122, 1.000000000000000000, 0.9659258262890683122, 1.000000000000000000, 0.9659258262890683122, 1.000000000000000000, 0.9659258262890683122, 1.000000000000000000, 0.9659258262890683122, 1.000000000000000000, 0.9659258262890683122, 1.000000000000000000, 0.9659258262890683122, 1.000000000000000000, 0.9659258262890683122, 1.000000000000000000, 0.9659258262890683122, 1.000000000000000000, 0.9659258262890683122, 1.000000000000000000, 0.9659258262890683122, 1.000000000000000000, 0.9659258262890683122, 1.000000000000000000, 0.9659258262890683122, 1.000000000000000000, 0.9659258262890683122, 1.000000000000000000, 0.9659258262890683122, 1.000000000000000000, 0.9659258262890683122, 1.000000000000000000, 0.9659258262890683122, 1.000000000000000000, 0.9659258262890683122, 1.000000000000000000, 0.9659258262890683122, 1.000000000000000000, 0.9659258262890683122, 1.000000000000000000, 0.9659258262890683122, 1.000000000000000000, 0.9659258262890683122, 1.000000000000000000, 0.9659258262890683122, 1.000000000000000000, 0.9659258262890683122, 1.000000000000000000, 0.9659258262890683122, 1.000000000000000000, 0.9659258262890683122, 1.000000000000000000, 0.9659258262890683122, 1.000000000000000000, 0.9659258262890683122, 1.000000000000000000, 0.9659258262890683122, 1.000000000000000000, 0.9659258262890683122, 1.000000000000000000, 0.9659258262890683122, 1.000000000000000000, 0.9659258262890683122, 1.000000000000000000, 0.9659258262890683122, 1.000000000000000000, 0.9659258262890683122, 1.000000000000000000) ) ) 
 REPRESENTATION_ITEM ( '' )  SURFACE ( )  );
#64820 = CARTESIAN_POINT ( 'NONE',  ( 4.559911319644449179, 28.89701867748817321, 9.422509992056141925 ) ) ;
#64821 = CARTESIAN_POINT ( 'NONE',  ( 1.472469842513823179, 60.59226448433412315, -4.923371831947296329 ) ) ;
#64822 = ORIENTED_EDGE ( 'NONE', *, *, #17762, .T. ) ;
#64823 = CARTESIAN_POINT ( 'NONE',  ( 1.472469842513823179, 60.59226448433412315, -4.923371831947296329 ) ) ;
#64824 = ORIENTED_EDGE ( 'NONE', *, *, #76713, .F. ) ;
#64825 = CARTESIAN_POINT ( 'NONE',  ( -10.58171042697161646, 0.2301503269722709466, -10.54749450092416296 ) ) ;
#64826 = CARTESIAN_POINT ( 'NONE',  ( 12.91533473730993009, 46.60535201082150536, -10.88017736071109987 ) ) ;
#64827 = CARTESIAN_POINT ( 'NONE',  ( 19.84674366389459266, 53.30059781766744464, 2.638427012816836559 ) ) ;
#64828 = CARTESIAN_POINT ( 'NONE',  ( 13.43411237798105340, 40.58196800326375353, 12.81628187352647963 ) ) ;
#64830 = CARTESIAN_POINT ( 'NONE',  ( -14.02068044289371684, 14.49999999999999822, -5.331089937175857330 ) ) ;
#64829 = CARTESIAN_POINT ( 'NONE',  ( 0.5774900079438590739, 2.647018677488170990, -5.440088680355550821 ) ) ;
#64831 = CARTESIAN_POINT ( 'NONE',  ( 17.96484262340118221, 59.93868534415484106, 7.964842623401181321 ) ) ;
#64832 = CARTESIAN_POINT ( 'NONE',  ( -0.3689425029237881626, 67.42874883491396076, 10.36894250292379027 ) ) ;
#64833 = CARTESIAN_POINT ( 'NONE',  ( 10.00000000000000178, 40.37363466993042493, 12.81628187352647608 ) ) ;
#64834 = CARTESIAN_POINT ( 'NONE',  ( 20.88017736071110519, 35.56368534415484106, 2.639326808657452039E-16 ) ) ;
#64835 = DIRECTION ( 'NONE',  ( 0.000000000000000000, 0.000000000000000000, 1.000000000000000000 ) ) ;
#64836 = ORIENTED_EDGE ( 'NONE', *, *, #44571, .F. ) ;
#64837 = CARTESIAN_POINT ( 'NONE',  ( -2.816281873526473856, 39.12363466993041783, 9.499525473075851096E-16 ) ) ;
#64838 = CARTESIAN_POINT ( 'NONE',  ( 20.88017736071110164, 40.35535201082150536, 2.915334737309930979 ) ) ;
#64839 = CARTESIAN_POINT ( 'NONE',  ( 0.1532563361054083140, 51.00893115100078745, 1.131784320476157264E-15 ) ) ;
#64840 = ORIENTED_EDGE ( 'NONE', *, *, #15283, .F. ) ;
#64841 = CARTESIAN_POINT ( 'NONE',  ( 1.472469842513823179, 65.59226448433412315, -4.923371831947296329 ) ) ;
#64843 = CARTESIAN_POINT ( 'NONE',  ( 17.20831665107776587, 52.88393115100078035, 7.208316651077764980 ) ) ;
#64842 = CARTESIAN_POINT ( 'NONE',  ( 19.72487221294570858, 0.000000000000000000, -6.500000000000000888 ) ) ;
#64844 = CARTESIAN_POINT ( 'NONE',  ( 2.035157376598824452, 28.68868534415484106, 7.964842623401179544 ) ) ;
#64845 = FACE_OUTER_BOUND ( 'NONE', #6071, .T. ) ;
#64846 = CARTESIAN_POINT ( 'NONE',  ( 7.361572987183169658, 34.96726448433411605, -9.846743663894592657 ) ) ;
#64847 = DIRECTION ( 'NONE',  ( 1.000000000000000000, 0.000000000000000000, 0.000000000000000000 ) ) ;
#64848 = TOROIDAL_SURFACE ( 'NONE', #76015, 18.53834841531100608, 7.000000000000000000 ) ;
#64849 = CARTESIAN_POINT ( 'NONE',  ( -7.750000000000000000, 40.74999999999999289, -3.750000000000000000 ) ) ;
#64851 = CARTESIAN_POINT ( 'NONE',  ( 14.92337183194729988, 14.34226448433411782, -8.527530157486177487 ) ) ;
#64850 = CARTESIAN_POINT ( 'NONE',  ( 18.52753015748618282, 28.92559781766745175, -4.923371831947291888 ) ) ;
#64852 = DIRECTION ( 'NONE',  ( -1.257402221000611116E-16, 1.000000000000000000, 0.000000000000000000 ) ) ;
#64854 = ORIENTED_EDGE ( 'NONE', *, *, #73972, .T. ) ;
#64853 = CARTESIAN_POINT ( 'NONE',  ( 1.472469842513823179, 65.59226448433412315, -4.923371831947296329 ) ) ;
#64855 = CARTESIAN_POINT ( 'NONE',  ( 0.6178305044545818747, 63.49863466993043204, -9.382169495545419124 ) ) ;
#64856 = CARTESIAN_POINT ( 'NONE',  ( 19.38216949554541202, 40.99863466993042493, 9.382169495545424454 ) ) ;
#64857 = CARTESIAN_POINT ( 'NONE',  ( 14.92337183194729633, 47.67559781766745175, 8.527530157486181039 ) ) ;
#64858 = SURFACE_STYLE_USAGE ( .BOTH. , #43839 ) ;
#64859 = CARTESIAN_POINT ( 'NONE',  ( 24.16423886937410614, 64.30374883491396076, 8.672049930838204340E-16 ) ) ;
#64860 = CARTESIAN_POINT ( 'NONE',  ( 18.52753015748618282, 18.92559781766745175, -4.923371831947291888 ) ) ;
#64861 = CARTESIAN_POINT ( 'NONE',  ( 20.00000000000000711, 81.00835155610852212, 4.500000004094268036 ) ) ;
#64862 = CARTESIAN_POINT ( 'NONE',  ( 6.204703633549690345, 52.84541550158062506, 14.16423886937410082 ) ) ;
#64863 = CARTESIAN_POINT ( 'NONE',  ( 19.42250999205614193, 5.147018677488171434, 5.440088680355555262 ) ) ;
#64864 = CARTESIAN_POINT ( 'NONE',  ( 20.36894250292379382, 33.67874883491396076, 10.36894250292379205 ) ) ;
#64865 = CARTESIAN_POINT ( 'NONE',  ( 24.16423886937409904, 34.09541550158064638, 3.795296366450317205 ) ) ;
#64866 = DIRECTION ( 'NONE',  ( -0.000000000000000000, -0.000000000000000000, 1.000000000000000000 ) ) ;
#64867 = CARTESIAN_POINT ( 'NONE',  ( 0.1532563361054082862, 16.21726448433411960, 2.638427012816831674 ) ) ;
#64869 = CARTESIAN_POINT ( 'NONE',  ( 10.00000000000000000, 54.75893115100078745, -9.846743663894594434 ) ) ;
#64868 = DIRECTION ( 'NONE',  ( 0.000000000000000000, 0.000000000000000000, 1.000000000000000000 ) ) ;
#64870 = CARTESIAN_POINT ( 'NONE',  ( 2.035157376598824452, 53.68868534415484817, 7.964842623401179544 ) ) ;
#64871 = CARTESIAN_POINT ( 'NONE',  ( 11.29340449002647162, -89.90880494512830978, 3.750000000000000444 ) ) ;
#64872 = EDGE_CURVE ( 'NONE', #14724, #86159, #83407, .T. ) ;
#64873 = DIRECTION ( 'NONE',  ( 0.000000000000000000, 0.000000000000000000, -1.000000000000000000 ) ) ;
#64874 = CARTESIAN_POINT ( 'NONE',  ( 14.92337183194729988, 59.34226448433412315, -8.527530157486177487 ) ) ;
#64875 = SURFACE_STYLE_USAGE ( .BOTH. , #12389 ) ;
#64876 = VERTEX_POINT ( 'NONE', #5725 ) ;
#64877 = CARTESIAN_POINT ( 'NONE',  ( 10.00000000000000000, 20.55374883491396787, -14.16423886937410082 ) ) ;
#64878 = MECHANICAL_DESIGN_GEOMETRIC_PRESENTATION_REPRESENTATION (  '', ( #12223 ), #42577 ) ;
#64879 = CARTESIAN_POINT ( 'NONE',  ( 2.791683348922240793, 1.633931151000784565, 7.208316651077764092 ) ) ;
#64880 = CARTESIAN_POINT ( 'NONE',  ( 20.88017736071110519, 45.56368534415484106, 2.639326808657452039E-16 ) ) ;
#64881 = CARTESIAN_POINT ( 'NONE',  ( 7.084665262690076126, 24.10535201082150181, 10.88017736071109987 ) ) ;
#64882 = CARTESIAN_POINT ( 'NONE',  ( -1.099225684535947600, 18.70696800326375353, -6.408140936763238038 ) ) ;
#64883 = CARTESIAN_POINT ( 'NONE',  ( 20.15039907845753220, 61.74884699246888431, 6.262539305110078836 ) ) ;
#64884 = CARTESIAN_POINT ( 'NONE',  ( 7.361572987183170547, 7.050597817667451750, 9.846743663894590881 ) ) ;
#64885 = CARTESIAN_POINT ( 'NONE',  ( 22.81628187352647785, 46.62363466993041783, 6.195893100308588602E-16 ) ) ;
#64886 = VERTEX_POINT ( 'NONE', #52689 ) ;
#64887 = CARTESIAN_POINT ( 'NONE',  ( 6.934035614004487869, -73.16521313705239038, -3.750000000000000000 ) ) ;
#64888 = CARTESIAN_POINT ( 'NONE',  ( 2.917880565312948704, 22.63708216824730002, 12.26659068614894643 ) ) ;
#64889 = CARTESIAN_POINT ( 'NONE',  ( 20.30776406404415724, 0.000000000000000000, -5.999999999999999112 ) ) ;
#64890 = FACE_OUTER_BOUND ( 'NONE', #80177, .T. ) ;
#64891 = CARTESIAN_POINT ( 'NONE',  ( 7.084665262690076126, 12.02201867748817321, -10.88017736071110164 ) ) ;
#64892 = FACE_OUTER_BOUND ( 'NONE', #64609, .T. ) ;
#64893 = CARTESIAN_POINT ( 'NONE',  ( 10.00000000000000000, 36.81368534415484106, -10.88017736071110342 ) ) ;
#64894 = CARTESIAN_POINT ( 'NONE',  ( 2.035157376598824452, 33.68868534415484106, 7.964842623401179544 ) ) ;
#64895 = CARTESIAN_POINT ( 'NONE',  ( -2.816281873526473856, 19.12363466993042138, 9.499525473075851096E-16 ) ) ;
#64896 = CARTESIAN_POINT ( 'NONE',  ( 10.00000000000000178, 62.25893115100078745, 9.846743663894594434 ) ) ;
#64897 = CARTESIAN_POINT ( 'NONE',  ( -0.8801773607110990882, 2.855352010821504471, -2.915334737309924318 ) ) ;
#64898 = CARTESIAN_POINT ( 'NONE',  ( 17.20831665107776587, 9.133931151000787452, -7.208316651077762316 ) ) ;
#64899 = ORIENTED_EDGE ( 'NONE', *, *, #32843, .T. ) ;
#64900 = VECTOR ( 'NONE', #10363, 1000.000000000000000 ) ;
#64901 = DIRECTION ( 'NONE',  ( -0.000000000000000000, -1.000000000000000000, 0.000000000000000000 ) ) ;
#64902 = CARTESIAN_POINT ( 'NONE',  ( 2.035157376598824452, 43.68868534415484106, 7.964842623401179544 ) ) ;
#64903 = CIRCLE ( 'NONE', #15426, 0.4999999999999985567 ) ;
#64904 =( GEOMETRIC_REPRESENTATION_CONTEXT ( 3 ) GLOBAL_UNCERTAINTY_ASSIGNED_CONTEXT ( ( #2250 ) ) GLOBAL_UNIT_ASSIGNED_CONTEXT ( ( #55656, #46665, #54162 ) ) REPRESENTATION_CONTEXT ( 'NONE', 'WORKASPACE' ) );
#64906 = EDGE_CURVE ( 'NONE', #79719, #46092, #96182, .T. ) ;
#64905 = AXIS2_PLACEMENT_3D ( 'NONE', #6599, #37112, #45086 ) ;
#64907 = CARTESIAN_POINT ( 'NONE',  ( 3.591859063236761518, -0.04303199673624671928, 11.09922568453594849 ) ) ;
#64908 = CARTESIAN_POINT ( 'NONE',  ( 2.035157376598824452, 63.68868534415484106, 7.964842623401179544 ) ) ;
#64909 = CARTESIAN_POINT ( 'NONE',  ( 1.472469842513823179, 21.42559781766745175, 4.923371831947296329 ) ) ;
#64910 = CARTESIAN_POINT ( 'NONE',  ( -2.816281873526473856, 44.12363466993042493, 9.499525473075851096E-16 ) ) ;
#64912 = LINE ( 'NONE', #2000, #44862 ) ;
#64911 = CARTESIAN_POINT ( 'NONE',  ( 10.00000000000000178, 69.31368534415484817, 10.88017736071110342 ) ) ;
#64913 = ORIENTED_EDGE ( 'NONE', *, *, #2248, .T. ) ;
#64914 = CARTESIAN_POINT ( 'NONE',  ( -12.25993886608611660, 15.00000000000000000, 8.642563219313529999 ) ) ;
#64915 = DIRECTION ( 'NONE',  ( 0.8070303256584299145, -0.5905099943842175847, 0.000000000000000000 ) ) ;
#64916 = CARTESIAN_POINT ( 'NONE',  ( 20.88017736071110875, 15.77201867748817143, -2.915334737309920765 ) ) ;
#64917 = CARTESIAN_POINT ( 'NONE',  ( 3.591859063236761518, 59.95696800326375353, 11.09922568453594849 ) ) ;
#64918 = CARTESIAN_POINT ( 'NONE',  ( 0.1532563361054083140, 26.00893115100078745, 1.131784320476157264E-15 ) ) ;
#64919 = CARTESIAN_POINT ( 'NONE',  ( 20.88017736071110164, 25.35535201082150891, 2.915334737309930979 ) ) ;
#64920 = CARTESIAN_POINT ( 'NONE',  ( 19.42250999205614193, 10.14701867748816966, 5.440088680355555262 ) ) ;
#64921 = VERTEX_POINT ( 'NONE', #66712 ) ;
#64922 = AXIS2_PLACEMENT_3D ( 'NONE', #64958, #16661, #77633 ) ;
#64923 = CARTESIAN_POINT ( 'NONE',  ( 10.00000000000000000, 16.81368534415483751, -10.88017736071110342 ) ) ;
#64924 = CARTESIAN_POINT ( 'NONE',  ( 17.96484262340118221, 19.93868534415484106, 7.964842623401181321 ) ) ;
#64926 = CARTESIAN_POINT ( 'NONE',  ( 20.88017736071110164, 25.35535201082150891, 2.915334737309930979 ) ) ;
#64925 = DIRECTION ( 'NONE',  ( -0.000000000000000000, -1.000000000000000000, -0.000000000000000000 ) ) ;
#64927 = ORIENTED_EDGE ( 'NONE', *, *, #94961, .F. ) ;
#64928 =( GEOMETRIC_REPRESENTATION_CONTEXT ( 3 ) GLOBAL_UNCERTAINTY_ASSIGNED_CONTEXT ( ( #59126 ) ) GLOBAL_UNIT_ASSIGNED_CONTEXT ( ( #65581, #56623, #35082 ) ) REPRESENTATION_CONTEXT ( 'NONE', 'WORKASPACE' ) );
#64929 = CARTESIAN_POINT ( 'NONE',  ( 0.000000000000000000, 0.5000000000000004441, 0.000000000000000000 ) ) ;
#64930 = CARTESIAN_POINT ( 'NONE',  ( 4.559911319644449179, 17.23035201082150536, -9.422509992056141925 ) ) ;
#64931 = CARTESIAN_POINT ( 'NONE',  ( 18.52753015748618282, 53.92559781766745175, -4.923371831947291888 ) ) ;
#64932 = CARTESIAN_POINT ( 'NONE',  ( 4.380000000000002558, 1.019547802438462547, 3.750000000000000000 ) ) ;
#64933 = CARTESIAN_POINT ( 'NONE',  ( -14.40939250469963895, 4.354406223596783273E-16, -1.618458416365949226 ) ) ;
#64934 = CARTESIAN_POINT ( 'NONE',  ( 13.79529636645030344, 33.26208216824730357, 14.16423886937410614 ) ) ;
#64935 = CARTESIAN_POINT ( 'NONE',  ( 12.91533473730993009, 41.60535201082149825, -10.88017736071109987 ) ) ;
#64936 = CARTESIAN_POINT ( 'NONE',  ( 2.035157376598822676, 17.43868534415483751, -7.964842623401177768 ) ) ;
#64937 = CARTESIAN_POINT ( 'NONE',  ( 18.52753015748617571, 63.09226448433412315, 4.923371831947298993 ) ) ;
#64938 =( GEOMETRIC_REPRESENTATION_CONTEXT ( 3 ) GLOBAL_UNCERTAINTY_ASSIGNED_CONTEXT ( ( #63447 ) ) GLOBAL_UNIT_ASSIGNED_CONTEXT ( ( #16511, #24512, #69508 ) ) REPRESENTATION_CONTEXT ( 'NONE', 'WORKASPACE' ) );
#64939 = CARTESIAN_POINT ( 'NONE',  ( -11.22915323889568562, 0.000000000000000000, -8.773176023390764300 ) ) ;
#64940 = CARTESIAN_POINT ( 'NONE',  ( 0.1532563361054082862, 51.21726448433412315, 2.638427012816831674 ) ) ;
#64941 = CARTESIAN_POINT ( 'NONE',  ( -0.04068437667224348436, 22.21974360917720404, -6.396802510829702193 ) ) ;
#64942 = CARTESIAN_POINT ( 'NONE',  ( 19.84674366389459266, 3.717264484334118713, -2.638427012816827677 ) ) ;
#64943 = CARTESIAN_POINT ( 'NONE',  ( 11.09922568453594671, -27.95969866340291077, -6.408140936763241591 ) ) ;
#64944 = ADVANCED_FACE ( 'NONE', ( #89700 ), #9969, .T. ) ;
#64945 = CARTESIAN_POINT ( 'NONE',  ( 4.559911319644449179, 13.89701867748817143, 9.422509992056141925 ) ) ;
#64946 = CARTESIAN_POINT ( 'NONE',  ( 1.472469842513823179, 11.42559781766745175, 4.923371831947296329 ) ) ;
#64948 = CARTESIAN_POINT ( 'NONE',  ( 12.91533473730993009, 51.60535201082149825, -10.88017736071109987 ) ) ;
#64947 = CARTESIAN_POINT ( 'NONE',  ( 19.42250999205614193, 60.14701867748817676, 5.440088680355555262 ) ) ;
#64950 = CARTESIAN_POINT ( 'NONE',  ( 16.40814093676324603, 62.45696800326376064, -11.09922568453594671 ) ) ;
#64949 = CARTESIAN_POINT ( 'NONE',  ( 2.035157376598824452, 13.68868534415483751, 7.964842623401179544 ) ) ;
#64951 = CARTESIAN_POINT ( 'NONE',  ( -0.3689425029237881626, 27.42874883491397142, 10.36894250292379027 ) ) ;
#64952 = EDGE_CURVE ( 'NONE', #39344, #94453, #48272, .T. ) ;
#64953 = DIRECTION ( 'NONE',  ( -1.927470528863119542E-16, 1.000000000000000000, 0.000000000000000000 ) ) ;
#64955 = CARTESIAN_POINT ( 'NONE',  ( 16.40814093676324603, 57.45696800326375353, -11.09922568453594671 ) ) ;
#64954 = VECTOR ( 'NONE', #29202, 1000.000000000000000 ) ;
#64956 = ORIENTED_EDGE ( 'NONE', *, *, #51299, .T. ) ;
#64957 = CARTESIAN_POINT ( 'NONE',  ( 16.40814093676324603, 7.456968003263754419, -11.09922568453594671 ) ) ;
#64958 = CARTESIAN_POINT ( 'NONE',  ( -3.750000000000000000, 10.25000000000000000, 2.750000000000000000 ) ) ;
#64959 = CARTESIAN_POINT ( 'NONE',  ( 4.559911319644449179, 33.89701867748817676, 9.422509992056141925 ) ) ;
#64960 = DIRECTION ( 'NONE',  ( -0.8141155183563226760, 0.000000000000000000, 0.5807029557109348872 ) ) ;
#64961 = EDGE_CURVE ( 'NONE', #1475, #20937, #37222, .T. ) ;
#64962 = ORIENTED_EDGE ( 'NONE', *, *, #1458, .F. ) ;
#64963 = CARTESIAN_POINT ( 'NONE',  ( 19.84674366389459266, 8.300597817667451750, 2.638427012816836559 ) ) ;
#64964 = CARTESIAN_POINT ( 'NONE',  ( 7.361572987183170547, 7.050597817667451750, 9.846743663894590881 ) ) ;
#64965 = CARTESIAN_POINT ( 'NONE',  ( 0.1532563361054083140, 21.00893115100078745, 1.131784320476157264E-15 ) ) ;
#64966 = CARTESIAN_POINT ( 'NONE',  ( 12.63842701281683034, 12.46726448433411782, 9.846743663894596210 ) ) ;
#64967 = CARTESIAN_POINT ( 'NONE',  ( 1.472469842513823179, 1.425597817667451528, 4.923371831947296329 ) ) ;
#64970 = CARTESIAN_POINT ( 'NONE',  ( -45.94000000000000483, 93.00000000000000000, -9.500000000000000000 ) ) ;
#64969 = AXIS2_PLACEMENT_3D ( 'NONE', #71043, #89473, #49995 ) ;
#64968 = CARTESIAN_POINT ( 'NONE',  ( -0.8801773607111008646, 58.27201867748816966, 2.915334737309923430 ) ) ;
#64971 = CARTESIAN_POINT ( 'NONE',  ( 4.559911319644449179, 63.89701867748817676, 9.422509992056141925 ) ) ;
#64973 = EDGE_LOOP ( 'NONE', ( #17877, #63094, #34963, #48500 ) ) ;
#64972 = CARTESIAN_POINT ( 'NONE',  ( 2.791683348922237240, 25.38393115100078390, -7.208316651077763204 ) ) ;
#64974 = AXIS2_PLACEMENT_3D ( 'NONE', #17123, #86592, #18101 ) ;
#64975 = CARTESIAN_POINT ( 'NONE',  ( -8.838651438279651273, 0.04922511925147145251, 11.81204219878332751 ) ) ;
#64976 = CARTESIAN_POINT ( 'NONE',  ( 7.361572987183170547, 57.05059781766744464, 9.846743663894590881 ) ) ;
#64977 = ORIENTED_EDGE ( 'NONE', *, *, #17906, .T. ) ;
#64978 = VERTEX_POINT ( 'NONE', #59694 ) ;
#64979 = CARTESIAN_POINT ( 'NONE',  ( 20.88017736071110875, 5.772018677488170546, -2.915334737309920765 ) ) ;
#64980 = CARTESIAN_POINT ( 'NONE',  ( 10.00000000000000000, 25.55374883491396787, -14.16423886937410082 ) ) ;
#64981 = DIRECTION ( 'NONE',  ( 0.000000000000000000, 0.000000000000000000, 1.000000000000000000 ) ) ;
#64982 = CARTESIAN_POINT ( 'NONE',  ( -4.164238869374099927, 17.01208216824730357, 3.795296366450308767 ) ) ;
#64983 = CARTESIAN_POINT ( 'NONE',  ( 6.204703633549690345, 30.76208216824730357, -14.16423886937410259 ) ) ;
#64984 = CARTESIAN_POINT ( 'NONE',  ( 2.917880565312948704, 2.637082168247300906, 12.26659068614894643 ) ) ;
#64985 = CARTESIAN_POINT ( 'NONE',  ( 17.96484262340118221, 31.18868534415483751, -7.964842623401177768 ) ) ;
#64986 = CARTESIAN_POINT ( 'NONE',  ( 12.63842701281683922, 14.55059781766744997, -9.846743663894590881 ) ) ;
#64988 = CARTESIAN_POINT ( 'NONE',  ( 1.472469842513823179, 20.59226448433411960, -4.923371831947296329 ) ) ;
#64987 = CARTESIAN_POINT ( 'NONE',  ( 4.559911319644449179, 57.23035201082150536, -9.422509992056141925 ) ) ;
#64989 = CARTESIAN_POINT ( 'NONE',  ( 19.42250999205614193, 15.14701867748817143, 5.440088680355555262 ) ) ;
#64990 = CARTESIAN_POINT ( 'NONE',  ( -2.816281873526473856, 44.33196800326375353, 3.434112377981055619 ) ) ;
#64991 = CARTESIAN_POINT ( 'NONE',  ( 5.076628168052704559, 50.17559781766745886, -8.527530157486179263 ) ) ;
#64992 = DIRECTION ( 'NONE',  ( 1.000000000000000000, -5.818595309480552676E-17, 0.000000000000000000 ) ) ;
#64993 = EDGE_CURVE ( 'NONE', #20387, #42602, #29680, .T. ) ;
#64994 = CARTESIAN_POINT ( 'NONE',  ( 22.81628187352647785, 26.41530133659708923, 3.434112377981063169 ) ) ;
#64995 = CARTESIAN_POINT ( 'NONE',  ( 3.469446951953614189E-15, -31.94625116508602858, 14.16423886937410259 ) ) ;
#64996 = CARTESIAN_POINT ( 'NONE',  ( 17.20831665107776587, 32.88393115100078745, 7.208316651077764980 ) ) ;
#64997 = CARTESIAN_POINT ( 'NONE',  ( 2.917880565312948704, 17.63708216824730357, 12.26659068614894643 ) ) ;
#64998 = EDGE_LOOP ( 'NONE', ( #12333, #36044, #35365, #28580, #96826, #27422 ) ) ;
#64999 = CARTESIAN_POINT ( 'NONE',  ( 4.219999999999999751, 10.00000000000000000, 2.750000000000000000 ) ) ;
#65000 = EDGE_CURVE ( 'NONE', #29785, #25526, #14716, .T. ) ;
#65001 = STYLED_ITEM ( 'NONE', ( #10828 ), #30076 ) ;
#65002 = CARTESIAN_POINT ( 'NONE',  ( 19.42250999205614548, 45.98035201082150536, -5.440088680355545492 ) ) ;
#65003 = CARTESIAN_POINT ( 'NONE',  ( 19.42250999205614193, 55.14701867748817676, 5.440088680355555262 ) ) ;
#65004 = CARTESIAN_POINT ( 'NONE',  ( 20.36894250292379738, 49.92874883491396787, -10.36894250292379027 ) ) ;
#65005 = CARTESIAN_POINT ( 'NONE',  ( 2.791683348922237240, 60.38393115100078745, -7.208316651077763204 ) ) ;
#65006 = CARTESIAN_POINT ( 'NONE',  ( 2.791683348922240793, 11.63393115100078568, 7.208316651077764092 ) ) ;
#65007 = CARTESIAN_POINT ( 'NONE',  ( 16.40814093676324603, 62.45696800326376064, -11.09922568453594671 ) ) ;
#65008 = CARTESIAN_POINT ( 'NONE',  ( -0.8801773607110991993, 47.85535201082150536, -2.915334737309923874 ) ) ;
#65009 = CARTESIAN_POINT ( 'NONE',  ( -6.866275848337627608, -80.67678253189124860, -2.500000000000000000 ) ) ;
#65010 = CARTESIAN_POINT ( 'NONE',  ( 10.00000000000000178, 52.25893115100078745, 9.846743663894594434 ) ) ;
#65011 = CARTESIAN_POINT ( 'NONE',  ( -2.915334737309917656, 19.10535201082151247, 10.88017736071110164 ) ) ;
#65012 =( LENGTH_UNIT ( ) NAMED_UNIT ( * ) SI_UNIT ( .MILLI., .METRE. ) );
#65013 = ADVANCED_FACE ( 'NONE', ( #7202 ), #86549, .T. ) ;
#65014 = CARTESIAN_POINT ( 'NONE',  ( 0.1089645850228953966, 13.16234555792570582, 6.479102184480805882 ) ) ;
#65015 =( NAMED_UNIT ( * ) PLANE_ANGLE_UNIT ( ) SI_UNIT ( $, .RADIAN. ) );
#65016 = CARTESIAN_POINT ( 'NONE',  ( 14.88232117145529720, 0.5000000000000004441, 1.875237731503240024 ) ) ;
#65017 = CARTESIAN_POINT ( 'NONE',  ( 19.84674366389459266, 3.717264484334118713, -2.638427012816827677 ) ) ;
#65018 = CARTESIAN_POINT ( 'NONE',  ( 0.1532563361054083140, 1.008931151000784787, 1.131784320476157264E-15 ) ) ;
#65019 = DIRECTION ( 'NONE',  ( 0.000000000000000000, 0.000000000000000000, 1.000000000000000000 ) ) ;
#65020 = EDGE_CURVE ( 'NONE', #88318, #7347, #60983, .T. ) ;
#65021 = CARTESIAN_POINT ( 'NONE',  ( 19.84674366389459621, 28.50893115100078745, 7.409399052514197653E-17 ) ) ;
#65022 = CARTESIAN_POINT ( 'NONE',  ( 12.91533473730993009, 21.60535201082150536, -10.88017736071109987 ) ) ;
#65023 = CARTESIAN_POINT ( 'NONE',  ( 0.1532563361054082862, 61.21726448433412315, 2.638427012816831674 ) ) ;
#65025 = CARTESIAN_POINT ( 'NONE',  ( 0.2751277870542909176, 60.30223176428830101, 6.499999999999992006 ) ) ;
#65024 = CARTESIAN_POINT ( 'NONE',  ( 2.035157376598822676, 37.43868534415484106, -7.964842623401177768 ) ) ;
#65026 =( NAMED_UNIT ( * ) PLANE_ANGLE_UNIT ( ) SI_UNIT ( $, .RADIAN. ) );
#65027 = CARTESIAN_POINT ( 'NONE',  ( 10.00000000000000000, 42.87363466993042493, -12.81628187352647608 ) ) ;
#65028 = ORIENTED_EDGE ( 'NONE', *, *, #49476, .T. ) ;
#65029 = CARTESIAN_POINT ( 'NONE',  ( 4.559911319644449179, 53.89701867748817676, 9.422509992056141925 ) ) ;
#65030 = ADVANCED_FACE ( 'NONE', ( #92651 ), #73589, .T. ) ;
#65032 = CARTESIAN_POINT ( 'NONE',  ( 0.000000000000000000, 0.000000000000000000, 0.000000000000000000 ) ) ;
#65031 = CARTESIAN_POINT ( 'NONE',  ( 22.81628187352648496, 16.83196800326374998, -3.434112377981050290 ) ) ;
#65033 = CARTESIAN_POINT ( 'NONE',  ( 17.96484262340118221, 31.18868534415483751, -7.964842623401177768 ) ) ;
#65034 = CARTESIAN_POINT ( 'NONE',  ( -0.3689425029237881626, 62.42874883491396787, 10.36894250292379027 ) ) ;
#65035 = VECTOR ( 'NONE', #62518, 1000.000000000000000 ) ;
#65036 = CARTESIAN_POINT ( 'NONE',  ( 17.20831665107776587, 49.13393115100078745, -7.208316651077762316 ) ) ;
#65037 = CARTESIAN_POINT ( 'NONE',  ( 19.84674366389459266, 8.717264484334116048, -2.638427012816827677 ) ) ;
#65038 = CARTESIAN_POINT ( 'NONE',  ( -0.8801773607111008646, 63.27201867748817676, 2.915334737309923430 ) ) ;
#65039 = CARTESIAN_POINT ( 'NONE',  ( 13.34343830728408697, 14.49999999999999112, -6.852200678592647698 ) ) ;
#65040 = CARTESIAN_POINT ( 'NONE',  ( 24.16423886937409904, 34.09541550158064638, 3.795296366450317205 ) ) ;
#65041 = AXIS2_PLACEMENT_3D ( 'NONE', #83844, #38356, #382 ) ;
#65042 = TOROIDAL_SURFACE ( 'NONE', #33083, 0.7500000000000008882, 0.2500000000000000000 ) ;
#65043 = CARTESIAN_POINT ( 'NONE',  ( -9.281709892946549800, -3.133174871893655771E-15, 11.30302492080699928 ) ) ;
#65044 = DIRECTION ( 'NONE',  ( -0.06975647374412544122, -0.9975640502598241977, 0.000000000000000000 ) ) ;
#65045 = STYLED_ITEM ( 'NONE', ( #29766 ), #68884 ) ;
#65046 = VERTEX_POINT ( 'NONE', #87130 ) ;
#65047 = CARTESIAN_POINT ( 'NONE',  ( 10.00000000000000000, 45.55374883491397497, -14.16423886937410082 ) ) ;
#65048 = CARTESIAN_POINT ( 'NONE',  ( 24.16423886937410614, 49.30374883491396787, 8.672049930838204340E-16 ) ) ;
#65049 = CARTESIAN_POINT ( 'NONE',  ( 1.472469842513823179, 16.42559781766745175, 4.923371831947296329 ) ) ;
#65050 = CARTESIAN_POINT ( 'NONE',  ( 13.43411237798105340, 15.58196800326374998, 12.81628187352647963 ) ) ;
#65051 = DIRECTION ( 'NONE',  ( 0.3665012267242946375, 0.000000000000000000, 0.9304175679820254619 ) ) ;
#65052 = CARTESIAN_POINT ( 'NONE',  ( -32.19000000000001194, 93.50000000000000000, 9.500000000000000000 ) ) ;
#65054 = CARTESIAN_POINT ( 'NONE',  ( 19.38216949554541557, 52.24863466993041072, -9.382169495545420901 ) ) ;
#65053 = FILL_AREA_STYLE_COLOUR ( '', #46728 ) ;
#65055 = CARTESIAN_POINT ( 'NONE',  ( -0.3689425029237881626, 47.42874883491396787, 10.36894250292379027 ) ) ;
#65056 = PRESENTATION_STYLE_ASSIGNMENT (( #64074 ) ) ;
#65057 = CARTESIAN_POINT ( 'NONE',  ( 5.076628168052704559, 5.175597817667451750, -8.527530157486179263 ) ) ;
#65058 = CARTESIAN_POINT ( 'NONE',  ( -8.527530157486173934, -3.574402182332542033, 4.923371831947302546 ) ) ;
#65059 = VERTEX_POINT ( 'NONE', #86658 ) ;
#65060 = CARTESIAN_POINT ( 'NONE',  ( 0.000000000000000000, 0.000000000000000000, 6.500000000000000888 ) ) ;
#65061 = CARTESIAN_POINT ( 'NONE',  ( 14.92337183194729988, 19.34226448433411960, -8.527530157486177487 ) ) ;
#65062 = ORIENTED_EDGE ( 'NONE', *, *, #36054, .F. ) ;
#65063 = SPHERICAL_SURFACE ( 'NONE', #92398, 0.2500000000000000000 ) ;
#65064 = ORIENTED_EDGE ( 'NONE', *, *, #93966, .F. ) ;
#65065 = CARTESIAN_POINT ( 'NONE',  ( -0.3689425029237898834, 11.17874883491396787, -10.36894250292378850 ) ) ;
#65067 = CARTESIAN_POINT ( 'NONE',  ( 15.44008868035555793, 31.39701867748817676, -9.422509992056140149 ) ) ;
#65066 = CARTESIAN_POINT ( 'NONE',  ( 17.96484262340118221, 19.93868534415484106, 7.964842623401181321 ) ) ;
#65069 = CARTESIAN_POINT ( 'NONE',  ( -2.816281873526473856, 4.123634669930420493, 9.499525473075851096E-16 ) ) ;
#65068 = CARTESIAN_POINT ( 'NONE',  ( 14.92337183194729633, 47.67559781766745175, 8.527530157486181039 ) ) ;
#65070 = DIRECTION ( 'NONE',  ( 0.000000000000000000, -1.000000000000000000, 0.000000000000000000 ) ) ;
#65071 = ADVANCED_FACE ( 'NONE', ( #2691 ), #71166, .T. ) ;
#65072 = CARTESIAN_POINT ( 'NONE',  ( 16.40814093676323893, 20.79030133659708923, 11.09922568453595026 ) ) ;
#65073 = ORIENTED_EDGE ( 'NONE', *, *, #77356, .T. ) ;
#65074 = CARTESIAN_POINT ( 'NONE',  ( 0.1532563361054082862, 36.21726448433410894, 2.638427012816831674 ) ) ;
#65075 = CARTESIAN_POINT ( 'NONE',  ( -0.3689425029237898834, 56.17874883491396076, -10.36894250292378850 ) ) ;
#65076 = VERTEX_POINT ( 'NONE', #56166 ) ;
#65077 = CARTESIAN_POINT ( 'NONE',  ( 17.08211943468705840, 50.13708216824730357, -12.26659068614894466 ) ) ;
#65078 = ORIENTED_EDGE ( 'NONE', *, *, #71522, .T. ) ;
#65079 = CARTESIAN_POINT ( 'NONE',  ( 20.88017736071110875, 35.77201867748816966, -2.915334737309920765 ) ) ;
#65080 = CARTESIAN_POINT ( 'NONE',  ( 15.44008868035555793, 46.39701867748817676, -9.422509992056140149 ) ) ;
#65081 = AXIS2_PLACEMENT_3D ( 'NONE', #60700, #52710, #21235 ) ;
#65082 = CARTESIAN_POINT ( 'NONE',  ( 17.96484262340118221, 49.93868534415484106, 7.964842623401181321 ) ) ;
#65083 = CARTESIAN_POINT ( 'NONE',  ( 19.89103541497711447, 5.662345557925709372, -6.479102184480793447 ) ) ;
#65084 = CARTESIAN_POINT ( 'NONE',  ( 17.96484262340118221, 39.93868534415484106, 7.964842623401181321 ) ) ;
#65085 = CARTESIAN_POINT ( 'NONE',  ( 1.354709868695515684, 0.5000000000000004441, 14.93870011653152652 ) ) ;
#65088 = ORIENTED_EDGE ( 'NONE', *, *, #52392, .T. ) ;
#65087 = CIRCLE ( 'NONE', #82676, 1.249999999999987121 ) ;
#65086 = CYLINDRICAL_SURFACE ( 'NONE', #52132, 6.349999999999995204 ) ;
#65089 = CARTESIAN_POINT ( 'NONE',  ( 7.361572987183169658, 19.96726448433411960, -9.846743663894592657 ) ) ;
#65090 = ORIENTED_EDGE ( 'NONE', *, *, #34635, .T. ) ;
#65091 = CARTESIAN_POINT ( 'NONE',  ( 11.40632860308399366, -69.21585191270298765, 4.000000000000000000 ) ) ;
#65092 = CARTESIAN_POINT ( 'NONE',  ( 10.00000000000000178, 57.25893115100078745, 9.846743663894594434 ) ) ;
#65093 = CARTESIAN_POINT ( 'NONE',  ( -39.69000000000001194, 92.00000000000000000, 9.500000000000000000 ) ) ;
#65094 = CARTESIAN_POINT ( 'NONE',  ( 16.40814093676323893, 50.79030133659708923, 11.09922568453595026 ) ) ;
#65095 = ADVANCED_FACE ( 'NONE', ( #18163 ), #75356, .F. ) ;
#65096 = FACE_OUTER_BOUND ( 'NONE', #31100, .T. ) ;
#65097 = STYLED_ITEM ( 'NONE', ( #28186 ), #11973 ) ;
#65098 = VERTEX_POINT ( 'NONE', #45083 ) ;
#65099 = DIRECTION ( 'NONE',  ( 0.000000000000000000, -0.000000000000000000, -1.000000000000000000 ) ) ;
#65100 = CARTESIAN_POINT ( 'NONE',  ( -1.354709868695410657, 14.49999999999999822, -14.93870011653153718 ) ) ;
#65102 = CARTESIAN_POINT ( 'NONE',  ( 12.63842701281683034, 27.46726448433411250, 9.846743663894596210 ) ) ;
#65101 = LINE ( 'NONE', #97621, #78568 ) ;
#65103 = CARTESIAN_POINT ( 'NONE',  ( -2.266590686148945544, 66.38708216824730357, -7.082119434687050408 ) ) ;
#65104 = CARTESIAN_POINT ( 'NONE',  ( -3.750000000000000888, 1.019547802438465212, 4.000000000000000000 ) ) ;
#65105 = ORIENTED_EDGE ( 'NONE', *, *, #38299, .F. ) ;
#65106 = DIRECTION ( 'NONE',  ( -1.000000000000000000, 0.000000000000000000, 0.000000000000000000 ) ) ;
#65107 = CARTESIAN_POINT ( 'NONE',  ( 14.92337183194729633, 32.67559781766745175, 8.527530157486181039 ) ) ;
#65108 = CARTESIAN_POINT ( 'NONE',  ( 22.81628187352647785, 1.415301336597087012, 3.434112377981063169 ) ) ;
#65109 = CARTESIAN_POINT ( 'NONE',  ( 2.035157376598822676, 67.43868534415484817, -7.964842623401177768 ) ) ;
#65110 = VECTOR ( 'NONE', #4045, 1000.000000000000000 ) ;
#65111 = CARTESIAN_POINT ( 'NONE',  ( 34.56412365047464874, 28.99999999999999645, -7.000000000000000888 ) ) ;
#65112 = EDGE_CURVE ( 'NONE', #16145, #17262, #44086, .T. ) ;
#65113 = CARTESIAN_POINT ( 'NONE',  ( 19.84674366389459621, 8.508931151000785675, 7.409399052514197653E-17 ) ) ;
#65114 = CARTESIAN_POINT ( 'NONE',  ( 12.63842701281683034, 62.46726448433410894, 9.846743663894596210 ) ) ;
#65115 = CIRCLE ( 'NONE', #90682, 0.2500000000000002220 ) ;
#65116 = CARTESIAN_POINT ( 'NONE',  ( 2.602085213965210642E-15, 78.91966277462714174, 9.500000000000000000 ) ) ;
#65117 = EDGE_CURVE ( 'NONE', #1561, #22307, #88350, .T. ) ;
#65118 = EDGE_CURVE ( 'NONE', #23568, #88606, #7262, .T. ) ;
#65119 = ORIENTED_EDGE ( 'NONE', *, *, #29798, .T. ) ;
#65120 = CARTESIAN_POINT ( 'NONE',  ( 19.42250999205614193, 15.14701867748817143, 5.440088680355555262 ) ) ;
#65121 = CARTESIAN_POINT ( 'NONE',  ( -2.266590686148945544, 2.220415501580634388, 7.082119434687048631 ) ) ;
#65122 = CARTESIAN_POINT ( 'NONE',  ( 7.361572987183170547, 12.05059781766744997, 9.846743663894590881 ) ) ;
#65123 = CARTESIAN_POINT ( 'NONE',  ( 12.91533473730992121, 44.52201867748816966, 10.88017736071110164 ) ) ;
#65125 = DIRECTION ( 'NONE',  ( 0.000000000000000000, 0.000000000000000000, -1.000000000000000000 ) ) ;
#65124 = CARTESIAN_POINT ( 'NONE',  ( 19.38216949554541202, 30.99863466993042138, 9.382169495545424454 ) ) ;
#65126 = CARTESIAN_POINT ( 'NONE',  ( -0.8801773607110991993, 7.855352010821504471, -2.915334737309923874 ) ) ;
#65127 = CARTESIAN_POINT ( 'NONE',  ( -6.000000000000014211, 80.07179676972448590, -6.500000000000000888 ) ) ;
#65128 = CARTESIAN_POINT ( 'NONE',  ( 66.76470751278411342, 40.99999999999997868, -9.500000000000000000 ) ) ;
#65129 = CARTESIAN_POINT ( 'NONE',  ( 1.472469842513823179, 46.42559781766745175, 4.923371831947296329 ) ) ;
#65130 = CARTESIAN_POINT ( 'NONE',  ( 19.84674366389459266, 18.71726448433411960, -2.638427012816827677 ) ) ;
#65131 = CARTESIAN_POINT ( 'NONE',  ( 10.88017736071109987, -24.22798132251182324, -2.915334737309928315 ) ) ;
#65132 = CARTESIAN_POINT ( 'NONE',  ( 21.09922568453595559, 27.04030133659708568, -6.408140936763230044 ) ) ;
#65133 = CARTESIAN_POINT ( 'NONE',  ( 14.99999999999997691, 80.32179676972448590, 4.250000000000000000 ) ) ;
#65135 = DIRECTION ( 'NONE',  ( 0.000000000000000000, -0.000000000000000000, 1.000000000000000000 ) ) ;
#65134 = CARTESIAN_POINT ( 'NONE',  ( 2.035157376598822676, 32.43868534415483396, -7.964842623401177768 ) ) ;
#65136 = LINE ( 'NONE', #66126, #67607 ) ;
#65137 = CARTESIAN_POINT ( 'NONE',  ( 22.26659068614894466, 43.88708216824729647, 7.082119434687054849 ) ) ;
#65138 = LINE ( 'NONE', #59119, #11382 ) ;
#65139 = CARTESIAN_POINT ( 'NONE',  ( 18.52753015748617571, 43.09226448433412315, 4.923371831947298993 ) ) ;
#65140 = CARTESIAN_POINT ( 'NONE',  ( 6.565887622018943937, 33.08196800326374643, -12.81628187352647608 ) ) ;
#65141 = CARTESIAN_POINT ( 'NONE',  ( 4.559911319644449179, 22.23035201082150536, -9.422509992056141925 ) ) ;
#65142 = CARTESIAN_POINT ( 'NONE',  ( 14.92337183194729633, 57.67559781766745886, 8.527530157486181039 ) ) ;
#65143 = ADVANCED_FACE ( 'NONE', ( #97135 ), #51109, .F. ) ;
#65144 = CARTESIAN_POINT ( 'NONE',  ( 7.084665262690076126, 52.02201867748816255, -10.88017736071110164 ) ) ;
#65145 = CARTESIAN_POINT ( 'NONE',  ( 19.38216949554541557, 2.248634669930420049, -9.382169495545420901 ) ) ;
#65146 = CARTESIAN_POINT ( 'NONE',  ( 20.36894250292379738, 29.92874883491396432, -10.36894250292379027 ) ) ;
#65147 = CARTESIAN_POINT ( 'NONE',  ( -14.94699059465100355, 14.63595249122795394, -1.259949270175012570 ) ) ;
#65148 = UNCERTAINTY_MEASURE_WITH_UNIT (LENGTH_MEASURE( 1.000000000000000082E-05 ), #87270, 'distance_accuracy_value', 'NONE');
#65149 = CARTESIAN_POINT ( 'NONE',  ( 5.076628168052704559, 30.17559781766745175, -8.527530157486179263 ) ) ;
#65150 = CARTESIAN_POINT ( 'NONE',  ( 3.591859063236761518, 64.95696800326376774, 11.09922568453594849 ) ) ;
#65151 = CARTESIAN_POINT ( 'NONE',  ( -2.816281873526471635, -1.084698663402913210, -3.434112377981056508 ) ) ;
#65152 = EDGE_LOOP ( 'NONE', ( #45328, #69090, #66950, #59294 ) ) ;
#65153 = EDGE_CURVE ( 'NONE', #33705, #18498, #28605, .T. ) ;
#65154 = CARTESIAN_POINT ( 'NONE',  ( 21.92686044187656336, 6.979976035794174472, 3.195792623639536423 ) ) ;
#65155 = CARTESIAN_POINT ( 'NONE',  ( -0.8801773607110991993, 7.855352010821506248, -2.915334737309923874 ) ) ;
#65156 = CARTESIAN_POINT ( 'NONE',  ( 15.44008868035555793, 61.39701867748817676, -9.422509992056140149 ) ) ;
#65158 = LINE ( 'NONE', #95676, #44569 ) ;
#65157 = CARTESIAN_POINT ( 'NONE',  ( 10.00000000000000178, 23.05374883491397142, 14.16423886937410082 ) ) ;
#65159 = CARTESIAN_POINT ( 'NONE',  ( 19.42250999205614548, 65.98035201082151957, -5.440088680355545492 ) ) ;
#65160 = CARTESIAN_POINT ( 'NONE',  ( 18.52753015748618282, 43.92559781766745175, -4.923371831947291888 ) ) ;
#65161 = CARTESIAN_POINT ( 'NONE',  ( -0.8801773607110991993, 27.85535201082150181, -2.915334737309923874 ) ) ;
#65162 = CARTESIAN_POINT ( 'NONE',  ( 0.8801356535991349261, 124.4373638429518962, 5.000000000000000000 ) ) ;
#65163 = FACE_OUTER_BOUND ( 'NONE', #24394, .T. ) ;
#65164 = ORIENTED_EDGE ( 'NONE', *, *, #52775, .T. ) ;
#65165 = AXIS2_PLACEMENT_3D ( 'NONE', #3007, #19460, #2522 ) ;
#65166 = DIRECTION ( 'NONE',  ( -1.000000000000000000, 0.000000000000000000, 0.000000000000000000 ) ) ;
#65167 = ORIENTED_EDGE ( 'NONE', *, *, #73729, .F. ) ;
#65168 = VERTEX_POINT ( 'NONE', #20115 ) ;
#65169 = LINE ( 'NONE', #42684, #83689 ) ;
#65170 = CARTESIAN_POINT ( 'NONE',  ( -2.266590686148945544, 11.38708216824730179, -7.082119434687050408 ) ) ;
#65171 = CARTESIAN_POINT ( 'NONE',  ( -0.3689425029237898834, 16.17874883491396076, -10.36894250292378850 ) ) ;
#65172 = CARTESIAN_POINT ( 'NONE',  ( 4.559911319644449179, 48.89701867748817676, 9.422509992056141925 ) ) ;
#65173 = CARTESIAN_POINT ( 'NONE',  ( 13.79529636645030344, 58.26208216824728936, 14.16423886937410614 ) ) ;
#65174 = CARTESIAN_POINT ( 'NONE',  ( 5.076628168052704559, 60.17559781766745175, -8.527530157486179263 ) ) ;
#65175 = CARTESIAN_POINT ( 'NONE',  ( 0.1532563361054100626, 35.80059781766745175, -2.638427012816831230 ) ) ;
#65177 = CARTESIAN_POINT ( 'NONE',  ( 0.1532563361054083140, 56.00893115100078745, 1.131784320476157264E-15 ) ) ;
#65176 = CARTESIAN_POINT ( 'NONE',  ( 17.96484262340118221, 31.18868534415483751, -7.964842623401177768 ) ) ;
#65178 = CARTESIAN_POINT ( 'NONE',  ( 20.36894250292379382, 48.67874883491396076, 10.36894250292379205 ) ) ;
#65179 = CARTESIAN_POINT ( 'NONE',  ( -0.3689425029237881626, 67.42874883491396076, 10.36894250292379027 ) ) ;
#65180 = CARTESIAN_POINT ( 'NONE',  ( 19.89220837332776171, 14.74062864464239375, 6.478736007405961672 ) ) ;
#65181 = SPHERICAL_SURFACE ( 'NONE', #73109, 0.2500000000000000000 ) ;
#65182 = AXIS2_PLACEMENT_3D ( 'NONE', #52905, #61881, #54379 ) ;
#65183 = CARTESIAN_POINT ( 'NONE',  ( 2.638427012816835227, -37.53273551566588395, 9.846743663894590881 ) ) ;
#65184 = EDGE_LOOP ( 'NONE', ( #48121, #51622, #41632, #40021 ) ) ;
#65185 = DIRECTION ( 'NONE',  ( 0.000000000000000000, 0.000000000000000000, -1.000000000000000000 ) ) ;
#65186 = ORIENTED_EDGE ( 'NONE', *, *, #27317, .F. ) ;
#65187 = CARTESIAN_POINT ( 'NONE',  ( 2.791683348922237240, 25.38393115100078390, -7.208316651077763204 ) ) ;
#65188 = ORIENTED_EDGE ( 'NONE', *, *, #89283, .T. ) ;
#65189 = CARTESIAN_POINT ( 'NONE',  ( 22.26659068614895176, 29.72041550158063572, -7.082119434687042414 ) ) ;
#65190 = CARTESIAN_POINT ( 'NONE',  ( 10.00000000000000000, 29.75893115100078745, -9.846743663894594434 ) ) ;
#65191 = CARTESIAN_POINT ( 'NONE',  ( 15.44008868035555793, 56.39701867748817676, -9.422509992056140149 ) ) ;
#65192 = AXIS2_PLACEMENT_3D ( 'NONE', #24433, #39430, #68940 ) ;
#65193 = CARTESIAN_POINT ( 'NONE',  ( 9.399392868737814766, 4.153235915537064750E-16, -11.04089732309474314 ) ) ;
#65194 = AXIS2_PLACEMENT_3D ( 'NONE', #58055, #27563, #20065 ) ;
#65195 = CARTESIAN_POINT ( 'NONE',  ( 20.88017736071110875, 55.77201867748816966, -2.915334737309920765 ) ) ;
#65196 = CARTESIAN_POINT ( 'NONE',  ( -5.204170427930421283E-15, 12.87363466993042493, -12.81628187352647608 ) ) ;
#65197 = VERTEX_POINT ( 'NONE', #35614 ) ;
#65198 = CARTESIAN_POINT ( 'NONE',  ( 7.084665262690076126, 49.10535201082149825, 10.88017736071109987 ) ) ;
#65199 = CARTESIAN_POINT ( 'NONE',  ( 10.00000000000000178, 18.05374883491396787, 14.16423886937410082 ) ) ;
#65200 = ORIENTED_EDGE ( 'NONE', *, *, #1567, .F. ) ;
#65201 = EDGE_LOOP ( 'NONE', ( #28920, #25057, #60780, #90470 ) ) ;
#65202 = CARTESIAN_POINT ( 'NONE',  ( -1.099225684535947600, 49.54030133659708923, 6.408140936763237150 ) ) ;
#65203 = CARTESIAN_POINT ( 'NONE',  ( 20.88017736071110519, 20.56368534415484106, 2.639326808657452039E-16 ) ) ;
#65204 = B_SPLINE_CURVE_WITH_KNOTS ( 'NONE', 3,
 ( #57718, #73211, #13211, #13711 ),
 .UNSPECIFIED., .F., .F.,
 ( 4, 4 ),
 ( 0.000000000000000000, 0.002657014572711316816 ),
 .UNSPECIFIED. ) ;
#65205 = CARTESIAN_POINT ( 'NONE',  ( 7.361572987183169658, 19.96726448433411960, -9.846743663894592657 ) ) ;
#65206 = CARTESIAN_POINT ( 'NONE',  ( 12.91533473730992121, 19.52201867748816611, 10.88017736071110164 ) ) ;
#65207 = CARTESIAN_POINT ( 'NONE',  ( 22.81628187352647785, 51.62363466993042493, 6.195893100308588602E-16 ) ) ;
#65208 = CARTESIAN_POINT ( 'NONE',  ( -46.43544119129187209, 103.9441758960464028, -5.610234333949387420 ) ) ;
#65209 = CARTESIAN_POINT ( 'NONE',  ( 0.1532563361054083140, 36.00893115100078745, 1.131784320476157264E-15 ) ) ;
#65210 = EDGE_CURVE ( 'NONE', #43044, #94701, #13108, .T. ) ;
#65211 = DIRECTION ( 'NONE',  ( 0.3007057995042701770, 0.000000000000000000, 0.9537169507482278208 ) ) ;
#65212 = DIRECTION ( 'NONE',  ( 1.000000000000000000, 0.000000000000000000, -0.000000000000000000 ) ) ;
#65213 = CARTESIAN_POINT ( 'NONE',  ( -9.383795276901610194, 0.2306972965111761253, -11.62679839395705272 ) ) ;
#65214 = FACE_OUTER_BOUND ( 'NONE', #42887, .T. ) ;
#65215 = CARTESIAN_POINT ( 'NONE',  ( 18.52753015748617571, 8.092264484334117824, 4.923371831947298993 ) ) ;
#65216 = CARTESIAN_POINT ( 'NONE',  ( -2.816281873526471635, 23.91530133659708568, -3.434112377981056508 ) ) ;
#65217 = CARTESIAN_POINT ( 'NONE',  ( 17.20831665107776587, 37.88393115100078745, 7.208316651077764980 ) ) ;
#65218 = PLANE ( 'NONE',  #60191 ) ;
#65219 = CARTESIAN_POINT ( 'NONE',  ( 13.79529636645031943, 25.34541550158063572, -14.16423886937409904 ) ) ;
#65220 = CARTESIAN_POINT ( 'NONE',  ( 10.00000000000000178, 27.25893115100078390, 9.846743663894594434 ) ) ;
#65221 = CARTESIAN_POINT ( 'NONE',  ( 3.591859063236761518, 34.95696800326375353, 11.09922568453594849 ) ) ;
#65223 = SURFACE_SIDE_STYLE ('',( #34732 ) ) ;
#65222 = CARTESIAN_POINT ( 'NONE',  ( 18.29284471827482150, 15.40189080397285259, -6.499999999999984901 ) ) ;
#65224 = CARTESIAN_POINT ( 'NONE',  ( 12.91533473730993009, 56.60535201082151247, -10.88017736071109987 ) ) ;
#65225 = ADVANCED_FACE ( 'NONE', ( #36615 ), #48348, .T. ) ;
#65226 = CARTESIAN_POINT ( 'NONE',  ( 22.81628187352647785, 1.415301336597087012, 3.434112377981063169 ) ) ;
#65227 = CARTESIAN_POINT ( 'NONE',  ( -10.76493118081678091, 2.303929616531696922E-16, -9.902252441915882386 ) ) ;
#65228 = CARTESIAN_POINT ( 'NONE',  ( 0.1532563361054082862, 31.21726448433412315, 2.638427012816831674 ) ) ;
#65229 = CARTESIAN_POINT ( 'NONE',  ( 17.96484262340118221, 29.93868534415484106, 7.964842623401181321 ) ) ;
#65230 = CARTESIAN_POINT ( 'NONE',  ( -2.816281873526473856, 29.12363466993041783, 9.499525473075851096E-16 ) ) ;
#65231 = APPLICATION_PROTOCOL_DEFINITION ( 'draft international standard', 'automotive_design', 1998, #72970 ) ;
#65232 = CARTESIAN_POINT ( 'NONE',  ( -11.21074626900200677, 89.89919991260448739, 6.510369878059174553 ) ) ;
#65233 = ADVANCED_FACE ( 'NONE', ( #66607 ), #29574, .T. ) ;
#65234 = CARTESIAN_POINT ( 'NONE',  ( 20.88017736071110164, 30.35535201082151247, 2.915334737309930979 ) ) ;
#65235 = ADVANCED_FACE ( 'NONE', ( #6596 ), #89107, .F. ) ;
#65236 = CARTESIAN_POINT ( 'NONE',  ( -9.742785792574931492, 3.338468844518207579, 5.625000000000008882 ) ) ;
#65237 = CARTESIAN_POINT ( 'NONE',  ( -0.8801773607111009756, 3.063685344154837509, 1.068504757029289695E-15 ) ) ;
#65239 = CARTESIAN_POINT ( 'NONE',  ( 0.5774900079438607392, 33.48035201082150536, 5.440088680355550821 ) ) ;
#65238 = CARTESIAN_POINT ( 'NONE',  ( 14.92337183194729988, 54.34226448433412315, -8.527530157486177487 ) ) ;
#65240 = DIRECTION ( 'NONE',  ( 0.000000000000000000, 1.000000000000000000, 0.000000000000000000 ) ) ;
#65241 = CARTESIAN_POINT ( 'NONE',  ( 17.96484262340118221, 61.18868534415482685, -7.964842623401177768 ) ) ;
#65242 = PRESENTATION_LAYER_ASSIGNMENT (  '', '', ( #9386 ) ) ;
#65244 = CARTESIAN_POINT ( 'NONE',  ( -0.000000000000000000, 78.34227958332743924, -8.952513576680836138 ) ) ;
#65243 = CARTESIAN_POINT ( 'NONE',  ( -0.8801773607111009756, 28.06368534415484106, 1.068504757029289695E-15 ) ) ;
#65245 = CARTESIAN_POINT ( 'NONE',  ( 1.472469842513823179, 5.592264484334118713, -4.923371831947296329 ) ) ;
#65246 = DIRECTION ( 'NONE',  ( -1.000000000000000000, 0.000000000000000000, 0.000000000000000000 ) ) ;
#65247 = CARTESIAN_POINT ( 'NONE',  ( 1.472469842513823179, 46.42559781766745175, 4.923371831947296329 ) ) ;
#65248 = CARTESIAN_POINT ( 'NONE',  ( -4.164238869374099039, 51.80374883491396787, 8.674139862899312516E-16 ) ) ;
#65249 = LINE ( 'NONE', #95777, #36984 ) ;
#65250 = CARTESIAN_POINT ( 'NONE',  ( 20.36894250292379738, 14.92874883491396432, -10.36894250292379027 ) ) ;
#65251 = CIRCLE ( 'NONE', #70071, 14.49999999999999822 ) ;
#65252 = CARTESIAN_POINT ( 'NONE',  ( -0.3689425029237881626, 32.42874883491395366, 10.36894250292379027 ) ) ;
#65253 = CARTESIAN_POINT ( 'NONE',  ( -2.816281873526473856, -0.8763653300695799508, 9.499525473075851096E-16 ) ) ;
#65254 = DIRECTION ( 'NONE',  ( 0.8038568606172245001, 0.000000000000000000, -0.5948227867513318223 ) ) ;
#65255 = ORIENTED_EDGE ( 'NONE', *, *, #95402, .T. ) ;
#65256 = CARTESIAN_POINT ( 'NONE',  ( 2.917880565312948704, 62.63708216824730357, 12.26659068614894643 ) ) ;
#65257 = CARTESIAN_POINT ( 'NONE',  ( 14.92337183194729988, 39.34226448433412315, -8.527530157486177487 ) ) ;
#65258 = FACE_OUTER_BOUND ( 'NONE', #68662, .T. ) ;
#65259 = CARTESIAN_POINT ( 'NONE',  ( 15.44008868035555260, 59.73035201082151247, 9.422509992056143702 ) ) ;
#65260 = CYLINDRICAL_SURFACE ( 'NONE', #85522, 2.000000000000001776 ) ;
#65261 = CARTESIAN_POINT ( 'NONE',  ( -1.099225684535947600, 58.70696800326375353, -6.408140936763238038 ) ) ;
#65262 = CARTESIAN_POINT ( 'NONE',  ( 13.43411237798105340, 30.58196800326374998, 12.81628187352647963 ) ) ;
#65263 = CARTESIAN_POINT ( 'NONE',  ( 7.361572987183170547, 27.05059781766745175, 9.846743663894590881 ) ) ;
#65264 = ORIENTED_EDGE ( 'NONE', *, *, #69675, .F. ) ;
#65265 = CARTESIAN_POINT ( 'NONE',  ( 0.1532563361054082862, 1.217264484334117824, 2.638427012816831674 ) ) ;
#65266 = EDGE_CURVE ( 'NONE', #24761, #62099, #35577, .T. ) ;
#65267 = CARTESIAN_POINT ( 'NONE',  ( 18.72515096720569971, 5.055090184799359676, 6.500000000000000000 ) ) ;
#65268 = CARTESIAN_POINT ( 'NONE',  ( 10.00000000000000178, 4.313685344154837509, 10.88017736071110342 ) ) ;
#65269 = CARTESIAN_POINT ( 'NONE',  ( -0.8801773607110991993, 17.85535201082150536, -2.915334737309923874 ) ) ;
#65270 = CARTESIAN_POINT ( 'NONE',  ( 6.204703633549690345, 42.84541550158063217, 14.16423886937410082 ) ) ;
#65271 = CARTESIAN_POINT ( 'NONE',  ( 4.559911319644449179, 32.23035201082150536, -9.422509992056141925 ) ) ;
#65272 = CARTESIAN_POINT ( 'NONE',  ( 7.084665262690076126, 69.10535201082151957, 10.88017736071109987 ) ) ;
#65273 = LINE ( 'NONE', #88287, #17631 ) ;
#65274 = CARTESIAN_POINT ( 'NONE',  ( -4.873787042390612001, -0.03417435944610275333, -13.39061984619925916 ) ) ;
#65275 = CARTESIAN_POINT ( 'NONE',  ( 5.076628168052704559, 5.175597817667451750, -8.527530157486179263 ) ) ;
#65276 = CARTESIAN_POINT ( 'NONE',  ( -7.750000000000000000, 0.000000000000000000, -3.750000000000000000 ) ) ;
#65277 =( NAMED_UNIT ( * ) SI_UNIT ( $, .STERADIAN. ) SOLID_ANGLE_UNIT ( ) );
#65278 = CARTESIAN_POINT ( 'NONE',  ( 0.1532563361054083140, 36.00893115100078745, 1.131784320476157264E-15 ) ) ;
#65279 = CARTESIAN_POINT ( 'NONE',  ( 0.6178305044545818747, -1.501365330069579951, -9.382169495545419124 ) ) ;
#65280 = CIRCLE ( 'NONE', #9414, 10.09999999999999787 ) ;
#65281 = CARTESIAN_POINT ( 'NONE',  ( 19.42250999205614193, 25.14701867748817321, 5.440088680355555262 ) ) ;
#65282 = B_SPLINE_CURVE_WITH_KNOTS ( 'NONE', 3,
 ( #51182, #81664, #65180, #5692, #28059, #20576 ),
 .UNSPECIFIED., .F., .F.,
 ( 4, 2, 4 ),
 ( 0.000000000000000000, 0.0002565770811490966858, 0.0005131541622981933715 ),
 .UNSPECIFIED. ) ;
#65283 = EDGE_CURVE ( 'NONE', #62023, #92057, #96629, .T. ) ;
#65284 = VERTEX_POINT ( 'NONE', #83088 ) ;
#65285 = CARTESIAN_POINT ( 'NONE',  ( 21.09922568453595559, 52.04030133659708923, -6.408140936763230044 ) ) ;
#65286 = LINE ( 'NONE', #26808, #49219 ) ;
#65287 = CARTESIAN_POINT ( 'NONE',  ( 10.00000000000000178, 69.31368534415484817, 10.88017736071110342 ) ) ;
#65288 = CARTESIAN_POINT ( 'NONE',  ( 12.63842701281683922, 24.55059781766745175, -9.846743663894590881 ) ) ;
#65290 = CARTESIAN_POINT ( 'NONE',  ( 14.92337183194729633, 22.67559781766745175, 8.527530157486181039 ) ) ;
#65289 = CARTESIAN_POINT ( 'NONE',  ( 20.36894250292379738, 64.92874883491397497, -10.36894250292379027 ) ) ;
#65291 = DIRECTION ( 'NONE',  ( 1.000000000000000000, 2.569960705150826877E-16, -0.000000000000000000 ) ) ;
#65292 = LINE ( 'NONE', #80808, #15177 ) ;
#65293 = CARTESIAN_POINT ( 'NONE',  ( 13.79529636645030344, 28.26208216824729647, 14.16423886937410614 ) ) ;
#65294 = CARTESIAN_POINT ( 'NONE',  ( 12.63842701281683034, 37.46726448433411605, 9.846743663894596210 ) ) ;
#65295 = CARTESIAN_POINT ( 'NONE',  ( -5.999999999999994671, 43.00000000000000000, 6.500000000000000888 ) ) ;
#65296 = CARTESIAN_POINT ( 'NONE',  ( -0.8801773607110991993, 27.85535201082150181, -2.915334737309923874 ) ) ;
#65297 = CARTESIAN_POINT ( 'NONE',  ( 15.44008868035555260, 64.73035201082151957, 9.422509992056143702 ) ) ;
#65298 = CIRCLE ( 'NONE', #81223, 15.00000000000000000 ) ;
#65299 = DIRECTION ( 'NONE',  ( 0.000000000000000000, 0.000000000000000000, 1.000000000000000000 ) ) ;
#65300 = VERTEX_POINT ( 'NONE', #14617 ) ;
#65301 = CARTESIAN_POINT ( 'NONE',  ( -2.816281873526473856, 44.33196800326375353, 3.434112377981055619 ) ) ;
#65302 = CARTESIAN_POINT ( 'NONE',  ( -0.8801773607110991993, 52.85535201082151247, -2.915334737309923874 ) ) ;
#65303 = ORIENTED_EDGE ( 'NONE', *, *, #4857, .T. ) ;
#65304 = CARTESIAN_POINT ( 'NONE',  ( 18.04007052943771683, 63.01528370094808196, 5.767676674365856293 ) ) ;
#65305 = LINE ( 'NONE', #94831, #30646 ) ;
#65306 = FACE_OUTER_BOUND ( 'NONE', #12022, .T. ) ;
#65307 = VERTEX_POINT ( 'NONE', #75588 ) ;
#65308 = CARTESIAN_POINT ( 'NONE',  ( 10.00000000000000178, 69.31368534415484817, 10.88017736071110342 ) ) ;
#65309 = CARTESIAN_POINT ( 'NONE',  ( 19.42250999205614193, 10.14701867748816966, 5.440088680355555262 ) ) ;
#65310 = CARTESIAN_POINT ( 'NONE',  ( 0.2751277870542969683, 2.282175860852373894, -6.500000000000000888 ) ) ;
#65311 = CARTESIAN_POINT ( 'NONE',  ( 0.2751277870542967463, 70.00000000000000000, 6.000000000000000000 ) ) ;
#65312 = CARTESIAN_POINT ( 'NONE',  ( 19.42250999205614193, 5.147018677488171434, 5.440088680355555262 ) ) ;
#65313 = CARTESIAN_POINT ( 'NONE',  ( 7.361572987183170547, 7.050597817667451750, 9.846743663894590881 ) ) ;
#65314 = CARTESIAN_POINT ( 'NONE',  ( 13.79529636645031943, 15.34541550158063750, -14.16423886937409904 ) ) ;
#65315 = CARTESIAN_POINT ( 'NONE',  ( 19.42250999205614548, 25.98035201082150891, -5.440088680355545492 ) ) ;
#65316 = CARTESIAN_POINT ( 'NONE',  ( 19.84674366389459621, 58.50893115100078745, 7.409399052514197653E-17 ) ) ;
#65317 = ORIENTED_EDGE ( 'NONE', *, *, #73608, .F. ) ;
#65318 = B_SPLINE_CURVE_WITH_KNOTS ( 'NONE', 3,
 ( #45964, #76453, #7969, #38953, #38467, #23955 ),
 .UNSPECIFIED., .F., .F.,
 ( 4, 2, 4 ),
 ( 0.000000000000000000, 0.0002565770811490986915, 0.0005131541622981973831 ),
 .UNSPECIFIED. ) ;
#65319 = CARTESIAN_POINT ( 'NONE',  ( 7.361572987183169658, 54.96726448433413026, -9.846743663894592657 ) ) ;
#65320 = ORIENTED_EDGE ( 'NONE', *, *, #75170, .T. ) ;
#65321 = VECTOR ( 'NONE', #39759, 1000.000000000000000 ) ;
#65322 = ADVANCED_FACE ( 'NONE', ( #20619 ), #43112, .T. ) ;
#65323 = CARTESIAN_POINT ( 'NONE',  ( 12.91533473730992121, 54.52201867748816255, 10.88017736071110164 ) ) ;
#65324 = CARTESIAN_POINT ( 'NONE',  ( 0.000000000000000000, 0.000000000000000000, 0.000000000000000000 ) ) ;
#65325 = CARTESIAN_POINT ( 'NONE',  ( 21.09922568453595559, 37.04030133659708923, -6.408140936763230044 ) ) ;
#65327 = DIRECTION ( 'NONE',  ( -0.000000000000000000, -1.000000000000000000, -0.000000000000000000 ) ) ;
#65326 = CARTESIAN_POINT ( 'NONE',  ( 2.035157376598824452, 8.688685344154839285, 7.964842623401179544 ) ) ;
#65328 = CARTESIAN_POINT ( 'NONE',  ( 4.559911319644449179, 63.89701867748817676, 9.422509992056141925 ) ) ;
#65329 = CARTESIAN_POINT ( 'NONE',  ( 4.559911319644449179, 8.897018677488173211, 9.422509992056141925 ) ) ;
#65330 = ADVANCED_FACE ( 'NONE', ( #74090 ), #39164, .T. ) ;
#65331 = STYLED_ITEM ( 'NONE', ( #98074 ), #60430 ) ;
#65332 = CARTESIAN_POINT ( 'NONE',  ( 19.38216949554541557, 47.24863466993041783, -9.382169495545420901 ) ) ;
#65333 = CARTESIAN_POINT ( 'NONE',  ( 2.035157376598822676, 27.43868534415483396, -7.964842623401177768 ) ) ;
#65334 = CARTESIAN_POINT ( 'NONE',  ( -7.993154516101138363, 0.04922511925147102924, 12.39982181464608679 ) ) ;
#65335 = ORIENTED_EDGE ( 'NONE', *, *, #45830, .T. ) ;
#65336 = CARTESIAN_POINT ( 'NONE',  ( -1.099225684535947600, 43.70696800326375353, -6.408140936763238038 ) ) ;
#65337 = CARTESIAN_POINT ( 'NONE',  ( 15.44008868035555260, 29.73035201082150891, 9.422509992056143702 ) ) ;
#65338 = CARTESIAN_POINT ( 'NONE',  ( 2.791683348922237240, 50.38393115100078035, -7.208316651077763204 ) ) ;
#65339 = VERTEX_POINT ( 'NONE', #63920 ) ;
#65340 = DIRECTION ( 'NONE',  ( 0.000000000000000000, 0.000000000000000000, 1.000000000000000000 ) ) ;
#65341 = CARTESIAN_POINT ( 'NONE',  ( 12.63842701281683922, 59.55059781766744464, -9.846743663894590881 ) ) ;
#65343 = CARTESIAN_POINT ( 'NONE',  ( 2.791683348922237240, 55.38393115100078745, -7.208316651077763204 ) ) ;
#65342 = CARTESIAN_POINT ( 'NONE',  ( 19.72487221294570858, 70.00000000000000000, 6.000000000000000000 ) ) ;
#65344 = CARTESIAN_POINT ( 'NONE',  ( -0.8801773607111009756, 18.06368534415484106, 1.068504757029289695E-15 ) ) ;
#65345 = CARTESIAN_POINT ( 'NONE',  ( 17.20831665107776587, 39.13393115100079456, -7.208316651077762316 ) ) ;
#65346 = CARTESIAN_POINT ( 'NONE',  ( 11.29168986245492157, 0.2301502372707088795, 9.783658503027474751 ) ) ;
#65347 = CARTESIAN_POINT ( 'NONE',  ( -12.74414838903266123, 15.00000000000000888, -7.178093659842149421 ) ) ;
#65348 = VECTOR ( 'NONE', #53496, 1000.000000000000000 ) ;
#65350 = CARTESIAN_POINT ( 'NONE',  ( 19.84674366389459266, 8.717264484334116048, -2.638427012816827677 ) ) ;
#65349 = CARTESIAN_POINT ( 'NONE',  ( 0.1532563361054083140, 36.00893115100078745, 1.131784320476157264E-15 ) ) ;
#65351 = CARTESIAN_POINT ( 'NONE',  ( 1.472469842513823179, 0.5922644843341181575, -4.923371831947296329 ) ) ;
#65353 = ORIENTED_EDGE ( 'NONE', *, *, #36355, .F. ) ;
#65352 = CARTESIAN_POINT ( 'NONE',  ( 7.361572987183169658, 59.96726448433410894, -9.846743663894592657 ) ) ;
#65354 =( LENGTH_UNIT ( ) NAMED_UNIT ( * ) SI_UNIT ( .MILLI., .METRE. ) );
#65355 = ADVANCED_FACE ( 'NONE', ( #47457 ), #1512, .T. ) ;
#65356 = CARTESIAN_POINT ( 'NONE',  ( 3.591859063236761518, 39.95696800326375353, 11.09922568453594849 ) ) ;
#65357 = CARTESIAN_POINT ( 'NONE',  ( 7.361572987183169658, 39.96726448433411605, -9.846743663894592657 ) ) ;
#65358 = CARTESIAN_POINT ( 'NONE',  ( -3.999999999999994671, 43.00000000000000711, 4.250000000000000000 ) ) ;
#65359 = CARTESIAN_POINT ( 'NONE',  ( 10.00000000000000178, 53.05374883491396787, 14.16423886937410082 ) ) ;
#65360 = CARTESIAN_POINT ( 'NONE',  ( 19.84674366389459621, 38.50893115100078745, 7.409399052514197653E-17 ) ) ;
#65361 = ADVANCED_FACE ( 'NONE', ( #56923 ), #4926, .T. ) ;
#65362 = CARTESIAN_POINT ( 'NONE',  ( -0.2418659066527637791, 40.11633188102327097, 6.114288769123057854 ) ) ;
#65363 = CARTESIAN_POINT ( 'NONE',  ( 2.917880565312948704, 57.63708216824731068, 12.26659068614894643 ) ) ;
#65364 = CARTESIAN_POINT ( 'NONE',  ( 12.83294900548068007, 14.49999999999999112, -7.766300266068417280 ) ) ;
#65365 = CARTESIAN_POINT ( 'NONE',  ( 20.88017736071110875, 5.772018677488170546, -2.915334737309920765 ) ) ;
#65366 = CARTESIAN_POINT ( 'NONE',  ( 17.08211943468705840, 40.13708216824731068, -12.26659068614894466 ) ) ;
#65368 = CYLINDRICAL_SURFACE ( 'NONE', #54168, 0.5000000000000004441 ) ;
#65367 = CARTESIAN_POINT ( 'NONE',  ( -0.3689425029237881626, 47.42874883491396787, 10.36894250292379027 ) ) ;
#65369 = CARTESIAN_POINT ( 'NONE',  ( 7.640985187756951014, 14.95037103177511284, 12.62032702734131995 ) ) ;
#65370 = CARTESIAN_POINT ( 'NONE',  ( 19.84674366389459266, 8.717264484334116048, -2.638427012816827677 ) ) ;
#65372 = CARTESIAN_POINT ( 'NONE',  ( 19.38216949554541202, 0.9986346699304200492, 9.382169495545424454 ) ) ;
#65371 = CARTESIAN_POINT ( 'NONE',  ( 0.8952175423694923584, 28.52576239577082262, 5.990408912944333863 ) ) ;
#65373 = ORIENTED_EDGE ( 'NONE', *, *, #95318, .F. ) ;
#65374 = CARTESIAN_POINT ( 'NONE',  ( 4.559911319644449179, 53.89701867748817676, 9.422509992056141925 ) ) ;
#65375 = CARTESIAN_POINT ( 'NONE',  ( -0.1038446121089043328, 64.24302437010796041, -6.337995344473781323 ) ) ;
#65376 = CARTESIAN_POINT ( 'NONE',  ( 17.20831665107776587, 47.88393115100078745, 7.208316651077764980 ) ) ;
#65377 = CARTESIAN_POINT ( 'NONE',  ( -46.93999999999855532, 100.4992147295316585, -9.114672001458391293 ) ) ;
#65378 = CARTESIAN_POINT ( 'NONE',  ( 17.20831665107776587, 49.13393115100078745, -7.208316651077762316 ) ) ;
#65379 = CARTESIAN_POINT ( 'NONE',  ( -0.3689425029237898834, 1.178748834913967869, -10.36894250292378850 ) ) ;
#65380 = EDGE_CURVE ( 'NONE', #66734, #75199, #42917, .T. ) ;
#65381 = CARTESIAN_POINT ( 'NONE',  ( 22.26659068614895176, 29.72041550158063572, -7.082119434687042414 ) ) ;
#65382 = EDGE_CURVE ( 'NONE', #7455, #61223, #28404, .T. ) ;
#65383 = SURFACE_SIDE_STYLE ('',( #41931 ) ) ;
#65385 = PLANE ( 'NONE',  #91782 ) ;
#65384 = CARTESIAN_POINT ( 'NONE',  ( 19.72487221294571569, 19.78217586085237301, 6.499999999999990230 ) ) ;
#65386 = CARTESIAN_POINT ( 'NONE',  ( 20.88017736071110164, 15.35535201082150358, 2.915334737309930979 ) ) ;
#65387 = CARTESIAN_POINT ( 'NONE',  ( -1.099225684535947600, 34.54030133659708923, 6.408140936763237150 ) ) ;
#65388 = CARTESIAN_POINT ( 'NONE',  ( 20.15039907845753575, 62.62777174578612716, -6.262539305110073506 ) ) ;
#65389 = CARTESIAN_POINT ( 'NONE',  ( 5.076628168052703671, 11.84226448433411960, 8.527530157486179263 ) ) ;
#65390 = DIRECTION ( 'NONE',  ( 0.000000000000000000, 1.000000000000000000, 0.000000000000000000 ) ) ;
#65391 = ORIENTED_EDGE ( 'NONE', *, *, #26557, .T. ) ;
#65392 = DIRECTION ( 'NONE',  ( -1.000000000000000000, 0.000000000000000000, -0.000000000000000000 ) ) ;
#65393 = EDGE_CURVE ( 'NONE', #18967, #48000, #18942, .T. ) ;
#65394 = CARTESIAN_POINT ( 'NONE',  ( 10.00000000000000178, 28.05374883491396787, 14.16423886937410082 ) ) ;
#65395 = CARTESIAN_POINT ( 'NONE',  ( 1.959929470562123965, 21.50257860105346808, 5.767676674365579181 ) ) ;
#65396 = CARTESIAN_POINT ( 'NONE',  ( -8.375939845167600595, 15.00000000000000000, -11.52849216984310310 ) ) ;
#65397 = CARTESIAN_POINT ( 'NONE',  ( 0.5774900079438607392, 8.480352010821505360, 5.440088680355550821 ) ) ;
#65398 = DIRECTION ( 'NONE',  ( -0.000000000000000000, -1.000000000000000000, -0.000000000000000000 ) ) ;
#65399 = DIRECTION ( 'NONE',  ( 1.000000000000000000, 0.000000000000000000, 0.000000000000000000 ) ) ;
#65400 = CARTESIAN_POINT ( 'NONE',  ( 0.5774900079438590739, 42.64701867748816966, -5.440088680355550821 ) ) ;
#65401 = CARTESIAN_POINT ( 'NONE',  ( 7.084665262690076126, 54.10535201082151247, 10.88017736071109987 ) ) ;
#65402 = CARTESIAN_POINT ( 'NONE',  ( 13.43411237798106583, 17.66530133659708923, -12.81628187352647252 ) ) ;
#65403 = FACE_OUTER_BOUND ( 'NONE', #64484, .T. ) ;
#65404 = DIRECTION ( 'NONE',  ( 0.000000000000000000, -0.000000000000000000, -1.000000000000000000 ) ) ;
#65405 = CARTESIAN_POINT ( 'NONE',  ( 1.472469842513823179, 5.592264484334118713, -4.923371831947296329 ) ) ;
#65406 = B_SPLINE_CURVE_WITH_KNOTS ( 'NONE', 3,
 ( #95686, #63693, #57179, #58152, #33198, #34670 ),
 .UNSPECIFIED., .F., .F.,
 ( 4, 2, 4 ),
 ( 3.409110551496207262E-05, 0.0004400426677368006120, 0.0008459942299586391311 ),
 .UNSPECIFIED. ) ;
#65407 = DIRECTION ( 'NONE',  ( 0.000000000000000000, 0.000000000000000000, -1.000000000000000000 ) ) ;
#65408 = CARTESIAN_POINT ( 'NONE',  ( 4.559911319644449179, 47.23035201082150536, -9.422509992056141925 ) ) ;
#65409 = CARTESIAN_POINT ( 'NONE',  ( 22.81628187352647785, 1.415301336597087012, 3.434112377981063169 ) ) ;
#65410 = CARTESIAN_POINT ( 'NONE',  ( 2.035157376598822676, 62.43868534415483396, -7.964842623401177768 ) ) ;
#65411 = CARTESIAN_POINT ( 'NONE',  ( 0.1532563361054082862, 21.21726448433412315, 2.638427012816831674 ) ) ;
#65412 = CARTESIAN_POINT ( 'NONE',  ( 6.565887622018943937, 50.16530133659708213, 12.81628187352647430 ) ) ;
#65413 = CARTESIAN_POINT ( 'NONE',  ( 18.52753015748618282, 8.925597817667451750, -4.923371831947291888 ) ) ;
#65414 = ORIENTED_EDGE ( 'NONE', *, *, #84910, .T. ) ;
#65415 = CARTESIAN_POINT ( 'NONE',  ( 1.932340009482164778, 56.49127512925449679, -6.500000000000043521 ) ) ;
#65416 = DIRECTION ( 'NONE',  ( 0.9799247046208295897, 0.000000000000000000, -0.1993679344171971901 ) ) ;
#65417 = CARTESIAN_POINT ( 'NONE',  ( 2.035157376598824452, 18.68868534415484106, 7.964842623401179544 ) ) ;
#65419 = CARTESIAN_POINT ( 'NONE',  ( 13.79529636645031943, 20.34541550158063572, -14.16423886937409904 ) ) ;
#65418 = CARTESIAN_POINT ( 'NONE',  ( -2.816281873526473856, 64.12363466993042493, 9.499525473075851096E-16 ) ) ;
#65420 = CARTESIAN_POINT ( 'NONE',  ( 5.076628168052703671, 36.84226448433412315, 8.527530157486179263 ) ) ;
#65421 = AXIS2_PLACEMENT_3D ( 'NONE', #97912, #31342, #84376 ) ;
#65422 = CARTESIAN_POINT ( 'NONE',  ( 7.084665262690076126, 17.02201867748817676, -10.88017736071110164 ) ) ;
#65423 = CARTESIAN_POINT ( 'NONE',  ( 19.42250999205614193, 5.147018677488171434, 5.440088680355555262 ) ) ;
#65424 = EDGE_LOOP ( 'NONE', ( #70513, #36827, #64318, #66059, #97433, #50355 ) ) ;
#65425 = CARTESIAN_POINT ( 'NONE',  ( 20.88017736071110875, 15.77201867748817143, -2.915334737309920765 ) ) ;
#65426 = VECTOR ( 'NONE', #98219, 1000.000000000000000 ) ;
#65427 = CARTESIAN_POINT ( 'NONE',  ( 12.91533473730993009, 36.60535201082151247, -10.88017736071109987 ) ) ;
#65429 = CARTESIAN_POINT ( 'NONE',  ( 7.084665262690076126, 24.10535201082150181, 10.88017736071109987 ) ) ;
#65428 = DIRECTION ( 'NONE',  ( 0.000000000000000000, 0.000000000000000000, 1.000000000000000000 ) ) ;
#65430 = ORIENTED_EDGE ( 'NONE', *, *, #31881, .T. ) ;
#65431 = CARTESIAN_POINT ( 'NONE',  ( 20.24186590665275887, 10.59014588040357374, -6.114288769123074729 ) ) ;
#65432 = CARTESIAN_POINT ( 'NONE',  ( 4.559911319644449179, 22.23035201082150536, -9.422509992056141925 ) ) ;
#65433 = CARTESIAN_POINT ( 'NONE',  ( 13.99999999999999822, 61.00000000000000711, 5.000000000000000000 ) ) ;
#65434 = CARTESIAN_POINT ( 'NONE',  ( 2.313926553644105868E-17, 1.839999999999999636, 0.000000000000000000 ) ) ;
#65435 = CARTESIAN_POINT ( 'NONE',  ( 16.40814093676324603, 62.45696800326376064, -11.09922568453594671 ) ) ;
#65436 = CARTESIAN_POINT ( 'NONE',  ( 0.5774900079438607392, 68.48035201082150536, 5.440088680355550821 ) ) ;
#65437 = CARTESIAN_POINT ( 'NONE',  ( -0.3689425029237881626, 37.42874883491396787, 10.36894250292379027 ) ) ;
#65438 = CARTESIAN_POINT ( 'NONE',  ( 20.88017736071110875, 35.77201867748816966, -2.915334737309920765 ) ) ;
#65439 = CARTESIAN_POINT ( 'NONE',  ( -0.8801773607111008646, 23.27201867748817676, 2.915334737309923430 ) ) ;
#65440 = DIRECTION ( 'NONE',  ( 0.9762960071199360268, 0.000000000000000000, -0.2164396139380906636 ) ) ;
#65441 = CARTESIAN_POINT ( 'NONE',  ( 19.39188664607695500, 60.83703382326399378, -6.499999999999968026 ) ) ;
#65442 = CARTESIAN_POINT ( 'NONE',  ( 7.361572987183170547, 52.05059781766745175, 9.846743663894590881 ) ) ;
#65443 = SPHERICAL_SURFACE ( 'NONE', #76648, 5.999999999999998224 ) ;
#65444 = CARTESIAN_POINT ( 'NONE',  ( 7.361572987183169658, 24.96726448433412315, -9.846743663894592657 ) ) ;
#65445 = CARTESIAN_POINT ( 'NONE',  ( 9.382169495545415572, -37.75136533006957507, -9.382169495545422677 ) ) ;
#65446 = VECTOR ( 'NONE', #38348, 1000.000000000000000 ) ;
#65447 = CARTESIAN_POINT ( 'NONE',  ( 4.559911319644449179, 12.23035201082150536, -9.422509992056141925 ) ) ;
#65448 = CARTESIAN_POINT ( 'NONE',  ( 19.84674366389459621, 13.50893115100078568, 7.409399052514197653E-17 ) ) ;
#65449 = CARTESIAN_POINT ( 'NONE',  ( 10.00000000000000178, 54.31368534415484106, 10.88017736071110342 ) ) ;
#65451 = CARTESIAN_POINT ( 'NONE',  ( 16.40814093676323893, 55.79030133659708923, 11.09922568453595026 ) ) ;
#65450 = CARTESIAN_POINT ( 'NONE',  ( -0.8801773607111008646, 13.27201867748817143, 2.915334737309923430 ) ) ;
#65452 = CARTESIAN_POINT ( 'NONE',  ( 6.204703633549690345, 27.84541550158063217, 14.16423886937410082 ) ) ;
#65453 = ADVANCED_FACE ( 'NONE', ( #73398 ), #27901, .F. ) ;
#65454 = DIRECTION ( 'NONE',  ( 0.000000000000000000, 1.000000000000000000, 0.000000000000000000 ) ) ;
#65455 = CARTESIAN_POINT ( 'NONE',  ( 14.99999999999998046, 79.82179676972448590, -6.250000000000000000 ) ) ;
#65456 = ORIENTED_EDGE ( 'NONE', *, *, #62079, .F. ) ;
#65457 = CARTESIAN_POINT ( 'NONE',  ( 16.40814093676323893, 5.790301336597087456, 11.09922568453595026 ) ) ;
#65458 = CARTESIAN_POINT ( 'NONE',  ( -0.1503990784575403861, 14.24884699246888964, -6.262539305110056631 ) ) ;
#65459 = CARTESIAN_POINT ( 'NONE',  ( 0.5774900079438590739, 37.64701867748817676, -5.440088680355550821 ) ) ;
#65460 = CARTESIAN_POINT ( 'NONE',  ( -8.000000000000000000, 80.07179676972448590, 6.500000000000000888 ) ) ;
#65461 = ORIENTED_EDGE ( 'NONE', *, *, #7847, .F. ) ;
#65462 = CARTESIAN_POINT ( 'NONE',  ( 17.20831665107776587, 14.13393115100078568, -7.208316651077762316 ) ) ;
#65463 = CARTESIAN_POINT ( 'NONE',  ( 14.92337183194729988, 9.342264484334119601, -8.527530157486177487 ) ) ;
#65464 = CARTESIAN_POINT ( 'NONE',  ( 7.361572987183170547, 17.05059781766745530, 9.846743663894590881 ) ) ;
#65465 = CARTESIAN_POINT ( 'NONE',  ( 0.1532563361054100626, 15.80059781766745353, -2.638427012816831230 ) ) ;
#65466 = CARTESIAN_POINT ( 'NONE',  ( 1.472469842513823179, 5.592264484334118713, -4.923371831947296329 ) ) ;
#65468 = CARTESIAN_POINT ( 'NONE',  ( 0.2751277870542914172, 23.21833443783937767, 6.499999999999992006 ) ) ;
#65467 = CARTESIAN_POINT ( 'NONE',  ( 18.52753015748617571, 3.092264484334118269, 4.923371831947298993 ) ) ;
#65469 = CARTESIAN_POINT ( 'NONE',  ( 1.472469842513823179, 0.5922644843341181575, -4.923371831947296329 ) ) ;
#65470 = B_SPLINE_CURVE_WITH_KNOTS ( 'NONE', 3,
 ( #73501, #95024, #42528, #27023, #4052, #73012 ),
 .UNSPECIFIED., .F., .F.,
 ( 4, 2, 4 ),
 ( 0.0002800313526871184180, 0.0006862368888281838043, 0.001092442424969249353 ),
 .UNSPECIFIED. ) ;
#65472 = VERTEX_POINT ( 'NONE', #19425 ) ;
#65471 = CARTESIAN_POINT ( 'NONE',  ( 12.63842701281683922, 19.55059781766745175, -9.846743663894590881 ) ) ;
#65473 = CIRCLE ( 'NONE', #17616, 0.5000000000000004441 ) ;
#65474 = CARTESIAN_POINT ( 'NONE',  ( 3.000000000000000444, 21.83999999999999986, 3.673940397442059868E-16 ) ) ;
#65475 = EDGE_CURVE ( 'NONE', #93851, #72124, #11596, .T. ) ;
#65476 = CARTESIAN_POINT ( 'NONE',  ( 3.591859063236761518, 4.956968003263753531, 11.09922568453594849 ) ) ;
#65477 = ORIENTED_EDGE ( 'NONE', *, *, #27712, .T. ) ;
#65478 = DIRECTION ( 'NONE',  ( 0.000000000000000000, 1.000000000000000000, -0.000000000000000000 ) ) ;
#65479 = CARTESIAN_POINT ( 'NONE',  ( 20.36894250292379738, 24.92874883491396787, -10.36894250292379027 ) ) ;
#65480 = EDGE_CURVE ( 'NONE', #63345, #93709, #58595, .T. ) ;
#65481 = UNCERTAINTY_MEASURE_WITH_UNIT (LENGTH_MEASURE( 1.000000000000000082E-05 ), #35171, 'distance_accuracy_value', 'NONE');
#65482 = CARTESIAN_POINT ( 'NONE',  ( 19.72487221294570858, 0.000000000000000000, -6.500000000000000888 ) ) ;
#65483 = CARTESIAN_POINT ( 'NONE',  ( 24.16423886937409904, 14.09541550158063217, 3.795296366450317205 ) ) ;
#65484 = B_SPLINE_CURVE_WITH_KNOTS ( 'NONE', 3,
 ( #22101, #61557, #7601, #53564, #32032, #68584 ),
 .UNSPECIFIED., .F., .F.,
 ( 4, 2, 4 ),
 ( 7.755077673624249124E-18, 0.0002626113303185950102, 0.0005252226606371823226 ),
 .UNSPECIFIED. ) ;
#65485 = COLOUR_RGB ( '', 0.31764706, 0.68627451, 0.89019608) ;
#65486 = CARTESIAN_POINT ( 'NONE',  ( 13.79529636645030344, 38.26208216824729647, 14.16423886937410614 ) ) ;
#65487 = PRESENTATION_STYLE_ASSIGNMENT (( #12980 ) ) ;
#65488 = CARTESIAN_POINT ( 'NONE',  ( -14.24131928502211863, -0.03417435944610275333, 0.4973178280104966764 ) ) ;
#65489 = CARTESIAN_POINT ( 'NONE',  ( 2.035157376598824452, 33.68868534415484106, 7.964842623401179544 ) ) ;
#65490 = CARTESIAN_POINT ( 'NONE',  ( -4.000000000000000000, 78.07179676972445748, -4.250000000000000000 ) ) ;
#65491 = CARTESIAN_POINT ( 'NONE',  ( 7.361572987183170547, 17.05059781766745530, 9.846743663894590881 ) ) ;
#65494 = CIRCLE ( 'NONE', #6480, 14.49999999999999822 ) ;
#65493 = CARTESIAN_POINT ( 'NONE',  ( 1.472469842513823179, 30.59226448433411960, -4.923371831947296329 ) ) ;
#65492 = CARTESIAN_POINT ( 'NONE',  ( 17.96484262340118221, 54.93868534415484106, 7.964842623401181321 ) ) ;
#65495 = ORIENTED_EDGE ( 'NONE', *, *, #66158, .T. ) ;
#65496 = CARTESIAN_POINT ( 'NONE',  ( -0.8801773607111009756, 13.06368534415483929, 1.068504757029289695E-15 ) ) ;
#65497 = CARTESIAN_POINT ( 'NONE',  ( 21.09922568453594849, 46.20696800326376064, 6.408140936763242479 ) ) ;
#65498 = CARTESIAN_POINT ( 'NONE',  ( 0.1532563361054083140, 51.00893115100078745, 1.131784320476157264E-15 ) ) ;
#65499 = CARTESIAN_POINT ( 'NONE',  ( 6.565887622018943937, 25.16530133659708213, 12.81628187352647430 ) ) ;
#65500 = CARTESIAN_POINT ( 'NONE',  ( -12.26659068614895354, -33.61291783175269643, -7.082119434687038861 ) ) ;
#65501 = CARTESIAN_POINT ( 'NONE',  ( 10.00000000000000178, 37.25893115100078745, 9.846743663894594434 ) ) ;
#65502 = CARTESIAN_POINT ( 'NONE',  ( 24.16423886937410614, 14.30374883491396787, 8.672049930838204340E-16 ) ) ;
#65503 = ORIENTED_EDGE ( 'NONE', *, *, #97764, .T. ) ;
#65504 = B_SPLINE_CURVE_WITH_KNOTS ( 'NONE', 3,
 ( #13627, #84107, #141, #60603, #91098, #8110 ),
 .UNSPECIFIED., .F., .F.,
 ( 4, 2, 4 ),
 ( 0.0002800912045164337893, 0.0006862973266905198974, 0.001092503448864605951 ),
 .UNSPECIFIED. ) ;
#65505 = CARTESIAN_POINT ( 'NONE',  ( 7.084665262690076126, 54.10535201082151247, 10.88017736071109987 ) ) ;
#65506 = CARTESIAN_POINT ( 'NONE',  ( 20.88017736071110164, 50.35535201082151247, 2.915334737309930979 ) ) ;
#65507 = CARTESIAN_POINT ( 'NONE',  ( 6.204703633549690345, 40.76208216824731778, -14.16423886937410259 ) ) ;
#65508 = CARTESIAN_POINT ( 'NONE',  ( 0.1532563361054082862, 56.21726448433411605, 2.638427012816831674 ) ) ;
#65509 = CARTESIAN_POINT ( 'NONE',  ( 6.565887622018943937, 63.08196800326376064, -12.81628187352647608 ) ) ;
#65510 = CARTESIAN_POINT ( 'NONE',  ( 10.00000000000000000, 41.81368534415484106, -10.88017736071110342 ) ) ;
#65511 = CYLINDRICAL_SURFACE ( 'NONE', #15122, 0.2500000000000002220 ) ;
#65512 = CARTESIAN_POINT ( 'NONE',  ( 16.40814093676324603, 22.45696800326375353, -11.09922568453594671 ) ) ;
#65513 = CARTESIAN_POINT ( 'NONE',  ( 1.472469842513823179, 50.59226448433411605, -4.923371831947296329 ) ) ;
#65514 = CARTESIAN_POINT ( 'NONE',  ( 2.915334737309921209, 21.60535201082150536, -10.88017736071110164 ) ) ;
#65515 =( LENGTH_UNIT ( ) NAMED_UNIT ( * ) SI_UNIT ( .MILLI., .METRE. ) );
#65516 = CARTESIAN_POINT ( 'NONE',  ( 12.91533473730993009, 61.60535201082150536, -10.88017736071109987 ) ) ;
#65517 = ORIENTED_EDGE ( 'NONE', *, *, #66947, .T. ) ;
#65518 = EDGE_CURVE ( 'NONE', #36347, #10365, #3452, .T. ) ;
#65519 = CARTESIAN_POINT ( 'NONE',  ( 20.88017736071110875, 5.772018677488170546, -2.915334737309920765 ) ) ;
#65520 = CARTESIAN_POINT ( 'NONE',  ( 1.042145700049403656, 59.74216108172000617, -6.499999999999937828 ) ) ;
#65521 = CARTESIAN_POINT ( 'NONE',  ( 19.42250999205614548, 65.98035201082151957, -5.440088680355545492 ) ) ;
#65522 = CARTESIAN_POINT ( 'NONE',  ( 18.52753015748617571, 3.092264484334118269, 4.923371831947298993 ) ) ;
#65523 = CARTESIAN_POINT ( 'NONE',  ( 17.97400638239511750, 77.67876782659151047, -4.131022355321664286 ) ) ;
#65524 = CARTESIAN_POINT ( 'NONE',  ( 10.00000000000000000, 29.75893115100078745, -9.846743663894594434 ) ) ;
#65525 = CARTESIAN_POINT ( 'NONE',  ( 7.084665262690076126, 27.02201867748817676, -10.88017736071110164 ) ) ;
#65526 = CARTESIAN_POINT ( 'NONE',  ( -2.816281873526473856, 9.123634669930421381, 9.499525473075851096E-16 ) ) ;
#65528 = CYLINDRICAL_SURFACE ( 'NONE', #25688, 0.5000000000000004441 ) ;
#65527 = CARTESIAN_POINT ( 'NONE',  ( 2.035157376598824452, 38.68868534415483396, 7.964842623401179544 ) ) ;
#65529 = DIRECTION ( 'NONE',  ( 1.000000000000000000, -0.000000000000000000, -0.000000000000000000 ) ) ;
#65530 = CARTESIAN_POINT ( 'NONE',  ( 0.6178305044545838731, 34.74863466993042493, 9.382169495545420901 ) ) ;
#65531 = ORIENTED_EDGE ( 'NONE', *, *, #95205, .F. ) ;
#65532 = CARTESIAN_POINT ( 'NONE',  ( 7.084665262690076126, 64.10535201082150536, 10.88017736071109987 ) ) ;
#65534 = CARTESIAN_POINT ( 'NONE',  ( 18.04007052943773459, 19.00257860105348584, -5.767676674365828760 ) ) ;
#65533 = CARTESIAN_POINT ( 'NONE',  ( 10.00000000000000178, 20.37363466993042138, 12.81628187352647608 ) ) ;
#65535 = CARTESIAN_POINT ( 'NONE',  ( 10.00000000000000178, 2.258931151000784787, 9.846743663894594434 ) ) ;
#65536 = CARTESIAN_POINT ( 'NONE',  ( 17.96484262340118221, 24.93868534415484461, 7.964842623401181321 ) ) ;
#65537 = CARTESIAN_POINT ( 'NONE',  ( 13.79529636645030344, 63.26208216824730357, 14.16423886937410614 ) ) ;
#65538 = CARTESIAN_POINT ( 'NONE',  ( 19.84674366389459621, 58.50893115100078745, 7.409399052514197653E-17 ) ) ;
#65539 = CARTESIAN_POINT ( 'NONE',  ( 5.076628168052703671, 1.842264484334118047, 8.527530157486179263 ) ) ;
#65540 = CARTESIAN_POINT ( 'NONE',  ( 2.035157376598824452, 58.68868534415482685, 7.964842623401179544 ) ) ;
#65541 = CARTESIAN_POINT ( 'NONE',  ( -8.439016546561676435, 15.00000000000000000, -11.79122553965791553 ) ) ;
#65542 = CARTESIAN_POINT ( 'NONE',  ( 6.204703633549690345, 27.84541550158063217, 14.16423886937410082 ) ) ;
#65543 = CYLINDRICAL_SURFACE ( 'NONE', #59972, 0.5000000000000002220 ) ;
#65544 = AXIS2_PLACEMENT_3D ( 'NONE', #32064, #70092, #56076 ) ;
#65545 = ORIENTED_EDGE ( 'NONE', *, *, #29591, .T. ) ;
#65546 = EDGE_LOOP ( 'NONE', ( #18160, #53566, #70981, #57332 ) ) ;
#65547 = CARTESIAN_POINT ( 'NONE',  ( -2.266590686148945544, 47.22041550158063927, 7.082119434687048631 ) ) ;
#65548 = CARTESIAN_POINT ( 'NONE',  ( 20.36894250292379382, 48.67874883491396076, 10.36894250292379205 ) ) ;
#65549 = CARTESIAN_POINT ( 'NONE',  ( 5.076628168052703671, 36.84226448433412315, 8.527530157486179263 ) ) ;
#65550 = CARTESIAN_POINT ( 'NONE',  ( -13.73866367547691958, 90.95360148970608805, 7.920681552399385872 ) ) ;
#65551 = CARTESIAN_POINT ( 'NONE',  ( 3.822225673302274362, 0.000000000000000000, -3.889525102760237552 ) ) ;
#65552 = CARTESIAN_POINT ( 'NONE',  ( 24.16423886937409904, 39.09541550158062506, 3.795296366450317205 ) ) ;
#65553 = CARTESIAN_POINT ( 'NONE',  ( 10.09792486685190482, 0.04962894416274275106, -10.75589247084411859 ) ) ;
#65554 = CARTESIAN_POINT ( 'NONE',  ( 10.00000000000000000, 4.758931151000784787, -9.846743663894594434 ) ) ;
#65555 = VECTOR ( 'NONE', #23501, 1000.000000000000000 ) ;
#65556 = AXIS2_PLACEMENT_3D ( 'NONE', #98040, #13027, #66527 ) ;
#65557 = CARTESIAN_POINT ( 'NONE',  ( 0.4195498155886434599, -2.441190589077521466E-17, 10.00000000000000000 ) ) ;
#65558 = CARTESIAN_POINT ( 'NONE',  ( -4.923371831947302546, 0.1755978176674541369, -8.527530157486173934 ) ) ;
#65559 = EDGE_LOOP ( 'NONE', ( #44762, #66417, #2769, #73936, #38786, #1308 ) ) ;
#65560 = FACE_OUTER_BOUND ( 'NONE', #17890, .T. ) ;
#65561 = EDGE_LOOP ( 'NONE', ( #35424, #64006, #28096, #33383 ) ) ;
#65562 = VERTEX_POINT ( 'NONE', #80915 ) ;
#65563 = CARTESIAN_POINT ( 'NONE',  ( 10.00000000000000178, 13.05374883491396787, 14.16423886937410082 ) ) ;
#65565 = CARTESIAN_POINT ( 'NONE',  ( 0.5774900079438607392, 28.48035201082150891, 5.440088680355550821 ) ) ;
#65564 = CARTESIAN_POINT ( 'NONE',  ( 17.96484262340118221, 16.18868534415483396, -7.964842623401177768 ) ) ;
#65567 = CARTESIAN_POINT ( 'NONE',  ( -2.816281873526471635, 23.91530133659708568, -3.434112377981056508 ) ) ;
#65566 = CARTESIAN_POINT ( 'NONE',  ( 0.1532563361054100626, 45.80059781766745886, -2.638427012816831230 ) ) ;
#65568 = SURFACE_SIDE_STYLE ('',( #35069 ) ) ;
#65569 = EDGE_CURVE ( 'NONE', #40063, #53280, #42428, .T. ) ;
#65570 = EDGE_CURVE ( 'NONE', #40043, #538, #20913, .T. ) ;
#65571 = CARTESIAN_POINT ( 'NONE',  ( -1.099225684535947600, 19.54030133659708568, 6.408140936763237150 ) ) ;
#65572 = ORIENTED_EDGE ( 'NONE', *, *, #95766, .T. ) ;
#65573 = CARTESIAN_POINT ( 'NONE',  ( 1.472469842513823179, 30.59226448433411960, -4.923371831947296329 ) ) ;
#65574 = CARTESIAN_POINT ( 'NONE',  ( 22.26659068614894466, 53.88708216824731068, 7.082119434687054849 ) ) ;
#65575 = ORIENTED_EDGE ( 'NONE', *, *, #4652, .F. ) ;
#65576 = CARTESIAN_POINT ( 'NONE',  ( 22.26659068614895176, 64.72041550158064638, -7.082119434687042414 ) ) ;
#65577 = EDGE_LOOP ( 'NONE', ( #2650, #87554, #65849, #70103, #24517, #73779 ) ) ;
#65578 = CARTESIAN_POINT ( 'NONE',  ( 19.42250999205614548, 50.98035201082151247, -5.440088680355545492 ) ) ;
#65579 = CARTESIAN_POINT ( 'NONE',  ( 17.96484262340118221, 44.93868534415483396, 7.964842623401181321 ) ) ;
#65580 = CARTESIAN_POINT ( 'NONE',  ( 20.88017736071110164, 45.35535201082149115, 2.915334737309930979 ) ) ;
#65581 =( LENGTH_UNIT ( ) NAMED_UNIT ( * ) SI_UNIT ( .MILLI., .METRE. ) );
#65582 = CARTESIAN_POINT ( 'NONE',  ( 20.88017736071110875, 40.77201867748818387, -2.915334737309920765 ) ) ;
#65583 = VECTOR ( 'NONE', #86560, 1000.000000000000000 ) ;
#65584 = CARTESIAN_POINT ( 'NONE',  ( 1.354709868695618935, 0.5000000000000004441, -14.93870011653151586 ) ) ;
#65586 = VERTEX_POINT ( 'NONE', #11429 ) ;
#65585 = DIRECTION ( 'NONE',  ( -0.000000000000000000, -0.000000000000000000, -1.000000000000000000 ) ) ;
#65587 = VECTOR ( 'NONE', #28987, 1000.000000000000227 ) ;
#65588 = EDGE_CURVE ( 'NONE', #46415, #52823, #83831, .T. ) ;
#65589 = CARTESIAN_POINT ( 'NONE',  ( 12.63842701281683034, 22.46726448433411605, 9.846743663894596210 ) ) ;
#65590 = ORIENTED_EDGE ( 'NONE', *, *, #71517, .F. ) ;
#65591 = CARTESIAN_POINT ( 'NONE',  ( 7.361572987183169658, 59.96726448433410894, -9.846743663894592657 ) ) ;
#65592 = CARTESIAN_POINT ( 'NONE',  ( 4.841283923550342649, 0.2306972965111894203, 14.13506365971150025 ) ) ;
#65593 = ADVANCED_FACE ( 'NONE', ( #12902 ), #43399, .T. ) ;
#65594 = DIRECTION ( 'NONE',  ( -0.000000000000000000, 1.000000000000000000, 0.000000000000000000 ) ) ;
#65595 = VERTEX_POINT ( 'NONE', #79441 ) ;
#65596 = CARTESIAN_POINT ( 'NONE',  ( -3.499999999999998668, 1.019547802438465434, 3.750000000000000000 ) ) ;
#65598 = CARTESIAN_POINT ( 'NONE',  ( 18.52753015748618282, 28.92559781766745175, -4.923371831947291888 ) ) ;
#65597 = CARTESIAN_POINT ( 'NONE',  ( 1.472469842513823179, 66.42559781766745175, 4.923371831947296329 ) ) ;
#65599 = CARTESIAN_POINT ( 'NONE',  ( 2.917880565312948704, 67.63708216824730357, 12.26659068614894643 ) ) ;
#65600 = VERTEX_POINT ( 'NONE', #10939 ) ;
#65601 =( BOUNDED_CURVE ( )  B_SPLINE_CURVE ( 2, ( #73381, #5408, #52364, #42899, #96909, #43379, #13885, #27392, #20400, #66877, #89869, #65879, #74868 ),
 .UNSPECIFIED., .F., .T. ) 
 B_SPLINE_CURVE_WITH_KNOTS ( ( 3, 2, 2, 2, 2, 2, 3 ),
 ( 0.5999999999999999778, 0.6055555555555555136, 0.6111111111111111605, 0.6166666666666666963, 0.6222222222222222321, 0.6277777777777777679, 0.6333333333333333037 ),
 .UNSPECIFIED. ) 
 CURVE ( )  GEOMETRIC_REPRESENTATION_ITEM ( )  RATIONAL_B_SPLINE_CURVE ( ( 1.000000000000000000, 0.9659258262890683122, 1.000000000000000000, 0.9659258262890683122, 1.000000000000000000, 0.9659258262890683122, 1.000000000000000000, 0.9659258262890683122, 1.000000000000000000, 0.9659258262890683122, 1.000000000000000000, 0.9659258262890683122, 1.000000000000000000 ) ) 
 REPRESENTATION_ITEM ( '' )  );
#65602 = LINE ( 'NONE', #95627, #81514 ) ;
#65603 = CARTESIAN_POINT ( 'NONE',  ( 10.00000000000000000, 29.75893115100078745, -9.846743663894594434 ) ) ;
#65604 = CARTESIAN_POINT ( 'NONE',  ( 0.6178305044545838731, 59.74863466993041783, 9.382169495545420901 ) ) ;
#65605 = EDGE_LOOP ( 'NONE', ( #16744, #75699, #97730, #65477 ) ) ;
#65606 = CARTESIAN_POINT ( 'NONE',  ( 22.81628187352647785, 6.415301336597088344, 3.434112377981063169 ) ) ;
#65607 = CARTESIAN_POINT ( 'NONE',  ( 0.1532563361054083140, 16.00893115100078390, 1.131784320476157264E-15 ) ) ;
#65608 = CARTESIAN_POINT ( 'NONE',  ( -10.39655283154069743, 14.95077488074853456, -10.46698568711278732 ) ) ;
#65609 = CARTESIAN_POINT ( 'NONE',  ( 12.63842701281683922, 9.550597817667449974, -9.846743663894590881 ) ) ;
#65610 = CARTESIAN_POINT ( 'NONE',  ( 17.20831665107776587, 54.13393115100079456, -7.208316651077762316 ) ) ;
#65611 = CARTESIAN_POINT ( 'NONE',  ( 20.88017736071110519, 20.56368534415484106, 2.639326808657452039E-16 ) ) ;
#65612 = AXIS2_PLACEMENT_3D ( 'NONE', #80539, #95544, #43515 ) ;
#65613 = ORIENTED_EDGE ( 'NONE', *, *, #69598, .F. ) ;
#65614 = CARTESIAN_POINT ( 'NONE',  ( 20.88017736071110875, 10.77201867748817143, -2.915334737309920765 ) ) ;
#65615 = CARTESIAN_POINT ( 'NONE',  ( 2.917880565312950480, 10.97041550158063572, -12.26659068614894821 ) ) ;
#65616 = CARTESIAN_POINT ( 'NONE',  ( 17.20831665107776587, 17.88393115100078745, 7.208316651077764980 ) ) ;
#65617 = CARTESIAN_POINT ( 'NONE',  ( 12.91533473730992121, 54.52201867748816255, 10.88017736071110164 ) ) ;
#65618 = AXIS2_PLACEMENT_3D ( 'NONE', #50789, #28767, #96801 ) ;
#65620 = CARTESIAN_POINT ( 'NONE',  ( 1.379999999999981908, 20.99999999999999645, 0.000000000000000000 ) ) ;
#65619 = CARTESIAN_POINT ( 'NONE',  ( 16.40814093676323893, 20.79030133659708923, 11.09922568453595026 ) ) ;
#65621 = CARTESIAN_POINT ( 'NONE',  ( -0.8801773607111008646, 3.272018677488171434, 2.915334737309923430 ) ) ;
#65622 = CARTESIAN_POINT ( 'NONE',  ( -1.926860441876563801, 57.66212336850780673, 1.004413902775740978E-15 ) ) ;
#65623 = DIRECTION ( 'NONE',  ( -1.483861936729427615E-16, 1.000000000000000000, 0.000000000000000000 ) ) ;
#65624 = CARTESIAN_POINT ( 'NONE',  ( 13.43411237798106583, 7.665301336597086568, -12.81628187352647252 ) ) ;
#65625 = CARTESIAN_POINT ( 'NONE',  ( 10.00000000000000178, 62.25893115100078745, 9.846743663894594434 ) ) ;
#65626 = CARTESIAN_POINT ( 'NONE',  ( 0.1532563361054083140, 11.00893115100078568, 1.131784320476157264E-15 ) ) ;
#65627 = CARTESIAN_POINT ( 'NONE',  ( -2.915334737309934532, -27.97798132251182679, -10.88017736071109987 ) ) ;
#65628 = CARTESIAN_POINT ( 'NONE',  ( 21.09922568453594849, 26.20696800326375353, 6.408140936763242479 ) ) ;
#65629 = CARTESIAN_POINT ( 'NONE',  ( -11.17367748615327372, -90.30033005415631919, -4.000000000000000000 ) ) ;
#65631 = LINE ( 'NONE', #72152, #63938 ) ;
#65630 = CARTESIAN_POINT ( 'NONE',  ( 7.084665262690076126, 27.02201867748817676, -10.88017736071110164 ) ) ;
#65632 = CARTESIAN_POINT ( 'NONE',  ( 14.82269085861175384, 14.49999999999999112, -2.299529454046946864 ) ) ;
#65633 = CARTESIAN_POINT ( 'NONE',  ( 10.00000000000000178, 43.05374883491397497, 14.16423886937410082 ) ) ;
#65634 = EDGE_CURVE ( 'NONE', #48124, #10040, #61121, .T. ) ;
#65635 = CARTESIAN_POINT ( 'NONE',  ( -6.898461952320517732, 15.00000000000000000, 12.75387089053304557 ) ) ;
#65636 = CARTESIAN_POINT ( 'NONE',  ( 22.81628187352648496, 51.83196800326376064, -3.434112377981050290 ) ) ;
#65637 = CARTESIAN_POINT ( 'NONE',  ( 12.91533473730993009, 21.60535201082150536, -10.88017736071109987 ) ) ;
#65638 = CARTESIAN_POINT ( 'NONE',  ( 1.472469842513823179, 46.42559781766745175, 4.923371831947296329 ) ) ;
#65639 = CARTESIAN_POINT ( 'NONE',  ( 7.084665262690076126, 49.10535201082149825, 10.88017736071109987 ) ) ;
#65640 = CARTESIAN_POINT ( 'NONE',  ( 22.26659068614895176, 29.72041550158063572, -7.082119434687042414 ) ) ;
#65641 = LINE ( 'NONE', #96665, #91874 ) ;
#65642 = CARTESIAN_POINT ( 'NONE',  ( 19.84674366389459266, 38.71726448433412315, -2.638427012816827677 ) ) ;
#65643 = PRESENTATION_STYLE_ASSIGNMENT (( #35144 ) ) ;
#65644 = CARTESIAN_POINT ( 'NONE',  ( -2.816281873526473856, -0.6680319967362464695, 3.434112377981055619 ) ) ;
#65645 = ORIENTED_EDGE ( 'NONE', *, *, #39553, .F. ) ;
#65646 = CARTESIAN_POINT ( 'NONE',  ( 20.88017736071110875, 30.77201867748816966, -2.915334737309920765 ) ) ;
#65647 = EDGE_CURVE ( 'NONE', #8190, #30537, #14830, .T. ) ;
#65648 = CARTESIAN_POINT ( 'NONE',  ( 17.99999999999999645, 91.28723161455539525, -8.000000000000000000 ) ) ;
#65649 = CARTESIAN_POINT ( 'NONE',  ( 6.673414917871782315, -55.62670566514463388, 3.750000000000001776 ) ) ;
#65650 = CARTESIAN_POINT ( 'NONE',  ( 12.91533473730993009, 16.60535201082150891, -10.88017736071109987 ) ) ;
#65651 = CARTESIAN_POINT ( 'NONE',  ( 24.16423886937410614, 19.30374883491397142, 8.672049930838204340E-16 ) ) ;
#65652 = CARTESIAN_POINT ( 'NONE',  ( 10.00000000000000178, 17.25893115100078745, 9.846743663894594434 ) ) ;
#65653 = CARTESIAN_POINT ( 'NONE',  ( 2.791683348922240793, 66.63393115100079456, 7.208316651077764092 ) ) ;
#65654 = CARTESIAN_POINT ( 'NONE',  ( 17.96484262340118221, 39.93868534415484106, 7.964842623401181321 ) ) ;
#65655 = LINE ( 'NONE', #33676, #81468 ) ;
#65656 = LINE ( 'NONE', #27663, #44166 ) ;
#65657 = TOROIDAL_SURFACE ( 'NONE', #89581, 2.500000000000000888, 0.5000000000000000000 ) ;
#65658 = VECTOR ( 'NONE', #38961, 999.9999999999998863 ) ;
#65659 = EDGE_LOOP ( 'NONE', ( #88206, #24510, #57096, #26126, #80360, #14181 ) ) ;
#65660 = DIRECTION ( 'NONE',  ( 1.000000000000000000, 0.000000000000000000, 0.000000000000000000 ) ) ;
#65661 = CARTESIAN_POINT ( 'NONE',  ( 12.63842701281683034, 47.46726448433412315, 9.846743663894596210 ) ) ;
#65662 = VERTEX_POINT ( 'NONE', #13903 ) ;
#65663 = ORIENTED_EDGE ( 'NONE', *, *, #82988, .F. ) ;
#65664 = CIRCLE ( 'NONE', #9730, 0.5000000000000004441 ) ;
#65665 = LINE ( 'NONE', #3220, #10177 ) ;
#65666 = CARTESIAN_POINT ( 'NONE',  ( -0.3689425029237881626, 12.42874883491396609, 10.36894250292379027 ) ) ;
#65667 = CARTESIAN_POINT ( 'NONE',  ( 24.16423886937410614, 14.51208216824730179, -3.795296366450302550 ) ) ;
#65668 = CARTESIAN_POINT ( 'NONE',  ( 15.44008868035555793, 51.39701867748816966, -9.422509992056140149 ) ) ;
#65669 = CARTESIAN_POINT ( 'NONE',  ( -4.164238869374098151, 56.59541550158063927, -3.795296366450310543 ) ) ;
#65670 = CARTESIAN_POINT ( 'NONE',  ( 19.38216949554541202, 5.998634669930420493, 9.382169495545424454 ) ) ;
#65671 = CARTESIAN_POINT ( 'NONE',  ( 12.63842701281683034, 37.46726448433411605, 9.846743663894596210 ) ) ;
#65672 = CARTESIAN_POINT ( 'NONE',  ( -10.60846096436510422, -98.07574024450978811, 4.000000000000000000 ) ) ;
#65674 = CARTESIAN_POINT ( 'NONE',  ( 13.43411237798105340, 10.58196800326375353, 12.81628187352647963 ) ) ;
#65673 = CARTESIAN_POINT ( 'NONE',  ( 0.5774900079438607392, 33.48035201082150536, 5.440088680355550821 ) ) ;
#65675 = CARTESIAN_POINT ( 'NONE',  ( -2.266590686148945544, 7.220415501580634832, 7.082119434687048631 ) ) ;
#65676 = CARTESIAN_POINT ( 'NONE',  ( -4.164238869374098151, 51.59541550158063217, -3.795296366450310543 ) ) ;
#65677 = CARTESIAN_POINT ( 'NONE',  ( 2.035157376598824452, 8.688685344154839285, 7.964842623401179544 ) ) ;
#65678 = CARTESIAN_POINT ( 'NONE',  ( 2.815433093577024426, 15.00000000000000000, 14.73340885523751709 ) ) ;
#65679 = DIRECTION ( 'NONE',  ( 0.000000000000000000, 0.000000000000000000, -1.000000000000000000 ) ) ;
#65680 = CARTESIAN_POINT ( 'NONE',  ( -9.846743663894596210, -34.19940218233254825, -2.638427012816824124 ) ) ;
#65681 = EDGE_LOOP ( 'NONE', ( #83786, #68294, #48787, #17639 ) ) ;
#65682 = DIRECTION ( 'NONE',  ( -0.000000000000000000, -1.000000000000000000, 0.000000000000000000 ) ) ;
#65683 = ORIENTED_EDGE ( 'NONE', *, *, #16714, .T. ) ;
#65684 = PRESENTATION_LAYER_ASSIGNMENT (  '', '', ( #9814 ) ) ;
#65685 = ORIENTED_EDGE ( 'NONE', *, *, #32162, .T. ) ;
#65686 = CARTESIAN_POINT ( 'NONE',  ( -2.266590686148945544, 52.22041550158064638, 7.082119434687048631 ) ) ;
#65687 = CARTESIAN_POINT ( 'NONE',  ( 19.84674366389459266, 43.30059781766744464, 2.638427012816836559 ) ) ;
#65688 = CARTESIAN_POINT ( 'NONE',  ( 2.035157376598824452, 63.68868534415484106, 7.964842623401179544 ) ) ;
#65689 = CARTESIAN_POINT ( 'NONE',  ( 24.35999999999999233, 37.99999999999997868, -7.000000000000000888 ) ) ;
#65690 = EDGE_CURVE ( 'NONE', #15070, #68783, #74380, .T. ) ;
#65691 = AXIS2_PLACEMENT_3D ( 'NONE', #84972, #78454, #9968 ) ;
#65692 = CARTESIAN_POINT ( 'NONE',  ( 2.035157376598824452, 48.68868534415483396, 7.964842623401179544 ) ) ;
#65693 = EDGE_CURVE ( 'NONE', #26466, #27072, #48847, .T. ) ;
#65694 = EDGE_CURVE ( 'NONE', #9024, #87326, #25742, .T. ) ;
#65695 = CARTESIAN_POINT ( 'NONE',  ( 11.09922568453594671, 2.040301336597091897, -6.408140936763241591 ) ) ;
#65696 = VERTEX_POINT ( 'NONE', #21906 ) ;
#65697 = CARTESIAN_POINT ( 'NONE',  ( 13.79529636645030344, 23.26208216824730002, 14.16423886937410614 ) ) ;
#65698 = CARTESIAN_POINT ( 'NONE',  ( 3.591859063236763294, 28.29030133659708568, -11.09922568453595026 ) ) ;
#65699 = VERTEX_POINT ( 'NONE', #98414 ) ;
#65700 = CARTESIAN_POINT ( 'NONE',  ( 22.81628187352647785, 41.62363466993042493, 6.195893100308588602E-16 ) ) ;
#65701 = CARTESIAN_POINT ( 'NONE',  ( 0.1532563361054082862, 36.21726448433410894, 2.638427012816831674 ) ) ;
#65702 = CARTESIAN_POINT ( 'NONE',  ( 0.5774900079438590739, 7.647018677488171434, -5.440088680355550821 ) ) ;
#65703 = MECHANICAL_DESIGN_GEOMETRIC_PRESENTATION_REPRESENTATION (  '', ( #89625 ), #78500 ) ;
#65704 = CARTESIAN_POINT ( 'NONE',  ( 6.565887622018943937, 50.16530133659708213, 12.81628187352647430 ) ) ;
#65705 = EDGE_CURVE ( 'NONE', #93129, #81651, #29870, .T. ) ;
#65706 = CARTESIAN_POINT ( 'NONE',  ( -8.000000000000000000, 40.99999999999999289, -6.250000000000000000 ) ) ;
#65707 = CARTESIAN_POINT ( 'NONE',  ( 17.20831665107776587, 42.88393115100077324, 7.208316651077764980 ) ) ;
#65708 = CARTESIAN_POINT ( 'NONE',  ( 20.15039907845753220, 22.62777174578612716, -6.262539305110077947 ) ) ;
#65709 = CARTESIAN_POINT ( 'NONE',  ( -1.915564264621230972, 4.378229052359348391E-16, -14.37291249357993372 ) ) ;
#65710 = DIRECTION ( 'NONE',  ( 0.000000000000000000, 0.000000000000000000, -1.000000000000000000 ) ) ;
#65711 = CARTESIAN_POINT ( 'NONE',  ( -9.282040431732539787, 1.863472483959460746E-16, -11.30407325590354439 ) ) ;
#65712 = CARTESIAN_POINT ( 'NONE',  ( 0.2751277870542982451, 17.28217586085238011, -6.500000000000002665 ) ) ;
#65713 = CARTESIAN_POINT ( 'NONE',  ( 0.1532563361054100626, 15.80059781766745353, -2.638427012816831230 ) ) ;
#65714 = CARTESIAN_POINT ( 'NONE',  ( 3.591859063236761518, 24.95696800326375353, 11.09922568453594849 ) ) ;
#65715 = EDGE_CURVE ( 'NONE', #89674, #61056, #83476, .T. ) ;
#65716 = DIRECTION ( 'NONE',  ( 0.000000000000000000, 1.000000000000000000, -0.000000000000000000 ) ) ;
#65717 = ORIENTED_EDGE ( 'NONE', *, *, #98936, .F. ) ;
#65718 = CARTESIAN_POINT ( 'NONE',  ( -13.48255862861917009, 15.00000000000000000, -5.335786055104346559 ) ) ;
#65719 = CARTESIAN_POINT ( 'NONE',  ( -4.164238869374099927, 17.01208216824730357, 3.795296366450308767 ) ) ;
#65720 = CARTESIAN_POINT ( 'NONE',  ( 10.00000000000000000, 34.75893115100078745, -9.846743663894594434 ) ) ;
#65721 = CARTESIAN_POINT ( 'NONE',  ( 13.43411237798105340, 40.58196800326375353, 12.81628187352647963 ) ) ;
#65723 =( NAMED_UNIT ( * ) PLANE_ANGLE_UNIT ( ) SI_UNIT ( $, .RADIAN. ) );
#65722 = FACE_OUTER_BOUND ( 'NONE', #64802, .T. ) ;
#65724 = CARTESIAN_POINT ( 'NONE',  ( 2.035157376598822676, 57.43868534415484106, -7.964842623401177768 ) ) ;
#65725 = CARTESIAN_POINT ( 'NONE',  ( -2.816281873526473856, 14.12363466993041961, 9.499525473075851096E-16 ) ) ;
#65726 = FACE_OUTER_BOUND ( 'NONE', #75267, .T. ) ;
#65727 = CARTESIAN_POINT ( 'NONE',  ( 0.1532563361054082862, 41.21726448433411605, 2.638427012816831674 ) ) ;
#65728 = CARTESIAN_POINT ( 'NONE',  ( 0.5774900079438607392, 43.48035201082151247, 5.440088680355550821 ) ) ;
#65729 = CARTESIAN_POINT ( 'NONE',  ( -1.099225684535947600, 38.70696800326375353, -6.408140936763238038 ) ) ;
#65730 = CARTESIAN_POINT ( 'NONE',  ( 12.63842701281683034, 37.46726448433411605, 9.846743663894596210 ) ) ;
#65731 = CARTESIAN_POINT ( 'NONE',  ( -209.0297971069972220, -96.11055066635684341, -48.62461743031692407 ) ) ;
#65732 = CARTESIAN_POINT ( 'NONE',  ( -11.93818897418494984, 90.30657785595315090, 6.860068911468413688 ) ) ;
#65733 = CARTESIAN_POINT ( 'NONE',  ( 10.00000000000000000, 36.81368534415484106, -10.88017736071110342 ) ) ;
#65734 = B_SPLINE_CURVE_WITH_KNOTS ( 'NONE', 3,
 ( #81431, #36433, #13429, #21936, #35436, #28432 ),
 .UNSPECIFIED., .F., .F.,
 ( 4, 2, 4 ),
 ( 7.788919273297050532E-18, 0.0002626113303185990760, 0.0005252226606371903457 ),
 .UNSPECIFIED. ) ;
#65735 = ORIENTED_EDGE ( 'NONE', *, *, #60753, .T. ) ;
#65736 = CARTESIAN_POINT ( 'NONE',  ( 4.559911319644449179, 68.89701867748817676, 9.422509992056141925 ) ) ;
#65737 = CARTESIAN_POINT ( 'NONE',  ( 0.5774900079438607392, 3.480352010821504027, 5.440088680355550821 ) ) ;
#65739 = CARTESIAN_POINT ( 'NONE',  ( 4.559911319644449179, 32.23035201082150536, -9.422509992056141925 ) ) ;
#65738 = CARTESIAN_POINT ( 'NONE',  ( 1.472469842513823179, 55.59226448433412315, -4.923371831947296329 ) ) ;
#65740 = FACE_OUTER_BOUND ( 'NONE', #35598, .T. ) ;
#65741 = CARTESIAN_POINT ( 'NONE',  ( 19.42250999205614193, 60.14701867748817676, 5.440088680355555262 ) ) ;
#65743 = CARTESIAN_POINT ( 'NONE',  ( 2.602085213965210642E-15, 78.91966277462714174, -9.500000000000000000 ) ) ;
#65742 = CARTESIAN_POINT ( 'NONE',  ( 20.88017736071110875, 30.77201867748816966, -2.915334737309920765 ) ) ;
#65744 = CARTESIAN_POINT ( 'NONE',  ( 19.84674366389459621, 18.50893115100078745, 7.409399052514197653E-17 ) ) ;
#65745 = LINE ( 'NONE', #5760, #56899 ) ;
#65746 = CARTESIAN_POINT ( 'NONE',  ( 7.361572987183170547, 47.05059781766745175, 9.846743663894590881 ) ) ;
#65748 = CARTESIAN_POINT ( 'NONE',  ( 20.32896413005680358, 19.74545670184113888, 5.963430220938287007 ) ) ;
#65747 = CARTESIAN_POINT ( 'NONE',  ( 24.16423886937409904, 54.09541550158063217, 3.795296366450317205 ) ) ;
#65749 = CARTESIAN_POINT ( 'NONE',  ( 1.383448333479235126, 62.37718327197428891, -6.499999999999977796 ) ) ;
#65750 = CARTESIAN_POINT ( 'NONE',  ( 17.08211943468705840, 5.137082168247300906, -12.26659068614894466 ) ) ;
#65751 = EDGE_CURVE ( 'NONE', #28589, #42131, #435, .T. ) ;
#65752 = CARTESIAN_POINT ( 'NONE',  ( -4.164238869374099039, 36.80374883491396787, 8.674139862899312516E-16 ) ) ;
#65753 = AXIS2_PLACEMENT_3D ( 'NONE', #4960, #89433, #95964 ) ;
#65754 = CARTESIAN_POINT ( 'NONE',  ( 10.00000000000000178, 0.3736346699304200492, 12.81628187352647608 ) ) ;
#65755 = CARTESIAN_POINT ( 'NONE',  ( 19.72487221294571569, 27.80223176428830811, -6.499999999999990230 ) ) ;
#65756 = VERTEX_POINT ( 'NONE', #36402 ) ;
#65757 = CARTESIAN_POINT ( 'NONE',  ( 15.44008868035555260, 19.73035201082150536, 9.422509992056143702 ) ) ;
#65758 = CARTESIAN_POINT ( 'NONE',  ( 17.20831665107776587, 39.13393115100079456, -7.208316651077762316 ) ) ;
#65760 = CARTESIAN_POINT ( 'NONE',  ( -13.42719148503548610, 90.83520141667820269, -7.724461209138739903 ) ) ;
#65759 = SURFACE_SIDE_STYLE ('',( #59246 ) ) ;
#65761 = CARTESIAN_POINT ( 'NONE',  ( 2.035157376598822676, 57.43868534415484106, -7.964842623401177768 ) ) ;
#65762 = DIRECTION ( 'NONE',  ( 1.000000000000000000, 0.000000000000000000, 0.000000000000000000 ) ) ;
#65763 = CARTESIAN_POINT ( 'NONE',  ( -2.816281873526473856, 59.33196800326374643, 3.434112377981055619 ) ) ;
#65764 = CARTESIAN_POINT ( 'NONE',  ( 13.43411237798105340, 20.58196800326374643, 12.81628187352647963 ) ) ;
#65765 = CARTESIAN_POINT ( 'NONE',  ( 2.791683348922237240, 25.38393115100078390, -7.208316651077763204 ) ) ;
#65766 = ORIENTED_EDGE ( 'NONE', *, *, #95193, .F. ) ;
#65767 = DIRECTION ( 'NONE',  ( 1.000000000000000000, -0.000000000000000000, -0.000000000000000000 ) ) ;
#65768 = CARTESIAN_POINT ( 'NONE',  ( -0.3689425029237898834, 66.17874883491396076, -10.36894250292378850 ) ) ;
#65769 = CARTESIAN_POINT ( 'NONE',  ( 20.88017736071110164, 20.35535201082150891, 2.915334737309930979 ) ) ;
#65770 = CARTESIAN_POINT ( 'NONE',  ( -4.164238869374099927, 47.01208216824729647, 3.795296366450308767 ) ) ;
#65771 = CARTESIAN_POINT ( 'NONE',  ( 17.96484262340118221, 36.18868534415484106, -7.964842623401177768 ) ) ;
#65772 = CARTESIAN_POINT ( 'NONE',  ( 19.42250999205614548, 60.98035201082151247, -5.440088680355545492 ) ) ;
#65773 = CARTESIAN_POINT ( 'NONE',  ( 20.15039907845753930, 70.00000000000000000, 6.262539305110068177 ) ) ;
#65774 = CARTESIAN_POINT ( 'NONE',  ( 18.52753015748618282, 28.92559781766745175, -4.923371831947291888 ) ) ;
#65775 = CARTESIAN_POINT ( 'NONE',  ( 19.84674366389459621, 13.50893115100078568, 7.409399052514197653E-17 ) ) ;
#65776 = AXIS2_PLACEMENT_3D ( 'NONE', #33998, #86537, #19022 ) ;
#65777 = DIRECTION ( 'NONE',  ( -0.9981347984218665870, 0.000000000000000000, -0.06104853953486361756 ) ) ;
#65778 = CARTESIAN_POINT ( 'NONE',  ( 12.63842701281683034, 37.46726448433411605, 9.846743663894596210 ) ) ;
#65779 = CARTESIAN_POINT ( 'NONE',  ( 0.1532563361054083140, 66.00893115100079456, 1.131784320476157264E-15 ) ) ;
#65780 = ORIENTED_EDGE ( 'NONE', *, *, #213, .F. ) ;
#65781 = CARTESIAN_POINT ( 'NONE',  ( 10.00000000000000178, 40.37363466993042493, 12.81628187352647608 ) ) ;
#65782 = CARTESIAN_POINT ( 'NONE',  ( 5.803070148808322948, 4.011383936018713867E-16, -13.28812917035388175 ) ) ;
#65783 = CARTESIAN_POINT ( 'NONE',  ( 10.00000000000000000, 66.81368534415484817, -10.88017736071110342 ) ) ;
#65784 = CARTESIAN_POINT ( 'NONE',  ( 16.40814093676323893, 45.79030133659708923, 11.09922568453595026 ) ) ;
#65786 = CARTESIAN_POINT ( 'NONE',  ( 19.84674366389459621, 33.50893115100078745, 7.409399052514197653E-17 ) ) ;
#65785 = CARTESIAN_POINT ( 'NONE',  ( -0.3689425029237898834, 61.17874883491396076, -10.36894250292378850 ) ) ;
#65787 = CARTESIAN_POINT ( 'NONE',  ( 19.50000000000000711, 70.00000000000000000, 5.000000000000000000 ) ) ;
#65788 = CARTESIAN_POINT ( 'NONE',  ( 0.1532563361054083140, 66.00893115100079456, 1.131784320476157264E-15 ) ) ;
#65789 = CARTESIAN_POINT ( 'NONE',  ( 22.26659068614894466, 18.88708216824730002, 7.082119434687054849 ) ) ;
#65790 = CARTESIAN_POINT ( 'NONE',  ( 22.26659068614895176, 34.72041550158063927, -7.082119434687042414 ) ) ;
#65791 = CARTESIAN_POINT ( 'NONE',  ( 2.791683348922237240, 50.38393115100078035, -7.208316651077763204 ) ) ;
#65792 = DIRECTION ( 'NONE',  ( 1.000000000000000000, 0.000000000000000000, 0.000000000000000000 ) ) ;
#65793 = CARTESIAN_POINT ( 'NONE',  ( 12.91533473730993009, 36.60535201082151247, -10.88017736071109987 ) ) ;
#65794 = CARTESIAN_POINT ( 'NONE',  ( 20.88017736071110875, 60.77201867748817676, -2.915334737309920765 ) ) ;
#65795 = CARTESIAN_POINT ( 'NONE',  ( 18.72515096720571037, 50.05509018479936856, 6.499999999999982236 ) ) ;
#65796 = ORIENTED_EDGE ( 'NONE', *, *, #17081, .F. ) ;
#65797 = CARTESIAN_POINT ( 'NONE',  ( -1.099225684535947600, 39.54030133659708923, 6.408140936763237150 ) ) ;
#65798 = EDGE_CURVE ( 'NONE', #15328, #46342, #91368, .T. ) ;
#65799 = CARTESIAN_POINT ( 'NONE',  ( 20.88017736071110875, 60.77201867748817676, -2.915334737309920765 ) ) ;
#65800 = EDGE_LOOP ( 'NONE', ( #10525, #12248, #89855, #49692, #40143, #34345 ) ) ;
#65801 = CARTESIAN_POINT ( 'NONE',  ( 22.26659068614895176, 4.720415501580633943, -7.082119434687042414 ) ) ;
#65802 = CARTESIAN_POINT ( 'NONE',  ( 0.2751277870542871429, 42.28217586085238366, -6.499999999999984901 ) ) ;
#65803 = CARTESIAN_POINT ( 'NONE',  ( 0.000000000000000000, 0.000000000000000000, -14.25000000000000000 ) ) ;
#65804 = EDGE_LOOP ( 'NONE', ( #38437, #8422, #50977, #79715 ) ) ;
#65805 = ADVANCED_FACE ( 'NONE', ( #76373 ), #68881, .F. ) ;
#65807 = EDGE_CURVE ( 'NONE', #96104, #31762, #10787, .T. ) ;
#65806 = CARTESIAN_POINT ( 'NONE',  ( 6.432108699068923130, -88.20011490510430008, 3.750000000000000000 ) ) ;
#65808 = CARTESIAN_POINT ( 'NONE',  ( 2.035157376598822676, 17.43868534415483751, -7.964842623401177768 ) ) ;
#65809 = VECTOR ( 'NONE', #81067, 1000.000000000000000 ) ;
#65810 = CARTESIAN_POINT ( 'NONE',  ( 2.917880565312950480, 15.97041550158063217, -12.26659068614894821 ) ) ;
#65811 = EDGE_CURVE ( 'NONE', #1475, #4350, #69242, .T. ) ;
#65812 = EDGE_CURVE ( 'NONE', #56002, #18731, #53366, .T. ) ;
#65813 = CARTESIAN_POINT ( 'NONE',  ( 0.5774900079438607392, 23.48035201082150536, 5.440088680355550821 ) ) ;
#65814 = CARTESIAN_POINT ( 'NONE',  ( 2.791683348922237240, 55.38393115100078745, -7.208316651077763204 ) ) ;
#65815 = EDGE_LOOP ( 'NONE', ( #98581, #58558, #82242, #95273 ) ) ;
#65816 = CARTESIAN_POINT ( 'NONE',  ( 17.20831665107776587, 59.13393115100078745, -7.208316651077762316 ) ) ;
#65817 = ORIENTED_EDGE ( 'NONE', *, *, #36870, .T. ) ;
#65818 = CARTESIAN_POINT ( 'NONE',  ( 10.00000000000000178, 54.31368534415484106, 10.88017736071110342 ) ) ;
#65819 = CARTESIAN_POINT ( 'NONE',  ( 1.472469842513823179, 60.59226448433412315, -4.923371831947296329 ) ) ;
#65820 = CARTESIAN_POINT ( 'NONE',  ( 22.81628187352647785, 36.41530133659707502, 3.434112377981063169 ) ) ;
#65822 = CARTESIAN_POINT ( 'NONE',  ( -14.89999999999999680, 98.49999999999998579, 8.000000000000000000 ) ) ;
#65821 = CARTESIAN_POINT ( 'NONE',  ( -0.8801773607110991993, 7.855352010821504471, -2.915334737309923874 ) ) ;
#65823 = CARTESIAN_POINT ( 'NONE',  ( 2.035157376598822676, 67.43868534415484817, -7.964842623401177768 ) ) ;
#65824 = CARTESIAN_POINT ( 'NONE',  ( 17.96484262340118221, 19.93868534415484106, 7.964842623401181321 ) ) ;
#65825 = ADVANCED_FACE ( 'NONE', ( #37897 ), #68389, .F. ) ;
#65826 = AXIS2_PLACEMENT_3D ( 'NONE', #56266, #95224, #4247 ) ;
#65827 = ORIENTED_EDGE ( 'NONE', *, *, #3881, .F. ) ;
#65828 = CARTESIAN_POINT ( 'NONE',  ( 0.6178305044545838731, 59.74863466993041783, 9.382169495545420901 ) ) ;
#65829 = CARTESIAN_POINT ( 'NONE',  ( 19.42250999205614193, 30.14701867748817321, 5.440088680355555262 ) ) ;
#65830 = CARTESIAN_POINT ( 'NONE',  ( 14.26139399675174957, 15.00000000000000000, 2.619664342934486356 ) ) ;
#65831 = CARTESIAN_POINT ( 'NONE',  ( 19.38216949554541557, 37.24863466993041783, -9.382169495545420901 ) ) ;
#65832 = CARTESIAN_POINT ( 'NONE',  ( 4.559911319644449179, 47.23035201082150536, -9.422509992056141925 ) ) ;
#65833 = VECTOR ( 'NONE', #89103, 1000.000000000000114 ) ;
#65834 = CARTESIAN_POINT ( 'NONE',  ( 19.84674366389459266, 53.30059781766744464, 2.638427012816836559 ) ) ;
#65836 = ORIENTED_EDGE ( 'NONE', *, *, #46871, .T. ) ;
#65835 = EDGE_CURVE ( 'NONE', #5117, #44051, #59482, .T. ) ;
#65837 = PRESENTATION_LAYER_ASSIGNMENT (  '', '', ( #56237 ) ) ;
#65838 = CIRCLE ( 'NONE', #16331, 0.5000000000000004441 ) ;
#65839 = CARTESIAN_POINT ( 'NONE',  ( 19.84674366389459266, 63.30059781766745886, 2.638427012816836559 ) ) ;
#65841 = CARTESIAN_POINT ( 'NONE',  ( 0.1532563361054082862, 51.21726448433412315, 2.638427012816831674 ) ) ;
#65840 = FACE_OUTER_BOUND ( 'NONE', #50696, .T. ) ;
#65842 = CARTESIAN_POINT ( 'NONE',  ( 15.44008868035555260, 24.73035201082150891, 9.422509992056143702 ) ) ;
#65843 = CARTESIAN_POINT ( 'NONE',  ( -14.26328062697247212, 0.04962887699556481347, 3.770429249334694255 ) ) ;
#65844 = DIRECTION ( 'NONE',  ( 0.000000000000000000, 1.000000000000000000, 0.000000000000000000 ) ) ;
#65846 = CARTESIAN_POINT ( 'NONE',  ( 10.00000000000000000, 9.758931151000785675, -9.846743663894594434 ) ) ;
#65845 = CARTESIAN_POINT ( 'NONE',  ( 19.84674366389459266, 43.30059781766744464, 2.638427012816836559 ) ) ;
#65847 = FACE_OUTER_BOUND ( 'NONE', #22954, .T. ) ;
#65849 = ORIENTED_EDGE ( 'NONE', *, *, #1437, .T. ) ;
#65848 = CARTESIAN_POINT ( 'NONE',  ( 0.1532563361054100626, 60.80059781766744464, -2.638427012816831230 ) ) ;
#65850 = ADVANCED_FACE ( 'NONE', ( #10339 ), #16858, .T. ) ;
#65851 = VECTOR ( 'NONE', #25725, 1000.000000000000000 ) ;
#65852 = CARTESIAN_POINT ( 'NONE',  ( 9.779999999999990479, 20.99999999999999645, 0.000000000000000000 ) ) ;
#65853 = CARTESIAN_POINT ( 'NONE',  ( -2.816281873526473856, 39.12363466993041783, 9.499525473075851096E-16 ) ) ;
#65854 = CARTESIAN_POINT ( 'NONE',  ( 14.92337183194729633, 32.67559781766745175, 8.527530157486181039 ) ) ;
#65855 = CARTESIAN_POINT ( 'NONE',  ( -0.8801773607111009756, 58.27201867748816966, 2.915334737309923874 ) ) ;
#65856 = CARTESIAN_POINT ( 'NONE',  ( 2.917880565312950480, 60.97041550158063927, -12.26659068614894821 ) ) ;
#65857 = CARTESIAN_POINT ( 'NONE',  ( 0.1532563361054100626, 30.80059781766744820, -2.638427012816831230 ) ) ;
#65858 = CARTESIAN_POINT ( 'NONE',  ( 4.630000000000003446, 1.019547802438462547, -4.000000000000000000 ) ) ;
#65859 = CARTESIAN_POINT ( 'NONE',  ( -2.266590686148945544, 56.38708216824731068, -7.082119434687050408 ) ) ;
#65860 = CARTESIAN_POINT ( 'NONE',  ( 7.618303901328586036, -2.732951804315999255E-15, -12.48478900416261617 ) ) ;
#65861 = CARTESIAN_POINT ( 'NONE',  ( 10.00000000000000000, 16.81368534415483751, -10.88017736071110342 ) ) ;
#65862 = CIRCLE ( 'NONE', #86648, 14.49999999999999822 ) ;
#65863 = CARTESIAN_POINT ( 'NONE',  ( -4.164238869374099927, 32.01208216824730357, 3.795296366450308767 ) ) ;
#65865 = LINE ( 'NONE', #73366, #3107 ) ;
#65864 = CARTESIAN_POINT ( 'NONE',  ( -2.266590686148945544, 52.22041550158064638, 7.082119434687048631 ) ) ;
#65866 = LINE ( 'NONE', #27868, #97929 ) ;
#65867 = CARTESIAN_POINT ( 'NONE',  ( 0.1532563361054083140, 16.00893115100078390, 1.131784320476157264E-15 ) ) ;
#65868 = CARTESIAN_POINT ( 'NONE',  ( 10.00000000000000178, 0.3736346699304200492, 12.81628187352647608 ) ) ;
#65869 = ORIENTED_EDGE ( 'NONE', *, *, #50727, .F. ) ;
#65870 = CARTESIAN_POINT ( 'NONE',  ( 17.96484262340118221, 51.18868534415483396, -7.964842623401177768 ) ) ;
#65871 = PRESENTATION_STYLE_ASSIGNMENT (( #27874 ) ) ;
#65872 = DIRECTION ( 'NONE',  ( -0.000000000000000000, 0.000000000000000000, 1.000000000000000000 ) ) ;
#65873 = LINE ( 'NONE', #88884, #48360 ) ;
#65874 = CARTESIAN_POINT ( 'NONE',  ( 14.73551000134586531, 14.95037106540114991, 0.7225335126798774210 ) ) ;
#65875 = CIRCLE ( 'NONE', #25928, 0.2500000000000002220 ) ;
#65876 = ORIENTED_EDGE ( 'NONE', *, *, #31618, .F. ) ;
#65877 = CARTESIAN_POINT ( 'NONE',  ( 17.08211943468705840, 40.13708216824731068, -12.26659068614894466 ) ) ;
#65879 = CARTESIAN_POINT ( 'NONE',  ( -3.014428414850124138, 8.963468844518210688, 11.25000000000000178 ) ) ;
#65878 = CARTESIAN_POINT ( 'NONE',  ( 8.879999999999991900, 21.00000000000000000, 0.000000000000000000 ) ) ;
#65880 = CARTESIAN_POINT ( 'NONE',  ( 12.91533473730993009, 21.60535201082150536, -10.88017736071109987 ) ) ;
#65882 = CARTESIAN_POINT ( 'NONE',  ( 13.43411237798106583, 37.66530133659708923, -12.81628187352647252 ) ) ;
#65881 = B_SPLINE_CURVE_WITH_KNOTS ( 'NONE', 3,
 ( #92169, #90683, #45187, #98722, #91174, #36711 ),
 .UNSPECIFIED., .F., .F.,
 ( 4, 2, 4 ),
 ( 3.409110551496115105E-05, 0.0004400426677367861379, 0.0008459942299586110503 ),
 .UNSPECIFIED. ) ;
#65883 = CARTESIAN_POINT ( 'NONE',  ( -11.92686044187656513, 9.688309369127519943, 3.903127820947815962E-15 ) ) ;
#65884 = CARTESIAN_POINT ( 'NONE',  ( -1.099225684535947600, 63.70696800326376774, -6.408140936763238038 ) ) ;
#65885 = VERTEX_POINT ( 'NONE', #9850 ) ;
#65886 = CARTESIAN_POINT ( 'NONE',  ( 7.155633850256548634, -69.45312897839663435, -4.000000000000000000 ) ) ;
#65887 = CARTESIAN_POINT ( 'NONE',  ( -11.17367748577515130, -90.30033005412217051, -3.999999999999999112 ) ) ;
#65888 = SURFACE_STYLE_USAGE ( .BOTH. , #52373 ) ;
#65889 = LINE ( 'NONE', #96919, #63040 ) ;
#65890 = CARTESIAN_POINT ( 'NONE',  ( -0.8801773607111009756, 28.06368534415484106, 1.068504757029289695E-15 ) ) ;
#65891 = LINE ( 'NONE', #88903, #6326 ) ;
#65892 = CARTESIAN_POINT ( 'NONE',  ( 5.073789285385966963, 0.000000000000000000, 1.998618750576407699 ) ) ;
#65893 = CARTESIAN_POINT ( 'NONE',  ( 7.084665262690076126, 44.10535201082151247, 10.88017736071109987 ) ) ;
#65894 = CARTESIAN_POINT ( 'NONE',  ( 17.96484262340118221, 44.93868534415483396, 7.964842623401181321 ) ) ;
#65895 = CARTESIAN_POINT ( 'NONE',  ( -2.816281873526471635, 8.915301336597083903, -3.434112377981056508 ) ) ;
#65896 = CARTESIAN_POINT ( 'NONE',  ( -5.803070148808410877, 4.629725225344712954E-16, 13.28812917035384267 ) ) ;
#65897 = DIRECTION ( 'NONE',  ( 0.04361938736533305799, 0.000000000000000000, 0.9990482215818579093 ) ) ;
#65898 = CARTESIAN_POINT ( 'NONE',  ( 17.20831665107776587, 22.88393115100078745, 7.208316651077764980 ) ) ;
#65899 = LINE ( 'NONE', #34910, #1420 ) ;
#65900 = ADVANCED_FACE ( 'NONE', ( #93335 ), #71338, .T. ) ;
#65901 = CARTESIAN_POINT ( 'NONE',  ( 17.96484262340118221, 44.93868534415483396, 7.964842623401181321 ) ) ;
#65902 = CARTESIAN_POINT ( 'NONE',  ( 21.09922568453595559, 7.040301336597086568, -6.408140936763230044 ) ) ;
#65903 = CARTESIAN_POINT ( 'NONE',  ( 17.96484262340118221, 66.18868534415483396, -7.964842623401177768 ) ) ;
#65904 = CARTESIAN_POINT ( 'NONE',  ( 2.791683348922237240, 25.38393115100078390, -7.208316651077763204 ) ) ;
#65905 = CARTESIAN_POINT ( 'NONE',  ( 0.6178305044545818747, 48.49863466993042493, -9.382169495545419124 ) ) ;
#65906 = CIRCLE ( 'NONE', #45147, 11.92686044187656513 ) ;
#65907 = CARTESIAN_POINT ( 'NONE',  ( 12.63842701281683034, 2.467264484334118269, 9.846743663894596210 ) ) ;
#65908 = CIRCLE ( 'NONE', #43570, 15.00000000000000000 ) ;
#65909 = ORIENTED_EDGE ( 'NONE', *, *, #80971, .F. ) ;
#65910 = CARTESIAN_POINT ( 'NONE',  ( 8.879999999999991900, 76.07179676972447169, 4.250000000000000000 ) ) ;
#65911 = LINE ( 'NONE', #95941, #9488 ) ;
#65912 = CARTESIAN_POINT ( 'NONE',  ( -0.8801773607111009756, 18.06368534415484106, 1.068504757029289695E-15 ) ) ;
#65914 = CARTESIAN_POINT ( 'NONE',  ( 13.79529636645031943, 35.34541550158063927, -14.16423886937409904 ) ) ;
#65913 = DIRECTION ( 'NONE',  ( 0.08715574274765114371, 0.9961946980917462113, 0.000000000000000000 ) ) ;
#65915 = CARTESIAN_POINT ( 'NONE',  ( 19.84674366389459621, 33.50893115100078745, 7.409399052514197653E-17 ) ) ;
#65916 = CIRCLE ( 'NONE', #27586, 3.000000000000000888 ) ;
#65917 = CARTESIAN_POINT ( 'NONE',  ( -0.8801773607110991993, 12.85535201082150358, -2.915334737309923874 ) ) ;
#65918 = CARTESIAN_POINT ( 'NONE',  ( 24.16423886937409904, 64.09541550158064638, 3.795296366450317205 ) ) ;
#65919 = VERTEX_POINT ( 'NONE', #24855 ) ;
#65920 = AXIS2_PLACEMENT_3D ( 'NONE', #95276, #25336, #18309 ) ;
#65921 = CARTESIAN_POINT ( 'NONE',  ( 2.035157376598824452, 8.688685344154839285, 7.964842623401179544 ) ) ;
#65922 = CARTESIAN_POINT ( 'NONE',  ( 15.44008868035555793, 36.39701867748816966, -9.422509992056140149 ) ) ;
#65923 = CARTESIAN_POINT ( 'NONE',  ( -11.96291822454869802, 15.00000000000000000, -8.193813980849247613 ) ) ;
#65924 = VERTEX_POINT ( 'NONE', #39368 ) ;
#65925 = CARTESIAN_POINT ( 'NONE',  ( 19.72487221294570858, 70.00000000000000000, 6.500000000000000888 ) ) ;
#65927 = ADVANCED_FACE ( 'NONE', ( #55338 ), #77834, .T. ) ;
#65926 = CARTESIAN_POINT ( 'NONE',  ( -0.8801773607110991993, 22.85535201082150181, -2.915334737309923874 ) ) ;
#65928 = CARTESIAN_POINT ( 'NONE',  ( -3.750000000000000000, 10.00000000000000000, -3.750000000000000000 ) ) ;
#65929 = CARTESIAN_POINT ( 'NONE',  ( -6.000000000000009770, 41.24999999999999289, 6.500000000000000888 ) ) ;
#65930 = CARTESIAN_POINT ( 'NONE',  ( -1.099225684535947600, 59.54030133659708923, 6.408140936763237150 ) ) ;
#65931 = DIRECTION ( 'NONE',  ( -1.000000000000000000, 0.000000000000000000, 0.000000000000000000 ) ) ;
#65932 = CARTESIAN_POINT ( 'NONE',  ( 24.16423886937410614, 34.51208216824731068, -3.795296366450302550 ) ) ;
#65933 = CARTESIAN_POINT ( 'NONE',  ( 10.00000000000000178, 54.31368534415484106, 10.88017736071110342 ) ) ;
#65934 = CARTESIAN_POINT ( 'NONE',  ( 19.42250999205614193, 30.14701867748817321, 5.440088680355555262 ) ) ;
#65936 = B_SPLINE_CURVE_WITH_KNOTS ( 'NONE', 3,
 ( #77828, #62329, #92837, #54828, #85340, #47328 ),
 .UNSPECIFIED., .F., .F.,
 ( 4, 2, 4 ),
 ( 0.0002800008091676944129, 0.0006862060465022835464, 0.001092411283836872788 ),
 .UNSPECIFIED. ) ;
#65935 = DIRECTION ( 'NONE',  ( 0.000000000000000000, 0.000000000000000000, 1.000000000000000000 ) ) ;
#65937 = EDGE_CURVE ( 'NONE', #35320, #66014, #11662, .T. ) ;
#65938 = CARTESIAN_POINT ( 'NONE',  ( 0.000000000000000000, -0.03417435944610275333, 14.25000000000000000 ) ) ;
#65939 = CARTESIAN_POINT ( 'NONE',  ( 12.63842701281683922, 54.55059781766745175, -9.846743663894590881 ) ) ;
#65940 = EDGE_LOOP ( 'NONE', ( #55763, #19816, #80620, #13425 ) ) ;
#65941 = VECTOR ( 'NONE', #50312, 1000.000000000000000 ) ;
#65942 = CARTESIAN_POINT ( 'NONE',  ( 5.076628168052703671, 26.84226448433411960, 8.527530157486179263 ) ) ;
#65943 = CARTESIAN_POINT ( 'NONE',  ( 6.408140936763236262, -27.54303199673624292, -11.09922568453595026 ) ) ;
#65944 = CARTESIAN_POINT ( 'NONE',  ( -0.8801773607110991993, 17.85535201082150536, -2.915334737309923874 ) ) ;
#65945 = CARTESIAN_POINT ( 'NONE',  ( 10.00000000000000000, 19.75893115100078390, -9.846743663894594434 ) ) ;
#65946 = CARTESIAN_POINT ( 'NONE',  ( 19.38216949554541202, 5.998634669930420493, 9.382169495545424454 ) ) ;
#65947 = CARTESIAN_POINT ( 'NONE',  ( -0.8801773607111008646, 53.27201867748816966, 2.915334737309923430 ) ) ;
#65949 = CARTESIAN_POINT ( 'NONE',  ( 21.09922568453594849, 56.20696800326375353, 6.408140936763242479 ) ) ;
#65948 = CARTESIAN_POINT ( 'NONE',  ( 12.91533473730992121, 19.52201867748816611, 10.88017736071110164 ) ) ;
#65950 = CARTESIAN_POINT ( 'NONE',  ( -4.164238869374098151, 41.59541550158061796, -3.795296366450310543 ) ) ;
#65951 = VECTOR ( 'NONE', #39956, 999.9999999999998863 ) ;
#65952 = AXIS2_PLACEMENT_3D ( 'NONE', #14332, #91800, #31773 ) ;
#65953 = CARTESIAN_POINT ( 'NONE',  ( 21.92686044187656691, 34.95379003517447813, 3.195792623639537755 ) ) ;
#65954 = ORIENTED_EDGE ( 'NONE', *, *, #93876, .T. ) ;
#65955 = CARTESIAN_POINT ( 'NONE',  ( 10.00000000000000178, 0.3736346699304200492, 12.81628187352647608 ) ) ;
#65956 = SURFACE_STYLE_USAGE ( .BOTH. , #35459 ) ;
#65957 = CARTESIAN_POINT ( 'NONE',  ( 20.88017736071110875, 35.77201867748816966, -2.915334737309920765 ) ) ;
#65958 = CARTESIAN_POINT ( 'NONE',  ( 14.92337183194729633, 57.67559781766745886, 8.527530157486181039 ) ) ;
#65960 = EDGE_LOOP ( 'NONE', ( #73511, #58290, #323, #7385 ) ) ;
#65959 = EDGE_CURVE ( 'NONE', #48237, #935, #67572, .T. ) ;
#65961 = CARTESIAN_POINT ( 'NONE',  ( 10.00000000000000178, 17.25893115100078745, 9.846743663894594434 ) ) ;
#65962 = CARTESIAN_POINT ( 'NONE',  ( 3.195792623639469809, 8.229976035794180689, -11.92686044187660066 ) ) ;
#65963 = CARTESIAN_POINT ( 'NONE',  ( 7.361572987183169658, 24.96726448433412315, -9.846743663894592657 ) ) ;
#65964 = CARTESIAN_POINT ( 'NONE',  ( 0.1532563361054100626, 5.800597817667452638, -2.638427012816831230 ) ) ;
#65965 = SURFACE_STYLE_USAGE ( .BOTH. , #49483 ) ;
#65966 = CARTESIAN_POINT ( 'NONE',  ( 32.06412365047463453, 26.99999999999998224, -9.500000000000000000 ) ) ;
#65968 = PLANE ( 'NONE',  #8423 ) ;
#65967 = CARTESIAN_POINT ( 'NONE',  ( 0.1532563361054082862, 6.217264484334118713, 2.638427012816831674 ) ) ;
#65969 = CARTESIAN_POINT ( 'NONE',  ( 12.63842701281683034, 2.467264484334118269, 9.846743663894596210 ) ) ;
#65971 = ORIENTED_EDGE ( 'NONE', *, *, #45437, .F. ) ;
#65970 = CARTESIAN_POINT ( 'NONE',  ( 0.1532563361054083140, 21.00893115100078745, 1.131784320476157264E-15 ) ) ;
#65972 = B_SPLINE_CURVE_WITH_KNOTS ( 'NONE', 3,
 ( #52602, #14126, #44610, #14634 ),
 .UNSPECIFIED., .F., .F.,
 ( 4, 4 ),
 ( 6.213755518593340002E-17, 0.001060528352562004582 ),
 .UNSPECIFIED. ) ;
#65973 = CARTESIAN_POINT ( 'NONE',  ( -33.42076923076923833, 91.65384615384616041, -9.500000000000000000 ) ) ;
#65974 = CARTESIAN_POINT ( 'NONE',  ( -2.816281873526471635, -1.084698663402913210, -3.434112377981056508 ) ) ;
#65975 = ORIENTED_EDGE ( 'NONE', *, *, #50608, .F. ) ;
#65976 = CARTESIAN_POINT ( 'NONE',  ( 7.084665262690076126, 7.022018677488169658, -10.88017736071110164 ) ) ;
#65977 = CARTESIAN_POINT ( 'NONE',  ( -0.3689425029237898834, 16.17874883491396076, -10.36894250292378850 ) ) ;
#65978 = VECTOR ( 'NONE', #25531, 1000.000000000000000 ) ;
#65979 = DIRECTION ( 'NONE',  ( 0.4305110968082926370, -0.000000000000000000, 0.9025852843498617384 ) ) ;
#65980 = MECHANICAL_DESIGN_GEOMETRIC_PRESENTATION_REPRESENTATION (  '', ( #64335 ), #22910 ) ;
#65981 = CARTESIAN_POINT ( 'NONE',  ( -4.164238869374099927, 22.01208216824730357, 3.795296366450308767 ) ) ;
#65982 = CARTESIAN_POINT ( 'NONE',  ( 20.36894250292379738, 44.92874883491396787, -10.36894250292379027 ) ) ;
#65983 = DIRECTION ( 'NONE',  ( 0.000000000000000000, 0.000000000000000000, -1.000000000000000000 ) ) ;
#65984 = CARTESIAN_POINT ( 'NONE',  ( 24.16423886937410614, 19.30374883491397142, 8.672049930838204340E-16 ) ) ;
#65985 = CARTESIAN_POINT ( 'NONE',  ( 19.42250999205614548, 30.98035201082150536, -5.440088680355545492 ) ) ;
#65986 = CARTESIAN_POINT ( 'NONE',  ( 13.40508947812165097, 15.00000000000000000, -5.527528931046084004 ) ) ;
#65987 = ORIENTED_EDGE ( 'NONE', *, *, #13337, .F. ) ;
#65988 = CARTESIAN_POINT ( 'NONE',  ( 1.472469842513823179, 10.59226448433411782, -4.923371831947296329 ) ) ;
#65990 = CARTESIAN_POINT ( 'NONE',  ( 19.84674366389459621, 28.50893115100078745, 7.409399052514197653E-17 ) ) ;
#65989 = CARTESIAN_POINT ( 'NONE',  ( 15.44008868035555260, 59.73035201082151247, 9.422509992056143702 ) ) ;
#65991 = CARTESIAN_POINT ( 'NONE',  ( 15.44008868035555260, 4.730352010821505360, 9.422509992056143702 ) ) ;
#65992 = CARTESIAN_POINT ( 'NONE',  ( 21.09922568453594849, 41.20696800326375353, 6.408140936763242479 ) ) ;
#65993 = CARTESIAN_POINT ( 'NONE',  ( 2.791683348922237240, 55.38393115100078745, -7.208316651077763204 ) ) ;
#65994 = PRESENTATION_STYLE_ASSIGNMENT (( #12506 ) ) ;
#65995 = CARTESIAN_POINT ( 'NONE',  ( 21.09922568453594849, 36.20696800326375353, 6.408140936763242479 ) ) ;
#65996 = CARTESIAN_POINT ( 'NONE',  ( 7.082119434687054849, -31.52958449841936073, 12.26659068614894288 ) ) ;
#65997 = CARTESIAN_POINT ( 'NONE',  ( 18.52753015748617571, 33.09226448433411605, 4.923371831947298993 ) ) ;
#65998 = CARTESIAN_POINT ( 'NONE',  ( -0.3689425029237881626, 32.42874883491395366, 10.36894250292379027 ) ) ;
#65999 = ORIENTED_EDGE ( 'NONE', *, *, #90170, .T. ) ;
#66000 = SURFACE_STYLE_USAGE ( .BOTH. , #1713 ) ;
#66001 = CARTESIAN_POINT ( 'NONE',  ( 15.44008868035555260, 54.73035201082150536, 9.422509992056143702 ) ) ;
#66002 = CARTESIAN_POINT ( 'NONE',  ( 20.88017736071110519, 60.56368534415484106, 2.639326808657452039E-16 ) ) ;
#66003 = CARTESIAN_POINT ( 'NONE',  ( 24.16423886937409904, 49.09541550158063217, 3.795296366450317205 ) ) ;
#66004 = CARTESIAN_POINT ( 'NONE',  ( 2.791683348922237240, 65.38393115100078035, -7.208316651077763204 ) ) ;
#66005 = CARTESIAN_POINT ( 'NONE',  ( 16.40814093676323893, 60.79030133659709634, 11.09922568453595026 ) ) ;
#66006 = CARTESIAN_POINT ( 'NONE',  ( 17.96484262340118221, 36.18868534415484106, -7.964842623401177768 ) ) ;
#66007 = DIRECTION ( 'NONE',  ( -0.000000000000000000, -1.000000000000000000, -0.000000000000000000 ) ) ;
#66008 = CARTESIAN_POINT ( 'NONE',  ( 3.591859063236763294, 28.29030133659708568, -11.09922568453595026 ) ) ;
#66009 = CARTESIAN_POINT ( 'NONE',  ( 0.1532563361054082862, 51.21726448433412315, 2.638427012816831674 ) ) ;
#66010 = CARTESIAN_POINT ( 'NONE',  ( -10.88017736071109987, 18.27201867748817321, 2.915334737309934532 ) ) ;
#66011 = SURFACE_STYLE_USAGE ( .BOTH. , #23620 ) ;
#66012 = CARTESIAN_POINT ( 'NONE',  ( 10.00000000000000178, 14.31368534415483929, 10.88017736071110342 ) ) ;
#66013 = CARTESIAN_POINT ( 'NONE',  ( -13.11254139118232231, 91.00000000000000000, -8.000000000000000000 ) ) ;
#66014 = VERTEX_POINT ( 'NONE', #54833 ) ;
#66015 = ADVANCED_FACE ( 'NONE', ( #77342 ), #38876, .T. ) ;
#66016 = ADVANCED_FACE ( 'NONE', ( #4315 ), #62759, .T. ) ;
#66017 = CARTESIAN_POINT ( 'NONE',  ( 0.5774900079438607392, 3.480352010821504027, 5.440088680355550821 ) ) ;
#66018 = DIRECTION ( 'NONE',  ( 0.000000000000000000, 0.000000000000000000, 1.000000000000000000 ) ) ;
#66019 = CARTESIAN_POINT ( 'NONE',  ( 2.791683348922237240, 0.3839311510007847872, -7.208316651077763204 ) ) ;
#66020 = CARTESIAN_POINT ( 'NONE',  ( 4.559911319644449179, 68.89701867748817676, 9.422509992056141925 ) ) ;
#66021 = CARTESIAN_POINT ( 'NONE',  ( 18.00000000000000000, 77.07179676972447169, -4.250000000000000000 ) ) ;
#66022 = CARTESIAN_POINT ( 'NONE',  ( 12.63842701281683922, 29.55059781766745175, -9.846743663894590881 ) ) ;
#66023 = CARTESIAN_POINT ( 'NONE',  ( -0.8801773607111009756, 18.06368534415484106, 1.068504757029289695E-15 ) ) ;
#66024 = CARTESIAN_POINT ( 'NONE',  ( 10.00000000000000000, 12.87363466993042138, -12.81628187352647608 ) ) ;
#66026 = CARTESIAN_POINT ( 'NONE',  ( 10.32896413005680181, 10.57879003517447813, -5.963430220938285231 ) ) ;
#66025 = CARTESIAN_POINT ( 'NONE',  ( 15.44008868035555793, 41.39701867748817676, -9.422509992056140149 ) ) ;
#66027 = CARTESIAN_POINT ( 'NONE',  ( 10.00000000000000000, 37.87363466993041783, -12.81628187352647608 ) ) ;
#66028 = VERTEX_POINT ( 'NONE', #57785 ) ;
#66029 = CARTESIAN_POINT ( 'NONE',  ( 20.88017736071110519, 65.56368534415483396, 2.639326808657452039E-16 ) ) ;
#66031 = LINE ( 'NONE', #96560, #23876 ) ;
#66030 = CARTESIAN_POINT ( 'NONE',  ( -1.099225684535947600, 14.54030133659708568, 6.408140936763237150 ) ) ;
#66032 = CARTESIAN_POINT ( 'NONE',  ( 12.91533473730993009, 46.60535201082150536, -10.88017736071109987 ) ) ;
#66033 = CARTESIAN_POINT ( 'NONE',  ( 2.791683348922240793, 61.63393115100079456, 7.208316651077764092 ) ) ;
#66034 = CARTESIAN_POINT ( 'NONE',  ( 6.204703633549690345, 65.76208216824731778, -14.16423886937410259 ) ) ;
#66035 = CARTESIAN_POINT ( 'NONE',  ( 18.52753015748618282, 53.92559781766745175, -4.923371831947291888 ) ) ;
#66036 = CARTESIAN_POINT ( 'NONE',  ( 19.84674366389459266, 3.717264484334118713, -2.638427012816827677 ) ) ;
#66037 = CARTESIAN_POINT ( 'NONE',  ( 0.5774900079438590739, 67.64701867748817676, -5.440088680355550821 ) ) ;
#66038 = CARTESIAN_POINT ( 'NONE',  ( 0.2751277870542967463, 0.000000000000000000, 6.500000000000000888 ) ) ;
#66039 = CARTESIAN_POINT ( 'NONE',  ( 20.36894250292379382, 23.67874883491397142, 10.36894250292379205 ) ) ;
#66040 = LINE ( 'NONE', #58541, #3418 ) ;
#66041 = CARTESIAN_POINT ( 'NONE',  ( -3.628626192036342069, -3.642031182891574126, -4.000000000000000000 ) ) ;
#66042 = ORIENTED_EDGE ( 'NONE', *, *, #89650, .F. ) ;
#66043 = ORIENTED_EDGE ( 'NONE', *, *, #69638, .F. ) ;
#66044 = CARTESIAN_POINT ( 'NONE',  ( -0.3689425029237881626, 62.42874883491396787, 10.36894250292379027 ) ) ;
#66046 = EDGE_CURVE ( 'NONE', #87620, #51199, #5304, .T. ) ;
#66045 = CARTESIAN_POINT ( 'NONE',  ( 10.00000000000000000, 45.55374883491397497, -14.16423886937410082 ) ) ;
#66047 = CARTESIAN_POINT ( 'NONE',  ( 2.791683348922237240, 30.38393115100078390, -7.208316651077763204 ) ) ;
#66048 = CARTESIAN_POINT ( 'NONE',  ( 3.591859063236761518, 24.95696800326375353, 11.09922568453594849 ) ) ;
#66049 = CARTESIAN_POINT ( 'NONE',  ( -9.000000000000003553, 80.99999999999994316, 1.249999999999987121 ) ) ;
#66051 = CARTESIAN_POINT ( 'NONE',  ( -4.249999999999999112, 78.07179676972445748, 6.500000000000000888 ) ) ;
#66050 = AXIS2_PLACEMENT_3D ( 'NONE', #25729, #58156, #50172 ) ;
#66052 = CARTESIAN_POINT ( 'NONE',  ( 6.204703633549690345, 62.84541550158063927, 14.16423886937410082 ) ) ;
#66053 = ADVANCED_FACE ( 'NONE', ( #19305 ), #75555, .T. ) ;
#66054 = CARTESIAN_POINT ( 'NONE',  ( 3.969999999999999751, 10.25000000000000000, -2.500000000000000000 ) ) ;
#66055 = CARTESIAN_POINT ( 'NONE',  ( 5.076628168052704559, 15.17559781766745175, -8.527530157486179263 ) ) ;
#66056 = AXIS2_PLACEMENT_3D ( 'NONE', #78956, #40975, #8500 ) ;
#66057 = CARTESIAN_POINT ( 'NONE',  ( 17.39651004071841811, 2.935752660568277328, 6.500000000000002665 ) ) ;
#66058 = CARTESIAN_POINT ( 'NONE',  ( 9.846743663894594434, -1.491068848999209440, -2.168404344971008868E-15 ) ) ;
#66059 = ORIENTED_EDGE ( 'NONE', *, *, #23066, .F. ) ;
#66060 = ORIENTED_EDGE ( 'NONE', *, *, #31602, .T. ) ;
#66061 = SURFACE_STYLE_USAGE ( .BOTH. , #11590 ) ;
#66062 = ORIENTED_EDGE ( 'NONE', *, *, #57607, .T. ) ;
#66064 = CARTESIAN_POINT ( 'NONE',  ( 4.559911319644449179, 28.89701867748817321, 9.422509992056141925 ) ) ;
#66063 = CARTESIAN_POINT ( 'NONE',  ( 19.42250999205614548, 15.98035201082150714, -5.440088680355545492 ) ) ;
#66066 = CARTESIAN_POINT ( 'NONE',  ( 13.43411237798105340, 20.58196800326374643, 12.81628187352647963 ) ) ;
#66065 = CARTESIAN_POINT ( 'NONE',  ( 7.361572987183169658, 54.96726448433413026, -9.846743663894592657 ) ) ;
#66067 = DIRECTION ( 'NONE',  ( 1.000000000000000000, 0.000000000000000000, 0.000000000000000000 ) ) ;
#66068 = B_SPLINE_CURVE_WITH_KNOTS ( 'NONE', 3,
 ( #82968, #23474, #22979, #76937 ),
 .UNSPECIFIED., .F., .F.,
 ( 4, 4 ),
 ( 3.417008968066607180E-17, 0.001060528352561980947 ),
 .UNSPECIFIED. ) ;
#66069 = CARTESIAN_POINT ( 'NONE',  ( 3.591859063236761518, 34.95696800326375353, 11.09922568453594849 ) ) ;
#66071 = ORIENTED_EDGE ( 'NONE', *, *, #15810, .F. ) ;
#66070 = CARTESIAN_POINT ( 'NONE',  ( 1.472469842513823179, 0.5922644843341181575, -4.923371831947296329 ) ) ;
#66072 = CARTESIAN_POINT ( 'NONE',  ( 0.1532563361054082862, 26.21726448433411605, 2.638427012816831674 ) ) ;
#66073 = CARTESIAN_POINT ( 'NONE',  ( 20.36894250292379738, 59.92874883491397497, -10.36894250292379027 ) ) ;
#66074 = ORIENTED_EDGE ( 'NONE', *, *, #93713, .T. ) ;
#66075 = CARTESIAN_POINT ( 'NONE',  ( 10.00000000000000178, 9.313685344154839285, 10.88017736071110342 ) ) ;
#66076 = ORIENTED_EDGE ( 'NONE', *, *, #23089, .T. ) ;
#66077 = CARTESIAN_POINT ( 'NONE',  ( 0.5774900079438607392, 48.48035201082150536, 5.440088680355550821 ) ) ;
#66078 = CARTESIAN_POINT ( 'NONE',  ( 20.88017736071110519, 45.56368534415484106, 2.639326808657452039E-16 ) ) ;
#66079 = CARTESIAN_POINT ( 'NONE',  ( 19.42250999205614548, 45.98035201082150536, -5.440088680355545492 ) ) ;
#66080 = FACE_OUTER_BOUND ( 'NONE', #55725, .T. ) ;
#66081 = CARTESIAN_POINT ( 'NONE',  ( 2.035157376598824452, 38.68868534415483396, 7.964842623401179544 ) ) ;
#66082 = CARTESIAN_POINT ( 'NONE',  ( 4.219999999999999751, 36.75000000000000000, 3.750000000000000000 ) ) ;
#66083 = EDGE_CURVE ( 'NONE', #1208, #36938, #57297, .T. ) ;
#66084 = ORIENTED_EDGE ( 'NONE', *, *, #25425, .T. ) ;
#66085 = CARTESIAN_POINT ( 'NONE',  ( 14.92337183194729633, 32.67559781766745175, 8.527530157486181039 ) ) ;
#66086 = ORIENTED_EDGE ( 'NONE', *, *, #65835, .T. ) ;
#66087 = CARTESIAN_POINT ( 'NONE',  ( 14.92337183194729988, 64.34226448433412315, -8.527530157486177487 ) ) ;
#66088 = CYLINDRICAL_SURFACE ( 'NONE', #80409, 11.92686044187656513 ) ;
#66089 = SURFACE_STYLE_USAGE ( .BOTH. , #43102 ) ;
#66090 = ORIENTED_EDGE ( 'NONE', *, *, #65634, .F. ) ;
#66091 = FILL_AREA_STYLE_COLOUR ( '', #89179 ) ;
#66092 = LINE ( 'NONE', #20108, #93742 ) ;
#66094 = CARTESIAN_POINT ( 'NONE',  ( 12.63842701281683922, 39.55059781766744464, -9.846743663894590881 ) ) ;
#66093 = CARTESIAN_POINT ( 'NONE',  ( 0.000000000000000000, 0.000000000000000000, 0.000000000000000000 ) ) ;
#66095 = CARTESIAN_POINT ( 'NONE',  ( 6.204703633549690345, 57.84541550158063927, 14.16423886937410082 ) ) ;
#66096 = DIRECTION ( 'NONE',  ( 0.9799247046208268141, 0.000000000000000000, 0.1993679344172108459 ) ) ;
#66097 = ORIENTED_EDGE ( 'NONE', *, *, #82546, .T. ) ;
#66098 = DIRECTION ( 'NONE',  ( 0.9969173337331289630, 0.000000000000000000, -0.07845909572783234254 ) ) ;
#66099 = CARTESIAN_POINT ( 'NONE',  ( 17.20831665107776587, 27.88393115100078390, 7.208316651077764980 ) ) ;
#66100 = CARTESIAN_POINT ( 'NONE',  ( 0.000000000000000000, 14.49999999999999822, 0.000000000000000000 ) ) ;
#66101 = CARTESIAN_POINT ( 'NONE',  ( 19.38216949554541202, 5.998634669930420493, 9.382169495545424454 ) ) ;
#66102 = CARTESIAN_POINT ( 'NONE',  ( 18.52753015748618282, 8.925597817667451750, -4.923371831947291888 ) ) ;
#66103 = DIRECTION ( 'NONE',  ( 0.8070303256584298035, -0.5905099943842175847, 0.000000000000000000 ) ) ;
#66104 = CARTESIAN_POINT ( 'NONE',  ( 2.791683348922240793, 11.63393115100078568, 7.208316651077764092 ) ) ;
#66105 = CARTESIAN_POINT ( 'NONE',  ( 3.591859063236763294, 3.290301336597087012, -11.09922568453595026 ) ) ;
#66106 = CARTESIAN_POINT ( 'NONE',  ( 14.40939250469964961, 15.00000000000000000, 1.618458416365853747 ) ) ;
#66107 = B_SPLINE_CURVE_WITH_KNOTS ( 'NONE', 3,
 ( #34931, #19451, #4463, #41972, #95453, #5450 ),
 .UNSPECIFIED., .F., .F.,
 ( 4, 2, 4 ),
 ( 3.409110551496096132E-05, 0.0004400426677367858127, 0.0008459942299586107250 ),
 .UNSPECIFIED. ) ;
#66108 = VECTOR ( 'NONE', #10406, 1000.000000000000227 ) ;
#66109 = EDGE_LOOP ( 'NONE', ( #24658, #15911, #15421, #28081, #16912, #87698 ) ) ;
#66110 = CARTESIAN_POINT ( 'NONE',  ( 4.559911319644449179, 7.230352010821505360, -9.422509992056141925 ) ) ;
#66111 = CARTESIAN_POINT ( 'NONE',  ( 24.16423886937410614, 9.512082168247301794, -3.795296366450302550 ) ) ;
#66112 = CARTESIAN_POINT ( 'NONE',  ( 19.84674366389459266, 28.71726448433411960, -2.638427012816827677 ) ) ;
#66113 = CARTESIAN_POINT ( 'NONE',  ( 19.42250999205614193, 50.14701867748817676, 5.440088680355555262 ) ) ;
#66115 = FACE_BOUND ( 'NONE', #80822, .T. ) ;
#66114 = CARTESIAN_POINT ( 'NONE',  ( 0.6178305044545818747, 28.49863466993041783, -9.382169495545419124 ) ) ;
#66116 = CARTESIAN_POINT ( 'NONE',  ( -12.60589901313227124, 0.5000000000000004441, 8.129656208641961257 ) ) ;
#66117 = FACE_OUTER_BOUND ( 'NONE', #50924, .T. ) ;
#66118 = CARTESIAN_POINT ( 'NONE',  ( 0.000000000000000000, 81.99999999999992895, -5.000000000000000000 ) ) ;
#66119 = CARTESIAN_POINT ( 'NONE',  ( 22.81628187352647785, 1.415301336597087012, 3.434112377981063169 ) ) ;
#66120 = CARTESIAN_POINT ( 'NONE',  ( 5.076628168052703671, 66.84226448433412315, 8.527530157486179263 ) ) ;
#66121 = CARTESIAN_POINT ( 'NONE',  ( 18.52753015748617571, 13.09226448433411960, 4.923371831947298993 ) ) ;
#66122 = CARTESIAN_POINT ( 'NONE',  ( -5.440088680355547268, -21.10298132251182324, 9.422509992056143702 ) ) ;
#66123 = CARTESIAN_POINT ( 'NONE',  ( 6.565887622018943937, 23.08196800326375708, -12.81628187352647608 ) ) ;
#66124 = CARTESIAN_POINT ( 'NONE',  ( -11.51381718487224681, -65.37259455511993167, -3.750000000000000000 ) ) ;
#66125 = CARTESIAN_POINT ( 'NONE',  ( 20.88017736071110519, 25.56368534415483751, 2.639326808657452039E-16 ) ) ;
#66126 = CARTESIAN_POINT ( 'NONE',  ( -14.99847009497944406, 15.00000000000000000, -0.2142307401082361173 ) ) ;
#66127 = CARTESIAN_POINT ( 'NONE',  ( 24.16423886937409904, 54.09541550158063217, 3.795296366450317205 ) ) ;
#66128 = EDGE_CURVE ( 'NONE', #58242, #64886, #64428, .T. ) ;
#66129 = DIRECTION ( 'NONE',  ( 0.000000000000000000, 0.000000000000000000, 1.000000000000000000 ) ) ;
#66130 = CARTESIAN_POINT ( 'NONE',  ( 12.91533473730992121, 29.52201867748817321, 10.88017736071110164 ) ) ;
#66131 = CARTESIAN_POINT ( 'NONE',  ( 10.00000000000000178, 47.25893115100078745, 9.846743663894594434 ) ) ;
#66132 = CARTESIAN_POINT ( 'NONE',  ( -0.8801773607111008646, 48.27201867748816966, 2.915334737309923430 ) ) ;
#66133 = CARTESIAN_POINT ( 'NONE',  ( 2.917880565312950480, 30.97041550158063572, -12.26659068614894821 ) ) ;
#66134 = LINE ( 'NONE', #43637, #56740 ) ;
#66135 = CARTESIAN_POINT ( 'NONE',  ( 10.00000000000000178, 42.25893115100078745, 9.846743663894594434 ) ) ;
#66136 = SURFACE_SIDE_STYLE ('',( #12160 ) ) ;
#66137 = CARTESIAN_POINT ( 'NONE',  ( 10.00000000000000178, 67.25893115100079456, 9.846743663894594434 ) ) ;
#66138 = ORIENTED_EDGE ( 'NONE', *, *, #8485, .T. ) ;
#66139 = CARTESIAN_POINT ( 'NONE',  ( 4.559911319644449179, 18.89701867748817321, 9.422509992056141925 ) ) ;
#66140 = CARTESIAN_POINT ( 'NONE',  ( 17.97713247904330558, 91.14635076194878138, -8.000000000000000000 ) ) ;
#66141 = CARTESIAN_POINT ( 'NONE',  ( 15.44008868035555793, 16.39701867748817321, -9.422509992056140149 ) ) ;
#66142 = CARTESIAN_POINT ( 'NONE',  ( 18.52753015748617571, 3.092264484334118269, 4.923371831947298993 ) ) ;
#66143 = CARTESIAN_POINT ( 'NONE',  ( 10.00000000000000000, 25.55374883491396787, -14.16423886937410082 ) ) ;
#66144 = CARTESIAN_POINT ( 'NONE',  ( 12.63842701281683922, 19.55059781766745175, -9.846743663894590881 ) ) ;
#66145 = CARTESIAN_POINT ( 'NONE',  ( 12.63842701281683922, 59.55059781766744464, -9.846743663894590881 ) ) ;
#66146 = CARTESIAN_POINT ( 'NONE',  ( 2.035157376598824452, 33.68868534415484106, 7.964842623401179544 ) ) ;
#66147 = CARTESIAN_POINT ( 'NONE',  ( -3.420591144908647241, 0.5000000000000004441, 14.60477854057953451 ) ) ;
#66148 = DIRECTION ( 'NONE',  ( 1.000000000000000000, 0.000000000000000000, 0.000000000000000000 ) ) ;
#66149 = STYLED_ITEM ( 'NONE', ( #53263 ), #51621 ) ;
#66150 = ORIENTED_EDGE ( 'NONE', *, *, #72450, .T. ) ;
#66151 = DIRECTION ( 'NONE',  ( -0.000000000000000000, 1.000000000000000000, -0.000000000000000000 ) ) ;
#66152 = CARTESIAN_POINT ( 'NONE',  ( 10.00000000000000000, 49.75893115100078745, -9.846743663894594434 ) ) ;
#66153 = EDGE_LOOP ( 'NONE', ( #2884, #43903, #55551, #93515, #3466, #32110, #12809, #63240 ) ) ;
#66154 = EDGE_LOOP ( 'NONE', ( #45038, #24554, #6346, #94034 ) ) ;
#66155 = CARTESIAN_POINT ( 'NONE',  ( 0.000000000000000000, 0.5000000000000004441, 0.000000000000000000 ) ) ;
#66156 = CARTESIAN_POINT ( 'NONE',  ( 17.08211943468705840, 25.13708216824730357, -12.26659068614894466 ) ) ;
#66158 = EDGE_CURVE ( 'NONE', #32127, #29785, #25836, .T. ) ;
#66157 = CARTESIAN_POINT ( 'NONE',  ( 17.08211943468705130, 13.47041550158063572, 12.26659068614894998 ) ) ;
#66159 = CARTESIAN_POINT ( 'NONE',  ( 10.00000000000000000, 61.81368534415484106, -10.88017736071110342 ) ) ;
#66160 = CARTESIAN_POINT ( 'NONE',  ( 22.26659068614894466, 53.88708216824731068, 7.082119434687054849 ) ) ;
#66161 = CARTESIAN_POINT ( 'NONE',  ( 6.565887622018943937, 0.1653013365970866511, 12.81628187352647430 ) ) ;
#66162 = CARTESIAN_POINT ( 'NONE',  ( 1.472469842513823179, 35.59226448433412315, -4.923371831947296329 ) ) ;
#66163 = CARTESIAN_POINT ( 'NONE',  ( -16.80847703285585482, 99.89644660940670917, 8.000000000000001776 ) ) ;
#66165 = CARTESIAN_POINT ( 'NONE',  ( 10.00000000000000178, 0.3736346699304200492, 12.81628187352647608 ) ) ;
#66164 = CARTESIAN_POINT ( 'NONE',  ( -0.8801773607111009756, 38.06368534415484106, 1.068504757029289695E-15 ) ) ;
#66166 = CARTESIAN_POINT ( 'NONE',  ( 6.204703633549690345, 17.84541550158063217, 14.16423886937410082 ) ) ;
#66167 = CARTESIAN_POINT ( 'NONE',  ( 13.79529636645030344, 53.26208216824730357, 14.16423886937410614 ) ) ;
#66168 = CARTESIAN_POINT ( 'NONE',  ( 15.44008868035555793, 21.39701867748817321, -9.422509992056140149 ) ) ;
#66169 = CARTESIAN_POINT ( 'NONE',  ( 19.84674366389459266, 38.71726448433412315, -2.638427012816827677 ) ) ;
#66170 = CARTESIAN_POINT ( 'NONE',  ( 31.00000000000000355, 44.99999999999999289, -7.000000000000000000 ) ) ;
#66171 = CARTESIAN_POINT ( 'NONE',  ( 4.559911319644449179, 38.89701867748817676, 9.422509992056141925 ) ) ;
#66172 = B_SPLINE_CURVE_WITH_KNOTS ( 'NONE', 3,
 ( #54180, #84693, #94150, #54667, #2201, #85184 ),
 .UNSPECIFIED., .F., .F.,
 ( 4, 2, 4 ),
 ( 0.0002800591277523066546, 0.0006862649357714347472, 0.001092470743790562894 ),
 .UNSPECIFIED. ) ;
#66173 = CARTESIAN_POINT ( 'NONE',  ( -9.846743663894594434, -38.99106884899920544, 3.469446951953614189E-15 ) ) ;
#66174 = EDGE_LOOP ( 'NONE', ( #8286, #65255, #73272, #78134 ) ) ;
#66175 = ORIENTED_EDGE ( 'NONE', *, *, #88613, .T. ) ;
#66176 = ORIENTED_EDGE ( 'NONE', *, *, #73827, .F. ) ;
#66177 = CARTESIAN_POINT ( 'NONE',  ( 22.26659068614895176, 49.72041550158063927, -7.082119434687042414 ) ) ;
#66178 = CARTESIAN_POINT ( 'NONE',  ( 17.20831665107776587, 42.88393115100077324, 7.208316651077764980 ) ) ;
#66179 = CARTESIAN_POINT ( 'NONE',  ( 20.88017736071110519, 55.56368534415484817, 2.639326808657452039E-16 ) ) ;
#66180 = FACE_OUTER_BOUND ( 'NONE', #62268, .T. ) ;
#66181 = CARTESIAN_POINT ( 'NONE',  ( 12.91533473730992121, 49.52201867748817676, 10.88017736071110164 ) ) ;
#66182 = COLOUR_RGB ( '', 0.31764706, 0.68627451, 0.89019608) ;
#66183 = VECTOR ( 'NONE', #86919, 1000.000000000000000 ) ;
#66184 = CARTESIAN_POINT ( 'NONE',  ( -3.434112377981047626, 10.16530133659709101, 12.81628187352647963 ) ) ;
#66185 = ORIENTED_EDGE ( 'NONE', *, *, #67690, .T. ) ;
#66186 = CARTESIAN_POINT ( 'NONE',  ( 24.16423886937410614, 19.30374883491397142, 8.672049930838204340E-16 ) ) ;
#66187 = STYLED_ITEM ( 'NONE', ( #31570 ), #95230 ) ;
#66188 = CARTESIAN_POINT ( 'NONE',  ( -2.816281873526471635, 18.91530133659708213, -3.434112377981056508 ) ) ;
#66189 = ORIENTED_EDGE ( 'NONE', *, *, #27143, .F. ) ;
#66190 = CARTESIAN_POINT ( 'NONE',  ( 0.6178305044545838731, 39.74863466993041072, 9.382169495545420901 ) ) ;
#66191 = EDGE_CURVE ( 'NONE', #84403, #67137, #18332, .T. ) ;
#66192 = CARTESIAN_POINT ( 'NONE',  ( 5.076628168052704559, 30.17559781766745175, -8.527530157486179263 ) ) ;
#66193 = CARTESIAN_POINT ( 'NONE',  ( 20.88017736071110519, 10.56368534415483751, 2.639326808657452039E-16 ) ) ;
#66194 = CIRCLE ( 'NONE', #59844, 2.999999999999999112 ) ;
#66195 =( BOUNDED_CURVE ( )  B_SPLINE_CURVE ( 2, ( #18579, #11559, #12546, #4571, #20043, #35032, #95558, #65534, #71591 ),
 .UNSPECIFIED., .F., .T. ) 
 B_SPLINE_CURVE_WITH_KNOTS ( ( 3, 2, 2, 2, 3 ),
 ( 0.2596570216176965484, 0.2619047619047619180, 0.2678571428571428492, 0.2738095238095238360, 0.2760572640965892055 ),
 .UNSPECIFIED. ) 
 CURVE ( )  GEOMETRIC_REPRESENTATION_ITEM ( )  RATIONAL_B_SPLINE_CURVE ( ( 0.9839835555609426354, 0.9871328979762479250, 1.000000000000000000, 0.9659258262890683122, 1.000000000000000000, 0.9659258262890683122, 1.000000000000000000, 0.9871328979762477029, 0.9839835555609424134 ) ) 
 REPRESENTATION_ITEM ( '' )  );
#66196 = CARTESIAN_POINT ( 'NONE',  ( -2.816281873526473856, 54.33196800326376064, 3.434112377981055619 ) ) ;
#66197 = FACE_OUTER_BOUND ( 'NONE', #12665, .T. ) ;
#66198 = CARTESIAN_POINT ( 'NONE',  ( 10.00000000000000000, 49.75893115100078745, -9.846743663894594434 ) ) ;
#66199 = EDGE_CURVE ( 'NONE', #89050, #7752, #95908, .T. ) ;
#66200 =( BOUNDED_CURVE ( )  B_SPLINE_CURVE ( 2, ( #32069, #86575, #55588, #49060, #70097, #94067, #9586, #1620, #86084, #40586, #2115, #10087, #56081 ),
 .UNSPECIFIED., .F., .F. ) 
 B_SPLINE_CURVE_WITH_KNOTS ( ( 3, 2, 2, 2, 2, 2, 3 ),
 ( 0.6999999999999999556, 0.7055555555555556024, 0.7111111111111111382, 0.7166666666666666741, 0.7222222222222222099, 0.7277777777777777457, 0.7298586539780400617 ),
 .UNSPECIFIED. ) 
 CURVE ( )  GEOMETRIC_REPRESENTATION_ITEM ( )  RATIONAL_B_SPLINE_CURVE ( ( 1.000000000000000000, 0.9659258262890683122, 1.000000000000000000, 0.9659258262890683122, 1.000000000000000000, 0.9659258262890683122, 1.000000000000000000, 0.9659258262890683122, 1.000000000000000000, 0.9659258262890683122, 1.000000000000000000, 0.9872372553186372635, 0.9840352796339646435 ) ) 
 REPRESENTATION_ITEM ( '' )  );
#66201 = CARTESIAN_POINT ( 'NONE',  ( 4.999999999999999112, 60.50000000000000711, 6.500000000000000888 ) ) ;
#66202 = PRESENTATION_LAYER_ASSIGNMENT (  '', '', ( #10343 ) ) ;
#66203 = DIRECTION ( 'NONE',  ( -0.000000000000000000, -0.000000000000000000, -1.000000000000000000 ) ) ;
#66204 = DIRECTION ( 'NONE',  ( 1.000000000000000000, 0.000000000000000000, 0.000000000000000000 ) ) ;
#66205 = DIRECTION ( 'NONE',  ( 0.3826834323650877279, 0.000000000000000000, -0.9238795325112876267 ) ) ;
#66206 = CARTESIAN_POINT ( 'NONE',  ( -0.3289641300568005855, 45.10497603579418069, 5.963430220938281678 ) ) ;
#66207 = CARTESIAN_POINT ( 'NONE',  ( 7.361572987183170547, 17.05059781766745530, 9.846743663894590881 ) ) ;
#66208 = CARTESIAN_POINT ( 'NONE',  ( 21.09922568453595559, 27.04030133659708568, -6.408140936763230044 ) ) ;
#66209 = EDGE_CURVE ( 'NONE', #26872, #62733, #71818, .T. ) ;
#66210 = ORIENTED_EDGE ( 'NONE', *, *, #77155, .T. ) ;
#66211 = CARTESIAN_POINT ( 'NONE',  ( 2.791683348922240793, 51.63393115100078745, 7.208316651077764092 ) ) ;
#66212 = CARTESIAN_POINT ( 'NONE',  ( 14.99999999999997868, 80.07179676972448590, 6.500000000000000888 ) ) ;
#66213 = CARTESIAN_POINT ( 'NONE',  ( -2.266590686148945544, 21.38708216824730357, -7.082119434687050408 ) ) ;
#66214 = CARTESIAN_POINT ( 'NONE',  ( 0.1532563361054082862, 51.21726448433412315, 2.638427012816831674 ) ) ;
#66215 = CARTESIAN_POINT ( 'NONE',  ( 3.591859063236763294, 43.29030133659708923, -11.09922568453595026 ) ) ;
#66217 = SURFACE_SIDE_STYLE ('',( #8565 ) ) ;
#66216 = CARTESIAN_POINT ( 'NONE',  ( -4.250000000000000000, 10.00000000000000000, -4.000000000000000000 ) ) ;
#66218 = CARTESIAN_POINT ( 'NONE',  ( 20.88017736071110164, 65.35535201082150536, 2.915334737309930979 ) ) ;
#66219 = CARTESIAN_POINT ( 'NONE',  ( -10.91061041304814694, 0.2306972965111899476, -10.20767530377064247 ) ) ;
#66220 = CIRCLE ( 'NONE', #19918, 15.00000000000000000 ) ;
#66221 = CARTESIAN_POINT ( 'NONE',  ( 12.63842701281683922, 29.55059781766745175, -9.846743663894590881 ) ) ;
#66222 = CARTESIAN_POINT ( 'NONE',  ( 12.91533473730993009, 41.60535201082149825, -10.88017736071109987 ) ) ;
#66223 = CARTESIAN_POINT ( 'NONE',  ( 16.40814093676324603, 42.45696800326375353, -11.09922568453594671 ) ) ;
#66224 = CARTESIAN_POINT ( 'NONE',  ( 12.63842701281683922, 29.55059781766745175, -9.846743663894590881 ) ) ;
#66225 = CARTESIAN_POINT ( 'NONE',  ( 9.898881779040729967, -0.03417435944610275333, -10.25059215482576214 ) ) ;
#66226 = CARTESIAN_POINT ( 'NONE',  ( 15.44008868035555260, 29.73035201082150891, 9.422509992056143702 ) ) ;
#66227 = ORIENTED_EDGE ( 'NONE', *, *, #62783, .T. ) ;
#66228 = CARTESIAN_POINT ( 'NONE',  ( 3.469446951953614189E-15, 6.368033628982654903, 11.25000000000000178 ) ) ;
#66229 = CARTESIAN_POINT ( 'NONE',  ( 7.084665262690076126, 17.02201867748817676, -10.88017736071110164 ) ) ;
#66231 = CARTESIAN_POINT ( 'NONE',  ( 19.42250999205614193, 40.14701867748817676, 5.440088680355555262 ) ) ;
#66230 = CARTESIAN_POINT ( 'NONE',  ( 14.92337183194729633, 57.67559781766745886, 8.527530157486181039 ) ) ;
#66232 = FACE_OUTER_BOUND ( 'NONE', #10855, .T. ) ;
#66233 = CARTESIAN_POINT ( 'NONE',  ( 2.035157376598822676, 57.43868534415484106, -7.964842623401177768 ) ) ;
#66235 = CARTESIAN_POINT ( 'NONE',  ( -0.000000000000000000, 71.60366622817831228, -5.031467577974828131 ) ) ;
#66234 = CARTESIAN_POINT ( 'NONE',  ( 10.00000000000000178, 24.31368534415484106, 10.88017736071110342 ) ) ;
#66236 = CARTESIAN_POINT ( 'NONE',  ( 0.1532563361054082862, 1.217264484334117824, 2.638427012816831674 ) ) ;
#66237 = CARTESIAN_POINT ( 'NONE',  ( 2.791683348922240793, 21.63393115100078745, 7.208316651077764092 ) ) ;
#66238 = CARTESIAN_POINT ( 'NONE',  ( 10.36894250292379027, 3.678748834913966981, 10.36894250292378672 ) ) ;
#66239 = CARTESIAN_POINT ( 'NONE',  ( 18.52753015748617571, 48.09226448433412315, 4.923371831947298993 ) ) ;
#66241 = CARTESIAN_POINT ( 'NONE',  ( 9.240973841163597768, 15.00000000000000000, -11.17382667070370061 ) ) ;
#66240 = CARTESIAN_POINT ( 'NONE',  ( -0.3689425029237881626, 52.42874883491396076, 10.36894250292379027 ) ) ;
#66242 = CARTESIAN_POINT ( 'NONE',  ( 1.492507162822264366, 62.19955587570481015, -6.500000000000073719 ) ) ;
#66243 = CARTESIAN_POINT ( 'NONE',  ( -2.266590686148945544, 11.38708216824730179, -7.082119434687050408 ) ) ;
#66244 = EDGE_CURVE ( 'NONE', #32140, #35669, #16639, .T. ) ;
#66245 = CARTESIAN_POINT ( 'NONE',  ( 20.36894250292379382, 38.67874883491396076, 10.36894250292379205 ) ) ;
#66246 = CARTESIAN_POINT ( 'NONE',  ( 10.00000000000000000, 7.873634669930421381, -12.81628187352647608 ) ) ;
#66247 = ORIENTED_EDGE ( 'NONE', *, *, #68773, .F. ) ;
#66248 = CARTESIAN_POINT ( 'NONE',  ( 10.00000000000000178, 14.31368534415483929, 10.88017736071110342 ) ) ;
#66249 = EDGE_CURVE ( 'NONE', #5813, #57430, #66776, .T. ) ;
#66250 = CARTESIAN_POINT ( 'NONE',  ( 0.1532563361054082862, 36.21726448433410894, 2.638427012816831674 ) ) ;
#66252 = CARTESIAN_POINT ( 'NONE',  ( -11.21074626900200677, 89.89919991260448739, -6.510369878059174553 ) ) ;
#66251 = DIRECTION ( 'NONE',  ( 0.9099612708765425495, 0.000000000000000000, 0.4146932426562403018 ) ) ;
#66253 = DIRECTION ( 'NONE',  ( 8.673617379884027583E-16, 1.000000000000000000, -0.000000000000000000 ) ) ;
#66254 = SURFACE_SIDE_STYLE ('',( #89263 ) ) ;
#66255 = CARTESIAN_POINT ( 'NONE',  ( 22.81628187352647785, 21.41530133659708923, 3.434112377981063169 ) ) ;
#66256 = CARTESIAN_POINT ( 'NONE',  ( 2.791683348922237240, 30.38393115100078390, -7.208316651077763204 ) ) ;
#66257 = ORIENTED_EDGE ( 'NONE', *, *, #76586, .T. ) ;
#66258 = CARTESIAN_POINT ( 'NONE',  ( 12.63842701281683034, 2.467264484334118269, 9.846743663894596210 ) ) ;
#66259 = CARTESIAN_POINT ( 'NONE',  ( -12.58848565468349001, 1.192622389734054483E-15, -7.447709424580051696 ) ) ;
#66260 = CARTESIAN_POINT ( 'NONE',  ( -0.8801773607110991993, 2.855352010821504471, -2.915334737309923874 ) ) ;
#66261 = CARTESIAN_POINT ( 'NONE',  ( -0.8801773607111008646, 13.27201867748817143, 2.915334737309923430 ) ) ;
#66262 = CARTESIAN_POINT ( 'NONE',  ( 2.917880565312950480, 40.97041550158063217, -12.26659068614894821 ) ) ;
#66263 = CARTESIAN_POINT ( 'NONE',  ( 19.42250999205614193, 40.14701867748817676, 5.440088680355555262 ) ) ;
#66264 = CARTESIAN_POINT ( 'NONE',  ( 4.559911319644449179, 67.23035201082150536, -9.422509992056141925 ) ) ;
#66265 = DIRECTION ( 'NONE',  ( -0.000000000000000000, -0.000000000000000000, 1.000000000000000000 ) ) ;
#66266 = CARTESIAN_POINT ( 'NONE',  ( 21.92686044187657401, 40.37045670184115664, -3.195792623639525765 ) ) ;
#66267 = CARTESIAN_POINT ( 'NONE',  ( 17.20831665107776587, 17.88393115100078745, 7.208316651077764980 ) ) ;
#66268 = SURFACE_STYLE_FILL_AREA ( #73283 ) ;
#66269 = CARTESIAN_POINT ( 'NONE',  ( 14.92337183194729633, 12.67559781766745353, 8.527530157486181039 ) ) ;
#66270 = SURFACE_SIDE_STYLE ('',( #60259 ) ) ;
#66271 = CARTESIAN_POINT ( 'NONE',  ( 10.00000000000000000, 39.75893115100078745, -9.846743663894594434 ) ) ;
#66272 = CARTESIAN_POINT ( 'NONE',  ( 19.84674366389459621, 63.50893115100078745, 7.409399052514197653E-17 ) ) ;
#66273 = CARTESIAN_POINT ( 'NONE',  ( 10.00000000000000000, 31.81368534415483751, -10.88017736071110342 ) ) ;
#66274 = ORIENTED_EDGE ( 'NONE', *, *, #35618, .F. ) ;
#66275 = CARTESIAN_POINT ( 'NONE',  ( 10.00000000000000000, 57.87363466993042493, -12.81628187352647608 ) ) ;
#66277 = EDGE_CURVE ( 'NONE', #1146, #28932, #44062, .T. ) ;
#66276 = FACE_OUTER_BOUND ( 'NONE', #71537, .T. ) ;
#66278 = CARTESIAN_POINT ( 'NONE',  ( 1.472469842513823179, 0.5922644843341181575, -4.923371831947296329 ) ) ;
#66279 = CARTESIAN_POINT ( 'NONE',  ( 22.81628187352648496, 46.83196800326376064, -3.434112377981050290 ) ) ;
#66281 = CARTESIAN_POINT ( 'NONE',  ( 2.791683348922237240, 40.38393115100078035, -7.208316651077763204 ) ) ;
#66280 = CARTESIAN_POINT ( 'NONE',  ( 17.08211943468705130, 63.47041550158063927, 12.26659068614894998 ) ) ;
#66282 = DIRECTION ( 'NONE',  ( 0.000000000000000000, 1.000000000000000000, 0.000000000000000000 ) ) ;
#66283 = CARTESIAN_POINT ( 'NONE',  ( 14.92337183194729988, 59.34226448433412315, -8.527530157486177487 ) ) ;
#66284 = CARTESIAN_POINT ( 'NONE',  ( 13.79529636645031943, 20.34541550158063572, -14.16423886937409904 ) ) ;
#66285 = CARTESIAN_POINT ( 'NONE',  ( 24.16423886937410614, 44.51208216824730357, -3.795296366450302550 ) ) ;
#66286 = CARTESIAN_POINT ( 'NONE',  ( 0.1532563361054100626, 40.80059781766745886, -2.638427012816831230 ) ) ;
#66287 = CARTESIAN_POINT ( 'NONE',  ( -14.88640444357871395, 0.2306972965111902807, 1.277895705730144993 ) ) ;
#66288 = CARTESIAN_POINT ( 'NONE',  ( 7.084665262690076126, 39.10535201082150536, 10.88017736071109987 ) ) ;
#66289 = EDGE_CURVE ( 'NONE', #78236, #33937, #95439, .T. ) ;
#66290 = CARTESIAN_POINT ( 'NONE',  ( 20.88017736071110875, 55.77201867748816966, -2.915334737309920765 ) ) ;
#66291 = CARTESIAN_POINT ( 'NONE',  ( 20.88017736071110875, 50.77201867748817676, -2.915334737309920321 ) ) ;
#66292 = ORIENTED_EDGE ( 'NONE', *, *, #80725, .F. ) ;
#66293 = CARTESIAN_POINT ( 'NONE',  ( -2.816281873526473856, 44.12363466993042493, 9.499525473075851096E-16 ) ) ;
#66294 = CARTESIAN_POINT ( 'NONE',  ( 15.44008868035555793, 66.39701867748817676, -9.422509992056140149 ) ) ;
#66295 = ORIENTED_EDGE ( 'NONE', *, *, #7012, .F. ) ;
#66296 = STYLED_ITEM ( 'NONE', ( #3290 ), #53385 ) ;
#66297 = CARTESIAN_POINT ( 'NONE',  ( -4.164238869374099927, 2.012082168247300906, 3.795296366450308767 ) ) ;
#66298 = CARTESIAN_POINT ( 'NONE',  ( 2.791683348922240793, 6.633931151000785675, 7.208316651077764092 ) ) ;
#66299 = CARTESIAN_POINT ( 'NONE',  ( -14.99847009497950978, 14.49999999999999112, 0.2142307401079103502 ) ) ;
#66300 = ORIENTED_EDGE ( 'NONE', *, *, #53520, .F. ) ;
#66301 = CARTESIAN_POINT ( 'NONE',  ( 0.5774900079438607392, 18.48035201082150536, 5.440088680355550821 ) ) ;
#66302 = CARTESIAN_POINT ( 'NONE',  ( -3.499999999999998668, 1.019547802438465434, -2.500000000000000000 ) ) ;
#66303 = TOROIDAL_SURFACE ( 'NONE', #15231, 14.49999999999999822, 0.5000000000000000000 ) ;
#66304 = CARTESIAN_POINT ( 'NONE',  ( -4.164238869374099039, 16.80374883491396787, 8.674139862899312516E-16 ) ) ;
#66305 = ORIENTED_EDGE ( 'NONE', *, *, #42164, .F. ) ;
#66306 = CARTESIAN_POINT ( 'NONE',  ( 0.5774900079438590739, 17.64701867748817321, -5.440088680355550821 ) ) ;
#66307 = CARTESIAN_POINT ( 'NONE',  ( 0.1532563361054082862, 61.21726448433412315, 2.638427012816831674 ) ) ;
#66308 = ORIENTED_EDGE ( 'NONE', *, *, #18765, .F. ) ;
#66309 = CARTESIAN_POINT ( 'NONE',  ( 19.84674366389459266, 63.30059781766745886, 2.638427012816836559 ) ) ;
#66310 = ORIENTED_EDGE ( 'NONE', *, *, #98402, .T. ) ;
#66311 = TOROIDAL_SURFACE ( 'NONE', #50321, 14.49999999999999822, 0.5000000000000000000 ) ;
#66312 = CARTESIAN_POINT ( 'NONE',  ( 19.84674366389459266, 3.300597817667451750, 2.638427012816836559 ) ) ;
#66313 = CARTESIAN_POINT ( 'NONE',  ( 0.1532563361054082862, 66.21726448433413736, 2.638427012816831674 ) ) ;
#66315 = DIRECTION ( 'NONE',  ( -1.000000000000000000, -0.000000000000000000, -0.000000000000000000 ) ) ;
#66314 = CARTESIAN_POINT ( 'NONE',  ( 4.559911319644449179, 12.23035201082150536, -9.422509992056141925 ) ) ;
#66316 = CARTESIAN_POINT ( 'NONE',  ( 1.472469842513823179, 1.425597817667451528, 4.923371831947296329 ) ) ;
#66317 = CARTESIAN_POINT ( 'NONE',  ( 19.42250999205614193, 20.14701867748817321, 5.440088680355555262 ) ) ;
#66318 = EDGE_CURVE ( 'NONE', #15469, #70448, #94241, .T. ) ;
#66319 = VECTOR ( 'NONE', #49083, 1000.000000000000114 ) ;
#66320 = ORIENTED_EDGE ( 'NONE', *, *, #96097, .F. ) ;
#66321 = CARTESIAN_POINT ( 'NONE',  ( 21.09922568453595559, 57.04030133659708923, -6.408140936763230044 ) ) ;
#66322 = CARTESIAN_POINT ( 'NONE',  ( 17.96484262340118221, 44.93868534415483396, 7.964842623401181321 ) ) ;
#66323 = CARTESIAN_POINT ( 'NONE',  ( 69.60148758828985649, 0.4999999999999935052, -9.500000000000000000 ) ) ;
#66324 = VECTOR ( 'NONE', #10563, 1000.000000000000000 ) ;
#66325 = CARTESIAN_POINT ( 'NONE',  ( -2.816281873526471635, 38.91530133659708213, -3.434112377981056508 ) ) ;
#66326 = CARTESIAN_POINT ( 'NONE',  ( 0.5774900079438607392, 53.48035201082151247, 5.440088680355550821 ) ) ;
#66327 = CARTESIAN_POINT ( 'NONE',  ( 2.791683348922240793, 56.63393115100078035, 7.208316651077764092 ) ) ;
#66328 = ORIENTED_EDGE ( 'NONE', *, *, #87058, .F. ) ;
#66329 = CARTESIAN_POINT ( 'NONE',  ( 19.84674366389459266, 23.30059781766745530, 2.638427012816836559 ) ) ;
#66330 = CARTESIAN_POINT ( 'NONE',  ( 10.00000000000000178, 5.373634669930420493, 12.81628187352647608 ) ) ;
#66332 = CARTESIAN_POINT ( 'NONE',  ( -7.264509831664783590, 14.76984904925306097, 13.05561747642785342 ) ) ;
#66331 = CARTESIAN_POINT ( 'NONE',  ( 7.313705784284503686, 15.00000000000000000, 13.09617149020748705 ) ) ;
#66333 = CARTESIAN_POINT ( 'NONE',  ( 15.44008868035555260, 19.73035201082150536, 9.422509992056143702 ) ) ;
#66334 = CARTESIAN_POINT ( 'NONE',  ( 7.361572987183169658, 54.96726448433413026, -9.846743663894592657 ) ) ;
#66335 = CARTESIAN_POINT ( 'NONE',  ( -0.1503990784575247319, 62.22266099184918176, -6.262539305110083276 ) ) ;
#66336 = CARTESIAN_POINT ( 'NONE',  ( 7.361572987183169658, 4.967264484334119601, -9.846743663894592657 ) ) ;
#66337 = CARTESIAN_POINT ( 'NONE',  ( 2.791683348922237240, 0.3839311510007847872, -7.208316651077763204 ) ) ;
#66339 = ORIENTED_EDGE ( 'NONE', *, *, #21522, .F. ) ;
#66338 = CARTESIAN_POINT ( 'NONE',  ( 1.472469842513823179, 66.42559781766745175, 4.923371831947296329 ) ) ;
#66340 = CARTESIAN_POINT ( 'NONE',  ( -10.93781366033354452, 14.63595249122790598, 10.26470809774058779 ) ) ;
#66341 = CARTESIAN_POINT ( 'NONE',  ( 0.000000000000000000, 15.00000000000000000, 0.000000000000000000 ) ) ;
#66342 = CARTESIAN_POINT ( 'NONE',  ( 3.591859063236763294, 33.29030133659708213, -11.09922568453595026 ) ) ;
#66343 = CARTESIAN_POINT ( 'NONE',  ( 5.076628168052704559, 30.17559781766745175, -8.527530157486179263 ) ) ;
#66344 = CARTESIAN_POINT ( 'NONE',  ( 0.8952175423695086787, 58.52576239577082617, 5.990408912944362285 ) ) ;
#66345 = CARTESIAN_POINT ( 'NONE',  ( 13.79529636645030344, 63.26208216824730357, 14.16423886937410614 ) ) ;
#66346 = CARTESIAN_POINT ( 'NONE',  ( 2.791683348922240793, 26.63393115100078745, 7.208316651077764092 ) ) ;
#66347 = ADVANCED_FACE ( 'NONE', ( #7772 ), #6277, .T. ) ;
#66348 = CARTESIAN_POINT ( 'NONE',  ( 13.99999999999999822, 61.00000000000000711, -5.000000000000000000 ) ) ;
#66349 = CARTESIAN_POINT ( 'NONE',  ( 17.08211943468705840, 60.13708216824729647, -12.26659068614894466 ) ) ;
#66351 = B_SPLINE_CURVE_WITH_KNOTS ( 'NONE', 3,
 ( #25311, #63276, #71294, #92795 ),
 .UNSPECIFIED., .F., .F.,
 ( 4, 4 ),
 ( 7.757919228897728493E-18, 0.002392975128318494595 ),
 .UNSPECIFIED. ) ;
#66350 = DIRECTION ( 'NONE',  ( 0.6038238647437427220, -0.7971177707001206869, 0.000000000000000000 ) ) ;
#66352 = CARTESIAN_POINT ( 'NONE',  ( 2.035157376598822676, 22.43868534415483396, -7.964842623401177768 ) ) ;
#66353 = CARTESIAN_POINT ( 'NONE',  ( -0.3689425029237898834, 56.17874883491396076, -10.36894250292378850 ) ) ;
#66355 = CARTESIAN_POINT ( 'NONE',  ( -46.30928139467842897, 104.0823827281712255, -5.529860068218142466 ) ) ;
#66354 = CARTESIAN_POINT ( 'NONE',  ( -0.3689425029237898834, 56.17874883491396076, -10.36894250292378850 ) ) ;
#66356 =( NAMED_UNIT ( * ) PLANE_ANGLE_UNIT ( ) SI_UNIT ( $, .RADIAN. ) );
#66357 = CARTESIAN_POINT ( 'NONE',  ( 5.076628168052703671, 11.84226448433411960, 8.527530157486179263 ) ) ;
#66358 = CARTESIAN_POINT ( 'NONE',  ( -2.816281873526471635, 3.915301336597087456, -3.434112377981056508 ) ) ;
#66359 = EDGE_LOOP ( 'NONE', ( #82786, #89570, #83736, #70154 ) ) ;
#66360 = CARTESIAN_POINT ( 'NONE',  ( 20.88017736071110519, 55.56368534415484817, 2.639326808657452039E-16 ) ) ;
#66361 = AXIS2_PLACEMENT_3D ( 'NONE', #27743, #59224, #72262 ) ;
#66362 = CARTESIAN_POINT ( 'NONE',  ( 0.1532563361054082862, 61.21726448433412315, 2.638427012816831674 ) ) ;
#66363 = DIRECTION ( 'NONE',  ( 0.000000000000000000, 0.000000000000000000, -1.000000000000000000 ) ) ;
#66364 = CARTESIAN_POINT ( 'NONE',  ( 7.079515573063599021, -88.00917032380691296, -4.000000000000000000 ) ) ;
#66365 = CARTESIAN_POINT ( 'NONE',  ( -4.164238869374099927, 2.012082168247300906, 3.795296366450308767 ) ) ;
#66366 = ORIENTED_EDGE ( 'NONE', *, *, #74756, .T. ) ;
#66367 = CARTESIAN_POINT ( 'NONE',  ( -9.886043635230025828, 89.00072246145502675, 5.688751881067944716 ) ) ;
#66368 = EDGE_LOOP ( 'NONE', ( #69511, #22350, #65105, #31562, #76608, #7451, #5354, #4133, #59551 ) ) ;
#66369 = AXIS2_PLACEMENT_3D ( 'NONE', #56343, #10348, #40848 ) ;
#66370 = CARTESIAN_POINT ( 'NONE',  ( 24.16423886937410614, 34.51208216824731068, -3.795296366450302550 ) ) ;
#66371 = EDGE_CURVE ( 'NONE', #75865, #84653, #33435, .T. ) ;
#66372 = ADVANCED_FACE ( 'NONE', ( #74769 ), #67274, .T. ) ;
#66373 = CARTESIAN_POINT ( 'NONE',  ( 1.472469842513823179, 0.5922644843341181575, -4.923371831947296329 ) ) ;
#66375 = CARTESIAN_POINT ( 'NONE',  ( -8.000000000000000000, 80.99999999999994316, 0.000000000000000000 ) ) ;
#66374 = DIRECTION ( 'NONE',  ( -0.1305261922200653402, -0.000000000000000000, 0.9914448613738086058 ) ) ;
#66376 = CARTESIAN_POINT ( 'NONE',  ( 7.084665262690076126, 22.02201867748817321, -10.88017736071110164 ) ) ;
#66377 = CARTESIAN_POINT ( 'NONE',  ( 13.43411237798106583, 32.66530133659708213, -12.81628187352647252 ) ) ;
#66378 = FILL_AREA_STYLE ('',( #82365 ) ) ;
#66379 = CARTESIAN_POINT ( 'NONE',  ( 13.43411237798106583, 32.66530133659708213, -12.81628187352647252 ) ) ;
#66380 = CARTESIAN_POINT ( 'NONE',  ( 21.09922568453595559, 62.04030133659709634, -6.408140936763230044 ) ) ;
#66381 = EDGE_LOOP ( 'NONE', ( #92857, #58175, #93291, #81270, #73582, #1790 ) ) ;
#66382 = DIRECTION ( 'NONE',  ( 0.000000000000000000, 1.000000000000000000, 0.000000000000000000 ) ) ;
#66383 = B_SPLINE_CURVE_WITH_KNOTS ( 'NONE', 3,
 ( #48680, #49176, #79678, #72166, #85221, #47200 ),
 .UNSPECIFIED., .F., .F.,
 ( 4, 2, 4 ),
 ( 0.0002800313526786637011, 0.0006862368888239586684, 0.001092442424969253690 ),
 .UNSPECIFIED. ) ;
#66384 = CARTESIAN_POINT ( 'NONE',  ( 6.204703633549690345, 27.84541550158063217, 14.16423886937410082 ) ) ;
#66385 = CARTESIAN_POINT ( 'NONE',  ( 8.564643372776616914, 14.49999999999999822, -12.31449893000740836 ) ) ;
#66386 = CARTESIAN_POINT ( 'NONE',  ( 19.42250999205614193, 25.14701867748817321, 5.440088680355555262 ) ) ;
#66387 = CARTESIAN_POINT ( 'NONE',  ( 0.000000000000000000, 0.5000000000000004441, 0.000000000000000000 ) ) ;
#66388 = FACE_OUTER_BOUND ( 'NONE', #96088, .T. ) ;
#66389 = CARTESIAN_POINT ( 'NONE',  ( 7.084665262690076126, 49.10535201082149825, 10.88017736071109987 ) ) ;
#66390 = CARTESIAN_POINT ( 'NONE',  ( 15.44008868035555793, 51.39701867748816966, -9.422509992056140149 ) ) ;
#66391 = CARTESIAN_POINT ( 'NONE',  ( 22.81628187352647785, 11.41530133659708390, 3.434112377981063169 ) ) ;
#66392 = DIRECTION ( 'NONE',  ( -0.8320502943378437211, 0.5547001962252290364, 0.000000000000000000 ) ) ;
#66393 = DIRECTION ( 'NONE',  ( -0.000000000000000000, -0.000000000000000000, -1.000000000000000000 ) ) ;
#66394 = CARTESIAN_POINT ( 'NONE',  ( 19.84674366389459266, 18.71726448433411960, -2.638427012816827677 ) ) ;
#66395 = CARTESIAN_POINT ( 'NONE',  ( -2.614810775378867191, 35.00346125376525919, -9.500000000000000000 ) ) ;
#66396 = CARTESIAN_POINT ( 'NONE',  ( 10.00000000000000178, 44.31368534415484106, 10.88017736071110342 ) ) ;
#66397 = AXIS2_PLACEMENT_3D ( 'NONE', #14427, #5933, #98437 ) ;
#66398 = UNCERTAINTY_MEASURE_WITH_UNIT (LENGTH_MEASURE( 1.000000000000000082E-05 ), #75256, 'distance_accuracy_value', 'NONE');
#66399 = AXIS2_PLACEMENT_3D ( 'NONE', #64321, #93358, #94832 ) ;
#66400 = VECTOR ( 'NONE', #40922, 1000.000000000000000 ) ;
#66402 = EDGE_CURVE ( 'NONE', #76544, #19964, #30363, .T. ) ;
#66401 = CARTESIAN_POINT ( 'NONE',  ( 13.43411237798105340, 10.58196800326375353, 12.81628187352647963 ) ) ;
#66403 = DIRECTION ( 'NONE',  ( 1.000000000000000000, 0.000000000000000000, 0.000000000000000000 ) ) ;
#66404 = CARTESIAN_POINT ( 'NONE',  ( 14.92337183194729988, 29.34226448433411960, -8.527530157486177487 ) ) ;
#66405 = CARTESIAN_POINT ( 'NONE',  ( 22.81628187352647785, 51.41530133659708923, 3.434112377981063169 ) ) ;
#66406 = CARTESIAN_POINT ( 'NONE',  ( 12.63842701281683922, 24.55059781766745175, -9.846743663894590881 ) ) ;
#66407 = EDGE_LOOP ( 'NONE', ( #73078, #52657, #4430, #18784 ) ) ;
#66408 = CARTESIAN_POINT ( 'NONE',  ( 17.08211943468705840, 10.13708216824730179, -12.26659068614894466 ) ) ;
#66409 = CARTESIAN_POINT ( 'NONE',  ( -47.70923076923077133, 97.34615384615383959, -9.500000000000000000 ) ) ;
#66410 = CARTESIAN_POINT ( 'NONE',  ( 0.5774900079438607392, 18.48035201082150536, 5.440088680355550821 ) ) ;
#66412 = CARTESIAN_POINT ( 'NONE',  ( 13.79529636645031943, 30.34541550158063927, -14.16423886937409904 ) ) ;
#66411 = DIRECTION ( 'NONE',  ( -0.3173046564050834295, 0.000000000000000000, -0.9483236552062023206 ) ) ;
#66413 = EDGE_CURVE ( 'NONE', #92402, #74265, #68759, .T. ) ;
#66414 = CARTESIAN_POINT ( 'NONE',  ( 18.52753015748618282, 33.92559781766745886, -4.923371831947291888 ) ) ;
#66415 = CARTESIAN_POINT ( 'NONE',  ( 20.88017736071110164, 15.35535201082150358, 2.915334737309930979 ) ) ;
#66416 = CARTESIAN_POINT ( 'NONE',  ( 22.26659068614894466, 63.88708216824730357, 7.082119434687054849 ) ) ;
#66417 = ORIENTED_EDGE ( 'NONE', *, *, #2197, .F. ) ;
#66418 = CARTESIAN_POINT ( 'NONE',  ( 10.00000000000000000, 21.81368534415484106, -10.88017736071110342 ) ) ;
#66419 = CARTESIAN_POINT ( 'NONE',  ( 7.084665262690076126, 39.10535201082150536, 10.88017736071109987 ) ) ;
#66420 = CARTESIAN_POINT ( 'NONE',  ( 0.4195498155886434599, 0.4999999999999998890, -9.500000000000000000 ) ) ;
#66421 = VERTEX_POINT ( 'NONE', #93705 ) ;
#66422 = CARTESIAN_POINT ( 'NONE',  ( 18.52753015748617571, 53.09226448433412315, 4.923371831947298993 ) ) ;
#66423 = CARTESIAN_POINT ( 'NONE',  ( -0.8801773607111009756, 33.06368534415484106, 1.068504757029289695E-15 ) ) ;
#66424 = VECTOR ( 'NONE', #10438, 1000.000000000000000 ) ;
#66425 = PLANE ( 'NONE',  #36110 ) ;
#66426 = CARTESIAN_POINT ( 'NONE',  ( 6.565887622018943937, 60.16530133659707502, 12.81628187352647430 ) ) ;
#66427 = CARTESIAN_POINT ( 'NONE',  ( 19.72487221294571569, 30.71833443783938122, -6.499999999999989342 ) ) ;
#66428 = CARTESIAN_POINT ( 'NONE',  ( -4.164238869374099039, 36.80374883491396787, 8.674139862899312516E-16 ) ) ;
#66429 = CARTESIAN_POINT ( 'NONE',  ( 20.88017736071110164, 55.35535201082149825, 2.915334737309930979 ) ) ;
#66430 = CARTESIAN_POINT ( 'NONE',  ( 2.791683348922237240, 65.38393115100078035, -7.208316651077763204 ) ) ;
#66431 = PLANE ( 'NONE',  #20602 ) ;
#66432 = CARTESIAN_POINT ( 'NONE',  ( 10.00000000000000000, 44.75893115100078745, -9.846743663894594434 ) ) ;
#66433 = CARTESIAN_POINT ( 'NONE',  ( 18.52753015748618282, 3.925597817667451306, -4.923371831947291888 ) ) ;
#66434 = ORIENTED_EDGE ( 'NONE', *, *, #19577, .F. ) ;
#66435 = CARTESIAN_POINT ( 'NONE',  ( 2.791683348922237240, 20.38393115100078745, -7.208316651077763204 ) ) ;
#66436 = CARTESIAN_POINT ( 'NONE',  ( 3.434112377981060948, -24.41803199673624647, 12.81628187352647430 ) ) ;
#66437 = CARTESIAN_POINT ( 'NONE',  ( 10.00000000000000000, 21.81368534415484106, -10.88017736071110342 ) ) ;
#66438 = CARTESIAN_POINT ( 'NONE',  ( 0.1532563361054083140, 21.00893115100078745, 1.131784320476157264E-15 ) ) ;
#66439 = CARTESIAN_POINT ( 'NONE',  ( 13.43411237798106583, 7.665301336597086568, -12.81628187352647252 ) ) ;
#66440 = CARTESIAN_POINT ( 'NONE',  ( 15.44008868035555260, 59.73035201082151247, 9.422509992056143702 ) ) ;
#66442 = CARTESIAN_POINT ( 'NONE',  ( 6.565887622018943937, 60.16530133659707502, 12.81628187352647430 ) ) ;
#66441 = CARTESIAN_POINT ( 'NONE',  ( 7.084665262690076126, 37.02201867748817676, -10.88017736071110164 ) ) ;
#66443 = CARTESIAN_POINT ( 'NONE',  ( -0.3689425029237881626, 42.42874883491396787, 10.36894250292379027 ) ) ;
#66444 = AXIS2_PLACEMENT_3D ( 'NONE', #49148, #72618, #58612 ) ;
#66445 = CARTESIAN_POINT ( 'NONE',  ( -13.16767742306221400, 0.04962884061926597229, 6.653539137814544979 ) ) ;
#66446 = ORIENTED_EDGE ( 'NONE', *, *, #79376, .T. ) ;
#66447 = CARTESIAN_POINT ( 'NONE',  ( 0.1532563361054100626, 65.80059781766745175, -2.638427012816831230 ) ) ;
#66448 = CARTESIAN_POINT ( 'NONE',  ( 4.559911319644449179, 2.230352010821504471, -9.422509992056141925 ) ) ;
#66449 = CARTESIAN_POINT ( 'NONE',  ( 20.88017736071110519, 40.56368534415484106, 2.639326808657452039E-16 ) ) ;
#66450 = CARTESIAN_POINT ( 'NONE',  ( 12.63842701281683034, 57.46726448433411605, 9.846743663894596210 ) ) ;
#66451 = VERTEX_POINT ( 'NONE', #70732 ) ;
#66452 = CARTESIAN_POINT ( 'NONE',  ( 12.63842701281683034, 17.46726448433411250, 9.846743663894596210 ) ) ;
#66453 = CARTESIAN_POINT ( 'NONE',  ( -0.8801773607111009756, 53.06368534415484106, 1.068504757029289695E-15 ) ) ;
#66454 = CARTESIAN_POINT ( 'NONE',  ( 2.791683348922240793, 31.63393115100078745, 7.208316651077764092 ) ) ;
#66455 = CARTESIAN_POINT ( 'NONE',  ( 0.1532563361054083140, 31.00893115100078390, 1.131784320476157264E-15 ) ) ;
#66456 = B_SPLINE_CURVE_WITH_KNOTS ( 'NONE', 3,
 ( #54540, #32029, #610, #31054 ),
 .UNSPECIFIED., .F., .F.,
 ( 4, 4 ),
 ( 1.097135458930219287E-17, 0.001060528352561992873 ),
 .UNSPECIFIED. ) ;
#66457 = AXIS2_PLACEMENT_3D ( 'NONE', #51251, #68731, #75231 ) ;
#66458 = CARTESIAN_POINT ( 'NONE',  ( 17.20831665107776587, 7.883931151000784787, 7.208316651077764980 ) ) ;
#66459 = EDGE_CURVE ( 'NONE', #43481, #1023, #57557, .T. ) ;
#66461 = CARTESIAN_POINT ( 'NONE',  ( -2.816281873526471635, 33.91530133659708213, -3.434112377981056508 ) ) ;
#66460 = LINE ( 'NONE', #59448, #14951 ) ;
#66463 = DIRECTION ( 'NONE',  ( 0.000000000000000000, 1.000000000000000000, 0.000000000000000000 ) ) ;
#66462 = CARTESIAN_POINT ( 'NONE',  ( 19.42250999205614193, 65.14701867748817676, 5.440088680355555262 ) ) ;
#66464 = CARTESIAN_POINT ( 'NONE',  ( 14.92337183194729633, 2.675597817667451750, 8.527530157486181039 ) ) ;
#66465 = AXIS2_PLACEMENT_3D ( 'NONE', #89247, #49756, #43740 ) ;
#66467 = ORIENTED_EDGE ( 'NONE', *, *, #79732, .F. ) ;
#66466 = CARTESIAN_POINT ( 'NONE',  ( 2.791683348922240793, 26.63393115100078745, 7.208316651077764092 ) ) ;
#66468 = CIRCLE ( 'NONE', #72884, 15.00000000000000000 ) ;
#66469 = B_SPLINE_CURVE_WITH_KNOTS ( 'NONE', 3,
 ( #31014, #77999, #70508, #46038, #61022, #9505, #7563, #38050, #32494, #54019 ),
 .UNSPECIFIED., .F., .F.,
 ( 4, 3, 3, 4 ),
 ( 7.757919228897728493E-18, 0.0006253016069561031978, 0.001250604074564932999, 0.002501455912506560415 ),
 .UNSPECIFIED. ) ;
#66470 = CARTESIAN_POINT ( 'NONE',  ( 4.906773990575423738, -8.256880746075376365, 3.999999999999999112 ) ) ;
#66471 = CARTESIAN_POINT ( 'NONE',  ( 5.076628168052703671, 66.84226448433412315, 8.527530157486179263 ) ) ;
#66472 = CARTESIAN_POINT ( 'NONE',  ( 7.084665262690076126, 2.022018677488170990, -10.88017736071110164 ) ) ;
#66473 = CIRCLE ( 'NONE', #87238, 2.896551724137931494 ) ;
#66474 = CARTESIAN_POINT ( 'NONE',  ( 24.16423886937410614, 14.51208216824730179, -3.795296366450302550 ) ) ;
#66475 = UNCERTAINTY_MEASURE_WITH_UNIT (LENGTH_MEASURE( 1.000000000000000082E-05 ), #67377, 'distance_accuracy_value', 'NONE');
#66476 = FACE_OUTER_BOUND ( 'NONE', #82457, .T. ) ;
#66477 = CARTESIAN_POINT ( 'NONE',  ( -4.164238869374099039, 11.80374883491396965, 8.674139862899312516E-16 ) ) ;
#66478 = CARTESIAN_POINT ( 'NONE',  ( -4.164238869374098151, 46.59541550158063927, -3.795296366450310543 ) ) ;
#66479 = CARTESIAN_POINT ( 'NONE',  ( -0.3689425029237898834, 1.178748834913967869, -10.36894250292378850 ) ) ;
#66481 = CARTESIAN_POINT ( 'NONE',  ( 19.42250999205614193, 65.14701867748817676, 5.440088680355555262 ) ) ;
#66480 = CARTESIAN_POINT ( 'NONE',  ( 2.917880565312950480, 10.97041550158063572, -12.26659068614894821 ) ) ;
#66482 = CARTESIAN_POINT ( 'NONE',  ( 20.88017736071110875, 45.77201867748816966, -2.915334737309920765 ) ) ;
#66483 = CARTESIAN_POINT ( 'NONE',  ( -11.59608414876355198, 14.76930270348881002, 9.421724210956202938 ) ) ;
#66484 = ORIENTED_EDGE ( 'NONE', *, *, #33090, .F. ) ;
#66485 = CARTESIAN_POINT ( 'NONE',  ( 14.92337183194729988, 34.34226448433411605, -8.527530157486177487 ) ) ;
#66486 = EDGE_CURVE ( 'NONE', #19583, #16885, #90646, .T. ) ;
#66488 = CARTESIAN_POINT ( 'NONE',  ( 19.84674366389459266, 23.71726448433412315, -2.638427012816827677 ) ) ;
#66487 = CARTESIAN_POINT ( 'NONE',  ( -0.8801773607111008646, 63.27201867748817676, 2.915334737309923430 ) ) ;
#66489 = ORIENTED_EDGE ( 'NONE', *, *, #93846, .T. ) ;
#66490 = CARTESIAN_POINT ( 'NONE',  ( 2.035157376598824452, 8.688685344154839285, 7.964842623401179544 ) ) ;
#66491 = CARTESIAN_POINT ( 'NONE',  ( -2.816281873526473856, 54.12363466993041783, 9.499525473075851096E-16 ) ) ;
#66492 = CARTESIAN_POINT ( 'NONE',  ( 7.361572987183170547, 52.05059781766745175, 9.846743663894590881 ) ) ;
#66493 = CARTESIAN_POINT ( 'NONE',  ( -6.581680125707231710, -88.31141629936868753, 3.750000000000000000 ) ) ;
#66494 = CARTESIAN_POINT ( 'NONE',  ( 2.791683348922240793, 31.63393115100078745, 7.208316651077764092 ) ) ;
#66496 = CARTESIAN_POINT ( 'NONE',  ( 13.43411237798105340, 45.58196800326374643, 12.81628187352647963 ) ) ;
#66495 = CIRCLE ( 'NONE', #63272, 15.00000000000000000 ) ;
#66497 = CARTESIAN_POINT ( 'NONE',  ( 3.795296366450314540, -21.73791783175269998, 14.16423886937410082 ) ) ;
#66498 = CARTESIAN_POINT ( 'NONE',  ( 0.5774900079438590739, 37.64701867748817676, -5.440088680355550821 ) ) ;
#66499 = CARTESIAN_POINT ( 'NONE',  ( 0.1532563361054083140, 36.00893115100078745, 1.131784320476157264E-15 ) ) ;
#66500 = ADVANCED_FACE ( 'NONE', ( #84742 ), #12810, .T. ) ;
#66501 = CARTESIAN_POINT ( 'NONE',  ( 17.08211943468705130, 23.47041550158063572, 12.26659068614894998 ) ) ;
#66502 = ORIENTED_EDGE ( 'NONE', *, *, #92365, .T. ) ;
#66503 = CARTESIAN_POINT ( 'NONE',  ( 24.16423886937409904, 4.095415501580634832, 3.795296366450317205 ) ) ;
#66504 = EDGE_CURVE ( 'NONE', #32902, #78512, #53641, .T. ) ;
#66505 = CARTESIAN_POINT ( 'NONE',  ( 0.5774900079438607392, 48.48035201082150536, 5.440088680355550821 ) ) ;
#66506 = CARTESIAN_POINT ( 'NONE',  ( 10.00000000000000178, 64.31368534415483396, 10.88017736071110342 ) ) ;
#66507 = CARTESIAN_POINT ( 'NONE',  ( -2.266590686148945544, 46.38708216824730357, -7.082119434687050408 ) ) ;
#66508 = CARTESIAN_POINT ( 'NONE',  ( 13.43411237798106583, 2.665301336597086568, -12.81628187352647252 ) ) ;
#66509 = CARTESIAN_POINT ( 'NONE',  ( 13.43411237798106583, 62.66530133659708923, -12.81628187352647252 ) ) ;
#66510 = CARTESIAN_POINT ( 'NONE',  ( 15.44008868035555260, 49.73035201082150536, 9.422509992056143702 ) ) ;
#66511 = CARTESIAN_POINT ( 'NONE',  ( 0.000000000000000000, 14.49999999999999822, 0.000000000000000000 ) ) ;
#66512 = CARTESIAN_POINT ( 'NONE',  ( 21.09922568453595559, 2.040301336597086568, -6.408140936763230044 ) ) ;
#66513 = CARTESIAN_POINT ( 'NONE',  ( 9.422509992056141925, 25.98035201082152312, -5.440088680355554374 ) ) ;
#66514 = CARTESIAN_POINT ( 'NONE',  ( -0.8801773607111009756, 18.06368534415484106, 1.068504757029289695E-15 ) ) ;
#66515 = CARTESIAN_POINT ( 'NONE',  ( 12.91533473730992121, 9.522018677488171434, 10.88017736071110164 ) ) ;
#66516 =( NAMED_UNIT ( * ) PLANE_ANGLE_UNIT ( ) SI_UNIT ( $, .RADIAN. ) );
#66517 = ORIENTED_EDGE ( 'NONE', *, *, #58179, .F. ) ;
#66518 = AXIS2_PLACEMENT_3D ( 'NONE', #89649, #13154, #80676 ) ;
#66519 = CARTESIAN_POINT ( 'NONE',  ( 12.91533473730992121, 9.522018677488171434, 10.88017736071110164 ) ) ;
#66520 = CARTESIAN_POINT ( 'NONE',  ( 17.20831665107776587, 2.883931151000785231, 7.208316651077764980 ) ) ;
#66521 = CIRCLE ( 'NONE', #69745, 6.599999999999995204 ) ;
#66522 = B_SPLINE_CURVE_WITH_KNOTS ( 'NONE', 3,
 ( #54453, #24970, #46467, #40461, #25468, #10445 ),
 .UNSPECIFIED., .F., .F.,
 ( 4, 2, 4 ),
 ( 3.409110551378489334E-05, 0.0004400426677356115675, 0.0008459942299574381604 ),
 .UNSPECIFIED. ) ;
#66523 = CARTESIAN_POINT ( 'NONE',  ( 2.791683348922237240, 30.38393115100078390, -7.208316651077763204 ) ) ;
#66524 = CARTESIAN_POINT ( 'NONE',  ( 12.91533473730992121, 39.52201867748817676, 10.88017736071110164 ) ) ;
#66525 = CARTESIAN_POINT ( 'NONE',  ( 3.591859063236761518, 9.956968003263753531, 11.09922568453594849 ) ) ;
#66527 = DIRECTION ( 'NONE',  ( 0.000000000000000000, 2.602085213965208275E-15, -1.000000000000000000 ) ) ;
#66526 = CARTESIAN_POINT ( 'NONE',  ( 19.42250999205614193, 30.14701867748817321, 5.440088680355555262 ) ) ;
#66528 = CARTESIAN_POINT ( 'NONE',  ( 9.879999999999990123, 20.99999999999999645, 0.000000000000000000 ) ) ;
#66529 = CARTESIAN_POINT ( 'NONE',  ( 22.81628187352647785, 36.41530133659707502, 3.434112377981063169 ) ) ;
#66530 = VERTEX_POINT ( 'NONE', #47216 ) ;
#66531 = CARTESIAN_POINT ( 'NONE',  ( 4.559911319644449179, 67.23035201082150536, -9.422509992056141925 ) ) ;
#66532 = CARTESIAN_POINT ( 'NONE',  ( 13.43411237798105340, 35.58196800326375353, 12.81628187352647963 ) ) ;
#66533 = EDGE_CURVE ( 'NONE', #10040, #35492, #22401, .T. ) ;
#66534 = CARTESIAN_POINT ( 'NONE',  ( 0.1532563361054100626, 0.8005978176674514168, -2.638427012816831230 ) ) ;
#66535 = CARTESIAN_POINT ( 'NONE',  ( 20.88017736071110164, 40.35535201082150536, 2.915334737309930979 ) ) ;
#66536 = DIRECTION ( 'NONE',  ( 0.000000000000000000, 1.000000000000000000, 0.000000000000000000 ) ) ;
#66537 = CARTESIAN_POINT ( 'NONE',  ( 10.00000000000000000, 60.55374883491397497, -14.16423886937410082 ) ) ;
#66538 = CARTESIAN_POINT ( 'NONE',  ( 19.84674366389459266, 53.71726448433411605, -2.638427012816827677 ) ) ;
#66539 = CARTESIAN_POINT ( 'NONE',  ( 18.52753015748618282, 18.92559781766745175, -4.923371831947291888 ) ) ;
#66540 = CARTESIAN_POINT ( 'NONE',  ( 20.88017736071110164, 65.35535201082150536, 2.915334737309930979 ) ) ;
#66541 = DIRECTION ( 'NONE',  ( -2.569960705150826877E-16, 1.000000000000000000, 0.000000000000000000 ) ) ;
#66542 = CARTESIAN_POINT ( 'NONE',  ( -2.266590686148945544, 32.22041550158063927, 7.082119434687048631 ) ) ;
#66543 = CARTESIAN_POINT ( 'NONE',  ( 20.15039907845753220, 25.60158574516642815, -6.262539305110077947 ) ) ;
#66544 = B_SPLINE_CURVE_WITH_KNOTS ( 'NONE', 3,
 ( #20468, #50955, #66445, #81451, #12952, #5960 ),
 .UNSPECIFIED., .F., .F.,
 ( 4, 2, 4 ),
 ( 0.0002800760588349525144, 0.0006862820326512275061, 0.001092488006467502498 ),
 .UNSPECIFIED. ) ;
#66545 = CARTESIAN_POINT ( 'NONE',  ( 11.13575493849772258, -94.04002841299546844, -3.749999999999999556 ) ) ;
#66546 = CARTESIAN_POINT ( 'NONE',  ( -3.522141228383032008, -0.8488377519105428926, -3.750000000000000000 ) ) ;
#66547 = EDGE_LOOP ( 'NONE', ( #85399, #52088, #4813, #21663 ) ) ;
#66548 = VERTEX_POINT ( 'NONE', #40222 ) ;
#66549 = CARTESIAN_POINT ( 'NONE',  ( -0.3689425029237898834, 61.17874883491396076, -10.36894250292378850 ) ) ;
#66550 = CARTESIAN_POINT ( 'NONE',  ( 22.26659068614894466, 58.88708216824729647, 7.082119434687054849 ) ) ;
#66551 = CARTESIAN_POINT ( 'NONE',  ( 0.1532563361054083140, 31.00893115100078390, 1.131784320476157264E-15 ) ) ;
#66552 = CARTESIAN_POINT ( 'NONE',  ( 6.565887622018943937, 30.16530133659708568, 12.81628187352647430 ) ) ;
#66553 = CARTESIAN_POINT ( 'NONE',  ( 0.000000000000000000, 14.49999999999999822, 0.000000000000000000 ) ) ;
#66554 = CARTESIAN_POINT ( 'NONE',  ( 20.88017736071110519, 10.56368534415483751, 2.639326808657452039E-16 ) ) ;
#66555 = CARTESIAN_POINT ( 'NONE',  ( 20.36894250292379738, 54.92874883491396076, -10.36894250292379027 ) ) ;
#66556 = CIRCLE ( 'NONE', #26637, 14.49999999999999822 ) ;
#66557 = CARTESIAN_POINT ( 'NONE',  ( 18.52753015748618282, 33.92559781766745886, -4.923371831947291888 ) ) ;
#66558 = CARTESIAN_POINT ( 'NONE',  ( -10.09048698379360687, 46.92328126389585208, -2.900000000000000355 ) ) ;
#66559 = CARTESIAN_POINT ( 'NONE',  ( 7.361572987183170547, 7.050597817667451750, 9.846743663894590881 ) ) ;
#66560 = CARTESIAN_POINT ( 'NONE',  ( 17.39651004071841101, 57.93575266056827644, 6.500000000000005329 ) ) ;
#66561 = CARTESIAN_POINT ( 'NONE',  ( -2.638427012816824124, 22.05059781766745886, 9.846743663894596210 ) ) ;
#66562 = ORIENTED_EDGE ( 'NONE', *, *, #26204, .T. ) ;
#66563 = EDGE_LOOP ( 'NONE', ( #61497, #8293, #75901, #64854 ) ) ;
#66564 = ORIENTED_EDGE ( 'NONE', *, *, #54141, .F. ) ;
#66566 = CARTESIAN_POINT ( 'NONE',  ( 17.20831665107776587, 44.13393115100078745, -7.208316651077762316 ) ) ;
#66565 = COLOUR_RGB ( '', 0.72549020, 0.75294118, 0.79215686) ;
#66568 = CARTESIAN_POINT ( 'NONE',  ( 12.91533473730993009, 21.60535201082150536, -10.88017736071109987 ) ) ;
#66567 = CARTESIAN_POINT ( 'NONE',  ( 4.559911319644449179, 18.89701867748817321, 9.422509992056141925 ) ) ;
#66570 = CARTESIAN_POINT ( 'NONE',  ( 22.81628187352647785, 16.41530133659708923, 3.434112377981063169 ) ) ;
#66569 = FILL_AREA_STYLE_COLOUR ( '', #16408 ) ;
#66571 = CARTESIAN_POINT ( 'NONE',  ( 6.204703633549690345, 0.7620821682473009062, -14.16423886937410259 ) ) ;
#66572 = AXIS2_PLACEMENT_3D ( 'NONE', #91062, #7594, #22096 ) ;
#66573 = AXIS2_PLACEMENT_3D ( 'NONE', #72069, #12058, #26565 ) ;
#66574 = AXIS2_PLACEMENT_3D ( 'NONE', #72506, #49027, #33035 ) ;
#66575 = CARTESIAN_POINT ( 'NONE',  ( 22.81628187352647785, 36.62363466993041783, 6.195893100308588602E-16 ) ) ;
#66577 = ORIENTED_EDGE ( 'NONE', *, *, #11961, .T. ) ;
#66576 = CARTESIAN_POINT ( 'NONE',  ( 7.361572987183169658, -0.03273551566588185635, -9.846743663894592657 ) ) ;
#66578 = CARTESIAN_POINT ( 'NONE',  ( 5.076628168052703671, 31.84226448433412315, 8.527530157486179263 ) ) ;
#66579 = CARTESIAN_POINT ( 'NONE',  ( 15.44008868035555793, 6.397018677488171434, -9.422509992056140149 ) ) ;
#66580 = VERTEX_POINT ( 'NONE', #48200 ) ;
#66581 = CARTESIAN_POINT ( 'NONE',  ( 15.44008868035555793, 6.397018677488171434, -9.422509992056140149 ) ) ;
#66582 = ORIENTED_EDGE ( 'NONE', *, *, #57142, .T. ) ;
#66583 = CARTESIAN_POINT ( 'NONE',  ( -0.8801773607111009756, 43.06368534415484106, 1.068504757029289695E-15 ) ) ;
#66584 = CARTESIAN_POINT ( 'NONE',  ( 17.96484262340118221, 59.93868534415484106, 7.964842623401181321 ) ) ;
#66585 = CARTESIAN_POINT ( 'NONE',  ( 20.88017736071110519, 55.56368534415484817, 2.639326808657452039E-16 ) ) ;
#66586 = CARTESIAN_POINT ( 'NONE',  ( 0.1532563361054083140, 1.008931151000784787, 1.131784320476157264E-15 ) ) ;
#66587 = CARTESIAN_POINT ( 'NONE',  ( 0.5774900079438607392, 43.48035201082151247, 5.440088680355550821 ) ) ;
#66588 = CARTESIAN_POINT ( 'NONE',  ( -46.94000000000001904, 101.9887809003992913, 6.851115700668153785 ) ) ;
#66589 = EDGE_CURVE ( 'NONE', #5813, #24761, #67997, .T. ) ;
#66591 = ORIENTED_EDGE ( 'NONE', *, *, #44311, .T. ) ;
#66590 = DIRECTION ( 'NONE',  ( 0.000000000000000000, 0.000000000000000000, -1.000000000000000000 ) ) ;
#66592 = CARTESIAN_POINT ( 'NONE',  ( 7.361572987183169658, 34.96726448433411605, -9.846743663894592657 ) ) ;
#66593 = ORIENTED_EDGE ( 'NONE', *, *, #15246, .T. ) ;
#66594 = CARTESIAN_POINT ( 'NONE',  ( 1.472469842513823179, 55.59226448433412315, -4.923371831947296329 ) ) ;
#66595 = CARTESIAN_POINT ( 'NONE',  ( 14.97687855664607781, 15.00000000000000000, 0.8325315005901553489 ) ) ;
#66596 = STYLED_ITEM ( 'NONE', ( #17421 ), #30369 ) ;
#66597 = CARTESIAN_POINT ( 'NONE',  ( 13.79529636645031943, 5.345415501580634832, -14.16423886937409904 ) ) ;
#66598 = ORIENTED_EDGE ( 'NONE', *, *, #46303, .T. ) ;
#66599 = CARTESIAN_POINT ( 'NONE',  ( -11.30818108475026129, 12.95584178848497281, 3.038558417133429668 ) ) ;
#66600 = CARTESIAN_POINT ( 'NONE',  ( -1.983216688680738082, 0.000000000000000000, -14.11131997956740491 ) ) ;
#66601 = PRESENTATION_STYLE_ASSIGNMENT (( #57610 ) ) ;
#66602 = CARTESIAN_POINT ( 'NONE',  ( -0.3689425029237881626, 57.42874883491397497, 10.36894250292379027 ) ) ;
#66603 = CARTESIAN_POINT ( 'NONE',  ( 38.04706783004212411, 28.99999999999999645, 7.000000000000000000 ) ) ;
#66604 = EDGE_LOOP ( 'NONE', ( #96313, #73797, #77755, #51843, #69608, #77485 ) ) ;
#66605 = CARTESIAN_POINT ( 'NONE',  ( 20.10239578412224759, 62.63377557478298741, -6.340343622311902294 ) ) ;
#66606 = CARTESIAN_POINT ( 'NONE',  ( 7.361572987183170547, 52.05059781766745175, 9.846743663894590881 ) ) ;
#66607 = FACE_OUTER_BOUND ( 'NONE', #97697, .T. ) ;
#66608 = CARTESIAN_POINT ( 'NONE',  ( 10.00000000000000178, 25.37363466993041783, 12.81628187352647608 ) ) ;
#66609 = CARTESIAN_POINT ( 'NONE',  ( 14.92337183194729633, 7.675597817667451750, 8.527530157486181039 ) ) ;
#66610 = DIRECTION ( 'NONE',  ( 0.000000000000000000, 0.000000000000000000, 1.000000000000000000 ) ) ;
#66611 = CARTESIAN_POINT ( 'NONE',  ( 10.00000000000000178, 12.25893115100078568, 9.846743663894594434 ) ) ;
#66612 = CARTESIAN_POINT ( 'NONE',  ( 10.00000000000000000, 2.873634669930420049, -12.81628187352647608 ) ) ;
#66613 = DIRECTION ( 'NONE',  ( 0.000000000000000000, 0.000000000000000000, -1.000000000000000000 ) ) ;
#66614 = EDGE_CURVE ( 'NONE', #70343, #44664, #25610, .T. ) ;
#66615 = ORIENTED_EDGE ( 'NONE', *, *, #87848, .F. ) ;
#66616 = EDGE_CURVE ( 'NONE', #7648, #54903, #65655, .T. ) ;
#66617 = CARTESIAN_POINT ( 'NONE',  ( 4.559911319644449179, 3.897018677488171434, 9.422509992056141925 ) ) ;
#66618 = CARTESIAN_POINT ( 'NONE',  ( 17.08211943468705130, 8.470415501580635720, 12.26659068614894998 ) ) ;
#66619 = CARTESIAN_POINT ( 'NONE',  ( 5.076628168052704559, 30.17559781766745175, -8.527530157486179263 ) ) ;
#66620 = CARTESIAN_POINT ( 'NONE',  ( 12.91533473730993009, 51.60535201082149825, -10.88017736071109987 ) ) ;
#66622 = PLANE ( 'NONE',  #56050 ) ;
#66621 = CARTESIAN_POINT ( 'NONE',  ( -2.816281873526471635, 28.91530133659708213, -3.434112377981056508 ) ) ;
#66623 = CARTESIAN_POINT ( 'NONE',  ( 15.44008868035555793, 16.39701867748817321, -9.422509992056140149 ) ) ;
#66624 = LINE ( 'NONE', #97152, #82047 ) ;
#66625 = CIRCLE ( 'NONE', #98579, 15.00000000000000000 ) ;
#66626 = CARTESIAN_POINT ( 'NONE',  ( 0.6178305044545838731, -0.2513653300695798953, 9.382169495545420901 ) ) ;
#66627 = CARTESIAN_POINT ( 'NONE',  ( 22.81628187352647785, 1.623634669930420271, 6.195893100308588602E-16 ) ) ;
#66628 = CARTESIAN_POINT ( 'NONE',  ( 17.20831665107776587, 12.88393115100078390, 7.208316651077764980 ) ) ;
#66629 = CARTESIAN_POINT ( 'NONE',  ( -5.440088680355558814, -27.76964798917849109, -9.422509992056136596 ) ) ;
#66630 = CARTESIAN_POINT ( 'NONE',  ( 21.09922568453595559, 37.04030133659708923, -6.408140936763230044 ) ) ;
#66631 = CARTESIAN_POINT ( 'NONE',  ( 8.629999999999995453, 41.24999999999999289, 6.250000000000000000 ) ) ;
#66632 = PRODUCT_DEFINITION ( 'UNKNOWN', '', #842, #36482 ) ;
#66635 = CARTESIAN_POINT ( 'NONE',  ( 12.87890026492940088, 0.04922511925147125822, -7.195834080858350745 ) ) ;
#66634 = B_SPLINE_CURVE_WITH_KNOTS ( 'NONE', 3,
 ( #75160, #6671, #68173, #98189 ),
 .UNSPECIFIED., .F., .F.,
 ( 4, 4 ),
 ( 0.000000000000000000, 0.0006041882680322678990 ),
 .UNSPECIFIED. ) ;
#66633 = CARTESIAN_POINT ( 'NONE',  ( 12.91533473730992121, 34.52201867748817676, 10.88017736071110164 ) ) ;
#66636 = CARTESIAN_POINT ( 'NONE',  ( -1.354709868695754826, 14.49999999999999112, 14.93870011653156915 ) ) ;
#66637 = CIRCLE ( 'NONE', #84215, 10.90000000000026326 ) ;
#66638 = CARTESIAN_POINT ( 'NONE',  ( 10.84451454130498149, 15.00000000000000000, 9.625305416630897781 ) ) ;
#66639 = CIRCLE ( 'NONE', #50723, 3.000000000000000000 ) ;
#66640 = CARTESIAN_POINT ( 'NONE',  ( 20.88017736071110875, 20.77201867748816611, -2.915334737309920765 ) ) ;
#66641 = CARTESIAN_POINT ( 'NONE',  ( 20.88017736071110875, 35.77201867748816966, -2.915334737309920765 ) ) ;
#66642 = CARTESIAN_POINT ( 'NONE',  ( 18.52753015748617571, 53.09226448433412315, 4.923371831947298993 ) ) ;
#66643 = CARTESIAN_POINT ( 'NONE',  ( 2.035157376598824452, 53.68868534415484817, 7.964842623401179544 ) ) ;
#66644 = CARTESIAN_POINT ( 'NONE',  ( 10.00000000000000000, 30.55374883491397142, -14.16423886937410082 ) ) ;
#66645 = DIRECTION ( 'NONE',  ( 0.000000000000000000, 1.000000000000000000, 0.000000000000000000 ) ) ;
#66646 = CARTESIAN_POINT ( 'NONE',  ( 5.076628168052703671, 36.84226448433412315, 8.527530157486179263 ) ) ;
#66647 = CARTESIAN_POINT ( 'NONE',  ( -2.816281873526473856, 59.33196800326374643, 3.434112377981055619 ) ) ;
#66648 = CARTESIAN_POINT ( 'NONE',  ( 6.565887622018943937, 3.081968003263753531, -12.81628187352647608 ) ) ;
#66649 = ORIENTED_EDGE ( 'NONE', *, *, #39878, .F. ) ;
#66650 = CARTESIAN_POINT ( 'NONE',  ( 7.084665262690076126, 24.10535201082150181, 10.88017736071109987 ) ) ;
#66651 = CARTESIAN_POINT ( 'NONE',  ( 4.559911319644449179, 7.230352010821504471, -9.422509992056141925 ) ) ;
#66652 = CARTESIAN_POINT ( 'NONE',  ( 17.96484262340118221, 11.18868534415484106, -7.964842623401177768 ) ) ;
#66653 = CARTESIAN_POINT ( 'NONE',  ( 2.791683348922237240, 0.3839311510007847872, -7.208316651077763204 ) ) ;
#66654 = CARTESIAN_POINT ( 'NONE',  ( 2.917880565312950480, 20.97041550158063217, -12.26659068614894821 ) ) ;
#66655 = CARTESIAN_POINT ( 'NONE',  ( 1.472469842513823179, 11.42559781766745175, 4.923371831947296329 ) ) ;
#66656 = PLANE ( 'NONE',  #94748 ) ;
#66657 = CARTESIAN_POINT ( 'NONE',  ( -0.8801773607111009756, 33.06368534415484106, 1.068504757029289695E-15 ) ) ;
#66658 = CARTESIAN_POINT ( 'NONE',  ( 12.80781515976314822, 0.000000000000000000, -6.246788841744324472 ) ) ;
#66659 = CARTESIAN_POINT ( 'NONE',  ( 10.93781366033343083, 14.49999999999999112, 10.26470809774079029 ) ) ;
#66660 = ORIENTED_EDGE ( 'NONE', *, *, #22728, .T. ) ;
#66661 = CARTESIAN_POINT ( 'NONE',  ( 4.864290147400408770, -17.52197929146259270, 2.500000000000000444 ) ) ;
#66662 = CARTESIAN_POINT ( 'NONE',  ( 10.00000000000000178, 47.25893115100078745, 9.846743663894594434 ) ) ;
#66663 = VERTEX_POINT ( 'NONE', #18705 ) ;
#66664 = EDGE_LOOP ( 'NONE', ( #70214, #68949, #30177, #42234 ) ) ;
#66665 = CARTESIAN_POINT ( 'NONE',  ( -14.82679024690668967, 0.2306972965111902529, -1.845086899513486367 ) ) ;
#66666 = CARTESIAN_POINT ( 'NONE',  ( -2.266590686148945544, 21.38708216824730357, -7.082119434687050408 ) ) ;
#66667 = CARTESIAN_POINT ( 'NONE',  ( -0.3689425029237881626, 17.42874883491397142, 10.36894250292379027 ) ) ;
#66668 = CARTESIAN_POINT ( 'NONE',  ( 20.88017736071110519, 65.56368534415483396, 2.639326808657452039E-16 ) ) ;
#66669 = CARTESIAN_POINT ( 'NONE',  ( 17.08211943468705130, 58.47041550158063927, 12.26659068614894998 ) ) ;
#66670 = CARTESIAN_POINT ( 'NONE',  ( -2.816281873526473856, -0.8763653300695799508, 9.499525473075851096E-16 ) ) ;
#66671 = CARTESIAN_POINT ( 'NONE',  ( 5.076628168052704559, 55.17559781766745175, -8.527530157486179263 ) ) ;
#66672 = CARTESIAN_POINT ( 'NONE',  ( -11.01435017095933588, -93.41041245700012041, 4.000000000000000000 ) ) ;
#66674 = CARTESIAN_POINT ( 'NONE',  ( 3.591859063236763294, 3.290301336597087012, -11.09922568453595026 ) ) ;
#66673 = CARTESIAN_POINT ( 'NONE',  ( 20.88017736071110519, 50.56368534415484106, 2.639326808657452039E-16 ) ) ;
#66675 = CARTESIAN_POINT ( 'NONE',  ( 10.00000000000000000, 10.55374883491396787, -14.16423886937410082 ) ) ;
#66676 = CARTESIAN_POINT ( 'NONE',  ( 24.16423886937410614, 54.51208216824730357, -3.795296366450302550 ) ) ;
#66677 = VECTOR ( 'NONE', #67891, 1000.000000000000114 ) ;
#66678 = CARTESIAN_POINT ( 'NONE',  ( 20.88017736071110164, 20.35535201082150891, 2.915334737309930979 ) ) ;
#66679 = DIRECTION ( 'NONE',  ( -1.000000000000000000, 0.000000000000000000, 0.000000000000000000 ) ) ;
#66680 = CARTESIAN_POINT ( 'NONE',  ( 19.42250999205614193, 40.14701867748817676, 5.440088680355555262 ) ) ;
#66681 = CARTESIAN_POINT ( 'NONE',  ( -9.846743663894590881, -18.78273551566588040, 2.638427012816840111 ) ) ;
#66682 = VERTEX_POINT ( 'NONE', #48693 ) ;
#66683 = CARTESIAN_POINT ( 'NONE',  ( -14.29730467489527967, 15.00000000000000000, -2.416004766803415471 ) ) ;
#66684 = ORIENTED_EDGE ( 'NONE', *, *, #66820, .T. ) ;
#66685 = VERTEX_POINT ( 'NONE', #41223 ) ;
#66686 = CARTESIAN_POINT ( 'NONE',  ( 24.16423886937410614, 44.30374883491397497, 8.672049930838204340E-16 ) ) ;
#66687 = CARTESIAN_POINT ( 'NONE',  ( 5.076628168052704559, 45.17559781766745175, -8.527530157486179263 ) ) ;
#66688 = CARTESIAN_POINT ( 'NONE',  ( 17.96484262340118221, 66.18868534415483396, -7.964842623401177768 ) ) ;
#66689 = CARTESIAN_POINT ( 'NONE',  ( 0.000000000000000000, 0.000000000000000000, 0.000000000000000000 ) ) ;
#66690 = AXIS2_PLACEMENT_3D ( 'NONE', #41609, #49089, #27558 ) ;
#66691 = CARTESIAN_POINT ( 'NONE',  ( -0.8801773607110991993, 52.85535201082151247, -2.915334737309923874 ) ) ;
#66692 = CARTESIAN_POINT ( 'NONE',  ( 0.6178305044545838731, 59.74863466993041783, 9.382169495545420901 ) ) ;
#66693 = CARTESIAN_POINT ( 'NONE',  ( -9.382169495545422677, 3.498634669930421826, -9.382169495545417348 ) ) ;
#66694 = VERTEX_POINT ( 'NONE', #64173 ) ;
#66695 = CARTESIAN_POINT ( 'NONE',  ( 20.36894250292379738, 19.92874883491396787, -10.36894250292379027 ) ) ;
#66696 = CARTESIAN_POINT ( 'NONE',  ( 10.00000000000000178, 20.37363466993042138, 12.81628187352647608 ) ) ;
#66697 = ORIENTED_EDGE ( 'NONE', *, *, #81967, .F. ) ;
#66698 = CARTESIAN_POINT ( 'NONE',  ( 16.40814093676324603, 47.45696800326375353, -11.09922568453594671 ) ) ;
#66699 = PRESENTATION_LAYER_ASSIGNMENT (  '', '', ( #65097 ) ) ;
#66700 = CARTESIAN_POINT ( 'NONE',  ( 12.63842701281683034, 32.46726448433412315, 9.846743663894596210 ) ) ;
#66701 = CARTESIAN_POINT ( 'NONE',  ( 17.96484262340118221, 11.18868534415483929, -7.964842623401177768 ) ) ;
#66702 = CARTESIAN_POINT ( 'NONE',  ( -2.816281873526473856, 54.12363466993041783, 9.499525473075851096E-16 ) ) ;
#66703 = CARTESIAN_POINT ( 'NONE',  ( 14.02068044289378967, 15.00000000000000000, -5.331089937175664595 ) ) ;
#66704 = CARTESIAN_POINT ( 'NONE',  ( 0.1532563361054082862, 46.21726448433411605, 2.638427012816831674 ) ) ;
#66705 = VECTOR ( 'NONE', #23850, 1000.000000000000000 ) ;
#66706 = EDGE_CURVE ( 'NONE', #5095, #9889, #4195, .T. ) ;
#66707 = EDGE_CURVE ( 'NONE', #4865, #92052, #87885, .T. ) ;
#66708 = VECTOR ( 'NONE', #91713, 1000.000000000000000 ) ;
#66709 = TOROIDAL_SURFACE ( 'NONE', #49147, 18.53834841531100608, 7.000000000000000000 ) ;
#66710 = CARTESIAN_POINT ( 'NONE',  ( 10.04796213703172647, 2.879912020664621153E-16, 10.62905469192473440 ) ) ;
#66711 = CARTESIAN_POINT ( 'NONE',  ( -46.34323875807881166, 103.6109741468810483, -6.190393423093146552 ) ) ;
#66712 = CARTESIAN_POINT ( 'NONE',  ( 20.15039907845753220, 45.60158574516643881, -6.262539305110077947 ) ) ;
#66713 = DIRECTION ( 'NONE',  ( -0.000000000000000000, -1.000000000000000000, -0.000000000000000000 ) ) ;
#66714 = DIRECTION ( 'NONE',  ( -5.818595309480553908E-17, -1.000000000000000000, -0.000000000000000000 ) ) ;
#66715 = CARTESIAN_POINT ( 'NONE',  ( 14.92337183194729988, 14.34226448433411782, -8.527530157486177487 ) ) ;
#66716 = CARTESIAN_POINT ( 'NONE',  ( 13.43411237798106583, 27.66530133659708568, -12.81628187352647252 ) ) ;
#66717 = CARTESIAN_POINT ( 'NONE',  ( -0.9940297508538862292, 15.00000000000000000, 14.21528771620248932 ) ) ;
#66718 = ORIENTED_EDGE ( 'NONE', *, *, #98591, .T. ) ;
#66719 = CARTESIAN_POINT ( 'NONE',  ( 14.92337183194729633, 62.67559781766745886, 8.527530157486181039 ) ) ;
#66720 = CARTESIAN_POINT ( 'NONE',  ( -9.876730923139385609, 0.3640475087720987935, 11.28938378619056948 ) ) ;
#66721 = ADVANCED_FACE ( 'NONE', ( #33195 ), #63688, .F. ) ;
#66722 = CARTESIAN_POINT ( 'NONE',  ( 22.26659068614895176, 14.72041550158063572, -7.082119434687042414 ) ) ;
#66723 = CARTESIAN_POINT ( 'NONE',  ( 12.63842701281683034, 42.46726448433412315, 9.846743663894596210 ) ) ;
#66724 = CARTESIAN_POINT ( 'NONE',  ( 3.591859063236761518, 49.95696800326375353, 11.09922568453594849 ) ) ;
#66725 = DIRECTION ( 'NONE',  ( -0.000000000000000000, 1.000000000000000000, 0.000000000000000000 ) ) ;
#66726 = CARTESIAN_POINT ( 'NONE',  ( 1.472469842513823179, 10.59226448433411782, -4.923371831947296329 ) ) ;
#66727 = FACE_BOUND ( 'NONE', #44353, .T. ) ;
#66728 = CARTESIAN_POINT ( 'NONE',  ( 10.00000000000000178, 52.25893115100078745, 9.846743663894594434 ) ) ;
#66729 = CARTESIAN_POINT ( 'NONE',  ( 12.91533473730992121, 44.52201867748816966, 10.88017736071110164 ) ) ;
#66730 = CARTESIAN_POINT ( 'NONE',  ( 7.361572987183169658, 29.96726448433411960, -9.846743663894592657 ) ) ;
#66731 = DIRECTION ( 'NONE',  ( -1.000000000000000000, 0.000000000000000000, 0.000000000000000000 ) ) ;
#66732 = ADVANCED_FACE ( 'NONE', ( #94695 ), #72179, .T. ) ;
#66733 = CARTESIAN_POINT ( 'NONE',  ( 10.00000000000000000, 46.81368534415484106, -10.88017736071110342 ) ) ;
#66734 = VERTEX_POINT ( 'NONE', #64659 ) ;
#66735 = DIRECTION ( 'NONE',  ( -0.000000000000000000, -0.000000000000000000, 1.000000000000000000 ) ) ;
#66736 = CARTESIAN_POINT ( 'NONE',  ( 10.00000000000000178, 19.31368534415484106, 10.88017736071110342 ) ) ;
#66738 = CARTESIAN_POINT ( 'NONE',  ( 7.084665262690076126, 47.02201867748818387, -10.88017736071110164 ) ) ;
#66737 = CARTESIAN_POINT ( 'NONE',  ( 2.791683348922240793, 51.63393115100078745, 7.208316651077764092 ) ) ;
#66739 = CARTESIAN_POINT ( 'NONE',  ( 0.000000000000000000, 14.49999999999999822, 0.000000000000000000 ) ) ;
#66740 = CARTESIAN_POINT ( 'NONE',  ( 0.5774900079438607392, 53.48035201082151247, 5.440088680355550821 ) ) ;
#66742 = FACE_OUTER_BOUND ( 'NONE', #36552, .T. ) ;
#66741 = CARTESIAN_POINT ( 'NONE',  ( 20.88017736071110875, 20.77201867748816611, -2.915334737309920765 ) ) ;
#66743 = CARTESIAN_POINT ( 'NONE',  ( 19.72487221294571569, 49.78217586085237656, 6.499999999999993783 ) ) ;
#66744 = CARTESIAN_POINT ( 'NONE',  ( 0.1532563361054082862, 21.21726448433412315, 2.638427012816831674 ) ) ;
#66745 =( LENGTH_UNIT ( ) NAMED_UNIT ( * ) SI_UNIT ( .MILLI., .METRE. ) );
#66746 = CARTESIAN_POINT ( 'NONE',  ( -14.16423886937409726, 12.01208216824730357, 3.795296366450320757 ) ) ;
#66747 = CARTESIAN_POINT ( 'NONE',  ( 0.1532563361054082862, 56.21726448433411605, 2.638427012816831674 ) ) ;
#66748 = CARTESIAN_POINT ( 'NONE',  ( 6.204703633549690345, 65.76208216824731778, -14.16423886937410259 ) ) ;
#66749 = CARTESIAN_POINT ( 'NONE',  ( 12.83294900548058415, 0.3640475087720986269, 7.766300266068457248 ) ) ;
#66750 = CARTESIAN_POINT ( 'NONE',  ( 20.36894250292379382, 8.678748834913967869, 10.36894250292379205 ) ) ;
#66751 = CARTESIAN_POINT ( 'NONE',  ( -4.164238869374099039, 51.80374883491396787, 8.674139862899312516E-16 ) ) ;
#66752 = VECTOR ( 'NONE', #20447, 1000.000000000000000 ) ;
#66753 = CARTESIAN_POINT ( 'NONE',  ( 22.81628187352647785, 1.623634669930420271, 6.195893100308588602E-16 ) ) ;
#66754 = ORIENTED_EDGE ( 'NONE', *, *, #1051, .F. ) ;
#66755 = CARTESIAN_POINT ( 'NONE',  ( 15.44008868035555793, 16.39701867748817321, -9.422509992056140149 ) ) ;
#66756 = CARTESIAN_POINT ( 'NONE',  ( 10.00000000000000000, 54.75893115100078745, -9.846743663894594434 ) ) ;
#66758 = DIRECTION ( 'NONE',  ( 0.000000000000000000, 0.000000000000000000, 1.000000000000000000 ) ) ;
#66757 = DIRECTION ( 'NONE',  ( 1.000000000000000000, 0.000000000000000000, 0.000000000000000000 ) ) ;
#66759 = CARTESIAN_POINT ( 'NONE',  ( 3.193136578976985440, 15.00000000000000888, 14.27383009353652987 ) ) ;
#66760 = CARTESIAN_POINT ( 'NONE',  ( 9.898881779040729967, 15.00000000000000000, -10.25059215482576214 ) ) ;
#66761 = CARTESIAN_POINT ( 'NONE',  ( -2.816281873526473856, 19.33196800326375708, 3.434112377981055619 ) ) ;
#66762 = CARTESIAN_POINT ( 'NONE',  ( 7.361572987183169658, 29.96726448433411960, -9.846743663894592657 ) ) ;
#66763 = ORIENTED_EDGE ( 'NONE', *, *, #22160, .F. ) ;
#66764 = CARTESIAN_POINT ( 'NONE',  ( 7.361572987183169658, 4.967264484334119601, -9.846743663894592657 ) ) ;
#66765 = FILL_AREA_STYLE ('',( #34780 ) ) ;
#66766 = CARTESIAN_POINT ( 'NONE',  ( 0.000000000000000000, 14.49999999999999822, 0.000000000000000000 ) ) ;
#66767 = CARTESIAN_POINT ( 'NONE',  ( 2.035157376598822676, 17.43868534415483751, -7.964842623401177768 ) ) ;
#66768 = CARTESIAN_POINT ( 'NONE',  ( -0.3689425029237881626, 37.42874883491396787, 10.36894250292379027 ) ) ;
#66769 = CARTESIAN_POINT ( 'NONE',  ( 20.88017736071110875, 40.77201867748818387, -2.915334737309920765 ) ) ;
#66770 = CARTESIAN_POINT ( 'NONE',  ( 20.88017736071110164, 65.35535201082150536, 2.915334737309930979 ) ) ;
#66771 = EDGE_CURVE ( 'NONE', #70993, #64180, #71218, .T. ) ;
#66772 = DIRECTION ( 'NONE',  ( 0.000000000000000000, 0.000000000000000000, 1.000000000000000000 ) ) ;
#66773 = CARTESIAN_POINT ( 'NONE',  ( 7.361572987183170547, 27.05059781766745175, 9.846743663894590881 ) ) ;
#66774 = SURFACE_SIDE_STYLE ('',( #49791 ) ) ;
#66775 = CARTESIAN_POINT ( 'NONE',  ( 0.1532563361054082862, 1.217264484334117824, 2.638427012816831674 ) ) ;
#66776 = LINE ( 'NONE', #89280, #14471 ) ;
#66777 = CARTESIAN_POINT ( 'NONE',  ( 2.791683348922237240, 35.38393115100079456, -7.208316651077763204 ) ) ;
#66778 = CARTESIAN_POINT ( 'NONE',  ( 0.1532563361054100626, 60.80059781766744464, -2.638427012816831230 ) ) ;
#66779 = ADVANCED_FACE ( 'NONE', ( #26679 ), #27662, .T. ) ;
#66780 = CARTESIAN_POINT ( 'NONE',  ( 12.91533473730993009, 41.60535201082149825, -10.88017736071109987 ) ) ;
#66781 = STYLED_ITEM ( 'NONE', ( #93570 ), #58821 ) ;
#66782 = VECTOR ( 'NONE', #82045, 1000.000000000000000 ) ;
#66783 = ORIENTED_EDGE ( 'NONE', *, *, #84928, .F. ) ;
#66784 = CARTESIAN_POINT ( 'NONE',  ( 16.40814093676323893, 60.79030133659709634, 11.09922568453595026 ) ) ;
#66785 = CARTESIAN_POINT ( 'NONE',  ( 4.219999999999999751, 37.00000000000000000, -3.750000000000000000 ) ) ;
#66786 = CARTESIAN_POINT ( 'NONE',  ( 5.076628168052703671, 11.84226448433411960, 8.527530157486179263 ) ) ;
#66787 = CARTESIAN_POINT ( 'NONE',  ( 19.38216949554541557, 47.24863466993041783, -9.382169495545420901 ) ) ;
#66789 = CARTESIAN_POINT ( 'NONE',  ( 5.076628168052704559, 30.17559781766745175, -8.527530157486179263 ) ) ;
#66788 = CARTESIAN_POINT ( 'NONE',  ( 10.00000000000000000, 11.81368534415483751, -10.88017736071110342 ) ) ;
#66790 = CARTESIAN_POINT ( 'NONE',  ( 15.00000000000000000, 77.07179676972447169, 6.250000000000000000 ) ) ;
#66791 = CARTESIAN_POINT ( 'NONE',  ( 17.08211943468705840, 45.13708216824730357, -12.26659068614894466 ) ) ;
#66792 = CARTESIAN_POINT ( 'NONE',  ( 17.20831665107776587, 39.13393115100079456, -7.208316651077762316 ) ) ;
#66793 = CARTESIAN_POINT ( 'NONE',  ( 6.579634127946608402, -87.99828267815712479, -2.500000000000000000 ) ) ;
#66794 = CARTESIAN_POINT ( 'NONE',  ( 20.88017736071110519, 35.56368534415484106, 2.639326808657452039E-16 ) ) ;
#66795 = CARTESIAN_POINT ( 'NONE',  ( 17.20831665107776587, 4.133931151000785675, -7.208316651077762316 ) ) ;
#66796 = CARTESIAN_POINT ( 'NONE',  ( 1.472469842513823179, 55.59226448433412315, -4.923371831947296329 ) ) ;
#66797 = ORIENTED_EDGE ( 'NONE', *, *, #71039, .F. ) ;
#66798 = CARTESIAN_POINT ( 'NONE',  ( 10.00000000000000178, 55.37363466993042493, 12.81628187352647608 ) ) ;
#66799 = EDGE_LOOP ( 'NONE', ( #33348, #9465, #1311, #21726 ) ) ;
#66800 = CARTESIAN_POINT ( 'NONE',  ( 19.42250999205614193, 60.14701867748817676, 5.440088680355555262 ) ) ;
#66801 = ORIENTED_EDGE ( 'NONE', *, *, #97677, .F. ) ;
#66802 = CARTESIAN_POINT ( 'NONE',  ( 17.08211943468705130, 3.470415501580634388, 12.26659068614894998 ) ) ;
#66803 = CARTESIAN_POINT ( 'NONE',  ( 0.1532563361054082862, 1.217264484334117824, 2.638427012816831674 ) ) ;
#66804 = CARTESIAN_POINT ( 'NONE',  ( -0.2418659066527711621, 59.26028685723174760, -6.114288769123046308 ) ) ;
#66805 = ORIENTED_EDGE ( 'NONE', *, *, #35235, .F. ) ;
#66806 = CARTESIAN_POINT ( 'NONE',  ( 20.88017736071110519, 15.56368534415483751, 2.639326808657452039E-16 ) ) ;
#66807 = CARTESIAN_POINT ( 'NONE',  ( -5.376821459230213485, 14.76984886575651501, 13.93958558162633921 ) ) ;
#66808 = EDGE_LOOP ( 'NONE', ( #19725, #56732, #29646, #12483, #72332, #63008, #20365, #4114 ) ) ;
#66809 = CARTESIAN_POINT ( 'NONE',  ( 2.035157376598824452, 23.68868534415484461, 7.964842623401179544 ) ) ;
#66810 = CARTESIAN_POINT ( 'NONE',  ( 10.00000000000000000, 64.75893115100078035, -9.846743663894594434 ) ) ;
#66811 = ORIENTED_EDGE ( 'NONE', *, *, #54184, .F. ) ;
#66812 = CARTESIAN_POINT ( 'NONE',  ( 0.1532563361054083140, 66.00893115100079456, 1.131784320476157264E-15 ) ) ;
#66813 = ORIENTED_EDGE ( 'NONE', *, *, #30362, .F. ) ;
#66814 = CARTESIAN_POINT ( 'NONE',  ( 7.361572987183170547, 2.050597817667451750, 9.846743663894590881 ) ) ;
#66815 = CARTESIAN_POINT ( 'NONE',  ( 0.1532563361054100626, 65.80059781766745175, -2.638427012816831230 ) ) ;
#66816 = CARTESIAN_POINT ( 'NONE',  ( 10.00000000000000178, 40.37363466993042493, 12.81628187352647608 ) ) ;
#66817 = CARTESIAN_POINT ( 'NONE',  ( -0.8801773607111009756, 23.06368534415484106, 1.068504757029289695E-15 ) ) ;
#66818 = CARTESIAN_POINT ( 'NONE',  ( 7.361572987183169658, 4.967264484334119601, -9.846743663894592657 ) ) ;
#66819 = CARTESIAN_POINT ( 'NONE',  ( 19.42250999205614193, 25.14701867748817321, 5.440088680355555262 ) ) ;
#66820 = EDGE_CURVE ( 'NONE', #92829, #10063, #75062, .T. ) ;
#66821 = AXIS2_PLACEMENT_3D ( 'NONE', #35930, #90397, #65931 ) ;
#66822 = EDGE_LOOP ( 'NONE', ( #60904, #77744, #60135, #92640, #98015, #30542 ) ) ;
#66823 = CARTESIAN_POINT ( 'NONE',  ( 22.81628187352647785, 56.41530133659708213, 3.434112377981063169 ) ) ;
#66824 = CARTESIAN_POINT ( 'NONE',  ( -0.8801773607111009756, 48.06368534415484817, 1.068504757029289695E-15 ) ) ;
#66825 = DIRECTION ( 'NONE',  ( 0.000000000000000000, 0.000000000000000000, 1.000000000000000000 ) ) ;
#66826 = CARTESIAN_POINT ( 'NONE',  ( 22.81628187352647785, 51.41530133659708923, 3.434112377981063169 ) ) ;
#66827 = CARTESIAN_POINT ( 'NONE',  ( 2.035157376598824452, 48.68868534415483396, 7.964842623401179544 ) ) ;
#66828 = CARTESIAN_POINT ( 'NONE',  ( 0.1532563361054082862, 56.21726448433411605, 2.638427012816831674 ) ) ;
#66829 = CARTESIAN_POINT ( 'NONE',  ( -7.684764310694971456, 14.49999999999999822, 12.88194075009929840 ) ) ;
#66830 = PRESENTATION_LAYER_ASSIGNMENT (  '', '', ( #44496 ) ) ;
#66831 = CARTESIAN_POINT ( 'NONE',  ( 19.84674366389459266, 13.71726448433411782, -2.638427012816827677 ) ) ;
#66832 = CARTESIAN_POINT ( 'NONE',  ( 16.40814093676323893, 5.790301336597087456, 11.09922568453595026 ) ) ;
#66834 = CARTESIAN_POINT ( 'NONE',  ( -4.250000000000000000, 78.07179676972445748, -6.500000000000000888 ) ) ;
#66833 = CARTESIAN_POINT ( 'NONE',  ( 0.000000000000000000, 14.49999999999999822, 0.000000000000000000 ) ) ;
#66835 = CARTESIAN_POINT ( 'NONE',  ( 12.91533473730992121, 19.52201867748816611, 10.88017736071110164 ) ) ;
#66836 = CARTESIAN_POINT ( 'NONE',  ( 10.00000000000000000, 49.75893115100078745, -9.846743663894594434 ) ) ;
#66837 = SURFACE_SIDE_STYLE ('',( #4874 ) ) ;
#66839 = CARTESIAN_POINT ( 'NONE',  ( 2.791683348922237240, 5.383931151000785675, -7.208316651077763204 ) ) ;
#66838 = COLOUR_RGB ( '', 0.09019608, 0.27058824, 0.51372549) ;
#66840 = DIRECTION ( 'NONE',  ( -0.000000000000000000, -1.000000000000000000, -0.000000000000000000 ) ) ;
#66842 = ORIENTED_EDGE ( 'NONE', *, *, #9045, .T. ) ;
#66841 = CARTESIAN_POINT ( 'NONE',  ( 10.00000000000000000, 7.873634669930421381, -12.81628187352647608 ) ) ;
#66843 = VECTOR ( 'NONE', #73706, 1000.000000000000000 ) ;
#66844 = DIRECTION ( 'NONE',  ( 0.000000000000000000, -0.000000000000000000, -1.000000000000000000 ) ) ;
#66845 = CARTESIAN_POINT ( 'NONE',  ( -1.099225684535947600, 44.54030133659708923, 6.408140936763237150 ) ) ;
#66846 = EDGE_CURVE ( 'NONE', #38139, #92170, #42196, .T. ) ;
#66847 = CARTESIAN_POINT ( 'NONE',  ( 19.84674366389459621, 33.50893115100078745, 7.409399052514197653E-17 ) ) ;
#66848 = B_SPLINE_CURVE_WITH_KNOTS ( 'NONE', 3,
 ( #68398, #53376, #25247, #24740 ),
 .UNSPECIFIED., .F., .F.,
 ( 4, 4 ),
 ( 5.284504157781969479E-17, 0.002562518741975526333 ),
 .UNSPECIFIED. ) ;
#66849 = CARTESIAN_POINT ( 'NONE',  ( -0.8801773607111009756, 58.06368534415484106, 1.068504757029289695E-15 ) ) ;
#66850 = CARTESIAN_POINT ( 'NONE',  ( 10.00000000000000178, 4.313685344154837509, 10.88017736071110342 ) ) ;
#66851 = CARTESIAN_POINT ( 'NONE',  ( 18.52753015748618282, 33.92559781766745886, -4.923371831947291888 ) ) ;
#66852 = CARTESIAN_POINT ( 'NONE',  ( 7.551349515323185990, 15.00000000000000000, -12.08468537022906020 ) ) ;
#66853 = EDGE_CURVE ( 'NONE', #24454, #93321, #87184, .T. ) ;
#66854 = CARTESIAN_POINT ( 'NONE',  ( 2.917880565312950480, 65.97041550158063217, -12.26659068614894821 ) ) ;
#66855 = DIRECTION ( 'NONE',  ( 0.7971177707001174673, 0.6038238647437470519, -0.000000000000000000 ) ) ;
#66856 = CARTESIAN_POINT ( 'NONE',  ( 19.42250999205614548, 20.98035201082150891, -5.440088680355545492 ) ) ;
#66857 = CARTESIAN_POINT ( 'NONE',  ( 10.00000000000000178, 48.05374883491396787, 14.16423886937410082 ) ) ;
#66858 = CARTESIAN_POINT ( 'NONE',  ( 17.08211943468705130, 53.47041550158063217, 12.26659068614894998 ) ) ;
#66859 = CARTESIAN_POINT ( 'NONE',  ( -0.1503990784575328643, 69.92552686551195507, 6.262539305110068177 ) ) ;
#66860 = VECTOR ( 'NONE', #21213, 1000.000000000000000 ) ;
#66861 = CARTESIAN_POINT ( 'NONE',  ( 17.20831665107776587, 7.883931151000784787, 7.208316651077764980 ) ) ;
#66862 = CARTESIAN_POINT ( 'NONE',  ( 22.81628187352647785, 1.623634669930420271, 6.195893100308588602E-16 ) ) ;
#66863 = ORIENTED_EDGE ( 'NONE', *, *, #7382, .F. ) ;
#66864 = CARTESIAN_POINT ( 'NONE',  ( 10.00000000000000178, 49.31368534415484106, 10.88017736071110342 ) ) ;
#66865 = LINE ( 'NONE', #34881, #27340 ) ;
#66866 = CARTESIAN_POINT ( 'NONE',  ( 2.791683348922240793, 56.63393115100078035, 7.208316651077764092 ) ) ;
#66867 = CARTESIAN_POINT ( 'NONE',  ( 18.72515096720590577, 61.07228050351029935, -6.499999999999718447 ) ) ;
#66868 = LINE ( 'NONE', #58869, #86631 ) ;
#66870 = CARTESIAN_POINT ( 'NONE',  ( 22.26659068614894466, 3.887082168247300906, 7.082119434687054849 ) ) ;
#66869 =( BOUNDED_CURVE ( )  B_SPLINE_CURVE ( 2, ( #9499, #65304, #42825, #85503, #77994, #1537, #87813, #62984, #62487 ),
 .UNSPECIFIED., .F., .F. ) 
 B_SPLINE_CURVE_WITH_KNOTS ( ( 3, 2, 2, 2, 3 ),
 ( 0.9025141644748393421, 0.9047619047619047672, 0.9107142857142856984, 0.9166666666666666297, 0.9189144069537320547 ),
 .UNSPECIFIED. ) 
 CURVE ( )  GEOMETRIC_REPRESENTATION_ITEM ( )  RATIONAL_B_SPLINE_CURVE ( ( 0.9839835555609424134, 0.9871328979762474809, 1.000000000000000000, 0.9659258262890683122, 1.000000000000000000, 0.9659258262890683122, 1.000000000000000000, 0.9871328979762477029, 0.9839835555609425244 ) ) 
 REPRESENTATION_ITEM ( '' )  );
#66871 = CARTESIAN_POINT ( 'NONE',  ( 1.472469842513823179, 25.59226448433412315, -4.923371831947296329 ) ) ;
#66872 = DIRECTION ( 'NONE',  ( 1.000000000000000000, 0.000000000000000000, 0.000000000000000000 ) ) ;
#66873 = ORIENTED_EDGE ( 'NONE', *, *, #56818, .F. ) ;
#66874 = CARTESIAN_POINT ( 'NONE',  ( 17.08211943468705130, 38.47041550158063217, 12.26659068614894998 ) ) ;
#66875 = CARTESIAN_POINT ( 'NONE',  ( 2.791683348922237240, 10.38393115100078390, -7.208316651077763204 ) ) ;
#66877 = CARTESIAN_POINT ( 'NONE',  ( -8.235571585149864760, 8.546802177851539284, 8.235571585149875418 ) ) ;
#66876 = DIRECTION ( 'NONE',  ( 0.000000000000000000, 0.000000000000000000, 1.000000000000000000 ) ) ;
#66878 = CARTESIAN_POINT ( 'NONE',  ( 17.96484262340118221, 31.18868534415483751, -7.964842623401177768 ) ) ;
#66879 = CARTESIAN_POINT ( 'NONE',  ( 6.565887622018943937, 33.08196800326374643, -12.81628187352647608 ) ) ;
#66880 = CARTESIAN_POINT ( 'NONE',  ( 20.88017736071110519, 5.563685344154837509, 2.639326808657452039E-16 ) ) ;
#66881 = CARTESIAN_POINT ( 'NONE',  ( 6.565887622018943937, 40.16530133659708923, 12.81628187352647430 ) ) ;
#66882 = CARTESIAN_POINT ( 'NONE',  ( 19.38216949554541202, 60.99863466993042493, 9.382169495545424454 ) ) ;
#66883 = ORIENTED_EDGE ( 'NONE', *, *, #93766, .F. ) ;
#66884 = LINE ( 'NONE', #58885, #29293 ) ;
#66885 = DIRECTION ( 'NONE',  ( 0.000000000000000000, 1.000000000000000000, 0.000000000000000000 ) ) ;
#66886 = CARTESIAN_POINT ( 'NONE',  ( 24.16423886937410614, 39.30374883491396787, 8.672049930838204340E-16 ) ) ;
#66887 = CARTESIAN_POINT ( 'NONE',  ( 10.00000000000000000, 5.553748834913967869, -14.16423886937410082 ) ) ;
#66888 = CARTESIAN_POINT ( 'NONE',  ( 4.559911319644449179, 23.89701867748817321, 9.422509992056141925 ) ) ;
#66889 = DIRECTION ( 'NONE',  ( 0.5547001962252290364, 0.8320502943378437211, 0.000000000000000000 ) ) ;
#66890 = CARTESIAN_POINT ( 'NONE',  ( 0.7375392941517235901, 15.00000000000000000, 14.98185688723471110 ) ) ;
#66891 = CARTESIAN_POINT ( 'NONE',  ( 0.5774900079438607392, 48.48035201082150536, 5.440088680355550821 ) ) ;
#66892 = CARTESIAN_POINT ( 'NONE',  ( 19.42250999205614548, 55.98035201082150536, -5.440088680355545492 ) ) ;
#66893 = CARTESIAN_POINT ( 'NONE',  ( -2.816281873526471635, 18.91530133659708213, -3.434112377981056508 ) ) ;
#66894 = DIRECTION ( 'NONE',  ( -0.000000000000000000, -1.000000000000000000, -0.000000000000000000 ) ) ;
#66895 = CARTESIAN_POINT ( 'NONE',  ( 0.2751277870542909176, 30.30223176428831167, 6.499999999999992006 ) ) ;
#66896 = CARTESIAN_POINT ( 'NONE',  ( 0.1532563361054100626, 25.80059781766744820, -2.638427012816831230 ) ) ;
#66897 = CARTESIAN_POINT ( 'NONE',  ( 4.559911319644449179, 58.89701867748817676, 9.422509992056141925 ) ) ;
#66898 = EDGE_CURVE ( 'NONE', #13755, #46052, #25721, .T. ) ;
#66899 = CARTESIAN_POINT ( 'NONE',  ( 19.38216949554541557, 22.24863466993041428, -9.382169495545420901 ) ) ;
#66900 = CARTESIAN_POINT ( 'NONE',  ( 10.14667048435138064, 4.748928130477084912E-16, 10.35833375027048042 ) ) ;
#66901 = CARTESIAN_POINT ( 'NONE',  ( 17.96484262340118221, 9.938685344154837509, 7.964842623401181321 ) ) ;
#66902 = CARTESIAN_POINT ( 'NONE',  ( 17.20831665107776587, 32.88393115100078745, 7.208316651077764980 ) ) ;
#66903 = CARTESIAN_POINT ( 'NONE',  ( 3.591859063236763294, 43.29030133659708923, -11.09922568453595026 ) ) ;
#66904 = CARTESIAN_POINT ( 'NONE',  ( 10.00000000000000178, 22.25893115100078745, 9.846743663894594434 ) ) ;
#66905 = CARTESIAN_POINT ( 'NONE',  ( 10.00000000000000000, 5.553748834913967869, -14.16423886937410082 ) ) ;
#66906 = CYLINDRICAL_SURFACE ( 'NONE', #39822, 0.5000000000000004441 ) ;
#66907 = CARTESIAN_POINT ( 'NONE',  ( 2.035157376598822676, 22.43868534415483396, -7.964842623401177768 ) ) ;
#66908 = DIRECTION ( 'NONE',  ( 0.000000000000000000, 0.000000000000000000, -1.000000000000000000 ) ) ;
#66909 = CARTESIAN_POINT ( 'NONE',  ( 7.361572987183170547, 42.05059781766745886, 9.846743663894590881 ) ) ;
#66910 = CIRCLE ( 'NONE', #42993, 0.2500000000000002220 ) ;
#66911 = CARTESIAN_POINT ( 'NONE',  ( 2.035157376598822676, 17.43868534415483751, -7.964842623401177768 ) ) ;
#66912 = CARTESIAN_POINT ( 'NONE',  ( 7.084665262690076126, 17.02201867748817676, -10.88017736071110164 ) ) ;
#66913 = VERTEX_POINT ( 'NONE', #56213 ) ;
#66914 = CARTESIAN_POINT ( 'NONE',  ( -0.8801773607111008646, 28.27201867748817321, 2.915334737309923430 ) ) ;
#66916 = CARTESIAN_POINT ( 'NONE',  ( 22.81628187352647785, 46.62363466993041783, 6.195893100308588602E-16 ) ) ;
#66915 = COLOUR_RGB ( '', 0.40784314, 0.44705882, 0.49803922) ;
#66917 = CARTESIAN_POINT ( 'NONE',  ( -0.8801773607111009756, 28.06368534415484106, 1.068504757029289695E-15 ) ) ;
#66919 = CARTESIAN_POINT ( 'NONE',  ( 4.559911319644449179, 33.89701867748817676, 9.422509992056141925 ) ) ;
#66918 = DIRECTION ( 'NONE',  ( -0.9862856015372308827, 0.000000000000000000, -0.1650476058606810681 ) ) ;
#66920 = ORIENTED_EDGE ( 'NONE', *, *, #11527, .T. ) ;
#66921 = CARTESIAN_POINT ( 'NONE',  ( 7.361572987183170547, 52.05059781766745175, 9.846743663894590881 ) ) ;
#66922 = CARTESIAN_POINT ( 'NONE',  ( 20.88017736071110519, 30.56368534415484106, 2.639326808657452039E-16 ) ) ;
#66923 = CARTESIAN_POINT ( 'NONE',  ( 4.380000000000000782, 0.08775168532224617013, 3.750000000000000000 ) ) ;
#66924 =( NAMED_UNIT ( * ) PLANE_ANGLE_UNIT ( ) SI_UNIT ( $, .RADIAN. ) );
#66925 =( LENGTH_UNIT ( ) NAMED_UNIT ( * ) SI_UNIT ( .MILLI., .METRE. ) );
#66926 = DIRECTION ( 'NONE',  ( 0.000000000000000000, 0.000000000000000000, -1.000000000000000000 ) ) ;
#66927 = CARTESIAN_POINT ( 'NONE',  ( 2.917880565312948704, 52.63708216824730357, 12.26659068614894643 ) ) ;
#66928 = CARTESIAN_POINT ( 'NONE',  ( 0.5774900079438607392, 53.48035201082151247, 5.440088680355550821 ) ) ;
#66929 = CARTESIAN_POINT ( 'NONE',  ( 2.791683348922240793, 66.63393115100079456, 7.208316651077764092 ) ) ;
#66930 = LINE ( 'NONE', #29408, #58844 ) ;
#66931 = CARTESIAN_POINT ( 'NONE',  ( 18.52753015748618282, 63.92559781766745886, -4.923371831947291888 ) ) ;
#66932 = CARTESIAN_POINT ( 'NONE',  ( 18.52753015748617571, 3.092264484334118269, 4.923371831947298993 ) ) ;
#66933 = CARTESIAN_POINT ( 'NONE',  ( 10.00000000000000178, 17.25893115100078745, 9.846743663894594434 ) ) ;
#66934 = EDGE_LOOP ( 'NONE', ( #43258, #63694, #11573, #19485 ) ) ;
#66935 = CARTESIAN_POINT ( 'NONE',  ( 19.84674366389459621, 23.50893115100078390, 7.409399052514197653E-17 ) ) ;
#66936 = CARTESIAN_POINT ( 'NONE',  ( 12.81628187352647608, -18.58469866340291077, 3.434112377981052511 ) ) ;
#66937 = CARTESIAN_POINT ( 'NONE',  ( 19.42250999205614193, 30.14701867748817321, 5.440088680355555262 ) ) ;
#66938 = CARTESIAN_POINT ( 'NONE',  ( 0.1532563361054083140, 26.00893115100078745, 1.131784320476157264E-15 ) ) ;
#66939 = CARTESIAN_POINT ( 'NONE',  ( 16.40814093676324603, 7.456968003263754419, -11.09922568453594671 ) ) ;
#66941 = CARTESIAN_POINT ( 'NONE',  ( 15.44008868035555793, 61.39701867748817676, -9.422509992056140149 ) ) ;
#66940 = CARTESIAN_POINT ( 'NONE',  ( 19.42250999205614548, 60.98035201082151247, -5.440088680355545492 ) ) ;
#66943 = CARTESIAN_POINT ( 'NONE',  ( 21.09922568453594849, 61.20696800326376064, 6.408140936763242479 ) ) ;
#66942 = CARTESIAN_POINT ( 'NONE',  ( 7.084665262690076126, 27.02201867748817676, -10.88017736071110164 ) ) ;
#66944 = CARTESIAN_POINT ( 'NONE',  ( 6.204703633549690345, 50.76208216824730357, -14.16423886937410259 ) ) ;
#66945 =( GEOMETRIC_REPRESENTATION_CONTEXT ( 3 ) GLOBAL_UNCERTAINTY_ASSIGNED_CONTEXT ( ( #94180 ) ) GLOBAL_UNIT_ASSIGNED_CONTEXT ( ( #15588, #29564, #78039 ) ) REPRESENTATION_CONTEXT ( 'NONE', 'WORKASPACE' ) );
#66946 = EDGE_CURVE ( 'NONE', #65284, #25080, #72660, .T. ) ;
#66947 = EDGE_CURVE ( 'NONE', #14724, #10425, #34665, .T. ) ;
#66948 = CARTESIAN_POINT ( 'NONE',  ( 20.15039907845753220, 42.62777174578613426, -6.262539305110077947 ) ) ;
#66949 = EDGE_CURVE ( 'NONE', #16898, #44301, #50166, .T. ) ;
#66950 = ORIENTED_EDGE ( 'NONE', *, *, #81754, .T. ) ;
#66951 = CARTESIAN_POINT ( 'NONE',  ( 6.565887622018943937, 5.165301336597086568, 12.81628187352647430 ) ) ;
#66952 = CARTESIAN_POINT ( 'NONE',  ( 0.5774900079438607392, 3.480352010821504027, 5.440088680355550821 ) ) ;
#66953 = CARTESIAN_POINT ( 'NONE',  ( 20.88017736071110519, 45.56368534415484106, 2.639326808657452039E-16 ) ) ;
#66954 = CARTESIAN_POINT ( 'NONE',  ( 2.917880565312950480, 0.9704155015806342766, -12.26659068614894821 ) ) ;
#66955 = ORIENTED_EDGE ( 'NONE', *, *, #95849, .T. ) ;
#66956 = CARTESIAN_POINT ( 'NONE',  ( 18.52753015748618282, 18.92559781766745175, -4.923371831947291888 ) ) ;
#66957 = VECTOR ( 'NONE', #23641, 1000.000000000000000 ) ;
#66958 = CARTESIAN_POINT ( 'NONE',  ( 19.42250999205614193, 60.14701867748817676, 5.440088680355555262 ) ) ;
#66959 = CARTESIAN_POINT ( 'NONE',  ( 14.92337183194729988, 34.34226448433411605, -8.527530157486177487 ) ) ;
#66960 = CARTESIAN_POINT ( 'NONE',  ( 18.52753015748617571, 28.09226448433411960, 4.923371831947298993 ) ) ;
#66961 = CARTESIAN_POINT ( 'NONE',  ( 7.361572987183170547, 17.05059781766745530, 9.846743663894590881 ) ) ;
#66962 = CARTESIAN_POINT ( 'NONE',  ( -6.787853370348936544, -86.25412202734867151, 2.500000000000000888 ) ) ;
#66964 = CARTESIAN_POINT ( 'NONE',  ( 6.689969769698956625, -0.03417435944610275333, -12.58200319823970226 ) ) ;
#66963 = CARTESIAN_POINT ( 'NONE',  ( 12.63842701281683922, 4.550597817667451750, -9.846743663894590881 ) ) ;
#66965 = CARTESIAN_POINT ( 'NONE',  ( 10.68821231714948539, -97.11200166802359490, 4.000000000000000000 ) ) ;
#66967 = ORIENTED_EDGE ( 'NONE', *, *, #73798, .T. ) ;
#66966 = CARTESIAN_POINT ( 'NONE',  ( 0.1532563361054082862, 31.21726448433412315, 2.638427012816831674 ) ) ;
#66968 = CARTESIAN_POINT ( 'NONE',  ( -2.816281873526471635, 53.91530133659709634, -3.434112377981056508 ) ) ;
#66969 = DIRECTION ( 'NONE',  ( -0.8038568606172203923, 0.000000000000000000, 0.5948227867513371514 ) ) ;
#66971 = EDGE_CURVE ( 'NONE', #53047, #11431, #74000, .T. ) ;
#66970 = CARTESIAN_POINT ( 'NONE',  ( 16.40814093676324603, 2.456968003263753531, -11.09922568453594671 ) ) ;
#66972 = CARTESIAN_POINT ( 'NONE',  ( 4.559911319644449179, 3.897018677488170990, 9.422509992056141925 ) ) ;
#66973 = CARTESIAN_POINT ( 'NONE',  ( -4.164238869374098151, 16.59541550158063927, -3.795296366450310543 ) ) ;
#66974 = CARTESIAN_POINT ( 'NONE',  ( 2.153642693323453372, 41.13791097397318453, -6.500000000000040856 ) ) ;
#66975 = EDGE_CURVE ( 'NONE', #57072, #13800, #28671, .T. ) ;
#66976 = CARTESIAN_POINT ( 'NONE',  ( -0.3689425029237898834, 36.17874883491396787, -10.36894250292378850 ) ) ;
#66977 = CARTESIAN_POINT ( 'NONE',  ( -4.164238869374099039, 41.80374883491397497, 8.674139862899312516E-16 ) ) ;
#66978 = CARTESIAN_POINT ( 'NONE',  ( 2.917880565312950480, 15.97041550158063217, -12.26659068614894821 ) ) ;
#66979 = CARTESIAN_POINT ( 'NONE',  ( -2.266590686148945544, 17.22041550158063572, 7.082119434687048631 ) ) ;
#66980 = CARTESIAN_POINT ( 'NONE',  ( 17.96484262340118221, 51.18868534415483396, -7.964842623401177768 ) ) ;
#66981 = CARTESIAN_POINT ( 'NONE',  ( 3.969999999999999751, 10.25000000000000000, 2.750000000000000000 ) ) ;
#66982 = ORIENTED_EDGE ( 'NONE', *, *, #6586, .T. ) ;
#66983 = CARTESIAN_POINT ( 'NONE',  ( 7.361572987183170547, 32.05059781766745175, 9.846743663894590881 ) ) ;
#66985 = CARTESIAN_POINT ( 'NONE',  ( 12.63842701281683922, 24.55059781766745175, -9.846743663894590881 ) ) ;
#66984 = CARTESIAN_POINT ( 'NONE',  ( 0.000000000000000000, 69.50000000000000000, 6.500000000000000888 ) ) ;
#66986 = CARTESIAN_POINT ( 'NONE',  ( 20.88017736071110164, 5.355352010821503583, 2.915334737309930979 ) ) ;
#66987 = CARTESIAN_POINT ( 'NONE',  ( 6.565887622018943937, 65.16530133659709634, 12.81628187352647430 ) ) ;
#66988 = CARTESIAN_POINT ( 'NONE',  ( 10.00000000000000178, 52.25893115100078745, 9.846743663894594434 ) ) ;
#66989 = SURFACE_STYLE_FILL_AREA ( #82482 ) ;
#66990 = CARTESIAN_POINT ( 'NONE',  ( 17.20831665107776587, 24.13393115100078035, -7.208316651077762316 ) ) ;
#66991 = CARTESIAN_POINT ( 'NONE',  ( 10.00000000000000178, 40.37363466993042493, 12.81628187352647608 ) ) ;
#66992 = CARTESIAN_POINT ( 'NONE',  ( 14.16423886937410437, -25.90458449841936073, 3.795296366450304770 ) ) ;
#66993 = CARTESIAN_POINT ( 'NONE',  ( 2.035157376598822676, 42.43868534415483396, -7.964842623401177768 ) ) ;
#66994 = CARTESIAN_POINT ( 'NONE',  ( 17.20831665107776587, 44.13393115100078745, -7.208316651077762316 ) ) ;
#66995 = CARTESIAN_POINT ( 'NONE',  ( 24.16423886937409904, 29.09541550158063572, 3.795296366450317205 ) ) ;
#66996 = ORIENTED_EDGE ( 'NONE', *, *, #60606, .F. ) ;
#66997 = CARTESIAN_POINT ( 'NONE',  ( -4.164238869374099039, 6.803748834913967869, 8.674139862899312516E-16 ) ) ;
#66998 = B_SPLINE_CURVE_WITH_KNOTS ( 'NONE', 3,
 ( #79289, #71308, #41316, #2827 ),
 .UNSPECIFIED., .F., .F.,
 ( 4, 4 ),
 ( 0.000000000000000000, 0.002392975128318458166 ),
 .UNSPECIFIED. ) ;
#66999 = CARTESIAN_POINT ( 'NONE',  ( 4.559911319644449179, 48.89701867748817676, 9.422509992056141925 ) ) ;
#67000 = CARTESIAN_POINT ( 'NONE',  ( 0.000000000000000000, -97.00000000000000000, -2.500000000000000000 ) ) ;
#67001 = CARTESIAN_POINT ( 'NONE',  ( -4.164238869374099039, 61.80374883491397497, 8.674139862899312516E-16 ) ) ;
#67002 = CARTESIAN_POINT ( 'NONE',  ( 10.00000000000000178, 67.25893115100079456, 9.846743663894594434 ) ) ;
#67003 = CARTESIAN_POINT ( 'NONE',  ( 0.000000000000000000, 0.5000000000000004441, 0.000000000000000000 ) ) ;
#67004 = CARTESIAN_POINT ( 'NONE',  ( 17.96484262340118221, 54.93868534415484106, 7.964842623401181321 ) ) ;
#67005 = CARTESIAN_POINT ( 'NONE',  ( 20.15039907845753220, 42.62777174578613426, -6.262539305110077947 ) ) ;
#67006 = AXIS2_PLACEMENT_3D ( 'NONE', #61843, #59873, #16360 ) ;
#67007 = CARTESIAN_POINT ( 'NONE',  ( -2.816281873526473856, 34.33196800326376064, 3.434112377981055619 ) ) ;
#67008 = CARTESIAN_POINT ( 'NONE',  ( 0.1532563361054083140, 61.00893115100078745, 1.131784320476157264E-15 ) ) ;
#67009 = CARTESIAN_POINT ( 'NONE',  ( -10.88017736071109987, 28.27201867748817676, 2.915334737309934532 ) ) ;
#67010 = CARTESIAN_POINT ( 'NONE',  ( 10.00000000000000000, 16.81368534415483751, -10.88017736071110342 ) ) ;
#67011 = CARTESIAN_POINT ( 'NONE',  ( 20.88017736071110519, 10.56368534415483929, 2.639326808657452039E-16 ) ) ;
#67012 = CARTESIAN_POINT ( 'NONE',  ( 14.92337183194729633, 42.67559781766745886, 8.527530157486181039 ) ) ;
#67013 = CARTESIAN_POINT ( 'NONE',  ( 2.603489959281614308, 41.58210964143329846, 6.500000000000031086 ) ) ;
#67014 = ORIENTED_EDGE ( 'NONE', *, *, #22725, .T. ) ;
#67015 = AXIS2_PLACEMENT_3D ( 'NONE', #51413, #80929, #65416 ) ;
#67016 = ADVANCED_FACE ( 'NONE', ( #4694 ), #51161, .T. ) ;
#67017 = CARTESIAN_POINT ( 'NONE',  ( 10.00000000000000178, 10.37363466993041961, 12.81628187352647608 ) ) ;
#67018 = CARTESIAN_POINT ( 'NONE',  ( 0.000000000000000000, 14.49999999999999822, 0.000000000000000000 ) ) ;
#67019 = CARTESIAN_POINT ( 'NONE',  ( 19.84674366389459266, 8.300597817667451750, 2.638427012816836559 ) ) ;
#67020 = CARTESIAN_POINT ( 'NONE',  ( 7.361572987183170547, 52.05059781766745175, 9.846743663894590881 ) ) ;
#67021 = CARTESIAN_POINT ( 'NONE',  ( 7.084665262690076126, 37.02201867748817676, -10.88017736071110164 ) ) ;
#67022 = CARTESIAN_POINT ( 'NONE',  ( 16.40814093676323893, 10.79030133659708923, 11.09922568453595026 ) ) ;
#67024 = CARTESIAN_POINT ( 'NONE',  ( 17.82110031882830725, 91.00000000000001421, 8.000000000000001776 ) ) ;
#67023 = CARTESIAN_POINT ( 'NONE',  ( 7.084665262690076126, 52.02201867748816255, -10.88017736071110164 ) ) ;
#67025 = DIRECTION ( 'NONE',  ( 0.000000000000000000, 0.000000000000000000, -1.000000000000000000 ) ) ;
#67026 = CARTESIAN_POINT ( 'NONE',  ( -2.816281873526471635, 48.91530133659708213, -3.434112377981056508 ) ) ;
#67027 = ORIENTED_EDGE ( 'NONE', *, *, #76054, .T. ) ;
#67028 = CARTESIAN_POINT ( 'NONE',  ( 4.559911319644449179, 63.89701867748817676, 9.422509992056141925 ) ) ;
#67030 = CARTESIAN_POINT ( 'NONE',  ( -4.164238869374099039, 1.803748834913967647, 8.674139862899312516E-16 ) ) ;
#67029 = CARTESIAN_POINT ( 'NONE',  ( 19.38216949554541202, 35.99863466993041072, 9.382169495545424454 ) ) ;
#67031 = SURFACE_STYLE_USAGE ( .BOTH. , #20044 ) ;
#67032 = CARTESIAN_POINT ( 'NONE',  ( -0.8801773607110991993, 42.85535201082150536, -2.915334737309923874 ) ) ;
#67033 = DIRECTION ( 'NONE',  ( -0.000000000000000000, -1.000000000000000000, -0.000000000000000000 ) ) ;
#67034 = CARTESIAN_POINT ( 'NONE',  ( 5.076628168052704559, 60.17559781766745175, -8.527530157486179263 ) ) ;
#67035 = CARTESIAN_POINT ( 'NONE',  ( 0.1532563361054082862, 16.21726448433411960, 2.638427012816831674 ) ) ;
#67036 = CARTESIAN_POINT ( 'NONE',  ( 2.791683348922237240, 10.38393115100078390, -7.208316651077763204 ) ) ;
#67037 = CARTESIAN_POINT ( 'NONE',  ( 13.21382278599139859, 7.555533889508357052E-16, -6.271621331965521406 ) ) ;
#67038 = CARTESIAN_POINT ( 'NONE',  ( 17.08211943468705130, 48.47041550158063927, 12.26659068614894998 ) ) ;
#67039 = CYLINDRICAL_SURFACE ( 'NONE', #48970, 15.00000000000000000 ) ;
#67040 = CARTESIAN_POINT ( 'NONE',  ( 9.113212362719171011, -7.248705549479112165, -3.749999999999999112 ) ) ;
#67041 = SURFACE_SIDE_STYLE ('',( #44030 ) ) ;
#67042 = ORIENTED_EDGE ( 'NONE', *, *, #21717, .F. ) ;
#67043 = CARTESIAN_POINT ( 'NONE',  ( 20.36894250292379382, 58.67874883491396076, 10.36894250292379205 ) ) ;
#67044 = CARTESIAN_POINT ( 'NONE',  ( 24.16423886937409904, 64.09541550158064638, 3.795296366450317205 ) ) ;
#67045 = CARTESIAN_POINT ( 'NONE',  ( 19.84674366389459266, 33.71726448433410894, -2.638427012816827677 ) ) ;
#67046 = CARTESIAN_POINT ( 'NONE',  ( 22.81628187352648496, 26.83196800326374998, -3.434112377981050290 ) ) ;
#67047 = SURFACE_STYLE_USAGE ( .BOTH. , #13052 ) ;
#67048 = FILL_AREA_STYLE_COLOUR ( '', #45073 ) ;
#67049 = CARTESIAN_POINT ( 'NONE',  ( 10.00000000000000000, 11.81368534415483751, -10.88017736071110342 ) ) ;
#67050 = CARTESIAN_POINT ( 'NONE',  ( 17.08211943468705130, 58.47041550158063927, 12.26659068614894998 ) ) ;
#67051 = CARTESIAN_POINT ( 'NONE',  ( 10.00000000000000178, 32.25893115100078745, 9.846743663894594434 ) ) ;
#67052 = CARTESIAN_POINT ( 'NONE',  ( 0.6076426042653192416, 12.37576471608601203, -6.500000000000002665 ) ) ;
#67053 = CARTESIAN_POINT ( 'NONE',  ( 19.84674366389459266, 3.717264484334118713, -2.638427012816827677 ) ) ;
#67054 = DIRECTION ( 'NONE',  ( 0.000000000000000000, 0.000000000000000000, -1.000000000000000000 ) ) ;
#67055 = CARTESIAN_POINT ( 'NONE',  ( -2.638427012816840111, 19.96726448433413026, -9.846743663894590881 ) ) ;
#67056 = ORIENTED_EDGE ( 'NONE', *, *, #74995, .F. ) ;
#67057 = VERTEX_POINT ( 'NONE', #98165 ) ;
#67059 = EDGE_CURVE ( 'NONE', #23929, #4006, #65473, .T. ) ;
#67058 =( LENGTH_UNIT ( ) NAMED_UNIT ( * ) SI_UNIT ( .MILLI., .METRE. ) );
#67060 = EDGE_LOOP ( 'NONE', ( #64698, #93594, #64051, #98451, #28653 ) ) ;
#67061 = CARTESIAN_POINT ( 'NONE',  ( 19.84674366389459266, 43.30059781766744464, 2.638427012816836559 ) ) ;
#67063 = CARTESIAN_POINT ( 'NONE',  ( 15.44008868035555793, 26.39701867748817321, -9.422509992056140149 ) ) ;
#67062 = CARTESIAN_POINT ( 'NONE',  ( 15.44008868035555260, 14.73035201082150536, 9.422509992056143702 ) ) ;
#67065 = CARTESIAN_POINT ( 'NONE',  ( 16.40814093676324603, 17.45696800326375353, -11.09922568453594671 ) ) ;
#67064 = CARTESIAN_POINT ( 'NONE',  ( 5.076628168052703671, 61.84226448433412315, 8.527530157486179263 ) ) ;
#67066 = EDGE_CURVE ( 'NONE', #80552, #92371, #63900, .T. ) ;
#67067 = CARTESIAN_POINT ( 'NONE',  ( 21.09922568453594849, 31.20696800326375353, 6.408140936763242479 ) ) ;
#67068 = EDGE_CURVE ( 'NONE', #8562, #76767, #1176, .T. ) ;
#67069 = VERTEX_POINT ( 'NONE', #67655 ) ;
#67070 = CARTESIAN_POINT ( 'NONE',  ( 17.20831665107776587, 29.13393115100078390, -7.208316651077762316 ) ) ;
#67071 = CARTESIAN_POINT ( 'NONE',  ( 19.42250999205614548, 10.98035201082150536, -5.440088680355545492 ) ) ;
#67072 = ORIENTED_EDGE ( 'NONE', *, *, #24772, .F. ) ;
#67073 = CARTESIAN_POINT ( 'NONE',  ( 12.91533473730993009, 6.605352010821504471, -10.88017736071109987 ) ) ;
#67074 = EDGE_LOOP ( 'NONE', ( #89813, #58417, #18576, #82570 ) ) ;
#67075 = CARTESIAN_POINT ( 'NONE',  ( 10.00000000000000000, 46.81368534415484106, -10.88017736071110342 ) ) ;
#67076 = AXIS2_PLACEMENT_3D ( 'NONE', #70350, #18325, #10823 ) ;
#67077 = CARTESIAN_POINT ( 'NONE',  ( 10.00000000000000000, 61.81368534415484106, -10.88017736071110342 ) ) ;
#67078 = CARTESIAN_POINT ( 'NONE',  ( 4.559911319644449179, 68.89701867748817676, 9.422509992056141925 ) ) ;
#67079 = FACE_OUTER_BOUND ( 'NONE', #37167, .T. ) ;
#67080 = CARTESIAN_POINT ( 'NONE',  ( 10.00000000000000178, 59.31368534415484106, 10.88017736071110342 ) ) ;
#67081 = AXIS2_PLACEMENT_3D ( 'NONE', #88829, #50837, #81330 ) ;
#67082 = EDGE_CURVE ( 'NONE', #96556, #58998, #36660, .T. ) ;
#67083 = CARTESIAN_POINT ( 'NONE',  ( 8.879999999999991900, 27.04366094290857347, 2.900000000000000355 ) ) ;
#67084 = COLOUR_RGB ( '', 0.31764706, 0.68627451, 0.89019608) ;
#67085 = FACE_OUTER_BOUND ( 'NONE', #29613, .T. ) ;
#67086 = CARTESIAN_POINT ( 'NONE',  ( 2.791683348922240793, 31.63393115100078745, 7.208316651077764092 ) ) ;
#67087 = ORIENTED_EDGE ( 'NONE', *, *, #37685, .T. ) ;
#67088 = CARTESIAN_POINT ( 'NONE',  ( 19.84674366389459266, 58.30059781766745886, 2.638427012816836559 ) ) ;
#67089 = PLANE ( 'NONE',  #11672 ) ;
#67090 = EDGE_CURVE ( 'NONE', #86126, #3586, #78612, .T. ) ;
#67091 =( NAMED_UNIT ( * ) SI_UNIT ( $, .STERADIAN. ) SOLID_ANGLE_UNIT ( ) );
#67092 = EDGE_LOOP ( 'NONE', ( #78737, #72896, #52639, #90650 ) ) ;
#67093 = CARTESIAN_POINT ( 'NONE',  ( -11.09639892720896093, 12.99830704344312693, 3.869676107586555336 ) ) ;
#67094 = DIRECTION ( 'NONE',  ( 0.000000000000000000, -1.000000000000000000, 0.000000000000000000 ) ) ;
#67096 = CARTESIAN_POINT ( 'NONE',  ( 19.84674366389459621, 38.50893115100078745, 7.409399052514197653E-17 ) ) ;
#67095 = CARTESIAN_POINT ( 'NONE',  ( 20.00000000000000711, 98.59912998021083297, -4.500000000000001776 ) ) ;
#67097 = CARTESIAN_POINT ( 'NONE',  ( 4.559911319644449179, 12.23035201082150714, -9.422509992056141925 ) ) ;
#67098 = CARTESIAN_POINT ( 'NONE',  ( 18.50749283717780003, 64.69955587570481725, 6.499999999999917399 ) ) ;
#67099 = ORIENTED_EDGE ( 'NONE', *, *, #66616, .F. ) ;
#67100 = DIRECTION ( 'NONE',  ( 0.000000000000000000, -1.000000000000000000, 0.000000000000000000 ) ) ;
#67101 = CARTESIAN_POINT ( 'NONE',  ( 7.361572987183170547, 42.05059781766745886, 9.846743663894590881 ) ) ;
#67102 = CARTESIAN_POINT ( 'NONE',  ( 6.767445849361248378, 14.63595249122789177, -13.38662304974498340 ) ) ;
#67103 = CARTESIAN_POINT ( 'NONE',  ( 0.6178305044545838731, 19.74863466993042138, 9.382169495545420901 ) ) ;
#67104 = CARTESIAN_POINT ( 'NONE',  ( 1.472469842513823179, 11.42559781766745175, 4.923371831947296329 ) ) ;
#67105 = CARTESIAN_POINT ( 'NONE',  ( -14.82269085861170232, 0.5000000000000004441, 2.299529454046861154 ) ) ;
#67106 = CARTESIAN_POINT ( 'NONE',  ( 3.591859063236761518, 4.956968003263753531, 11.09922568453594849 ) ) ;
#67107 = CARTESIAN_POINT ( 'NONE',  ( 1.959929470562070675, 26.50257860105346452, 5.767676674365487699 ) ) ;
#67108 = ORIENTED_EDGE ( 'NONE', *, *, #81967, .T. ) ;
#67109 = CARTESIAN_POINT ( 'NONE',  ( 10.00000000000000178, 4.313685344154837509, 10.88017736071110342 ) ) ;
#67110 = CARTESIAN_POINT ( 'NONE',  ( 6.204703633549690345, 12.84541550158063572, 14.16423886937410082 ) ) ;
#67111 = CARTESIAN_POINT ( 'NONE',  ( 7.361572987183169658, 29.96726448433411960, -9.846743663894592657 ) ) ;
#67112 = CARTESIAN_POINT ( 'NONE',  ( 20.88017736071110519, 55.56368534415484817, 2.639326808657452039E-16 ) ) ;
#67114 = CARTESIAN_POINT ( 'NONE',  ( -10.58981376305275468, -0.03417435944610275333, -9.535111140613857117 ) ) ;
#67113 = CARTESIAN_POINT ( 'NONE',  ( 3.591859063236761518, 44.95696800326376064, 11.09922568453594849 ) ) ;
#67115 = CARTESIAN_POINT ( 'NONE',  ( -0.8801773607111009756, 8.063685344154837509, 1.068504757029289695E-15 ) ) ;
#67116 = FACE_OUTER_BOUND ( 'NONE', #28995, .T. ) ;
#67117 = FACE_OUTER_BOUND ( 'NONE', #32656, .T. ) ;
#67118 = CARTESIAN_POINT ( 'NONE',  ( -2.816281873526471635, 3.915301336597087456, -3.434112377981056508 ) ) ;
#67119 = CARTESIAN_POINT ( 'NONE',  ( 2.791683348922240793, 66.63393115100079456, 7.208316651077764092 ) ) ;
#67120 = CARTESIAN_POINT ( 'NONE',  ( 19.84674366389459621, 28.50893115100078745, 7.409399052514197653E-17 ) ) ;
#67121 = CARTESIAN_POINT ( 'NONE',  ( -7.964842623401172439, -6.311314655845153609, 7.964842623401183097 ) ) ;
#67122 = CARTESIAN_POINT ( 'NONE',  ( 22.81628187352647785, 36.41530133659707502, 3.434112377981063169 ) ) ;
#67124 = CARTESIAN_POINT ( 'NONE',  ( 14.73513795193454534, 0.04922511925147087658, 0.7223639599947853096 ) ) ;
#67123 = CARTESIAN_POINT ( 'NONE',  ( 17.96484262340118221, 46.18868534415484106, -7.964842623401177768 ) ) ;
#67125 = DIRECTION ( 'NONE',  ( 0.000000000000000000, 0.000000000000000000, 1.000000000000000000 ) ) ;
#67126 = CARTESIAN_POINT ( 'NONE',  ( -0.8801773607111008646, 38.27201867748816255, 2.915334737309923430 ) ) ;
#67127 = AXIS2_PLACEMENT_3D ( 'NONE', #28281, #75261, #75754 ) ;
#67128 = CARTESIAN_POINT ( 'NONE',  ( 0.5774900079438607392, 33.48035201082150536, 5.440088680355550821 ) ) ;
#67129 = CARTESIAN_POINT ( 'NONE',  ( 10.00000000000000178, 62.25893115100078745, 9.846743663894594434 ) ) ;
#67130 = CARTESIAN_POINT ( 'NONE',  ( 15.44008868035555260, 49.73035201082150536, 9.422509992056143702 ) ) ;
#67132 = UNCERTAINTY_MEASURE_WITH_UNIT (LENGTH_MEASURE( 1.000000000000000082E-05 ), #36406, 'distance_accuracy_value', 'NONE');
#67131 = B_SPLINE_CURVE_WITH_KNOTS ( 'NONE', 3,
 ( #37320, #76775, #30771, #38788 ),
 .UNSPECIFIED., .F., .F.,
 ( 4, 4 ),
 ( 5.421010862427522170E-20, 0.002657014572711328959 ),
 .UNSPECIFIED. ) ;
#67133 = CARTESIAN_POINT ( 'NONE',  ( 17.20831665107776587, 34.13393115100078745, -7.208316651077762316 ) ) ;
#67134 = CARTESIAN_POINT ( 'NONE',  ( 19.42250999205614193, 15.14701867748817143, 5.440088680355555262 ) ) ;
#67135 = VECTOR ( 'NONE', #67384, 1000.000000000000000 ) ;
#67136 = CARTESIAN_POINT ( 'NONE',  ( 10.00000000000000178, 10.37363466993041961, 12.81628187352647608 ) ) ;
#67137 = VERTEX_POINT ( 'NONE', #75633 ) ;
#67138 = CARTESIAN_POINT ( 'NONE',  ( 17.96484262340118221, 26.18868534415483396, -7.964842623401177768 ) ) ;
#67139 = CARTESIAN_POINT ( 'NONE',  ( 0.5774900079438590739, 2.647018677488170990, -5.440088680355550821 ) ) ;
#67140 = CARTESIAN_POINT ( 'NONE',  ( -0.8801773607110991993, 12.85535201082150358, -2.915334737309923874 ) ) ;
#67141 = CARTESIAN_POINT ( 'NONE',  ( -0.8801773607111008646, 63.27201867748817676, 2.915334737309923430 ) ) ;
#67142 = CARTESIAN_POINT ( 'NONE',  ( 24.16423886937409904, 29.09541550158063572, 3.795296366450317205 ) ) ;
#67143 = EDGE_CURVE ( 'NONE', #73111, #33570, #62339, .T. ) ;
#67144 = CARTESIAN_POINT ( 'NONE',  ( 19.84674366389459621, 18.50893115100078745, 7.409399052514197653E-17 ) ) ;
#67145 = CARTESIAN_POINT ( 'NONE',  ( 20.88017736071110519, 50.56368534415484106, 2.639326808657452039E-16 ) ) ;
#67146 = CARTESIAN_POINT ( 'NONE',  ( -12.80781515976305762, -0.03417435944610275333, -6.246788841744501219 ) ) ;
#67147 = DIRECTION ( 'NONE',  ( 0.7716245833877193316, 0.000000000000000000, -0.6360782202777648386 ) ) ;
#67148 = VECTOR ( 'NONE', #69294, 1000.000000000000000 ) ;
#67149 = EDGE_CURVE ( 'NONE', #72566, #72059, #60127, .T. ) ;
#67150 = VERTEX_POINT ( 'NONE', #66147 ) ;
#67151 = CARTESIAN_POINT ( 'NONE',  ( -14.43063482171890399, 15.00000000000000888, -2.386446184883220578 ) ) ;
#67152 = CARTESIAN_POINT ( 'NONE',  ( 14.92337183194729988, 39.34226448433412315, -8.527530157486177487 ) ) ;
#67153 = ORIENTED_EDGE ( 'NONE', *, *, #74082, .T. ) ;
#67154 = ORIENTED_EDGE ( 'NONE', *, *, #98535, .T. ) ;
#67155 = DIRECTION ( 'NONE',  ( 0.09584575252023383451, 0.000000000000000000, -0.9953961983671778535 ) ) ;
#67156 = CARTESIAN_POINT ( 'NONE',  ( 2.917880565312948704, 22.63708216824730002, 12.26659068614894643 ) ) ;
#67157 = CARTESIAN_POINT ( 'NONE',  ( 10.00000000000000000, 20.55374883491396787, -14.16423886937410082 ) ) ;
#67158 = CARTESIAN_POINT ( 'NONE',  ( 20.88017736071110875, 60.77201867748817676, -2.915334737309920765 ) ) ;
#67159 = CARTESIAN_POINT ( 'NONE',  ( 2.035157376598824452, 3.688685344154837953, 7.964842623401179544 ) ) ;
#67160 = CARTESIAN_POINT ( 'NONE',  ( 0.6178305044545838731, 4.748634669930420493, 9.382169495545420901 ) ) ;
#67161 = CARTESIAN_POINT ( 'NONE',  ( 12.63842701281683922, 54.55059781766745175, -9.846743663894590881 ) ) ;
#67162 = DIRECTION ( 'NONE',  ( 0.000000000000000000, 0.000000000000000000, 1.000000000000000000 ) ) ;
#67164 = CARTESIAN_POINT ( 'NONE',  ( 22.81628187352647785, 6.415301336597088344, 3.434112377981063169 ) ) ;
#67163 = CARTESIAN_POINT ( 'NONE',  ( -0.8801773607111009756, 48.06368534415484817, 1.068504757029289695E-15 ) ) ;
#67165 = CARTESIAN_POINT ( 'NONE',  ( 6.204703633549690345, 10.76208216824729824, -14.16423886937410259 ) ) ;
#67166 = CARTESIAN_POINT ( 'NONE',  ( 20.88017736071110164, 20.35535201082150891, 2.915334737309930979 ) ) ;
#67167 = CARTESIAN_POINT ( 'NONE',  ( 15.44008868035555260, 19.73035201082150536, 9.422509992056143702 ) ) ;
#67168 = CARTESIAN_POINT ( 'NONE',  ( 17.39651004071838614, 52.93575266056826933, 6.500000000000032863 ) ) ;
#67169 = CARTESIAN_POINT ( 'NONE',  ( 10.00000000000000178, 44.31368534415484106, 10.88017736071110342 ) ) ;
#67170 = AXIS2_PLACEMENT_3D ( 'NONE', #55065, #40080, #9087 ) ;
#67171 = CARTESIAN_POINT ( 'NONE',  ( 3.591859063236761518, 49.95696800326375353, 11.09922568453594849 ) ) ;
#67172 = CARTESIAN_POINT ( 'NONE',  ( -9.846743663894596210, -24.19940218233254114, -2.638427012816824124 ) ) ;
#67173 = ORIENTED_EDGE ( 'NONE', *, *, #80208, .T. ) ;
#67174 = CARTESIAN_POINT ( 'NONE',  ( 20.15039907845753930, 4.722660991849187972, 6.262539305110067289 ) ) ;
#67175 = ORIENTED_EDGE ( 'NONE', *, *, #9982, .F. ) ;
#67176 = ORIENTED_EDGE ( 'NONE', *, *, #51871, .F. ) ;
#67177 = MECHANICAL_DESIGN_GEOMETRIC_PRESENTATION_REPRESENTATION (  '', ( #9814 ), #97536 ) ;
#67178 = CARTESIAN_POINT ( 'NONE',  ( 11.81378540890930751, 15.00000000000000000, 7.968498874458199488 ) ) ;
#67180 = CARTESIAN_POINT ( 'NONE',  ( 17.96484262340118221, 6.188685344154837509, -7.964842623401177768 ) ) ;
#67179 = CARTESIAN_POINT ( 'NONE',  ( -0.3689425029237881626, 47.42874883491396787, 10.36894250292379027 ) ) ;
#67182 = CARTESIAN_POINT ( 'NONE',  ( 1.472469842513823179, 50.59226448433411605, -4.923371831947296329 ) ) ;
#67181 = CARTESIAN_POINT ( 'NONE',  ( 18.52753015748618282, 18.92559781766745175, -4.923371831947291888 ) ) ;
#67183 = FACE_OUTER_BOUND ( 'NONE', #19283, .T. ) ;
#67184 = B_SPLINE_CURVE_WITH_KNOTS ( 'NONE', 3,
 ( #11386, #93904, #63877, #72369, #55914, #24441 ),
 .UNSPECIFIED., .F., .F.,
 ( 4, 2, 4 ),
 ( 0.000000000000000000, 0.0002605067024380913927, 0.0005210134048761827855 ),
 .UNSPECIFIED. ) ;
#67185 = CARTESIAN_POINT ( 'NONE',  ( -0.8801773607110991993, 62.85535201082150536, -2.915334737309923874 ) ) ;
#67186 = ADVANCED_FACE ( 'NONE', ( #52145 ), #61774, .T. ) ;
#67187 = CIRCLE ( 'NONE', #16081, 9.999999999999998224 ) ;
#67188 = CARTESIAN_POINT ( 'NONE',  ( -3.434112377981067610, 18.08196800326375708, -12.81628187352647252 ) ) ;
#67189 = EDGE_CURVE ( 'NONE', #76776, #3849, #6155, .T. ) ;
#67190 = ORIENTED_EDGE ( 'NONE', *, *, #35460, .T. ) ;
#67191 = CARTESIAN_POINT ( 'NONE',  ( -0.3689425029237898834, 31.17874883491396787, -10.36894250292378850 ) ) ;
#67192 = CARTESIAN_POINT ( 'NONE',  ( 22.81628187352647785, 26.41530133659708923, 3.434112377981063169 ) ) ;
#67193 = VERTEX_POINT ( 'NONE', #5672 ) ;
#67194 = CARTESIAN_POINT ( 'NONE',  ( 16.40814093676323893, 45.79030133659708923, 11.09922568453595026 ) ) ;
#67195 = CARTESIAN_POINT ( 'NONE',  ( 4.559911319644449179, 18.89701867748817321, 9.422509992056141925 ) ) ;
#67196 = CARTESIAN_POINT ( 'NONE',  ( 5.076628168052704559, 40.17559781766745175, -8.527530157486179263 ) ) ;
#67197 = CARTESIAN_POINT ( 'NONE',  ( 17.96484262340118221, 14.93868534415483751, 7.964842623401181321 ) ) ;
#67198 = CARTESIAN_POINT ( 'NONE',  ( -1.099225684535947600, 64.54030133659709634, 6.408140936763237150 ) ) ;
#67199 = CARTESIAN_POINT ( 'NONE',  ( -0.1503990784575277295, 39.24884699246889141, -6.262539305110077947 ) ) ;
#67200 = CARTESIAN_POINT ( 'NONE',  ( 2.791683348922240793, 36.63393115100078035, 7.208316651077764092 ) ) ;
#67201 = CARTESIAN_POINT ( 'NONE',  ( 14.92337183194729988, 54.34226448433412315, -8.527530157486177487 ) ) ;
#67204 = EDGE_LOOP ( 'NONE', ( #36704, #10454, #19848, #32478, #98208, #45568 ) ) ;
#67203 = VECTOR ( 'NONE', #47076, 999.9999999999998863 ) ;
#67202 = CARTESIAN_POINT ( 'NONE',  ( -0.1503990784575328643, 70.00000000000000000, 6.262539305110068177 ) ) ;
#67205 = DIRECTION ( 'NONE',  ( -0.000000000000000000, -1.000000000000000000, -0.000000000000000000 ) ) ;
#67206 = DIRECTION ( 'NONE',  ( 0.000000000000000000, 1.000000000000000000, 0.000000000000000000 ) ) ;
#67207 = CARTESIAN_POINT ( 'NONE',  ( -45.94000000000000483, 93.00000000000000000, -8.999999999999998224 ) ) ;
#67208 = EDGE_CURVE ( 'NONE', #52058, #57773, #15491, .T. ) ;
#67209 = CARTESIAN_POINT ( 'NONE',  ( -41.94000000000001194, 93.50000000000000000, -9.500000000000000000 ) ) ;
#67210 = CARTESIAN_POINT ( 'NONE',  ( 19.84674366389459266, 18.30059781766745175, 2.638427012816836559 ) ) ;
#67211 = CARTESIAN_POINT ( 'NONE',  ( 10.00000000000000000, 42.87363466993042493, -12.81628187352647608 ) ) ;
#67212 = AXIS2_PLACEMENT_3D ( 'NONE', #73771, #74765, #96303 ) ;
#67213 = LINE ( 'NONE', #53681, #21239 ) ;
#67214 = ADVANCED_FACE ( 'NONE', ( #97670 ), #91126, .F. ) ;
#67215 = ORIENTED_EDGE ( 'NONE', *, *, #14696, .T. ) ;
#67216 = CARTESIAN_POINT ( 'NONE',  ( 19.84674366389459266, 58.30059781766745886, 2.638427012816836559 ) ) ;
#67217 = CARTESIAN_POINT ( 'NONE',  ( -9.399392868737892925, 4.026710370808002065E-16, 11.04089732309467919 ) ) ;
#67218 = CARTESIAN_POINT ( 'NONE',  ( 22.26659068614894466, 33.88708216824730357, 7.082119434687054849 ) ) ;
#67219 = CARTESIAN_POINT ( 'NONE',  ( 14.92337183194729988, 44.34226448433412315, -8.527530157486177487 ) ) ;
#67220 = CARTESIAN_POINT ( 'NONE',  ( 22.81628187352648496, 51.83196800326376064, -3.434112377981050290 ) ) ;
#67222 = DIRECTION ( 'NONE',  ( -0.000000000000000000, -1.000000000000000000, -0.000000000000000000 ) ) ;
#67221 = CARTESIAN_POINT ( 'NONE',  ( 5.054308323419911098, 70.51564955044841554, -12.00000000000000000 ) ) ;
#67223 = CARTESIAN_POINT ( 'NONE',  ( 10.00000000000000000, -0.2410688489992152128, -9.846743663894594434 ) ) ;
#67224 = CARTESIAN_POINT ( 'NONE',  ( 0.000000000000000000, 15.00000000000000000, 0.000000000000000000 ) ) ;
#67225 = CARTESIAN_POINT ( 'NONE',  ( 5.076628168052704559, 50.17559781766745886, -8.527530157486179263 ) ) ;
#67226 = CARTESIAN_POINT ( 'NONE',  ( 17.96484262340118221, 41.18868534415484106, -7.964842623401177768 ) ) ;
#67227 = CARTESIAN_POINT ( 'NONE',  ( 7.361572987183170547, 32.05059781766745175, 9.846743663894590881 ) ) ;
#67228 = DIRECTION ( 'NONE',  ( -0.9975640502598243087, 0.06975647374412544122, 0.000000000000000000 ) ) ;
#67229 = CARTESIAN_POINT ( 'NONE',  ( 15.44008868035555260, 39.73035201082150536, 9.422509992056143702 ) ) ;
#67230 = ORIENTED_EDGE ( 'NONE', *, *, #88708, .F. ) ;
#67231 = CARTESIAN_POINT ( 'NONE',  ( -3.843478602184351889, 0.2306972965111881713, -14.43834224996327897 ) ) ;
#67232 = CARTESIAN_POINT ( 'NONE',  ( 20.88017736071110164, 20.35535201082150891, 2.915334737309930979 ) ) ;
#67234 = CARTESIAN_POINT ( 'NONE',  ( -0.8801773607110991993, 37.85535201082151247, -2.915334737309923874 ) ) ;
#67233 = CARTESIAN_POINT ( 'NONE',  ( 19.84674366389459266, 63.30059781766745886, 2.638427012816836559 ) ) ;
#67235 = DIRECTION ( 'NONE',  ( -1.154631945610162802E-14, 0.000000000000000000, 1.000000000000000000 ) ) ;
#67236 = CARTESIAN_POINT ( 'NONE',  ( 17.96484262340118221, 64.93868534415483396, 7.964842623401181321 ) ) ;
#67237 = CARTESIAN_POINT ( 'NONE',  ( -8.000000000000000000, 80.32179676972448590, 3.750000000000000000 ) ) ;
#67239 = DIRECTION ( 'NONE',  ( -1.000000000000000000, 0.000000000000000000, 0.000000000000000000 ) ) ;
#67238 = CARTESIAN_POINT ( 'NONE',  ( 17.96484262340118221, 31.18868534415483751, -7.964842623401177768 ) ) ;
#67240 = CARTESIAN_POINT ( 'NONE',  ( 19.84674366389459266, 13.71726448433411782, -2.638427012816827677 ) ) ;
#67241 = CARTESIAN_POINT ( 'NONE',  ( 12.63842701281683034, 22.46726448433411605, 9.846743663894596210 ) ) ;
#67242 = CARTESIAN_POINT ( 'NONE',  ( -1.796645268984824240, 14.76930270348881002, 14.83273813124057661 ) ) ;
#67243 = CARTESIAN_POINT ( 'NONE',  ( -10.36894250292378317, 17.42874883491396787, 10.36894250292379560 ) ) ;
#67244 = CARTESIAN_POINT ( 'NONE',  ( 10.00000000000000000, -2.126365330069579951, -12.81628187352647608 ) ) ;
#67246 = CYLINDRICAL_SURFACE ( 'NONE', #56894, 0.2500000000000002220 ) ;
#67245 = CARTESIAN_POINT ( 'NONE',  ( 2.917880565312950480, 60.97041550158063927, -12.26659068614894821 ) ) ;
#67247 =( GEOMETRIC_REPRESENTATION_CONTEXT ( 3 ) GLOBAL_UNCERTAINTY_ASSIGNED_CONTEXT ( ( #7132 ) ) GLOBAL_UNIT_ASSIGNED_CONTEXT ( ( #61334, #37378, #53846 ) ) REPRESENTATION_CONTEXT ( 'NONE', 'WORKASPACE' ) );
#67248 = CARTESIAN_POINT ( 'NONE',  ( -6.000000000000009770, 41.24999999999999289, -6.500000000000000888 ) ) ;
#67249 = CARTESIAN_POINT ( 'NONE',  ( -0.3689425029237881626, 7.428748834913967869, 10.36894250292379027 ) ) ;
#67250 = CARTESIAN_POINT ( 'NONE',  ( 10.00000000000000178, 48.05374883491396787, 14.16423886937410082 ) ) ;
#67251 = CARTESIAN_POINT ( 'NONE',  ( 21.09922568453595559, 2.040301336597086568, -6.408140936763230044 ) ) ;
#67252 = VECTOR ( 'NONE', #64518, 1000.000000000000114 ) ;
#67253 = ORIENTED_EDGE ( 'NONE', *, *, #40114, .T. ) ;
#67254 = CARTESIAN_POINT ( 'NONE',  ( 14.92337183194729633, 12.67559781766745353, 8.527530157486181039 ) ) ;
#67255 = CARTESIAN_POINT ( 'NONE',  ( 2.035157376598824452, 8.688685344154839285, 7.964842623401179544 ) ) ;
#67256 = CARTESIAN_POINT ( 'NONE',  ( 0.1532563361054082862, 46.21726448433411605, 2.638427012816831674 ) ) ;
#67258 = CARTESIAN_POINT ( 'NONE',  ( -13.01808377376649339, 90.72591000950063744, -7.552080394871468094 ) ) ;
#67257 = FACE_OUTER_BOUND ( 'NONE', #44303, .T. ) ;
#67259 = CARTESIAN_POINT ( 'NONE',  ( 19.84674366389459266, 3.300597817667451750, 2.638427012816836559 ) ) ;
#67260 = CARTESIAN_POINT ( 'NONE',  ( -2.816281873526473856, 24.12363466993042138, 9.499525473075851096E-16 ) ) ;
#67261 = CARTESIAN_POINT ( 'NONE',  ( 18.52753015748618282, 23.92559781766745530, -4.923371831947291888 ) ) ;
#67262 = VERTEX_POINT ( 'NONE', #66658 ) ;
#67263 = CARTESIAN_POINT ( 'NONE',  ( 14.92337183194729633, 12.67559781766745353, 8.527530157486181039 ) ) ;
#67264 = CARTESIAN_POINT ( 'NONE',  ( 9.261738776797663775, -15.50721619310240662, -4.000000000000000000 ) ) ;
#67265 = CARTESIAN_POINT ( 'NONE',  ( -12.03829478939416120, 2.168404344971008868E-16, -8.307695547791567492 ) ) ;
#67266 = CARTESIAN_POINT ( 'NONE',  ( 4.559911319644449179, 8.897018677488171434, 9.422509992056141925 ) ) ;
#67267 = CARTESIAN_POINT ( 'NONE',  ( 13.79529636645031943, 45.34541550158062506, -14.16423886937409904 ) ) ;
#67268 = CARTESIAN_POINT ( 'NONE',  ( 12.91533473730992121, 39.52201867748817676, 10.88017736071110164 ) ) ;
#67269 = CARTESIAN_POINT ( 'NONE',  ( 20.88017736071110164, 60.35535201082151957, 2.915334737309930979 ) ) ;
#67270 = CARTESIAN_POINT ( 'NONE',  ( -0.4957494408796453977, 15.11603861882761812, 9.500000000000000000 ) ) ;
#67271 = CARTESIAN_POINT ( 'NONE',  ( 0.1532563361054083140, 26.00893115100078745, 1.131784320476157264E-15 ) ) ;
#67272 = CARTESIAN_POINT ( 'NONE',  ( 17.96484262340118221, 11.18868534415483929, -7.964842623401177768 ) ) ;
#67273 = CARTESIAN_POINT ( 'NONE',  ( 0.1532563361054083140, 1.008931151000784787, 1.131784320476157264E-15 ) ) ;
#67274 = CYLINDRICAL_SURFACE ( 'NONE', #70360, 0.2500000000000002220 ) ;
#67275 = CARTESIAN_POINT ( 'NONE',  ( 17.20831665107776587, 42.88393115100077324, 7.208316651077764980 ) ) ;
#67276 = EDGE_CURVE ( 'NONE', #31971, #35670, #42947, .T. ) ;
#67277 = EDGE_CURVE ( 'NONE', #74063, #60663, #44642, .T. ) ;
#67278 = CARTESIAN_POINT ( 'NONE',  ( 20.88017736071110519, 30.56368534415484106, 2.639326808657452039E-16 ) ) ;
#67279 = VECTOR ( 'NONE', #32947, 1000.000000000000000 ) ;
#67280 = ORIENTED_EDGE ( 'NONE', *, *, #31605, .T. ) ;
#67281 = CARTESIAN_POINT ( 'NONE',  ( 6.565887622018943937, 58.08196800326376064, -12.81628187352647608 ) ) ;
#67282 = CARTESIAN_POINT ( 'NONE',  ( -5.999999999999994671, 43.00000000000000000, 4.000000000000000000 ) ) ;
#67283 = CARTESIAN_POINT ( 'NONE',  ( 18.52753015748617571, 8.092264484334117824, 4.923371831947298993 ) ) ;
#67284 = CARTESIAN_POINT ( 'NONE',  ( 16.40814093676324603, 47.45696800326375353, -11.09922568453594671 ) ) ;
#67286 = CARTESIAN_POINT ( 'NONE',  ( 1.472469842513823179, 41.42559781766745886, 4.923371831947296329 ) ) ;
#67285 = CARTESIAN_POINT ( 'NONE',  ( -2.266590686148945544, 67.22041550158063217, 7.082119434687048631 ) ) ;
#67287 = CARTESIAN_POINT ( 'NONE',  ( 32.06412365047463453, 22.49999999999998934, -10.00000000000000000 ) ) ;
#67288 = CARTESIAN_POINT ( 'NONE',  ( -2.266590686148945544, 22.22041550158063572, 7.082119434687048631 ) ) ;
#67289 = CARTESIAN_POINT ( 'NONE',  ( 17.08211943468705840, 40.13708216824731068, -12.26659068614894466 ) ) ;
#67290 = CARTESIAN_POINT ( 'NONE',  ( 18.52753015748618282, 38.92559781766745175, -4.923371831947291888 ) ) ;
#67291 = MECHANICAL_DESIGN_GEOMETRIC_PRESENTATION_REPRESENTATION (  '', ( #35366 ), #24184 ) ;
#67292 = CARTESIAN_POINT ( 'NONE',  ( 7.084665262690076126, 37.02201867748817676, -10.88017736071110164 ) ) ;
#67293 = CARTESIAN_POINT ( 'NONE',  ( 7.361572987183170547, 2.050597817667451750, 9.846743663894590881 ) ) ;
#67294 = CARTESIAN_POINT ( 'NONE',  ( -4.021995598252596338, -6.415937870593706904, 4.000000000000000000 ) ) ;
#67295 = EDGE_LOOP ( 'NONE', ( #69287, #56999, #57181, #58078, #40371, #98516 ) ) ;
#67296 = CARTESIAN_POINT ( 'NONE',  ( 16.40814093676324603, 57.45696800326375353, -11.09922568453594671 ) ) ;
#67297 = CARTESIAN_POINT ( 'NONE',  ( 12.91533473730992121, 64.52201867748817676, 10.88017736071110164 ) ) ;
#67298 = ORIENTED_EDGE ( 'NONE', *, *, #841, .T. ) ;
#67299 = CARTESIAN_POINT ( 'NONE',  ( -0.3689425029237898834, 11.17874883491396787, -10.36894250292378850 ) ) ;
#67300 = CARTESIAN_POINT ( 'NONE',  ( 0.1532563361054100626, 10.80059781766745175, -2.638427012816831230 ) ) ;
#67301 = CARTESIAN_POINT ( 'NONE',  ( -1.926860441876562025, 59.47997603579417358, -3.195792623639529761 ) ) ;
#67302 = ORIENTED_EDGE ( 'NONE', *, *, #46382, .T. ) ;
#67303 = CARTESIAN_POINT ( 'NONE',  ( 17.96484262340118221, 29.93868534415484106, 7.964842623401181321 ) ) ;
#67304 = EDGE_CURVE ( 'NONE', #66028, #84144, #60817, .T. ) ;
#67305 = EDGE_CURVE ( 'NONE', #66734, #49892, #49005, .T. ) ;
#67306 = ORIENTED_EDGE ( 'NONE', *, *, #18762, .F. ) ;
#67307 = CARTESIAN_POINT ( 'NONE',  ( 17.96484262340118221, 41.18868534415484106, -7.964842623401177768 ) ) ;
#67308 = CARTESIAN_POINT ( 'NONE',  ( 10.00000000000000178, 67.25893115100079456, 9.846743663894594434 ) ) ;
#67309 = ORIENTED_EDGE ( 'NONE', *, *, #48740, .T. ) ;
#67310 = CARTESIAN_POINT ( 'NONE',  ( 22.81628187352648496, 11.83196800326375531, -3.434112377981050290 ) ) ;
#67311 = ORIENTED_EDGE ( 'NONE', *, *, #94046, .T. ) ;
#67312 = CARTESIAN_POINT ( 'NONE',  ( 19.42250999205614193, 65.14701867748817676, 5.440088680355555262 ) ) ;
#67313 = CARTESIAN_POINT ( 'NONE',  ( 14.92337183194729988, 59.34226448433412315, -8.527530157486177487 ) ) ;
#67315 = CARTESIAN_POINT ( 'NONE',  ( 0.000000000000000000, 70.00000000000000000, 5.000000000000000000 ) ) ;
#67314 = CARTESIAN_POINT ( 'NONE',  ( 10.00000000000000178, 19.31368534415484106, 10.88017736071110342 ) ) ;
#67316 = CARTESIAN_POINT ( 'NONE',  ( 7.361572987183170547, 2.050597817667451750, 9.846743663894590881 ) ) ;
#67317 = CARTESIAN_POINT ( 'NONE',  ( -0.8801773607110991993, 17.85535201082150536, -2.915334737309923874 ) ) ;
#67318 = MECHANICAL_DESIGN_GEOMETRIC_PRESENTATION_REPRESENTATION (  '', ( #22651 ), #80091 ) ;
#67319 = VECTOR ( 'NONE', #10920, 1000.000000000000000 ) ;
#67320 = VERTEX_POINT ( 'NONE', #39129 ) ;
#67321 = CARTESIAN_POINT ( 'NONE',  ( 16.40814093676323893, 50.79030133659708923, 11.09922568453595026 ) ) ;
#67322 = CARTESIAN_POINT ( 'NONE',  ( 4.559911319644449179, 43.89701867748816966, 9.422509992056141925 ) ) ;
#67323 = CARTESIAN_POINT ( 'NONE',  ( 2.174473938468889589, 0.000000000000000000, 5.000947681547232904 ) ) ;
#67324 = CARTESIAN_POINT ( 'NONE',  ( -1.099225684535947600, 53.70696800326376064, -6.408140936763238038 ) ) ;
#67325 = CARTESIAN_POINT ( 'NONE',  ( 12.91533473730992121, 49.52201867748817676, 10.88017736071110164 ) ) ;
#67326 = CARTESIAN_POINT ( 'NONE',  ( -2.816281873526471635, 3.915301336597087456, -3.434112377981056508 ) ) ;
#67327 = CARTESIAN_POINT ( 'NONE',  ( 5.076628168052703671, 21.84226448433411960, 8.527530157486179263 ) ) ;
#67328 = CARTESIAN_POINT ( 'NONE',  ( 16.40814093676324603, 2.456968003263753531, -11.09922568453594671 ) ) ;
#67330 = CARTESIAN_POINT ( 'NONE',  ( 17.20831665107776587, 64.13393115100079456, -7.208316651077762316 ) ) ;
#67329 = DIRECTION ( 'NONE',  ( -1.257402221000611116E-16, 1.000000000000000000, 0.000000000000000000 ) ) ;
#67331 = CARTESIAN_POINT ( 'NONE',  ( 15.44008868035555793, 41.39701867748817676, -9.422509992056140149 ) ) ;
#67332 = CARTESIAN_POINT ( 'NONE',  ( 14.92337183194729633, 47.67559781766745175, 8.527530157486181039 ) ) ;
#67333 = SURFACE_STYLE_USAGE ( .BOTH. , #66837 ) ;
#67334 = EDGE_CURVE ( 'NONE', #97012, #87349, #9109, .T. ) ;
#67335 = CARTESIAN_POINT ( 'NONE',  ( 2.791683348922237240, 25.38393115100078390, -7.208316651077763204 ) ) ;
#67336 = CARTESIAN_POINT ( 'NONE',  ( 10.00000000000000178, 12.25893115100078568, 9.846743663894594434 ) ) ;
#67338 = ORIENTED_EDGE ( 'NONE', *, *, #87033, .F. ) ;
#67337 = CARTESIAN_POINT ( 'NONE',  ( -2.816281873526473856, 9.123634669930421381, 9.499525473075851096E-16 ) ) ;
#67339 =( GEOMETRIC_REPRESENTATION_CONTEXT ( 3 ) GLOBAL_UNCERTAINTY_ASSIGNED_CONTEXT ( ( #92242 ) ) GLOBAL_UNIT_ASSIGNED_CONTEXT ( ( #4059, #65015, #28016 ) ) REPRESENTATION_CONTEXT ( 'NONE', 'WORKASPACE' ) );
#67340 = CARTESIAN_POINT ( 'NONE',  ( -10.82344394350238304, 14.95077488074853811, 10.02492699998869163 ) ) ;
#67341 = CARTESIAN_POINT ( 'NONE',  ( 0.000000000000000000, 0.000000000000000000, 0.000000000000000000 ) ) ;
#67342 = CARTESIAN_POINT ( 'NONE',  ( 0.2751277870542967463, 70.00000000000000000, -6.000000000000000000 ) ) ;
#67343 = CARTESIAN_POINT ( 'NONE',  ( 22.81628187352647785, 56.62363466993042493, 6.195893100308588602E-16 ) ) ;
#67344 = CARTESIAN_POINT ( 'NONE',  ( 18.52753015748617571, 33.09226448433411605, 4.923371831947298993 ) ) ;
#67345 = CARTESIAN_POINT ( 'NONE',  ( 6.660444548080930893, -84.28805632650643531, -2.500000000000001332 ) ) ;
#67346 = CARTESIAN_POINT ( 'NONE',  ( 10.00000000000000000, 11.81368534415483751, -10.88017736071110342 ) ) ;
#67347 = CARTESIAN_POINT ( 'NONE',  ( 19.84674366389459266, 28.30059781766745886, 2.638427012816836559 ) ) ;
#67348 = MECHANICAL_DESIGN_GEOMETRIC_PRESENTATION_REPRESENTATION (  '', ( #51358 ), #52997 ) ;
#67349 = CARTESIAN_POINT ( 'NONE',  ( 1.274849032794164172, 18.57228050351029935, 6.499999999999802824 ) ) ;
#67350 = CARTESIAN_POINT ( 'NONE',  ( 2.035157376598822676, 7.438685344154837509, -7.964842623401177768 ) ) ;
#67351 = FACE_OUTER_BOUND ( 'NONE', #4567, .T. ) ;
#67352 = CARTESIAN_POINT ( 'NONE',  ( 4.559911319644449179, 17.23035201082150536, -9.422509992056141925 ) ) ;
#67353 = CARTESIAN_POINT ( 'NONE',  ( 24.16423886937409904, 54.09541550158063217, 3.795296366450317205 ) ) ;
#67355 = FACE_OUTER_BOUND ( 'NONE', #18648, .T. ) ;
#67354 = CARTESIAN_POINT ( 'NONE',  ( 13.79529636645031943, 50.34541550158064638, -14.16423886937409904 ) ) ;
#67356 = CARTESIAN_POINT ( 'NONE',  ( -16.94000000000001549, 92.00000000000000000, -10.09898361729590199 ) ) ;
#67357 = VECTOR ( 'NONE', #39072, 1000.000000000000000 ) ;
#67358 = CARTESIAN_POINT ( 'NONE',  ( 2.791683348922237240, 30.38393115100078390, -7.208316651077763204 ) ) ;
#67359 = CARTESIAN_POINT ( 'NONE',  ( 17.20831665107776587, 62.88393115100078745, 7.208316651077764980 ) ) ;
#67360 = CARTESIAN_POINT ( 'NONE',  ( 2.603489959281588995, 40.43575266056827644, -6.500000000000003553 ) ) ;
#67361 = CARTESIAN_POINT ( 'NONE',  ( 2.791683348922237240, 55.38393115100078745, -7.208316651077763204 ) ) ;
#67362 = CARTESIAN_POINT ( 'NONE',  ( 10.83696084481538691, -98.17058944465519232, -3.750000000000000000 ) ) ;
#67363 = DIRECTION ( 'NONE',  ( 1.000000000000000000, 0.000000000000000000, 0.000000000000000000 ) ) ;
#67364 = CARTESIAN_POINT ( 'NONE',  ( 6.204703633549690345, 5.762082168247301794, -14.16423886937410259 ) ) ;
#67365 = CARTESIAN_POINT ( 'NONE',  ( 14.92337183194729988, 29.34226448433411960, -8.527530157486177487 ) ) ;
#67366 = LINE ( 'NONE', #21377, #57668 ) ;
#67367 = CARTESIAN_POINT ( 'NONE',  ( -4.164238869374099927, 37.01208216824731068, 3.795296366450308767 ) ) ;
#67368 = CARTESIAN_POINT ( 'NONE',  ( 0.1532563361054083140, 6.008931151000784787, 1.131784320476157264E-15 ) ) ;
#67370 = DIRECTION ( 'NONE',  ( 0.000000000000000000, -1.000000000000000000, 0.000000000000000000 ) ) ;
#67369 = CARTESIAN_POINT ( 'NONE',  ( 5.000000000000000888, 16.50982297312471303, -7.000000000000000000 ) ) ;
#67371 = CARTESIAN_POINT ( 'NONE',  ( 20.88017736071110519, 30.56368534415484106, 2.639326808657452039E-16 ) ) ;
#67372 = CARTESIAN_POINT ( 'NONE',  ( 22.81628187352648496, 41.83196800326375353, -3.434112377981050290 ) ) ;
#67373 = CARTESIAN_POINT ( 'NONE',  ( 0.5774900079438590739, 2.647018677488170990, -5.440088680355550821 ) ) ;
#67374 = CARTESIAN_POINT ( 'NONE',  ( 16.40814093676324603, 37.45696800326376064, -11.09922568453594671 ) ) ;
#67375 = CARTESIAN_POINT ( 'NONE',  ( 19.50000000000000355, 79.40087001978915282, 5.000000000000000000 ) ) ;
#67376 = ORIENTED_EDGE ( 'NONE', *, *, #66706, .F. ) ;
#67377 =( LENGTH_UNIT ( ) NAMED_UNIT ( * ) SI_UNIT ( .MILLI., .METRE. ) );
#67378 = CARTESIAN_POINT ( 'NONE',  ( 20.10421743870886857, 35.60736173766203194, -6.337391062633418670 ) ) ;
#67379 = CARTESIAN_POINT ( 'NONE',  ( 20.36894250292379738, 34.92874883491396076, -10.36894250292379027 ) ) ;
#67380 = CARTESIAN_POINT ( 'NONE',  ( 22.26659068614894466, 3.887082168247300906, 7.082119434687054849 ) ) ;
#67381 = CARTESIAN_POINT ( 'NONE',  ( 12.91533473730993009, 11.60535201082150536, -10.88017736071109987 ) ) ;
#67382 = CARTESIAN_POINT ( 'NONE',  ( 10.00000000000000000, 16.81368534415483751, -10.88017736071110342 ) ) ;
#67383 = LINE ( 'NONE', #52869, #92540 ) ;
#67384 = DIRECTION ( 'NONE',  ( -0.000000000000000000, -0.000000000000000000, 1.000000000000000000 ) ) ;
#67385 = CARTESIAN_POINT ( 'NONE',  ( 19.42250999205614193, 55.14701867748817676, 5.440088680355555262 ) ) ;
#67386 = CARTESIAN_POINT ( 'NONE',  ( 12.91533473730992121, 49.52201867748817676, 10.88017736071110164 ) ) ;
#67387 = CARTESIAN_POINT ( 'NONE',  ( 10.00000000000000000, 32.87363466993042493, -12.81628187352647608 ) ) ;
#67388 = CARTESIAN_POINT ( 'NONE',  ( -2.815433093577217161, 0.3639308411966859502, 14.73340885523751531 ) ) ;
#67389 = CARTESIAN_POINT ( 'NONE',  ( 20.10384461210890805, 26.74302437010793554, 6.337995344473785764 ) ) ;
#67390 = CARTESIAN_POINT ( 'NONE',  ( 14.92337183194729988, 29.34226448433411960, -8.527530157486177487 ) ) ;
#67391 = CARTESIAN_POINT ( 'NONE',  ( 15.44008868035555793, 56.39701867748817676, -9.422509992056140149 ) ) ;
#67392 = EDGE_CURVE ( 'NONE', #75686, #34469, #44215, .T. ) ;
#67393 = UNCERTAINTY_MEASURE_WITH_UNIT (LENGTH_MEASURE( 1.000000000000000082E-05 ), #19755, 'distance_accuracy_value', 'NONE');
#67394 = AXIS2_PLACEMENT_3D ( 'NONE', #21567, #82048, #37061 ) ;
#67395 = CARTESIAN_POINT ( 'NONE',  ( -2.816281873526473856, 19.12363466993042138, 9.499525473075851096E-16 ) ) ;
#67396 = SURFACE_SIDE_STYLE ('',( #67897 ) ) ;
#67397 = CARTESIAN_POINT ( 'NONE',  ( 4.559911319644449179, 3.897018677488170990, 9.422509992056141925 ) ) ;
#67398 = CARTESIAN_POINT ( 'NONE',  ( 7.361572987183170547, 37.05059781766744464, 9.846743663894590881 ) ) ;
#67399 = CARTESIAN_POINT ( 'NONE',  ( 13.43411237798105340, 55.58196800326374643, 12.81628187352647963 ) ) ;
#67400 = CARTESIAN_POINT ( 'NONE',  ( 0.1532563361054100626, 15.80059781766745353, -2.638427012816831230 ) ) ;
#67401 = CARTESIAN_POINT ( 'NONE',  ( -4.164238869374098151, 11.59541550158063217, -3.795296366450310543 ) ) ;
#67402 = CARTESIAN_POINT ( 'NONE',  ( 20.88017736071110164, 30.35535201082150891, 2.915334737309930979 ) ) ;
#67403 = CARTESIAN_POINT ( 'NONE',  ( 2.035157376598824452, 38.68868534415483396, 7.964842623401179544 ) ) ;
#67404 = FILL_AREA_STYLE_COLOUR ( '', #61619 ) ;
#67405 = CARTESIAN_POINT ( 'NONE',  ( 0.1532563361054082862, 41.21726448433411605, 2.638427012816831674 ) ) ;
#67406 = CARTESIAN_POINT ( 'NONE',  ( 0.5774900079438607392, 38.48035201082150536, 5.440088680355550821 ) ) ;
#67407 = CARTESIAN_POINT ( 'NONE',  ( 2.035157376598822676, 17.43868534415483751, -7.964842623401177768 ) ) ;
#67408 = ORIENTED_EDGE ( 'NONE', *, *, #4755, .T. ) ;
#67409 = EDGE_CURVE ( 'NONE', #97093, #55640, #2415, .T. ) ;
#67410 = CARTESIAN_POINT ( 'NONE',  ( 19.42250999205614548, 25.98035201082150891, -5.440088680355545492 ) ) ;
#67411 = CARTESIAN_POINT ( 'NONE',  ( 0.6178305044545838731, 39.74863466993041072, 9.382169495545420901 ) ) ;
#67412 = CARTESIAN_POINT ( 'NONE',  ( 15.44008868035555260, 29.73035201082150891, 9.422509992056143702 ) ) ;
#67414 = CARTESIAN_POINT ( 'NONE',  ( 2.035157376598824452, 38.68868534415483396, 7.964842623401179544 ) ) ;
#67413 = DIRECTION ( 'NONE',  ( 0.000000000000000000, 1.000000000000000000, 0.000000000000000000 ) ) ;
#67415 = AXIS2_PLACEMENT_3D ( 'NONE', #19238, #65212, #65710 ) ;
#67416 = ORIENTED_EDGE ( 'NONE', *, *, #56673, .F. ) ;
#67417 = CARTESIAN_POINT ( 'NONE',  ( 7.361572987183169658, 59.96726448433410894, -9.846743663894592657 ) ) ;
#67418 = CARTESIAN_POINT ( 'NONE',  ( 20.88017736071110875, 30.77201867748816966, -2.915334737309920765 ) ) ;
#67419 = DIRECTION ( 'NONE',  ( -1.000000000000000000, 0.000000000000000000, 0.000000000000000000 ) ) ;
#67420 = ADVANCED_FACE ( 'NONE', ( #54596 ), #18684, .T. ) ;
#67421 = CARTESIAN_POINT ( 'NONE',  ( 14.76100041229771342, 0.2306972965111887264, -2.313205896730830879 ) ) ;
#67422 = LINE ( 'NONE', #52416, #1406 ) ;
#67423 = CARTESIAN_POINT ( 'NONE',  ( -0.3689425029237881626, 42.42874883491396787, 10.36894250292379027 ) ) ;
#67424 = CARTESIAN_POINT ( 'NONE',  ( 4.559911319644449179, 48.89701867748817676, 9.422509992056141925 ) ) ;
#67425 = DIRECTION ( 'NONE',  ( 0.000000000000000000, 0.000000000000000000, 1.000000000000000000 ) ) ;
#67426 = VECTOR ( 'NONE', #65716, 1000.000000000000000 ) ;
#67427 = CARTESIAN_POINT ( 'NONE',  ( 4.267749253172103074, 0.000000000000000000, -3.394721039305288457 ) ) ;
#67428 = CARTESIAN_POINT ( 'NONE',  ( 0.1532563361054100626, 65.80059781766745175, -2.638427012816831230 ) ) ;
#67429 = VECTOR ( 'NONE', #29086, 1000.000000000000000 ) ;
#67430 = CARTESIAN_POINT ( 'NONE',  ( 70.00000000000000000, -4.073016716636387686E-15, -9.500000000000000000 ) ) ;
#67431 = CARTESIAN_POINT ( 'NONE',  ( 0.1532563361054083140, 16.00893115100078390, 1.131784320476157264E-15 ) ) ;
#67432 = EDGE_CURVE ( 'NONE', #5083, #89199, #61602, .T. ) ;
#67433 = ORIENTED_EDGE ( 'NONE', *, *, #59118, .T. ) ;
#67434 = AXIS2_PLACEMENT_3D ( 'NONE', #43547, #51053, #81543 ) ;
#67435 = CARTESIAN_POINT ( 'NONE',  ( 19.84674366389459266, 23.30059781766745530, 2.638427012816836559 ) ) ;
#67436 = CARTESIAN_POINT ( 'NONE',  ( -12.81628187352647252, -20.66803199673624292, 3.434112377981066722 ) ) ;
#67437 = AXIS2_PLACEMENT_3D ( 'NONE', #68978, #70451, #92935 ) ;
#67438 = CARTESIAN_POINT ( 'NONE',  ( 17.96484262340118221, 21.18868534415483396, -7.964842623401177768 ) ) ;
#67439 = CARTESIAN_POINT ( 'NONE',  ( 10.00000000000000178, 22.25893115100078745, 9.846743663894594434 ) ) ;
#67440 = DIRECTION ( 'NONE',  ( -1.000000000000000000, 0.000000000000000000, 0.000000000000000000 ) ) ;
#67441 = CARTESIAN_POINT ( 'NONE',  ( 6.565887622018943937, 10.16530133659708746, 12.81628187352647430 ) ) ;
#67443 = CARTESIAN_POINT ( 'NONE',  ( 2.035157376598822676, 62.43868534415483396, -7.964842623401177768 ) ) ;
#67442 = FACE_OUTER_BOUND ( 'NONE', #3480, .T. ) ;
#67445 = CARTESIAN_POINT ( 'NONE',  ( 10.00000000000000178, 4.313685344154837509, 10.88017736071110342 ) ) ;
#67444 = CARTESIAN_POINT ( 'NONE',  ( -0.8801773607111008646, 38.27201867748816255, 2.915334737309923430 ) ) ;
#67446 = CARTESIAN_POINT ( 'NONE',  ( 24.16423886937410614, 49.51208216824730357, -3.795296366450302550 ) ) ;
#67447 = CARTESIAN_POINT ( 'NONE',  ( 20.24186590665275531, 35.59014588040358262, -6.114288769123075618 ) ) ;
#67448 = EDGE_LOOP ( 'NONE', ( #62607, #60552, #60784, #64805 ) ) ;
#67449 = CARTESIAN_POINT ( 'NONE',  ( 22.81628187352647785, 11.62363466993042138, 6.195893100308588602E-16 ) ) ;
#67450 = CARTESIAN_POINT ( 'NONE',  ( 2.035157376598822676, 7.438685344154837509, -7.964842623401177768 ) ) ;
#67451 = CARTESIAN_POINT ( 'NONE',  ( 7.084665262690076126, 42.02201867748816966, -10.88017736071110164 ) ) ;
#67452 = LINE ( 'NONE', #44931, #79271 ) ;
#67453 = VERTEX_POINT ( 'NONE', #70112 ) ;
#67454 = CARTESIAN_POINT ( 'NONE',  ( 7.084665262690076126, 54.10535201082151247, 10.88017736071109987 ) ) ;
#67455 = CARTESIAN_POINT ( 'NONE',  ( 7.361572987183169658, 39.96726448433411605, -9.846743663894592657 ) ) ;
#67456 = CARTESIAN_POINT ( 'NONE',  ( 18.52753015748617571, 23.09226448433411960, 4.923371831947298993 ) ) ;
#67457 = CARTESIAN_POINT ( 'NONE',  ( 2.791683348922240793, 11.63393115100078568, 7.208316651077764092 ) ) ;
#67458 = CARTESIAN_POINT ( 'NONE',  ( -7.079903288604985079, -69.52484394646408816, 2.500000000000000000 ) ) ;
#67459 = EDGE_CURVE ( 'NONE', #77584, #48019, #62095, .T. ) ;
#67461 = FACE_BOUND ( 'NONE', #94356, .T. ) ;
#67460 = CARTESIAN_POINT ( 'NONE',  ( 19.84674366389459266, 3.300597817667451750, 2.638427012816836559 ) ) ;
#67462 = LINE ( 'NONE', #38448, #69716 ) ;
#67464 = VERTEX_POINT ( 'NONE', #1637 ) ;
#67463 = CARTESIAN_POINT ( 'NONE',  ( 14.92337183194729988, 29.34226448433411960, -8.527530157486177487 ) ) ;
#67465 = CARTESIAN_POINT ( 'NONE',  ( 0.6178305044545838731, 59.74863466993041783, 9.382169495545420901 ) ) ;
#67466 = AXIS2_PLACEMENT_3D ( 'NONE', #89451, #73449, #13450 ) ;
#67467 = CARTESIAN_POINT ( 'NONE',  ( 0.2849401152835440709, 0.2301503025712808848, 14.93790629078169019 ) ) ;
#67468 = CARTESIAN_POINT ( 'NONE',  ( 7.361572987183170547, 67.05059781766746596, 9.846743663894590881 ) ) ;
#67469 = CARTESIAN_POINT ( 'NONE',  ( -4.164238869374099039, 26.80374883491397142, 8.674139862899312516E-16 ) ) ;
#67470 =( BOUNDED_CURVE ( )  B_SPLINE_CURVE ( 2, ( #80696, #95190, #34188, #4715, #19698, #50690, #35177, #11704, #81183 ),
 .UNSPECIFIED., .F., .T. ) 
 B_SPLINE_CURVE_WITH_KNOTS ( ( 3, 2, 2, 2, 3 ),
 ( 0.01156950836880285202, 0.01190476190476197349, 0.01785714285714290472, 0.02380952380952383596, 0.02414477734548295743 ),
 .UNSPECIFIED. ) 
 CURVE ( )  GEOMETRIC_REPRESENTATION_ITEM ( )  RATIONAL_B_SPLINE_CURVE ( ( 0.9963778908391762723, 0.9980808541467921513, 1.000000000000000000, 0.9659258262890682012, 1.000000000000000000, 0.9659258262890682012, 1.000000000000000000, 0.9980808541467921513, 0.9963778908391762723 ) ) 
 REPRESENTATION_ITEM ( '' )  );
#67471 = UNCERTAINTY_MEASURE_WITH_UNIT (LENGTH_MEASURE( 1.000000000000000082E-05 ), #27736, 'distance_accuracy_value', 'NONE');
#67472 = CARTESIAN_POINT ( 'NONE',  ( -8.000343251535921851, 84.06932101904432386, 3.750000000000000000 ) ) ;
#67473 = CARTESIAN_POINT ( 'NONE',  ( 13.79529636645031943, 35.34541550158063927, -14.16423886937409904 ) ) ;
#67474 = EDGE_CURVE ( 'NONE', #5244, #22303, #23647, .T. ) ;
#67475 = CARTESIAN_POINT ( 'NONE',  ( 20.36894250292379382, 48.67874883491396076, 10.36894250292379205 ) ) ;
#67476 = CARTESIAN_POINT ( 'NONE',  ( 22.26659068614895176, 4.720415501580633943, -7.082119434687042414 ) ) ;
#67477 = CARTESIAN_POINT ( 'NONE',  ( -4.164238869374098151, 6.595415501580634832, -3.795296366450310543 ) ) ;
#67478 = CARTESIAN_POINT ( 'NONE',  ( 17.96484262340118221, 49.93868534415484106, 7.964842623401181321 ) ) ;
#67479 = CARTESIAN_POINT ( 'NONE',  ( 6.903457398626329677, -84.61157762779829739, -2.750000000000000000 ) ) ;
#67480 = CARTESIAN_POINT ( 'NONE',  ( 12.63842701281683922, 29.55059781766745175, -9.846743663894590881 ) ) ;
#67482 = CARTESIAN_POINT ( 'NONE',  ( 7.361572987183170547, 27.05059781766745175, 9.846743663894590881 ) ) ;
#67481 = CARTESIAN_POINT ( 'NONE',  ( -6.689969769699040114, 15.00000000000000000, 12.58200319823965785 ) ) ;
#67483 = CARTESIAN_POINT ( 'NONE',  ( 2.035157376598822676, 27.43868534415483396, -7.964842623401177768 ) ) ;
#67484 = CARTESIAN_POINT ( 'NONE',  ( 6.565887622018943937, 60.16530133659707502, 12.81628187352647430 ) ) ;
#67485 = CARTESIAN_POINT ( 'NONE',  ( 0.1532563361054083140, 61.00893115100078745, 1.131784320476157264E-15 ) ) ;
#67486 = DIRECTION ( 'NONE',  ( 0.000000000000000000, 0.000000000000000000, 1.000000000000000000 ) ) ;
#67487 = CARTESIAN_POINT ( 'NONE',  ( 12.63842701281683034, 32.46726448433412315, 9.846743663894596210 ) ) ;
#67488 = CARTESIAN_POINT ( 'NONE',  ( 19.38216949554541202, 45.99863466993041072, 9.382169495545424454 ) ) ;
#67489 = CARTESIAN_POINT ( 'NONE',  ( -14.16423886937410082, -23.19625116508602858, 4.336808689942017736E-15 ) ) ;
#67490 = AXIS2_PLACEMENT_3D ( 'NONE', #19915, #5428, #11924 ) ;
#67491 = CARTESIAN_POINT ( 'NONE',  ( 17.96484262340118221, 39.93868534415484106, 7.964842623401181321 ) ) ;
#67492 = CARTESIAN_POINT ( 'NONE',  ( 5.076628168052704559, 50.17559781766745886, -8.527530157486179263 ) ) ;
#67493 = CARTESIAN_POINT ( 'NONE',  ( -2.266590686148945544, 31.38708216824730002, -7.082119434687050408 ) ) ;
#67494 = VERTEX_POINT ( 'NONE', #46130 ) ;
#67495 = FACE_OUTER_BOUND ( 'NONE', #38067, .T. ) ;
#67496 = CARTESIAN_POINT ( 'NONE',  ( 17.96484262340118221, 64.93868534415483396, 7.964842623401181321 ) ) ;
#67497 = CARTESIAN_POINT ( 'NONE',  ( 19.42250999205614548, 60.98035201082151247, -5.440088680355545492 ) ) ;
#67498 = CARTESIAN_POINT ( 'NONE',  ( 20.36894250292379382, 63.67874883491396787, 10.36894250292379205 ) ) ;
#67499 = CARTESIAN_POINT ( 'NONE',  ( 0.1532563361054100626, 65.80059781766745175, -2.638427012816831230 ) ) ;
#67500 = CIRCLE ( 'NONE', #83487, 15.00000000000000000 ) ;
#67501 = DIRECTION ( 'NONE',  ( 0.000000000000000000, 0.000000000000000000, 1.000000000000000000 ) ) ;
#67502 = CARTESIAN_POINT ( 'NONE',  ( 4.559911319644449179, 48.89701867748817676, 9.422509992056141925 ) ) ;
#67503 = CARTESIAN_POINT ( 'NONE',  ( -0.7375392941519274270, 14.63595249122789177, 14.98185688723471110 ) ) ;
#67504 = CARTESIAN_POINT ( 'NONE',  ( 10.88017736071109987, 30.77201867748818032, -2.915334737309928315 ) ) ;
#67505 = CARTESIAN_POINT ( 'NONE',  ( -0.8801773607110991993, 7.855352010821504471, -2.915334737309923874 ) ) ;
#67507 =( GEOMETRIC_REPRESENTATION_CONTEXT ( 3 ) GLOBAL_UNCERTAINTY_ASSIGNED_CONTEXT ( ( #78102 ) ) GLOBAL_UNIT_ASSIGNED_CONTEXT ( ( #88765, #88270, #29246 ) ) REPRESENTATION_CONTEXT ( 'NONE', 'WORKASPACE' ) );
#67506 = CARTESIAN_POINT ( 'NONE',  ( 17.96484262340118221, 9.938685344154839285, 7.964842623401181321 ) ) ;
#67508 = CARTESIAN_POINT ( 'NONE',  ( 0.1532563361054083140, 56.00893115100078745, 1.131784320476157264E-15 ) ) ;
#67509 = CARTESIAN_POINT ( 'NONE',  ( 16.40814093676323893, 45.79030133659708923, 11.09922568453595026 ) ) ;
#67510 = CARTESIAN_POINT ( 'NONE',  ( -14.29730467489535428, 3.987535082655999417E-16, 2.416004766803123260 ) ) ;
#67511 = ORIENTED_EDGE ( 'NONE', *, *, #39579, .F. ) ;
#67512 = CARTESIAN_POINT ( 'NONE',  ( 10.00000000000000178, 14.31368534415483751, 10.88017736071110342 ) ) ;
#67513 = ADVANCED_FACE ( 'NONE', ( #32088 ), #62586, .T. ) ;
#67514 = CARTESIAN_POINT ( 'NONE',  ( 22.81628187352647785, 16.62363466993042138, 6.195893100308588602E-16 ) ) ;
#67515 = DIRECTION ( 'NONE',  ( 0.000000000000000000, 1.000000000000000000, 0.000000000000000000 ) ) ;
#67516 = AXIS2_PLACEMENT_3D ( 'NONE', #34548, #56102, #57555 ) ;
#67517 = CARTESIAN_POINT ( 'NONE',  ( 10.00000000000000178, 17.25893115100078745, 9.846743663894594434 ) ) ;
#67518 = CARTESIAN_POINT ( 'NONE',  ( 19.84674366389459266, 53.71726448433411605, -2.638427012816827677 ) ) ;
#67519 = ADVANCED_FACE ( 'NONE', ( #77107 ), #54107, .F. ) ;
#67520 = CARTESIAN_POINT ( 'NONE',  ( -0.8801773607111009756, 38.06368534415484106, 1.068504757029289695E-15 ) ) ;
#67521 = CARTESIAN_POINT ( 'NONE',  ( 21.09922568453595559, 7.040301336597086568, -6.408140936763230044 ) ) ;
#67523 = CARTESIAN_POINT ( 'NONE',  ( 17.97699586832901986, 91.14602379785867470, 8.000000000000000000 ) ) ;
#67522 = CARTESIAN_POINT ( 'NONE',  ( 15.44008868035555260, 54.73035201082150536, 9.422509992056143702 ) ) ;
#67524 =( NAMED_UNIT ( * ) PLANE_ANGLE_UNIT ( ) SI_UNIT ( $, .RADIAN. ) );
#67525 = CARTESIAN_POINT ( 'NONE',  ( 6.565887622018943937, 58.08196800326376064, -12.81628187352647608 ) ) ;
#67526 = ORIENTED_EDGE ( 'NONE', *, *, #96791, .F. ) ;
#67527 = CARTESIAN_POINT ( 'NONE',  ( 15.44008868035555793, 61.39701867748817676, -9.422509992056140149 ) ) ;
#67529 = CARTESIAN_POINT ( 'NONE',  ( 17.08211943468705840, 5.137082168247300906, -12.26659068614894466 ) ) ;
#67528 = CARTESIAN_POINT ( 'NONE',  ( 22.81628187352648496, 31.83196800326375353, -3.434112377981050290 ) ) ;
#67530 = CARTESIAN_POINT ( 'NONE',  ( 18.52753015748618282, 8.925597817667451750, -4.923371831947291888 ) ) ;
#67531 = CARTESIAN_POINT ( 'NONE',  ( 15.44008868035555260, 34.73035201082151247, 9.422509992056143702 ) ) ;
#67532 = CARTESIAN_POINT ( 'NONE',  ( -11.36220558718869711, 4.706058445226104967E-16, 9.008345252845160189 ) ) ;
#67533 = STYLED_ITEM ( 'NONE', ( #71879 ), #9051 ) ;
#67534 = LINE ( 'NONE', #45011, #19453 ) ;
#67535 = CARTESIAN_POINT ( 'NONE',  ( 1.472469842513823179, 10.59226448433411782, -4.923371831947296329 ) ) ;
#67536 = CARTESIAN_POINT ( 'NONE',  ( 12.63842701281683922, 9.550597817667449974, -9.846743663894590881 ) ) ;
#67537 = LINE ( 'NONE', #97069, #45810 ) ;
#67538 = CARTESIAN_POINT ( 'NONE',  ( 10.00000000000000000, 40.55374883491397497, -14.16423886937410082 ) ) ;
#67539 = EDGE_CURVE ( 'NONE', #45712, #14534, #47435, .T. ) ;
#67540 = DIRECTION ( 'NONE',  ( -1.000000000000000000, 5.782411586589362323E-17, -0.000000000000000000 ) ) ;
#67541 = CARTESIAN_POINT ( 'NONE',  ( 11.44532407938881136, -77.50611495452966437, -3.750000000000000000 ) ) ;
#67542 = CARTESIAN_POINT ( 'NONE',  ( -5.331138373842556177, -28.69357394138843986, -4.000000000001612932 ) ) ;
#67543 = ORIENTED_EDGE ( 'NONE', *, *, #13905, .T. ) ;
#67544 = TOROIDAL_SURFACE ( 'NONE', #57956, 14.49999999999999822, 0.5000000000000000000 ) ;
#67545 = CARTESIAN_POINT ( 'NONE',  ( 2.917880565312950480, 65.97041550158063217, -12.26659068614894821 ) ) ;
#67546 = CARTESIAN_POINT ( 'NONE',  ( 10.00000000000000178, 58.05374883491397497, 14.16423886937410082 ) ) ;
#67547 = CARTESIAN_POINT ( 'NONE',  ( 0.1532563361054100626, 25.80059781766744820, -2.638427012816831230 ) ) ;
#67548 = EDGE_CURVE ( 'NONE', #40259, #29043, #55438, .T. ) ;
#67549 = CARTESIAN_POINT ( 'NONE',  ( -2.816281873526473856, 29.33196800326376064, 3.434112377981055619 ) ) ;
#67550 = CARTESIAN_POINT ( 'NONE',  ( 8.879999999999991900, 20.99999999999999645, 0.000000000000000000 ) ) ;
#67552 = CARTESIAN_POINT ( 'NONE',  ( -4.164238869374099039, 6.803748834913967869, 8.674139862899312516E-16 ) ) ;
#67551 = CARTESIAN_POINT ( 'NONE',  ( -8.854007681965594401, 87.37522428062922586, -4.483348028979307287 ) ) ;
#67553 = CARTESIAN_POINT ( 'NONE',  ( 2.035157376598824452, 13.68868534415483751, 7.964842623401179544 ) ) ;
#67554 = CARTESIAN_POINT ( 'NONE',  ( 17.08211943468705840, 60.13708216824729647, -12.26659068614894466 ) ) ;
#67555 = CARTESIAN_POINT ( 'NONE',  ( 0.1532563361054100626, 30.80059781766744820, -2.638427012816831230 ) ) ;
#67556 = FACE_OUTER_BOUND ( 'NONE', #63362, .T. ) ;
#67557 = CARTESIAN_POINT ( 'NONE',  ( 19.84674366389459266, 28.71726448433411960, -2.638427012816827677 ) ) ;
#67558 = EDGE_CURVE ( 'NONE', #952, #28596, #87076, .T. ) ;
#67559 = DIRECTION ( 'NONE',  ( 0.000000000000000000, 1.000000000000000000, 0.000000000000000000 ) ) ;
#67560 = CARTESIAN_POINT ( 'NONE',  ( 8.527530157486179263, 18.09226448433412671, 4.923371831947292776 ) ) ;
#67561 = ORIENTED_EDGE ( 'NONE', *, *, #88395, .F. ) ;
#67562 = ORIENTED_EDGE ( 'NONE', *, *, #27998, .T. ) ;
#67563 = DIRECTION ( 'NONE',  ( -0.8320502943378437211, 0.5547001962252290364, 0.000000000000000000 ) ) ;
#67564 = ORIENTED_EDGE ( 'NONE', *, *, #85065, .F. ) ;
#67565 = CARTESIAN_POINT ( 'NONE',  ( 7.361572987183169658, 49.96726448433410894, -9.846743663894592657 ) ) ;
#67566 = CARTESIAN_POINT ( 'NONE',  ( 2.917880565312950480, 20.97041550158063217, -12.26659068614894821 ) ) ;
#67568 = CARTESIAN_POINT ( 'NONE',  ( 17.96484262340118221, 44.93868534415483396, 7.964842623401181321 ) ) ;
#67567 = CARTESIAN_POINT ( 'NONE',  ( 0.5774900079438607392, 38.48035201082150536, 5.440088680355550821 ) ) ;
#67570 = CARTESIAN_POINT ( 'NONE',  ( 21.09922568453594849, 11.20696800326375531, 6.408140936763242479 ) ) ;
#67569 = CARTESIAN_POINT ( 'NONE',  ( 7.361572987183170547, 67.05059781766746596, 9.846743663894590881 ) ) ;
#67571 =( LENGTH_UNIT ( ) NAMED_UNIT ( * ) SI_UNIT ( .MILLI., .METRE. ) );
#67572 = CIRCLE ( 'NONE', #6895, 15.00000000000000000 ) ;
#67573 = CARTESIAN_POINT ( 'NONE',  ( -2.816281873526473856, 29.12363466993041783, 9.499525473075851096E-16 ) ) ;
#67574 = ORIENTED_EDGE ( 'NONE', *, *, #17170, .T. ) ;
#67575 = CIRCLE ( 'NONE', #93107, 14.49999999999999822 ) ;
#67576 = CARTESIAN_POINT ( 'NONE',  ( 0.1532563361054100626, 45.80059781766745886, -2.638427012816831230 ) ) ;
#67577 = VECTOR ( 'NONE', #74752, 1000.000000000000000 ) ;
#67578 = CARTESIAN_POINT ( 'NONE',  ( 7.084665262690076126, 4.105352010821503583, 10.88017736071109987 ) ) ;
#67579 = ORIENTED_EDGE ( 'NONE', *, *, #32559, .T. ) ;
#67580 = PRESENTATION_LAYER_ASSIGNMENT (  '', '', ( #6909 ) ) ;
#67581 = CARTESIAN_POINT ( 'NONE',  ( 17.96484262340118221, 21.18868534415483396, -7.964842623401177768 ) ) ;
#67582 = VERTEX_POINT ( 'NONE', #73043 ) ;
#67583 = CARTESIAN_POINT ( 'NONE',  ( 12.91533473730992121, 44.52201867748816966, 10.88017736071110164 ) ) ;
#67584 = CARTESIAN_POINT ( 'NONE',  ( 7.084665262690076126, 54.10535201082151247, 10.88017736071109987 ) ) ;
#67585 = CARTESIAN_POINT ( 'NONE',  ( 15.44008868035555260, 59.73035201082151247, 9.422509992056143702 ) ) ;
#67586 = CARTESIAN_POINT ( 'NONE',  ( 14.92337183194729633, 2.675597817667451750, 8.527530157486181039 ) ) ;
#67587 = CARTESIAN_POINT ( 'NONE',  ( 20.88017736071110875, 50.77201867748817676, -2.915334737309920765 ) ) ;
#67588 = CARTESIAN_POINT ( 'NONE',  ( -0.2418659066527494572, 29.26028685723174050, -6.114288769123083611 ) ) ;
#67589 = EDGE_CURVE ( 'NONE', #86221, #8055, #69790, .T. ) ;
#67590 = CARTESIAN_POINT ( 'NONE',  ( 9.261744320279156284, -15.50732398184426764, 3.999999999999999112 ) ) ;
#67591 = CARTESIAN_POINT ( 'NONE',  ( 7.361572987183170547, 22.05059781766745530, 9.846743663894590881 ) ) ;
#67592 = ORIENTED_EDGE ( 'NONE', *, *, #91159, .F. ) ;
#67593 = DIRECTION ( 'NONE',  ( -0.07626964003977962370, 0.9970872288863209532, 0.000000000000000000 ) ) ;
#67594 =( NAMED_UNIT ( * ) SI_UNIT ( $, .STERADIAN. ) SOLID_ANGLE_UNIT ( ) );
#67595 = CARTESIAN_POINT ( 'NONE',  ( 20.36894250292379738, 4.928748834913967869, -10.36894250292379027 ) ) ;
#67596 = ORIENTED_EDGE ( 'NONE', *, *, #45451, .F. ) ;
#67597 = CARTESIAN_POINT ( 'NONE',  ( -11.05007230724497092, 12.65949770494214377, -2.855270967710901164 ) ) ;
#67598 = CARTESIAN_POINT ( 'NONE',  ( 19.72487221294570858, 29.78217586085238366, 6.499999999999992895 ) ) ;
#67599 = DIRECTION ( 'NONE',  ( 0.000000000000000000, 0.000000000000000000, 1.000000000000000000 ) ) ;
#67600 = CARTESIAN_POINT ( 'NONE',  ( -0.8801773607111009756, 13.06368534415483929, 1.068504757029289695E-15 ) ) ;
#67601 = LINE ( 'NONE', #50615, #16324 ) ;
#67602 = ORIENTED_EDGE ( 'NONE', *, *, #19427, .T. ) ;
#67603 = CARTESIAN_POINT ( 'NONE',  ( 11.42891328973224141, -3.217031133671831504E-15, -9.126250717928387601 ) ) ;
#67604 = CARTESIAN_POINT ( 'NONE',  ( 19.84674366389459266, 48.30059781766745175, 2.638427012816836559 ) ) ;
#67605 = DIRECTION ( 'NONE',  ( -0.000000000000000000, -1.000000000000000000, -0.000000000000000000 ) ) ;
#67607 = VECTOR ( 'NONE', #95657, 1000.000000000000000 ) ;
#67606 = CARTESIAN_POINT ( 'NONE',  ( 16.40814093676323893, 15.79030133659708746, 11.09922568453595026 ) ) ;
#67608 = CARTESIAN_POINT ( 'NONE',  ( 7.361572987183170547, 12.05059781766744997, 9.846743663894590881 ) ) ;
#67609 = CARTESIAN_POINT ( 'NONE',  ( 1.821158202401484294, 36.16688879859522388, 6.499999999999917399 ) ) ;
#67610 = CARTESIAN_POINT ( 'NONE',  ( 5.076628168052704559, 20.17559781766745175, -8.527530157486179263 ) ) ;
#67611 = CARTESIAN_POINT ( 'NONE',  ( 3.591859063236763294, -1.709698663402913210, -11.09922568453595026 ) ) ;
#67612 = CARTESIAN_POINT ( 'NONE',  ( 3.420591144908545100, 15.00000000000000000, -14.60477854057955938 ) ) ;
#67613 = AXIS2_PLACEMENT_3D ( 'NONE', #6957, #21467, #69426 ) ;
#67614 = ORIENTED_EDGE ( 'NONE', *, *, #13242, .F. ) ;
#67615 = CARTESIAN_POINT ( 'NONE',  ( -0.8801773607110991993, 27.85535201082150181, -2.915334737309923874 ) ) ;
#67616 = CARTESIAN_POINT ( 'NONE',  ( 2.917880565312950480, 15.97041550158063217, -12.26659068614894821 ) ) ;
#67617 = CARTESIAN_POINT ( 'NONE',  ( 18.52753015748618282, 33.92559781766745886, -4.923371831947291888 ) ) ;
#67618 = CARTESIAN_POINT ( 'NONE',  ( 19.42250999205614548, 55.98035201082150536, -5.440088680355545492 ) ) ;
#67620 = CARTESIAN_POINT ( 'NONE',  ( -3.711005778769052021, -5.293034685380286319, -2.750000000000000444 ) ) ;
#67619 = CARTESIAN_POINT ( 'NONE',  ( 19.38216949554541202, 40.99863466993042493, 9.382169495545424454 ) ) ;
#67621 = CARTESIAN_POINT ( 'NONE',  ( 0.5774900079438607392, 13.48035201082150358, 5.440088680355550821 ) ) ;
#67622 = CARTESIAN_POINT ( 'NONE',  ( 6.898461952320431578, 15.00000000000000000, -12.75387089053309175 ) ) ;
#67623 = CARTESIAN_POINT ( 'NONE',  ( 12.98685442714775640, 15.00000000000000000, 6.449155920607609893 ) ) ;
#67624 = CARTESIAN_POINT ( 'NONE',  ( 10.00000000000000178, 10.37363466993041961, 12.81628187352647608 ) ) ;
#67625 = CARTESIAN_POINT ( 'NONE',  ( 7.361572987183170547, 67.05059781766746596, 9.846743663894590881 ) ) ;
#67626 = CARTESIAN_POINT ( 'NONE',  ( 12.63842701281683034, 32.46726448433412315, 9.846743663894596210 ) ) ;
#67627 = CARTESIAN_POINT ( 'NONE',  ( -5.440088680355547268, -16.10298132251182324, 9.422509992056143702 ) ) ;
#67628 = CARTESIAN_POINT ( 'NONE',  ( 22.81628187352648496, 36.83196800326376064, -3.434112377981050290 ) ) ;
#67629 = FACE_OUTER_BOUND ( 'NONE', #48611, .T. ) ;
#67631 = CARTESIAN_POINT ( 'NONE',  ( 11.81378540890936080, 15.00000000000000000, -7.968498874458115999 ) ) ;
#67630 = CARTESIAN_POINT ( 'NONE',  ( 20.88017736071110519, 40.56368534415484106, 2.639326808657452039E-16 ) ) ;
#67632 = CARTESIAN_POINT ( 'NONE',  ( 0.000000000000000000, 0.000000000000000000, 0.000000000000000000 ) ) ;
#67633 = CARTESIAN_POINT ( 'NONE',  ( 8.879999999999999005, 20.99999999999999645, 0.000000000000000000 ) ) ;
#67634 = CARTESIAN_POINT ( 'NONE',  ( 7.084665262690076126, 47.02201867748818387, -10.88017736071110164 ) ) ;
#67635 = EDGE_CURVE ( 'NONE', #49672, #68696, #88265, .T. ) ;
#67636 = CARTESIAN_POINT ( 'NONE',  ( 4.559911319644449179, 43.89701867748816966, 9.422509992056141925 ) ) ;
#67637 = CARTESIAN_POINT ( 'NONE',  ( 1.472469842513823179, 65.59226448433412315, -4.923371831947296329 ) ) ;
#67638 = CARTESIAN_POINT ( 'NONE',  ( 20.88017736071110164, 65.35535201082150536, 2.915334737309930979 ) ) ;
#67639 = VECTOR ( 'NONE', #16354, 1000.000000000000000 ) ;
#67640 = EDGE_CURVE ( 'NONE', #53171, #15924, #36233, .T. ) ;
#67641 = EDGE_CURVE ( 'NONE', #47206, #50542, #7577, .T. ) ;
#67642 = TOROIDAL_SURFACE ( 'NONE', #11739, 7.538348415311010520, 7.000000000000000000 ) ;
#67643 = CARTESIAN_POINT ( 'NONE',  ( 19.84674366389459621, 38.50893115100078745, 7.409399052514197653E-17 ) ) ;
#67644 = CARTESIAN_POINT ( 'NONE',  ( 19.42250999205614193, 10.14701867748816966, 5.440088680355555262 ) ) ;
#67645 = CARTESIAN_POINT ( 'NONE',  ( 19.38216949554541202, 15.99863466993042138, 9.382169495545424454 ) ) ;
#67646 = ORIENTED_EDGE ( 'NONE', *, *, #28961, .T. ) ;
#67647 = CARTESIAN_POINT ( 'NONE',  ( -0.8801773607111008646, 28.27201867748817321, 2.915334737309923430 ) ) ;
#67648 = VECTOR ( 'NONE', #56461, 1000.000000000000000 ) ;
#67649 = DIRECTION ( 'NONE',  ( 0.8070303256584299145, -0.5905099943842175847, 0.000000000000000000 ) ) ;
#67650 = CARTESIAN_POINT ( 'NONE',  ( -0.8801773607111009756, 28.06368534415484106, 1.068504757029289695E-15 ) ) ;
#67651 = CARTESIAN_POINT ( 'NONE',  ( 18.52753015748618282, 3.925597817667451306, -4.923371831947291888 ) ) ;
#67652 = CARTESIAN_POINT ( 'NONE',  ( 22.26659068614894466, 43.88708216824729647, 7.082119434687054849 ) ) ;
#67653 = CARTESIAN_POINT ( 'NONE',  ( 14.92337183194729633, 12.67559781766745353, 8.527530157486181039 ) ) ;
#67654 = CARTESIAN_POINT ( 'NONE',  ( 20.88017736071110875, 40.77201867748818387, -2.915334737309920765 ) ) ;
#67655 = CARTESIAN_POINT ( 'NONE',  ( 64.56412365047461321, 29.00000000000000355, -7.000000000000000000 ) ) ;
#67656 = CARTESIAN_POINT ( 'NONE',  ( -4.164238869374099927, 2.012082168247300906, 3.795296366450308767 ) ) ;
#67657 = VERTEX_POINT ( 'NONE', #34544 ) ;
#67658 = FACE_BOUND ( 'NONE', #84952, .T. ) ;
#67659 = CARTESIAN_POINT ( 'NONE',  ( 17.20831665107776587, 52.88393115100078035, 7.208316651077764980 ) ) ;
#67660 = EDGE_LOOP ( 'NONE', ( #20711, #75078, #56149, #32153, #12109, #35567 ) ) ;
#67661 = ORIENTED_EDGE ( 'NONE', *, *, #54940, .T. ) ;
#67662 = DIRECTION ( 'NONE',  ( 1.000000000000000000, 0.000000000000000000, 0.000000000000000000 ) ) ;
#67663 = CARTESIAN_POINT ( 'NONE',  ( 10.00000000000000000, 25.55374883491396787, -14.16423886937410082 ) ) ;
#67664 = CARTESIAN_POINT ( 'NONE',  ( -0.3689425029237898834, 21.17874883491396432, -10.36894250292378850 ) ) ;
#67665 = CARTESIAN_POINT ( 'NONE',  ( 7.084665262690076126, 62.02201867748816966, -10.88017736071110164 ) ) ;
#67666 = CARTESIAN_POINT ( 'NONE',  ( 10.00000000000000178, 4.313685344154837509, 10.88017736071110342 ) ) ;
#67667 = CARTESIAN_POINT ( 'NONE',  ( 13.43411237798105340, 5.581968003263753531, 12.81628187352647963 ) ) ;
#67668 = CARTESIAN_POINT ( 'NONE',  ( 0.1532563361054100626, 45.80059781766745886, -2.638427012816831230 ) ) ;
#67669 = CARTESIAN_POINT ( 'NONE',  ( -8.081444665679372363, -7.288330178580077146, 4.000000000000000000 ) ) ;
#67671 = CARTESIAN_POINT ( 'NONE',  ( 19.38216949554541202, 10.99863466993042138, 9.382169495545424454 ) ) ;
#67670 = CARTESIAN_POINT ( 'NONE',  ( 7.084665262690076126, 42.02201867748816966, -10.88017736071110164 ) ) ;
#67672 = CARTESIAN_POINT ( 'NONE',  ( 10.00000000000000178, 13.05374883491396787, 14.16423886937410082 ) ) ;
#67673 = CARTESIAN_POINT ( 'NONE',  ( 20.88017736071110875, 15.77201867748817143, -2.915334737309920765 ) ) ;
#67674 = CARTESIAN_POINT ( 'NONE',  ( 7.084665262690076126, 14.10535201082150358, 10.88017736071109987 ) ) ;
#67675 = CARTESIAN_POINT ( 'NONE',  ( 19.84674366389459266, 53.30059781766744464, 2.638427012816836559 ) ) ;
#67676 = CARTESIAN_POINT ( 'NONE',  ( 4.559911319644449179, 57.23035201082150536, -9.422509992056141925 ) ) ;
#67677 = EDGE_CURVE ( 'NONE', #67800, #35833, #94087, .T. ) ;
#67678 = CARTESIAN_POINT ( 'NONE',  ( -4.923371831947292776, -23.15773551566587685, 8.527530157486181039 ) ) ;
#67679 = ORIENTED_EDGE ( 'NONE', *, *, #32736, .T. ) ;
#67680 = DIRECTION ( 'NONE',  ( -0.5547001962252291474, -0.8320502943378437211, -0.000000000000000000 ) ) ;
#67681 = ORIENTED_EDGE ( 'NONE', *, *, #61311, .F. ) ;
#67682 = FILL_AREA_STYLE ('',( #35313 ) ) ;
#67683 = CARTESIAN_POINT ( 'NONE',  ( 10.00000000000000178, 32.25893115100078745, 9.846743663894594434 ) ) ;
#67684 = ORIENTED_EDGE ( 'NONE', *, *, #54300, .F. ) ;
#67685 = CARTESIAN_POINT ( 'NONE',  ( 0.000000000000000000, 12.49999999999999112, 11.25000000000000178 ) ) ;
#67687 = CARTESIAN_POINT ( 'NONE',  ( 2.035157376598822676, 2.438685344154838397, -7.964842623401177768 ) ) ;
#67686 = CARTESIAN_POINT ( 'NONE',  ( 6.204703633549690345, 42.84541550158063217, 14.16423886937410082 ) ) ;
#67689 = CARTESIAN_POINT ( 'NONE',  ( 0.1532563361054083140, 51.00893115100078745, 1.131784320476157264E-15 ) ) ;
#67688 = CARTESIAN_POINT ( 'NONE',  ( 7.361572987183170547, 22.05059781766745530, 9.846743663894590881 ) ) ;
#67690 = EDGE_CURVE ( 'NONE', #69690, #89907, #17128, .T. ) ;
#67691 = CARTESIAN_POINT ( 'NONE',  ( 17.20831665107776587, 4.133931151000785675, -7.208316651077762316 ) ) ;
#67692 = CARTESIAN_POINT ( 'NONE',  ( 3.469446951953614189E-15, 15.37363466993042849, 12.81628187352647608 ) ) ;
#67693 = ORIENTED_EDGE ( 'NONE', *, *, #9140, .T. ) ;
#67694 = CARTESIAN_POINT ( 'NONE',  ( 17.08211943468705130, 38.47041550158063217, 12.26659068614894998 ) ) ;
#67695 = CARTESIAN_POINT ( 'NONE',  ( -1.099225684535947600, 19.54030133659708568, 6.408140936763237150 ) ) ;
#67696 = EDGE_LOOP ( 'NONE', ( #8012, #169, #39549, #59422, #18406, #76870 ) ) ;
#67697 = CARTESIAN_POINT ( 'NONE',  ( -2.816281873526473856, 64.33196800326376774, 3.434112377981055619 ) ) ;
#67698 = CARTESIAN_POINT ( 'NONE',  ( 20.88017736071110519, 30.56368534415484106, 2.639326808657452039E-16 ) ) ;
#67699 = CARTESIAN_POINT ( 'NONE',  ( 0.1532563361054082862, 41.21726448433411605, 2.638427012816831674 ) ) ;
#67700 = CARTESIAN_POINT ( 'NONE',  ( 15.44008868035555793, 31.39701867748817676, -9.422509992056140149 ) ) ;
#67701 = CARTESIAN_POINT ( 'NONE',  ( 10.00000000000000178, 60.37363466993041783, 12.81628187352647608 ) ) ;
#67702 = DIRECTION ( 'NONE',  ( -0.000000000000000000, 1.000000000000000000, -0.000000000000000000 ) ) ;
#67703 = CARTESIAN_POINT ( 'NONE',  ( 19.84674366389459266, 43.30059781766744464, 2.638427012816836559 ) ) ;
#67704 = CARTESIAN_POINT ( 'NONE',  ( 0.1532563361054083140, 46.00893115100079456, 1.131784320476157264E-15 ) ) ;
#67705 = DIRECTION ( 'NONE',  ( 0.000000000000000000, 0.000000000000000000, 1.000000000000000000 ) ) ;
#67706 = CIRCLE ( 'NONE', #66050, 2.000000000000001776 ) ;
#67707 = CARTESIAN_POINT ( 'NONE',  ( -3.420591144908350589, 15.00000000000000000, -14.60477854057960556 ) ) ;
#67708 = CARTESIAN_POINT ( 'NONE',  ( -8.839000071696917260, 0.04962890530003090384, -11.81225584161653330 ) ) ;
#67709 = DIRECTION ( 'NONE',  ( 0.000000000000000000, 1.000000000000000000, 0.000000000000000000 ) ) ;
#67710 = CARTESIAN_POINT ( 'NONE',  ( 19.84674366389459266, 18.71726448433411960, -2.638427012816827677 ) ) ;
#67711 = CARTESIAN_POINT ( 'NONE',  ( -2.816281873526471635, 38.91530133659708213, -3.434112377981056508 ) ) ;
#67713 = CARTESIAN_POINT ( 'NONE',  ( 0.000000000000000000, 14.49999999999999822, 0.000000000000000000 ) ) ;
#67712 = AXIS2_PLACEMENT_3D ( 'NONE', #72875, #11398, #41921 ) ;
#67714 = ORIENTED_EDGE ( 'NONE', *, *, #58022, .T. ) ;
#67715 = CARTESIAN_POINT ( 'NONE',  ( 0.1532563361054100626, 55.80059781766745175, -2.638427012816831230 ) ) ;
#67716 = DIRECTION ( 'NONE',  ( 0.000000000000000000, 0.000000000000000000, 1.000000000000000000 ) ) ;
#67717 = CARTESIAN_POINT ( 'NONE',  ( 18.52753015748618282, 43.92559781766745175, -4.923371831947291888 ) ) ;
#67718 = CARTESIAN_POINT ( 'NONE',  ( -4.164238869374099927, 37.01208216824731068, 3.795296366450308767 ) ) ;
#67719 = CARTESIAN_POINT ( 'NONE',  ( 0.1532563361054100626, 40.80059781766745886, -2.638427012816831230 ) ) ;
#67720 = B_SPLINE_CURVE_WITH_KNOTS ( 'NONE', 3,
 ( #21337, #27835, #51827, #74817, #58321, #44316, #4374, #88839, #20347, #59807 ),
 .UNSPECIFIED., .F., .F.,
 ( 4, 2, 2, 2, 4 ),
 ( 1.177569344012831190E-16, 0.001974336156922556259, 0.002961504235383763048, 0.003455088274614364924, 0.003948672313844965934 ),
 .UNSPECIFIED. ) ;
#67721 = CARTESIAN_POINT ( 'NONE',  ( 10.00000000000000000, 52.87363466993041783, -12.81628187352647608 ) ) ;
#67722 = CARTESIAN_POINT ( 'NONE',  ( -3.750000000000000000, 10.00000000000000000, 2.500000000000000000 ) ) ;
#67723 = CARTESIAN_POINT ( 'NONE',  ( 19.84674366389459266, 8.300597817667451750, 2.638427012816836559 ) ) ;
#67724 = CARTESIAN_POINT ( 'NONE',  ( 17.08211943468705840, 5.137082168247300906, -12.26659068614894466 ) ) ;
#67725 = EDGE_CURVE ( 'NONE', #40043, #30756, #37901, .T. ) ;
#67726 = CARTESIAN_POINT ( 'NONE',  ( 7.361572987183169658, 49.96726448433410894, -9.846743663894592657 ) ) ;
#67727 = CARTESIAN_POINT ( 'NONE',  ( 19.42250999205614193, 45.14701867748817676, 5.440088680355555262 ) ) ;
#67728 = CARTESIAN_POINT ( 'NONE',  ( 19.84674366389459266, 43.30059781766744464, 2.638427012816836559 ) ) ;
#67729 = CARTESIAN_POINT ( 'NONE',  ( 8.879999999999991900, 20.99999999999999645, -1.249999999999987121 ) ) ;
#67730 = B_SPLINE_CURVE_WITH_KNOTS ( 'NONE', 3,
 ( #17998, #80462, #87951, #78493, #25988, #48480, #40509, #10007, #86971, #32983, #63485, #10489, #3491, #93989, #41000, #71499, #49957, #56962, #33461, #63958, #18484, #87463, #18978, #49457, #79962, #11466, #35935, #5947, #36437, #14437 ),
 .UNSPECIFIED., .F., .F.,
 ( 4, 2, 2, 2, 2, 2, 2, 2, 2, 2, 2, 2, 2, 2, 4 ),
 ( -6.000000000268970806E-08, 0.003118256826059614614, 0.006236573652119231474, 0.01247320730423846606, 0.02494647460847693524, 0.03741974191271540962, 0.04989300921695387359, 0.06236627652119233756, 0.07483954382543078765, 0.08107617747755001270, 0.08731281112966925162, 0.09354944478178846279, 0.09666776160784808225, 0.09822692002087787810, 0.09978607843390764620 ),
 .UNSPECIFIED. ) ;
#67731 = CARTESIAN_POINT ( 'NONE',  ( 20.88017736071110875, 50.77201867748817676, -2.915334737309920765 ) ) ;
#67732 = ORIENTED_EDGE ( 'NONE', *, *, #47320, .T. ) ;
#67733 = CARTESIAN_POINT ( 'NONE',  ( 1.707155281725172502, 52.90189080397286148, 6.499999999999955591 ) ) ;
#67734 = CARTESIAN_POINT ( 'NONE',  ( 2.035157376598824452, 13.68868534415483751, 7.964842623401179544 ) ) ;
#67736 = CARTESIAN_POINT ( 'NONE',  ( 12.91533473730992121, 49.52201867748817676, 10.88017736071110164 ) ) ;
#67735 = CARTESIAN_POINT ( 'NONE',  ( 6.565887622018943937, 0.1653013365970866511, 12.81628187352647430 ) ) ;
#67737 = CARTESIAN_POINT ( 'NONE',  ( 0.000000000000000000, 14.49999999999999822, 0.000000000000000000 ) ) ;
#67738 = LINE ( 'NONE', #62175, #44356 ) ;
#67739 = CYLINDRICAL_SURFACE ( 'NONE', #48569, 0.5000000000000004441 ) ;
#67741 = CARTESIAN_POINT ( 'NONE',  ( -7.684764310694971456, 15.00000000000000000, 12.88194075009929840 ) ) ;
#67740 = CARTESIAN_POINT ( 'NONE',  ( 15.44008868035555260, 44.73035201082151247, 9.422509992056143702 ) ) ;
#67742 = CARTESIAN_POINT ( 'NONE',  ( 2.791683348922237240, 15.38393115100078212, -7.208316651077763204 ) ) ;
#67743 = CARTESIAN_POINT ( 'NONE',  ( 19.84674366389459266, 18.30059781766745175, 2.638427012816836559 ) ) ;
#67744 = DIRECTION ( 'NONE',  ( 0.000000000000000000, 0.000000000000000000, -1.000000000000000000 ) ) ;
#67745 = CARTESIAN_POINT ( 'NONE',  ( -7.082119434687044190, 22.63708216824730712, 12.26659068614894998 ) ) ;
#67746 = CARTESIAN_POINT ( 'NONE',  ( 21.09922568453594849, 1.206968003263753531, 6.408140936763242479 ) ) ;
#67747 = EDGE_CURVE ( 'NONE', #69120, #58939, #57272, .T. ) ;
#67749 = DIRECTION ( 'NONE',  ( -1.000000000000000000, 0.000000000000000000, 0.000000000000000000 ) ) ;
#67748 = CARTESIAN_POINT ( 'NONE',  ( 4.559911319644449179, 2.230352010821504916, -9.422509992056141925 ) ) ;
#67750 = CARTESIAN_POINT ( 'NONE',  ( 17.08211943468705130, 18.47041550158063572, 12.26659068614894998 ) ) ;
#67751 = CARTESIAN_POINT ( 'NONE',  ( 6.204703633549690345, 47.84541550158064638, 14.16423886937410082 ) ) ;
#67752 = EDGE_CURVE ( 'NONE', #74794, #30654, #71100, .T. ) ;
#67753 = ORIENTED_EDGE ( 'NONE', *, *, #74466, .T. ) ;
#67754 = CARTESIAN_POINT ( 'NONE',  ( 19.84674366389459621, 18.50893115100078745, 7.409399052514197653E-17 ) ) ;
#67755 = CARTESIAN_POINT ( 'NONE',  ( 0.5774900079438607392, 8.480352010821505360, 5.440088680355550821 ) ) ;
#67756 = CARTESIAN_POINT ( 'NONE',  ( 19.84674366389459266, 53.71726448433411605, -2.638427012816827677 ) ) ;
#67758 = CARTESIAN_POINT ( 'NONE',  ( -9.000000000000001776, 80.99999999999994316, 0.000000000000000000 ) ) ;
#67757 = CARTESIAN_POINT ( 'NONE',  ( 13.79529636645031943, 5.345415501580634832, -14.16423886937409904 ) ) ;
#67759 = LINE ( 'NONE', #53731, #80726 ) ;
#67760 = EDGE_CURVE ( 'NONE', #54280, #71137, #55606, .T. ) ;
#67761 = CARTESIAN_POINT ( 'NONE',  ( 10.00000000000000178, 2.258931151000784787, 9.846743663894594434 ) ) ;
#67762 = CARTESIAN_POINT ( 'NONE',  ( 0.6178305044545818747, 43.49863466993042493, -9.382169495545419124 ) ) ;
#67763 = CARTESIAN_POINT ( 'NONE',  ( 0.1532563361054082862, 41.21726448433411605, 2.638427012816831674 ) ) ;
#67764 = VERTEX_POINT ( 'NONE', #57062 ) ;
#67765 = CARTESIAN_POINT ( 'NONE',  ( 12.63842701281683922, 9.550597817667449974, -9.846743663894590881 ) ) ;
#67766 = CARTESIAN_POINT ( 'NONE',  ( 11.10657215102223638, -52.67603735982828539, -4.000000000003583800 ) ) ;
#67767 = CARTESIAN_POINT ( 'NONE',  ( -14.82269085861176983, 14.49999999999999112, 2.299529454046846499 ) ) ;
#67768 = CARTESIAN_POINT ( 'NONE',  ( 7.084665262690076126, 4.105352010821503583, 10.88017736071109987 ) ) ;
#67769 = CARTESIAN_POINT ( 'NONE',  ( -4.164238869374099927, 52.01208216824729647, 3.795296366450308767 ) ) ;
#67770 = CARTESIAN_POINT ( 'NONE',  ( 22.26659068614894466, 3.887082168247300906, 7.082119434687054849 ) ) ;
#67771 = CARTESIAN_POINT ( 'NONE',  ( 7.361572987183169658, 19.96726448433411960, -9.846743663894592657 ) ) ;
#67772 = CARTESIAN_POINT ( 'NONE',  ( 15.44008868035555793, 11.39701867748817143, -9.422509992056140149 ) ) ;
#67773 = CARTESIAN_POINT ( 'NONE',  ( 2.791683348922240793, 1.633931151000784565, 7.208316651077764092 ) ) ;
#67774 = CARTESIAN_POINT ( 'NONE',  ( 4.838527690343618737, 0.5000000000000004441, -14.19819177887726624 ) ) ;
#67775 = CARTESIAN_POINT ( 'NONE',  ( 14.92337183194729633, 47.67559781766745175, 8.527530157486181039 ) ) ;
#67776 = CARTESIAN_POINT ( 'NONE',  ( 20.88017736071110519, 40.56368534415484106, 2.639326808657452039E-16 ) ) ;
#67777 = ORIENTED_EDGE ( 'NONE', *, *, #56679, .T. ) ;
#67778 = CARTESIAN_POINT ( 'NONE',  ( 19.38216949554541202, 55.99863466993041072, 9.382169495545424454 ) ) ;
#67779 = DIRECTION ( 'NONE',  ( -0.000000000000000000, -0.000000000000000000, -1.000000000000000000 ) ) ;
#67780 = VECTOR ( 'NONE', #20487, 1000.000000000000000 ) ;
#67781 = CARTESIAN_POINT ( 'NONE',  ( 14.92337183194729988, 9.342264484334119601, -8.527530157486177487 ) ) ;
#67782 = CARTESIAN_POINT ( 'NONE',  ( 19.38216949554541202, 40.99863466993042493, 9.382169495545424454 ) ) ;
#67784 = CARTESIAN_POINT ( 'NONE',  ( 17.20831665107776587, 32.88393115100078745, 7.208316651077764980 ) ) ;
#67783 = CARTESIAN_POINT ( 'NONE',  ( 20.88017736071110875, 10.77201867748817143, -2.915334737309920765 ) ) ;
#67785 = CARTESIAN_POINT ( 'NONE',  ( 20.00000000000000355, 90.60976979464908254, 4.970182472450021649 ) ) ;
#67786 = FACE_OUTER_BOUND ( 'NONE', #33151, .T. ) ;
#67787 = CARTESIAN_POINT ( 'NONE',  ( 24.16423886937409904, 24.09541550158063927, 3.795296366450317205 ) ) ;
#67788 = CARTESIAN_POINT ( 'NONE',  ( 6.204703633549690345, 50.76208216824730357, -14.16423886937410259 ) ) ;
#67789 = CARTESIAN_POINT ( 'NONE',  ( 5.076628168052703671, 56.84226448433412315, 8.527530157486179263 ) ) ;
#67790 = DIRECTION ( 'NONE',  ( -0.000000000000000000, -1.000000000000000000, -0.000000000000000000 ) ) ;
#67791 = CARTESIAN_POINT ( 'NONE',  ( 0.5774900079438607392, 43.48035201082151247, 5.440088680355550821 ) ) ;
#67792 = VECTOR ( 'NONE', #54564, 1000.000000000000000 ) ;
#67793 = EDGE_CURVE ( 'NONE', #88979, #90692, #88051, .T. ) ;
#67794 = CARTESIAN_POINT ( 'NONE',  ( 0.1532563361054100626, 5.800597817667452638, -2.638427012816831230 ) ) ;
#67795 =( NAMED_UNIT ( * ) SI_UNIT ( $, .STERADIAN. ) SOLID_ANGLE_UNIT ( ) );
#67796 = ORIENTED_EDGE ( 'NONE', *, *, #43800, .F. ) ;
#67797 = CARTESIAN_POINT ( 'NONE',  ( -2.816281873526471635, 53.91530133659709634, -3.434112377981056508 ) ) ;
#67798 = ORIENTED_EDGE ( 'NONE', *, *, #97234, .F. ) ;
#67799 = CARTESIAN_POINT ( 'NONE',  ( 0.1532563361054083140, 1.008931151000784787, 1.131784320476157264E-15 ) ) ;
#67800 = VERTEX_POINT ( 'NONE', #87563 ) ;
#67801 = CARTESIAN_POINT ( 'NONE',  ( -0.3689425029237898834, 6.178748834913968757, -10.36894250292378850 ) ) ;
#67802 = CARTESIAN_POINT ( 'NONE',  ( 7.361572987183170547, 2.050597817667451750, 9.846743663894590881 ) ) ;
#67803 = CARTESIAN_POINT ( 'NONE',  ( 0.5774900079438590739, 27.64701867748817676, -5.440088680355550821 ) ) ;
#67804 =( LENGTH_UNIT ( ) NAMED_UNIT ( * ) SI_UNIT ( .MILLI., .METRE. ) );
#67805 = B_SPLINE_CURVE_WITH_KNOTS ( 'NONE', 3,
 ( #43672, #12683, #72681, #43182 ),
 .UNSPECIFIED., .F., .F.,
 ( 4, 4 ),
 ( 0.000000000000000000, 0.001036303429213370712 ),
 .UNSPECIFIED. ) ;
#67807 = ADVANCED_FACE ( 'NONE', ( #27054 ), #25130, .T. ) ;
#67806 = ORIENTED_EDGE ( 'NONE', *, *, #54217, .F. ) ;
#67808 = CARTESIAN_POINT ( 'NONE',  ( 0.5774900079438590739, 27.64701867748817676, -5.440088680355550821 ) ) ;
#67809 =( BOUNDED_CURVE ( )  B_SPLINE_CURVE ( 2, ( #63644, #56171, #19633, #88612, #65611, #80131, #96138, #28112, #58106 ),
 .UNSPECIFIED., .F., .F. ) 
 B_SPLINE_CURVE_WITH_KNOTS ( ( 3, 2, 2, 2, 3 ),
 ( 0.2605718029354654464, 0.2619047619047619180, 0.2678571428571428492, 0.2738095238095238360, 0.2751424827788204741 ),
 .UNSPECIFIED. ) 
 CURVE ( )  GEOMETRIC_REPRESENTATION_ITEM ( )  RATIONAL_B_SPLINE_CURVE ( ( 0.9881565478350731180, 0.9923695281211488695, 1.000000000000000000, 0.9659258262890683122, 1.000000000000000000, 0.9659258262890683122, 1.000000000000000000, 0.9923695281211478703, 0.9881565478350720078 ) ) 
 REPRESENTATION_ITEM ( '' )  );
#67810 = ORIENTED_EDGE ( 'NONE', *, *, #81770, .T. ) ;
#67811 = CARTESIAN_POINT ( 'NONE',  ( 2.035157376598824452, 33.68868534415484106, 7.964842623401179544 ) ) ;
#67812 = CARTESIAN_POINT ( 'NONE',  ( 7.361572987183170547, 67.05059781766746596, 9.846743663894590881 ) ) ;
#67813 = VERTEX_POINT ( 'NONE', #4578 ) ;
#67814 = EDGE_LOOP ( 'NONE', ( #77325, #71174, #72171, #69530 ) ) ;
#67815 = CARTESIAN_POINT ( 'NONE',  ( 16.40814093676324603, 12.45696800326375353, -11.09922568453594671 ) ) ;
#67816 =( NAMED_UNIT ( * ) PLANE_ANGLE_UNIT ( ) SI_UNIT ( $, .RADIAN. ) );
#67817 = CARTESIAN_POINT ( 'NONE',  ( 2.791683348922240793, 1.633931151000784565, 7.208316651077764092 ) ) ;
#67818 = CARTESIAN_POINT ( 'NONE',  ( -14.35840480524203144, 15.00000000000000000, 4.340070442838751319 ) ) ;
#67820 = DIRECTION ( 'NONE',  ( 0.000000000000000000, -1.000000000000000000, -0.000000000000000000 ) ) ;
#67819 = CARTESIAN_POINT ( 'NONE',  ( 20.88017736071110164, 15.35535201082150358, 2.915334737309930979 ) ) ;
#67821 = CARTESIAN_POINT ( 'NONE',  ( 17.20831665107776587, 9.133931151000787452, -7.208316651077762316 ) ) ;
#67822 = CARTESIAN_POINT ( 'NONE',  ( 12.91533473730993009, 21.60535201082150536, -10.88017736071109987 ) ) ;
#67823 = STYLED_ITEM ( 'NONE', ( #1668 ), #52391 ) ;
#67824 = VERTEX_POINT ( 'NONE', #82031 ) ;
#67825 = CARTESIAN_POINT ( 'NONE',  ( 22.81628187352647785, 56.62363466993042493, 6.195893100308588602E-16 ) ) ;
#67826 = CARTESIAN_POINT ( 'NONE',  ( 10.00000000000000178, 39.31368534415484106, 10.88017736071110342 ) ) ;
#67827 = CARTESIAN_POINT ( 'NONE',  ( -46.68456736488006698, 103.6675473310227176, -5.775421524742654356 ) ) ;
#67828 = CARTESIAN_POINT ( 'NONE',  ( 10.00000000000000000, 52.87363466993041783, -12.81628187352647608 ) ) ;
#67829 = CARTESIAN_POINT ( 'NONE',  ( 4.559911319644449179, 42.23035201082151247, -9.422509992056141925 ) ) ;
#67830 = CARTESIAN_POINT ( 'NONE',  ( 1.472469842513823179, 66.42559781766745175, 4.923371831947296329 ) ) ;
#67831 = DIRECTION ( 'NONE',  ( -5.818595309480553908E-17, -1.000000000000000000, -0.000000000000000000 ) ) ;
#67832 = CARTESIAN_POINT ( 'NONE',  ( 10.00000000000000178, 17.25893115100078745, 9.846743663894594434 ) ) ;
#67833 = CARTESIAN_POINT ( 'NONE',  ( -1.099225684535947600, 59.54030133659708923, 6.408140936763237150 ) ) ;
#67834 = CARTESIAN_POINT ( 'NONE',  ( 6.034057809536170325, -36.05796335879009007, -3.750000000000000444 ) ) ;
#67836 = AXIS2_PLACEMENT_3D ( 'NONE', #44278, #74782, #14799 ) ;
#67835 = CARTESIAN_POINT ( 'NONE',  ( -2.816281873526473856, 4.123634669930420493, 9.499525473075851096E-16 ) ) ;
#67838 = CARTESIAN_POINT ( 'NONE',  ( 19.84674366389459266, 63.30059781766745886, 2.638427012816836559 ) ) ;
#67837 = CARTESIAN_POINT ( 'NONE',  ( 14.94699059465101776, 0.5000000000000004441, -1.259949270174818059 ) ) ;
#67839 = CARTESIAN_POINT ( 'NONE',  ( 2.035157376598822676, 42.43868534415483396, -7.964842623401177768 ) ) ;
#67840 = CARTESIAN_POINT ( 'NONE',  ( 2.791683348922240793, 46.63393115100077324, 7.208316651077764092 ) ) ;
#67841 =( LENGTH_UNIT ( ) NAMED_UNIT ( * ) SI_UNIT ( .MILLI., .METRE. ) );
#67842 = EDGE_CURVE ( 'NONE', #20604, #64886, #52036, .T. ) ;
#67843 = CARTESIAN_POINT ( 'NONE',  ( 0.1532563361054082862, 11.21726448433411605, 2.638427012816831674 ) ) ;
#67845 = EDGE_LOOP ( 'NONE', ( #1657, #15019, #54615, #88615, #71882, #19830 ) ) ;
#67844 = CARTESIAN_POINT ( 'NONE',  ( 21.09922568453594849, 6.206968003263753531, 6.408140936763242479 ) ) ;
#67846 = SURFACE_STYLE_USAGE ( .BOTH. , #31300 ) ;
#67847 = CARTESIAN_POINT ( 'NONE',  ( 1.472469842513823179, 65.59226448433412315, -4.923371831947296329 ) ) ;
#67848 = STYLED_ITEM ( 'NONE', ( #20742 ), #32234 ) ;
#67849 = CARTESIAN_POINT ( 'NONE',  ( 4.471066085527736433, -3.611416924289630348, -2.500000000000000000 ) ) ;
#67850 = CARTESIAN_POINT ( 'NONE',  ( -2.266590686148945544, 66.38708216824730357, -7.082119434687050408 ) ) ;
#67851 = CARTESIAN_POINT ( 'NONE',  ( 0.1532563361054082862, 41.21726448433411605, 2.638427012816831674 ) ) ;
#67852 =( GEOMETRIC_REPRESENTATION_CONTEXT ( 3 ) GLOBAL_UNCERTAINTY_ASSIGNED_CONTEXT ( ( #97494 ) ) GLOBAL_UNIT_ASSIGNED_CONTEXT ( ( #4906, #3433, #96405 ) ) REPRESENTATION_CONTEXT ( 'NONE', 'WORKASPACE' ) );
#67853 = DIRECTION ( 'NONE',  ( 0.000000000000000000, 0.000000000000000000, 1.000000000000000000 ) ) ;
#67854 = CARTESIAN_POINT ( 'NONE',  ( 4.559911319644449179, 2.230352010821504916, -9.422509992056141925 ) ) ;
#67855 = CARTESIAN_POINT ( 'NONE',  ( 2.603489959281586774, 5.435752660568278216, -6.500000000000001776 ) ) ;
#67856 = CARTESIAN_POINT ( 'NONE',  ( 10.00000000000000000, 21.81368534415484106, -10.88017736071110342 ) ) ;
#67857 = CARTESIAN_POINT ( 'NONE',  ( 2.917880565312950480, 45.97041550158063927, -12.26659068614894821 ) ) ;
#67859 = CARTESIAN_POINT ( 'NONE',  ( 20.15039907845753575, 15.60158574516642815, -6.262539305110077059 ) ) ;
#67858 = CARTESIAN_POINT ( 'NONE',  ( -0.3689425029237898834, 61.17874883491396076, -10.36894250292378850 ) ) ;
#67860 = CARTESIAN_POINT ( 'NONE',  ( 1.472469842513823179, 26.42559781766745175, 4.923371831947296329 ) ) ;
#67861 = CARTESIAN_POINT ( 'NONE',  ( 3.591859063236761518, 14.95696800326375531, 11.09922568453594849 ) ) ;
#67862 = ORIENTED_EDGE ( 'NONE', *, *, #69387, .T. ) ;
#67863 = DIRECTION ( 'NONE',  ( 0.6246950475544238435, 0.7808688094430307203, 0.000000000000000000 ) ) ;
#67864 = CARTESIAN_POINT ( 'NONE',  ( 9.820177974736324700, 0.2301504389881812163, 11.25994418464059343 ) ) ;
#67865 = DIRECTION ( 'NONE',  ( 0.000000000000000000, 0.000000000000000000, 1.000000000000000000 ) ) ;
#67866 = CARTESIAN_POINT ( 'NONE',  ( 24.16423886937409904, 14.09541550158063217, 3.795296366450317205 ) ) ;
#67867 = CARTESIAN_POINT ( 'NONE',  ( 2.791683348922237240, 20.38393115100078745, -7.208316651077763204 ) ) ;
#67868 = EDGE_CURVE ( 'NONE', #29547, #84748, #20247, .T. ) ;
#67869 = DIRECTION ( 'NONE',  ( -0.000000000000000000, -0.000000000000000000, -1.000000000000000000 ) ) ;
#67870 = VERTEX_POINT ( 'NONE', #75025 ) ;
#67871 = CARTESIAN_POINT ( 'NONE',  ( 20.36894250292379382, 43.67874883491397497, 10.36894250292379205 ) ) ;
#67872 = CARTESIAN_POINT ( 'NONE',  ( 2.791683348922240793, 6.633931151000785675, 7.208316651077764092 ) ) ;
#67874 = CARTESIAN_POINT ( 'NONE',  ( -14.03351048042399007, 15.00000000000000000, 2.474486531753619989 ) ) ;
#67873 = DIRECTION ( 'NONE',  ( -1.000000000000000000, 0.000000000000000000, 0.000000000000000000 ) ) ;
#67875 = CARTESIAN_POINT ( 'NONE',  ( 19.42250999205614193, 35.14701867748816966, 5.440088680355555262 ) ) ;
#67876 = CARTESIAN_POINT ( 'NONE',  ( -1.099225684535947600, 49.54030133659708923, 6.408140936763237150 ) ) ;
#67877 = EDGE_CURVE ( 'NONE', #70287, #11472, #67537, .T. ) ;
#67878 = CARTESIAN_POINT ( 'NONE',  ( 19.38216949554541202, 30.99863466993042138, 9.382169495545424454 ) ) ;
#67879 = CARTESIAN_POINT ( 'NONE',  ( 2.791683348922240793, 6.633931151000785675, 7.208316651077764092 ) ) ;
#67880 = ORIENTED_EDGE ( 'NONE', *, *, #73972, .F. ) ;
#67881 = CARTESIAN_POINT ( 'NONE',  ( 1.912066916745601031, 1.523660046708132265, -6.500000000000000888 ) ) ;
#67882 = CARTESIAN_POINT ( 'NONE',  ( 6.204703633549690345, 35.76208216824729647, -14.16423886937410259 ) ) ;
#67883 = CARTESIAN_POINT ( 'NONE',  ( 17.08211943468705130, 8.470415501580635720, 12.26659068614894998 ) ) ;
#67884 = CARTESIAN_POINT ( 'NONE',  ( 17.96484262340118221, 6.188685344154836621, -7.964842623401177768 ) ) ;
#67885 = CARTESIAN_POINT ( 'NONE',  ( -0.8801773607111009756, 23.06368534415484106, 1.068504757029289695E-15 ) ) ;
#67886 = CARTESIAN_POINT ( 'NONE',  ( 0.000000000000000000, 14.49999999999999822, 0.000000000000000000 ) ) ;
#67887 = CARTESIAN_POINT ( 'NONE',  ( -13.61464873478158211, 15.00000000000000000, -6.296136897218027606 ) ) ;
#67888 = CARTESIAN_POINT ( 'NONE',  ( 0.5774900079438590739, 57.64701867748817676, -5.440088680355550821 ) ) ;
#67889 = CARTESIAN_POINT ( 'NONE',  ( 0.5774900079438590739, 62.64701867748817676, -5.440088680355550821 ) ) ;
#67890 = CARTESIAN_POINT ( 'NONE',  ( 13.43411237798105340, 20.58196800326374643, 12.81628187352647963 ) ) ;
#67891 = DIRECTION ( 'NONE',  ( -0.6626200482157408311, 0.000000000000000000, 0.7489557207889990798 ) ) ;
#67892 = APPLICATION_CONTEXT ( 'automotive_design' ) ;
#67893 = CARTESIAN_POINT ( 'NONE',  ( 0.1957200283969100785, 30.25733960839543712, 6.499999999999992006 ) ) ;
#67894 = CARTESIAN_POINT ( 'NONE',  ( 1.472469842513823179, 20.59226448433411960, -4.923371831947296329 ) ) ;
#67895 = COLOUR_RGB ( '', 0.72549020, 0.75294118, 0.79215686) ;
#67896 = CARTESIAN_POINT ( 'NONE',  ( 6.565887622018943937, 25.16530133659708213, 12.81628187352647430 ) ) ;
#67897 = SURFACE_STYLE_FILL_AREA ( #6389 ) ;
#67898 = CARTESIAN_POINT ( 'NONE',  ( 17.96484262340118221, 6.188685344154836621, -7.964842623401177768 ) ) ;
#67899 = CARTESIAN_POINT ( 'NONE',  ( 17.20831665107776587, 34.13393115100078745, -7.208316651077762316 ) ) ;
#67900 = CARTESIAN_POINT ( 'NONE',  ( 3.591859063236761518, 64.95696800326376774, 11.09922568453594849 ) ) ;
#67902 = CARTESIAN_POINT ( 'NONE',  ( 2.917880565312948704, 2.637082168247300906, 12.26659068614894643 ) ) ;
#67901 = CARTESIAN_POINT ( 'NONE',  ( 10.00000000000000000, 19.75893115100078390, -9.846743663894594434 ) ) ;
#67903 = CARTESIAN_POINT ( 'NONE',  ( 9.050000000000002487, 99.99999999999998579, 8.000000000000000000 ) ) ;
#67904 = CARTESIAN_POINT ( 'NONE',  ( 12.91533473730993009, 31.60535201082150891, -10.88017736071109987 ) ) ;
#67905 = DIRECTION ( 'NONE',  ( 0.000000000000000000, -1.000000000000000000, 0.000000000000000000 ) ) ;
#67906 = CARTESIAN_POINT ( 'NONE',  ( 0.1532563361054083140, 46.00893115100079456, 1.131784320476157264E-15 ) ) ;
#67907 = CARTESIAN_POINT ( 'NONE',  ( 15.44008868035555260, 34.73035201082151247, 9.422509992056143702 ) ) ;
#67908 = AXIS2_PLACEMENT_3D ( 'NONE', #87013, #18523, #49013 ) ;
#67909 = CARTESIAN_POINT ( 'NONE',  ( 7.084665262690076126, 19.10535201082150181, 10.88017736071109987 ) ) ;
#67910 = ORIENTED_EDGE ( 'NONE', *, *, #75674, .T. ) ;
#67911 = AXIS2_PLACEMENT_3D ( 'NONE', #46298, #38801, #821 ) ;
#67912 = CARTESIAN_POINT ( 'NONE',  ( 7.084665262690076126, 27.02201867748817676, -10.88017736071110164 ) ) ;
#67913 = CARTESIAN_POINT ( 'NONE',  ( 0.6178305044545838731, 49.74863466993041072, 9.382169495545420901 ) ) ;
#67914 = CARTESIAN_POINT ( 'NONE',  ( 0.5774900079438590739, 42.64701867748816966, -5.440088680355550821 ) ) ;
#67916 = CARTESIAN_POINT ( 'NONE',  ( 7.084665262690076126, 34.10535201082151247, 10.88017736071109987 ) ) ;
#67915 = PRESENTATION_STYLE_ASSIGNMENT (( #91389 ) ) ;
#67917 = ORIENTED_EDGE ( 'NONE', *, *, #26548, .F. ) ;
#67918 = CARTESIAN_POINT ( 'NONE',  ( 12.63842701281683034, 52.46726448433413026, 9.846743663894596210 ) ) ;
#67919 = CARTESIAN_POINT ( 'NONE',  ( 20.88017736071110875, 35.77201867748816966, -2.915334737309920765 ) ) ;
#67920 = CARTESIAN_POINT ( 'NONE',  ( 6.829574850505125028, -88.00372650098209704, 3.750000000000000000 ) ) ;
#67921 = FACE_OUTER_BOUND ( 'NONE', #49194, .T. ) ;
#67922 = CARTESIAN_POINT ( 'NONE',  ( 19.80777595082616926, 30.68878173731741299, -6.499999999999961808 ) ) ;
#67923 = CARTESIAN_POINT ( 'NONE',  ( 10.00000000000000000, 40.55374883491397497, -14.16423886937410082 ) ) ;
#67924 = CARTESIAN_POINT ( 'NONE',  ( 10.00000000000000178, 49.31368534415484106, 10.88017736071110342 ) ) ;
#67925 = CARTESIAN_POINT ( 'NONE',  ( -14.35840480524207585, 14.63606918001612200, 4.340070442838747766 ) ) ;
#67926 = CIRCLE ( 'NONE', #4046, 15.00000000000000000 ) ;
#67927 = DIRECTION ( 'NONE',  ( 0.3007057995042831666, 0.000000000000000000, -0.9537169507482237130 ) ) ;
#67928 = CARTESIAN_POINT ( 'NONE',  ( 5.076628168052703671, 56.84226448433412315, 8.527530157486179263 ) ) ;
#67929 = CARTESIAN_POINT ( 'NONE',  ( 4.559911319644449179, 3.897018677488170990, 9.422509992056141925 ) ) ;
#67930 = CARTESIAN_POINT ( 'NONE',  ( 17.20831665107776587, 34.13393115100078745, -7.208316651077762316 ) ) ;
#67931 = ORIENTED_EDGE ( 'NONE', *, *, #46064, .T. ) ;
#67932 = CARTESIAN_POINT ( 'NONE',  ( 0.1532563361054082862, 36.21726448433410894, 2.638427012816831674 ) ) ;
#67933 = CARTESIAN_POINT ( 'NONE',  ( -6.408140936763246032, -21.70969866340290721, -11.09922568453594316 ) ) ;
#67934 = CARTESIAN_POINT ( 'NONE',  ( 20.88017736071110164, 25.35535201082150891, 2.915334737309930979 ) ) ;
#67935 = CARTESIAN_POINT ( 'NONE',  ( 17.20831665107776587, 29.13393115100078390, -7.208316651077762316 ) ) ;
#67936 = CARTESIAN_POINT ( 'NONE',  ( 19.38216949554541202, 25.99863466993042138, 9.382169495545424454 ) ) ;
#67937 = CARTESIAN_POINT ( 'NONE',  ( 1.274849032794231007, 38.57228050351032067, 6.499999999999895195 ) ) ;
#67939 = CARTESIAN_POINT ( 'NONE',  ( 3.591859063236761518, 64.95696800326376774, 11.09922568453594849 ) ) ;
#67938 = CARTESIAN_POINT ( 'NONE',  ( -0.8801773607111009756, 38.06368534415484106, 1.068504757029289695E-15 ) ) ;
#67940 = CARTESIAN_POINT ( 'NONE',  ( 24.16423886937409904, 49.09541550158063217, 3.795296366450317205 ) ) ;
#67941 = DIRECTION ( 'NONE',  ( 0.000000000000000000, -1.000000000000000000, 0.000000000000000000 ) ) ;
#67942 = VERTEX_POINT ( 'NONE', #22046 ) ;
#67943 = CARTESIAN_POINT ( 'NONE',  ( 0.6178305044545838731, 19.74863466993042138, 9.382169495545420901 ) ) ;
#67944 = CARTESIAN_POINT ( 'NONE',  ( 10.00000000000000000, 1.813685344154837731, -10.88017736071110342 ) ) ;
#67945 = CARTESIAN_POINT ( 'NONE',  ( 19.42250999205614193, 50.14701867748817676, 5.440088680355555262 ) ) ;
#67946 = FILL_AREA_STYLE_COLOUR ( '', #85698 ) ;
#67947 = VERTEX_POINT ( 'NONE', #96065 ) ;
#67948 = CARTESIAN_POINT ( 'NONE',  ( 0.5774900079438607392, 58.48035201082151247, 5.440088680355550821 ) ) ;
#67949 = CARTESIAN_POINT ( 'NONE',  ( 12.63842701281683922, 29.55059781766745175, -9.846743663894590881 ) ) ;
#67950 = CARTESIAN_POINT ( 'NONE',  ( 1.472469842513823179, 25.59226448433412315, -4.923371831947296329 ) ) ;
#67951 = CARTESIAN_POINT ( 'NONE',  ( 14.92337183194729988, 9.342264484334119601, -8.527530157486177487 ) ) ;
#67952 = DIRECTION ( 'NONE',  ( -0.000000000000000000, -1.000000000000000000, -0.000000000000000000 ) ) ;
#67953 = CIRCLE ( 'NONE', #2541, 15.00000000000000000 ) ;
#67955 = CARTESIAN_POINT ( 'NONE',  ( 16.40814093676323893, 35.79030133659708923, 11.09922568453595026 ) ) ;
#67954 = CARTESIAN_POINT ( 'NONE',  ( -6.867320125558078914, -58.36821204062274404, 2.750000000000000000 ) ) ;
#67956 = EDGE_CURVE ( 'NONE', #42198, #96185, #34486, .T. ) ;
#67958 = CARTESIAN_POINT ( 'NONE',  ( 19.72487221294571569, 50.71833443783938122, -6.499999999999983125 ) ) ;
#67957 = CARTESIAN_POINT ( 'NONE',  ( 14.92337183194729988, 14.34226448433411782, -8.527530157486177487 ) ) ;
#67959 = CARTESIAN_POINT ( 'NONE',  ( -14.17193700899791153, 15.00000000000000000, 1.489530601563921808 ) ) ;
#67961 = ORIENTED_EDGE ( 'NONE', *, *, #80971, .T. ) ;
#67960 = CARTESIAN_POINT ( 'NONE',  ( 18.52753015748618282, 38.92559781766745175, -4.923371831947291888 ) ) ;
#67962 = CARTESIAN_POINT ( 'NONE',  ( -5.428133280998947541, 0.000000000000000000, 0.5226697871167153009 ) ) ;
#67963 = CARTESIAN_POINT ( 'NONE',  ( 22.81628187352647785, 11.41530133659708390, 3.434112377981063169 ) ) ;
#67964 = AXIS2_PLACEMENT_3D ( 'NONE', #98778, #60730, #91230 ) ;
#67965 = CARTESIAN_POINT ( 'NONE',  ( 17.96484262340118221, 56.18868534415484817, -7.964842623401177768 ) ) ;
#67966 = CARTESIAN_POINT ( 'NONE',  ( 22.26659068614894466, 28.88708216824730357, 7.082119434687054849 ) ) ;
#67967 = DIRECTION ( 'NONE',  ( 0.000000000000000000, 0.000000000000000000, 1.000000000000000000 ) ) ;
#67968 = CARTESIAN_POINT ( 'NONE',  ( 17.08211943468705130, 28.47041550158063572, 12.26659068614894998 ) ) ;
#67969 = CARTESIAN_POINT ( 'NONE',  ( 2.917880565312948704, 47.63708216824730357, 12.26659068614894643 ) ) ;
#67970 = CARTESIAN_POINT ( 'NONE',  ( 6.204703633549690345, 12.84541550158063572, 14.16423886937410082 ) ) ;
#67972 = CARTESIAN_POINT ( 'NONE',  ( -0.3289641300568009741, 37.24545670184114243, -5.963430220938281678 ) ) ;
#67971 = CARTESIAN_POINT ( 'NONE',  ( 6.204703633549690345, 15.76208216824730179, -14.16423886937410259 ) ) ;
#67973 = CARTESIAN_POINT ( 'NONE',  ( -0.8801773607111008646, 48.27201867748816966, 2.915334737309923430 ) ) ;
#67974 = CARTESIAN_POINT ( 'NONE',  ( 14.02068044289378967, 0.5000000000000004441, -5.331089937175664595 ) ) ;
#67975 = CARTESIAN_POINT ( 'NONE',  ( 12.63842701281683034, 27.46726448433411250, 9.846743663894596210 ) ) ;
#67977 = CARTESIAN_POINT ( 'NONE',  ( 0.1532563361054082862, 46.21726448433411605, 2.638427012816831674 ) ) ;
#67976 = CARTESIAN_POINT ( 'NONE',  ( 2.603489959281614308, 56.58210964143329846, 6.500000000000031086 ) ) ;
#67978 = CARTESIAN_POINT ( 'NONE',  ( 10.00000000000000178, 29.31368534415483751, 10.88017736071110342 ) ) ;
#67979 = CARTESIAN_POINT ( 'NONE',  ( 16.40814093676324603, 62.45696800326376064, -11.09922568453594671 ) ) ;
#67980 = DIRECTION ( 'NONE',  ( -0.000000000000000000, 1.000000000000000000, -0.000000000000000000 ) ) ;
#67981 = CARTESIAN_POINT ( 'NONE',  ( 11.94665733272910302, 14.76984983274819996, -8.972157519073995502 ) ) ;
#67982 = CARTESIAN_POINT ( 'NONE',  ( 0.6178305044545838731, 39.74863466993041072, 9.382169495545420901 ) ) ;
#67984 = AXIS2_PLACEMENT_3D ( 'NONE', #71104, #2136, #94089 ) ;
#67983 = CARTESIAN_POINT ( 'NONE',  ( -3.795296366450300773, -17.15458449841936073, 14.16423886937410437 ) ) ;
#67985 = CARTESIAN_POINT ( 'NONE',  ( 10.00000000000000178, 44.31368534415484106, 10.88017736071110342 ) ) ;
#67986 = CARTESIAN_POINT ( 'NONE',  ( 0.1532563361054082862, 51.21726448433412315, 2.638427012816831674 ) ) ;
#67987 = CIRCLE ( 'NONE', #90297, 2.999999999999997780 ) ;
#67988 = CARTESIAN_POINT ( 'NONE',  ( -4.164238869374098151, 26.59541550158063217, -3.795296366450310543 ) ) ;
#67989 = EDGE_CURVE ( 'NONE', #75294, #43658, #91823, .T. ) ;
#67990 = EDGE_LOOP ( 'NONE', ( #55511, #1275, #69173, #87931, #93547, #72346 ) ) ;
#67991 = ADVANCED_FACE ( 'NONE', ( #50552 ), #2719, .T. ) ;
#67992 = PRESENTATION_LAYER_ASSIGNMENT (  '', '', ( #98345 ) ) ;
#67993 = CARTESIAN_POINT ( 'NONE',  ( 0.5774900079438590739, 62.64701867748817676, -5.440088680355550821 ) ) ;
#67994 = CARTESIAN_POINT ( 'NONE',  ( -0.8801773607110991993, 62.85535201082150536, -2.915334737309923874 ) ) ;
#67995 = CARTESIAN_POINT ( 'NONE',  ( 17.08211943468705840, 65.13708216824730357, -12.26659068614894466 ) ) ;
#67996 = CARTESIAN_POINT ( 'NONE',  ( 22.81628187352647785, 1.415301336597087012, 3.434112377981063169 ) ) ;
#67997 = B_SPLINE_CURVE_WITH_KNOTS ( 'NONE', 3,
 ( #38266, #290, #91749, #53745, #84263, #57174 ),
 .UNSPECIFIED., .F., .F.,
 ( 4, 2, 4 ),
 ( 3.409110551496124592E-05, 0.0004400426677367849453, 0.0008459942299586086650 ),
 .UNSPECIFIED. ) ;
#67998 = LINE ( 'NONE', #21017, #65587 ) ;
#67999 = CARTESIAN_POINT ( 'NONE',  ( 20.88017736071110164, 50.35535201082151247, 2.915334737309930979 ) ) ;
#68000 = CARTESIAN_POINT ( 'NONE',  ( -6.741983435833344807, 0.04922511925147134149, -13.12218577464097180 ) ) ;
#68001 = CARTESIAN_POINT ( 'NONE',  ( 22.26659068614894466, 48.88708216824730357, 7.082119434687054849 ) ) ;
#68002 = CARTESIAN_POINT ( 'NONE',  ( 10.88017736071110164, 25.35535201082151957, 2.915334737309921209 ) ) ;
#68003 = CARTESIAN_POINT ( 'NONE',  ( 7.084665262690076126, 12.02201867748817143, -10.88017736071110164 ) ) ;
#68004 = CARTESIAN_POINT ( 'NONE',  ( 19.42250999205614548, 25.98035201082150891, -5.440088680355545492 ) ) ;
#68005 = CARTESIAN_POINT ( 'NONE',  ( 17.20831665107776587, 52.88393115100078035, 7.208316651077764980 ) ) ;
#68006 = CARTESIAN_POINT ( 'NONE',  ( 3.591859063236761518, 44.95696800326376064, 11.09922568453594849 ) ) ;
#68007 = LINE ( 'NONE', #82007, #12091 ) ;
#68008 = ORIENTED_EDGE ( 'NONE', *, *, #45168, .T. ) ;
#68009 = CARTESIAN_POINT ( 'NONE',  ( 2.035157376598822676, 17.43868534415483751, -7.964842623401177768 ) ) ;
#68010 = CARTESIAN_POINT ( 'NONE',  ( -2.816281873526471635, 23.91530133659708568, -3.434112377981056508 ) ) ;
#68011 = FACE_OUTER_BOUND ( 'NONE', #77927, .T. ) ;
#68012 = AXIS2_PLACEMENT_3D ( 'NONE', #62432, #54446, #38974 ) ;
#68013 = CARTESIAN_POINT ( 'NONE',  ( 12.63842701281683034, 52.46726448433413026, 9.846743663894596210 ) ) ;
#68014 = CARTESIAN_POINT ( 'NONE',  ( 15.44008868035555260, 39.73035201082150536, 9.422509992056143702 ) ) ;
#68015 = CARTESIAN_POINT ( 'NONE',  ( 13.43411237798106583, 27.66530133659708568, -12.81628187352647252 ) ) ;
#68017 = DIRECTION ( 'NONE',  ( 0.000000000000000000, 0.000000000000000000, 1.000000000000000000 ) ) ;
#68016 = CARTESIAN_POINT ( 'NONE',  ( 19.42250999205614193, 45.14701867748817676, 5.440088680355555262 ) ) ;
#68018 = SURFACE_STYLE_FILL_AREA ( #41590 ) ;
#68019 = CARTESIAN_POINT ( 'NONE',  ( -1.099225684535947600, 54.54030133659708923, 6.408140936763237150 ) ) ;
#68020 = ORIENTED_EDGE ( 'NONE', *, *, #34546, .F. ) ;
#68021 = CARTESIAN_POINT ( 'NONE',  ( 1.492507162822232836, 17.19955587570481370, -6.499999999999984901 ) ) ;
#68022 = CARTESIAN_POINT ( 'NONE',  ( 12.91533473730992121, 54.52201867748816255, 10.88017736071110164 ) ) ;
#68023 = CARTESIAN_POINT ( 'NONE',  ( 0.6178305044545838731, 29.74863466993042138, 9.382169495545420901 ) ) ;
#68024 = CARTESIAN_POINT ( 'NONE',  ( 17.96484262340118221, 34.93868534415482685, 7.964842623401181321 ) ) ;
#68025 = CARTESIAN_POINT ( 'NONE',  ( 5.076628168052704559, 65.17559781766745175, -8.527530157486179263 ) ) ;
#68026 = DIRECTION ( 'NONE',  ( -0.000000000000000000, -1.000000000000000000, -0.000000000000000000 ) ) ;
#68027 = CARTESIAN_POINT ( 'NONE',  ( 17.20831665107776587, 22.88393115100078745, 7.208316651077764980 ) ) ;
#68028 = EDGE_CURVE ( 'NONE', #84532, #98193, #66639, .T. ) ;
#68029 = CARTESIAN_POINT ( 'NONE',  ( 18.52753015748618282, 3.925597817667451306, -4.923371831947291888 ) ) ;
#68030 = DIRECTION ( 'NONE',  ( 0.000000000000000000, 0.000000000000000000, 1.000000000000000000 ) ) ;
#68031 = CARTESIAN_POINT ( 'NONE',  ( 13.79529636645030344, 43.26208216824730357, 14.16423886937410614 ) ) ;
#68032 = CARTESIAN_POINT ( 'NONE',  ( 12.03768810259485100, -3.163668057994810583E-15, -8.306778944023331945 ) ) ;
#68033 = EDGE_CURVE ( 'NONE', #20694, #58781, #74528, .T. ) ;
#68034 = CARTESIAN_POINT ( 'NONE',  ( -0.8801773607111009756, 13.06368534415483929, 1.068504757029289695E-15 ) ) ;
#68035 = CARTESIAN_POINT ( 'NONE',  ( -7.116171662430651246, -80.69120418497929847, -3.999999999998387956 ) ) ;
#68036 = ORIENTED_EDGE ( 'NONE', *, *, #54184, .T. ) ;
#68037 = CARTESIAN_POINT ( 'NONE',  ( 17.96484262340118221, 9.938685344154839285, 7.964842623401181321 ) ) ;
#68038 = CARTESIAN_POINT ( 'NONE',  ( 17.08211943468705840, 60.13708216824729647, -12.26659068614894466 ) ) ;
#68039 = CARTESIAN_POINT ( 'NONE',  ( 12.63842701281683034, 47.46726448433412315, 9.846743663894596210 ) ) ;
#68040 = CARTESIAN_POINT ( 'NONE',  ( 13.43411237798105340, 35.58196800326375353, 12.81628187352647963 ) ) ;
#68041 = DIRECTION ( 'NONE',  ( -0.08715574274765093554, -0.9961946980917463224, 0.000000000000000000 ) ) ;
#68043 = CARTESIAN_POINT ( 'NONE',  ( 24.16423886937410614, 4.303748834913967869, 8.672049930838204340E-16 ) ) ;
#68042 = CARTESIAN_POINT ( 'NONE',  ( 2.815433093577111467, 14.49999999999999112, -14.73340885523756683 ) ) ;
#68044 = CARTESIAN_POINT ( 'NONE',  ( -0.8801773607110991993, 7.855352010821504471, -2.915334737309923874 ) ) ;
#68045 = CARTESIAN_POINT ( 'NONE',  ( -2.266590686148945544, 57.22041550158063217, 7.082119434687048631 ) ) ;
#68046 = CARTESIAN_POINT ( 'NONE',  ( 19.84674366389459621, 48.50893115100078745, 7.409399052514197653E-17 ) ) ;
#68047 = LINE ( 'NONE', #44044, #1357 ) ;
#68048 = CARTESIAN_POINT ( 'NONE',  ( 12.63842701281683922, 29.55059781766745175, -9.846743663894590881 ) ) ;
#68049 = DIRECTION ( 'NONE',  ( 1.000000000000000000, 0.000000000000000000, 0.000000000000000000 ) ) ;
#68050 = CARTESIAN_POINT ( 'NONE',  ( -9.846743663894590881, 21.21726448433412315, 2.638427012816840111 ) ) ;
#68051 = ORIENTED_EDGE ( 'NONE', *, *, #74995, .T. ) ;
#68052 = ORIENTED_EDGE ( 'NONE', *, *, #2682, .T. ) ;
#68053 = CARTESIAN_POINT ( 'NONE',  ( 3.969999999999999751, 10.25000000000000000, -3.750000000000000000 ) ) ;
#68054 = ORIENTED_EDGE ( 'NONE', *, *, #74548, .F. ) ;
#68055 = CARTESIAN_POINT ( 'NONE',  ( -4.164238869374099039, 21.80374883491396787, 8.674139862899312516E-16 ) ) ;
#68057 = CARTESIAN_POINT ( 'NONE',  ( 7.084665262690076126, 37.02201867748817676, -10.88017736071110164 ) ) ;
#68056 = CARTESIAN_POINT ( 'NONE',  ( 2.035157376598822676, 27.43868534415483396, -7.964842623401177768 ) ) ;
#68059 = CARTESIAN_POINT ( 'NONE',  ( 0.6178305044545838731, 24.74863466993042493, 9.382169495545420901 ) ) ;
#68058 = CARTESIAN_POINT ( 'NONE',  ( 17.20831665107776587, 64.13393115100079456, -7.208316651077762316 ) ) ;
#68060 = CARTESIAN_POINT ( 'NONE',  ( 2.917880565312950480, 0.9704155015806342766, -12.26659068614894821 ) ) ;
#68061 = CIRCLE ( 'NONE', #93588, 15.00000000000000000 ) ;
#68062 = AXIS2_PLACEMENT_3D ( 'NONE', #89357, #98372, #90830 ) ;
#68063 = VECTOR ( 'NONE', #9877, 1000.000000000000227 ) ;
#68065 = CARTESIAN_POINT ( 'NONE',  ( 10.00000000000000178, 30.37363466993042138, 12.81628187352647608 ) ) ;
#68064 = VECTOR ( 'NONE', #74188, 1000.000000000000000 ) ;
#68066 = ORIENTED_EDGE ( 'NONE', *, *, #5923, .F. ) ;
#68067 =( BOUNDED_CURVE ( )  B_SPLINE_CURVE ( 2, ( #36950, #67447, #50460, #97467, #5476, #65953, #80965, #12465, #13961 ),
 .UNSPECIFIED., .F., .F. ) 
 B_SPLINE_CURVE_WITH_KNOTS ( ( 3, 2, 2, 2, 3 ),
 ( 0.4758552226545170183, 0.4761904761904762196, 0.4821428571428571508, 0.4880952380952381375, 0.4884304916311972833 ),
 .UNSPECIFIED. ) 
 CURVE ( )  GEOMETRIC_REPRESENTATION_ITEM ( )  RATIONAL_B_SPLINE_CURVE ( ( 0.9963778908391753841, 0.9980808541467917072, 1.000000000000000000, 0.9659258262890682012, 1.000000000000000000, 0.9659258262890682012, 1.000000000000000000, 0.9980808541467920403, 0.9963778908391759392 ) ) 
 REPRESENTATION_ITEM ( '' )  );
#68068 = CARTESIAN_POINT ( 'NONE',  ( 17.20831665107776587, 39.13393115100079456, -7.208316651077762316 ) ) ;
#68069 = CARTESIAN_POINT ( 'NONE',  ( -0.8801773607110991993, 12.85535201082150358, -2.915334737309923874 ) ) ;
#68070 = VERTEX_POINT ( 'NONE', #96567 ) ;
#68071 = CARTESIAN_POINT ( 'NONE',  ( 17.96484262340118221, 16.18868534415483396, -7.964842623401177768 ) ) ;
#68072 = EDGE_LOOP ( 'NONE', ( #87631, #77183, #89655, #64824 ) ) ;
#68073 = CARTESIAN_POINT ( 'NONE',  ( 7.084665262690076126, 62.02201867748816966, -10.88017736071110164 ) ) ;
#68074 = CARTESIAN_POINT ( 'NONE',  ( 2.035157376598824452, 53.68868534415484817, 7.964842623401179544 ) ) ;
#68075 = CARTESIAN_POINT ( 'NONE',  ( 12.91533473730993009, 66.60535201082150536, -10.88017736071109987 ) ) ;
#68076 = CARTESIAN_POINT ( 'NONE',  ( 19.42250999205614548, 55.98035201082150536, -5.440088680355545492 ) ) ;
#68077 = LINE ( 'NONE', #67083, #63408 ) ;
#68078 = EDGE_CURVE ( 'NONE', #48000, #41634, #26730, .T. ) ;
#68080 = ORIENTED_EDGE ( 'NONE', *, *, #29023, .F. ) ;
#68079 = LINE ( 'NONE', #69062, #9025 ) ;
#68081 = CARTESIAN_POINT ( 'NONE',  ( 17.20831665107776587, 39.13393115100079456, -7.208316651077762316 ) ) ;
#68082 = ORIENTED_EDGE ( 'NONE', *, *, #60727, .F. ) ;
#68083 = CARTESIAN_POINT ( 'NONE',  ( 5.076628168052704559, 65.17559781766745175, -8.527530157486179263 ) ) ;
#68084 = ADVANCED_FACE ( 'NONE', ( #5062 ), #7639, .T. ) ;
#68085 = DIRECTION ( 'NONE',  ( 0.000000000000000000, 0.000000000000000000, 1.000000000000000000 ) ) ;
#68086 = CARTESIAN_POINT ( 'NONE',  ( 6.204703633549690345, 7.845415501580634832, 14.16423886937410082 ) ) ;
#68087 = VERTEX_POINT ( 'NONE', #45014 ) ;
#68088 = DIRECTION ( 'NONE',  ( 0.000000000000000000, 0.000000000000000000, 1.000000000000000000 ) ) ;
#68089 = CARTESIAN_POINT ( 'NONE',  ( -8.439016546559974685, 15.00000000000000000, 11.79122553964965014 ) ) ;
#68090 = CARTESIAN_POINT ( 'NONE',  ( 4.559911319644449179, 8.897018677488173211, 9.422509992056141925 ) ) ;
#68091 = CARTESIAN_POINT ( 'NONE',  ( -11.81378540890925066, -0.03417435944610275333, -7.968498874458281200 ) ) ;
#68093 = ORIENTED_EDGE ( 'NONE', *, *, #87137, .T. ) ;
#68092 = CARTESIAN_POINT ( 'NONE',  ( 22.81628187352648496, 46.83196800326376064, -3.434112377981050290 ) ) ;
#68094 = DIRECTION ( 'NONE',  ( -0.9999619230641713097, 0.000000000000000000, 0.008726535498367547425 ) ) ;
#68095 = CARTESIAN_POINT ( 'NONE',  ( 2.791683348922237240, 40.38393115100078035, -7.208316651077763204 ) ) ;
#68096 = CARTESIAN_POINT ( 'NONE',  ( 19.72487221294570858, 0.000000000000000000, -6.500000000000000888 ) ) ;
#68097 =( GEOMETRIC_REPRESENTATION_CONTEXT ( 3 ) GLOBAL_UNCERTAINTY_ASSIGNED_CONTEXT ( ( #72300 ) ) GLOBAL_UNIT_ASSIGNED_CONTEXT ( ( #46609, #61120, #91630 ) ) REPRESENTATION_CONTEXT ( 'NONE', 'WORKASPACE' ) );
#68098 = CARTESIAN_POINT ( 'NONE',  ( 19.38216949554541202, 20.99863466993042138, 9.382169495545424454 ) ) ;
#68099 = CARTESIAN_POINT ( 'NONE',  ( 2.791683348922237240, 30.38393115100078390, -7.208316651077763204 ) ) ;
#68100 = DIRECTION ( 'NONE',  ( 0.000000000000000000, 0.000000000000000000, 1.000000000000000000 ) ) ;
#68101 = CARTESIAN_POINT ( 'NONE',  ( 10.00000000000000178, 67.25893115100079456, 9.846743663894594434 ) ) ;
#68102 = B_SPLINE_CURVE_WITH_KNOTS ( 'NONE', 3,
 ( #85289, #94249, #1324, #9286, #69801, #32265 ),
 .UNSPECIFIED., .F., .F.,
 ( 4, 2, 4 ),
 ( 0.0002800086601590456403, 0.0006862139742846182309, 0.001092419288410190767 ),
 .UNSPECIFIED. ) ;
#68103 = DIRECTION ( 'NONE',  ( 0.000000000000000000, -1.000000000000000000, 0.000000000000000000 ) ) ;
#68104 = ADVANCED_FACE ( 'NONE', ( #28042 ), #37540, .F. ) ;
#68105 = ORIENTED_EDGE ( 'NONE', *, *, #20646, .T. ) ;
#68106 = ORIENTED_EDGE ( 'NONE', *, *, #1822, .F. ) ;
#68107 = CARTESIAN_POINT ( 'NONE',  ( 19.42250999205614193, 25.14701867748817321, 5.440088680355555262 ) ) ;
#68108 = CARTESIAN_POINT ( 'NONE',  ( -4.164238869374098151, 16.59541550158063927, -3.795296366450310543 ) ) ;
#68109 = CARTESIAN_POINT ( 'NONE',  ( 14.92337183194729988, 34.34226448433411605, -8.527530157486177487 ) ) ;
#68110 = CARTESIAN_POINT ( 'NONE',  ( 14.92337183194729988, 4.342264484334117824, -8.527530157486177487 ) ) ;
#68112 = CARTESIAN_POINT ( 'NONE',  ( 0.000000000000000000, 0.000000000000000000, 0.000000000000000000 ) ) ;
#68111 = CARTESIAN_POINT ( 'NONE',  ( 22.81628187352647785, 36.62363466993041783, 6.195893100308588602E-16 ) ) ;
#68113 = CARTESIAN_POINT ( 'NONE',  ( 19.42250999205614548, 15.98035201082150714, -5.440088680355545492 ) ) ;
#68114 = EDGE_CURVE ( 'NONE', #45674, #35045, #44296, .T. ) ;
#68115 = CARTESIAN_POINT ( 'NONE',  ( -13.95697193428306093, -2.793938176518308880E-15, -4.371663894959005425 ) ) ;
#68116 = CARTESIAN_POINT ( 'NONE',  ( 21.09922568453594849, 11.20696800326375531, 6.408140936763242479 ) ) ;
#68117 = CARTESIAN_POINT ( 'NONE',  ( 19.38216949554541557, 2.248634669930420049, -9.382169495545420901 ) ) ;
#68118 = CARTESIAN_POINT ( 'NONE',  ( 7.361572987183170547, 22.05059781766745530, 9.846743663894590881 ) ) ;
#68119 = CARTESIAN_POINT ( 'NONE',  ( -10.88017736071110164, -17.14464798917848753, -2.915334737309917212 ) ) ;
#68120 = CARTESIAN_POINT ( 'NONE',  ( 10.00000000000000000, 37.87363466993041783, -12.81628187352647608 ) ) ;
#68121 = CARTESIAN_POINT ( 'NONE',  ( 18.06765999051784988, 23.99127512925449679, 6.500000000000021316 ) ) ;
#68124 = DIRECTION ( 'NONE',  ( 0.000000000000000000, 0.000000000000000000, 1.000000000000000000 ) ) ;
#68123 = B_SPLINE_CURVE_WITH_KNOTS ( 'NONE', 3,
 ( #95618, #35094, #65592, #29077, #43100, #97122 ),
 .UNSPECIFIED., .F., .F.,
 ( 4, 2, 4 ),
 ( 3.409110551496115105E-05, 0.0004400426677367873306, 0.0008459942299586134355 ),
 .UNSPECIFIED. ) ;
#68122 = CARTESIAN_POINT ( 'NONE',  ( 0.5774900079438590739, 42.64701867748816966, -5.440088680355550821 ) ) ;
#68125 = MECHANICAL_DESIGN_GEOMETRIC_PRESENTATION_REPRESENTATION (  '', ( #42561 ), #44111 ) ;
#68126 = DIRECTION ( 'NONE',  ( 0.9304175679820206879, 0.000000000000000000, 0.3665012267243071831 ) ) ;
#68127 = CARTESIAN_POINT ( 'NONE',  ( 15.44008868035555260, 39.73035201082150536, 9.422509992056143702 ) ) ;
#68128 = CARTESIAN_POINT ( 'NONE',  ( 4.559911319644449179, 48.89701867748817676, 9.422509992056141925 ) ) ;
#68129 = CARTESIAN_POINT ( 'NONE',  ( 7.361572987183169658, 59.96726448433410894, -9.846743663894592657 ) ) ;
#68130 = CARTESIAN_POINT ( 'NONE',  ( -0.8801773607111008646, 63.27201867748817676, 2.915334737309923430 ) ) ;
#68131 = TOROIDAL_SURFACE ( 'NONE', #2698, 2.900000000000001243, 0.1000000000000000056 ) ;
#68132 = CARTESIAN_POINT ( 'NONE',  ( 2.791683348922240793, 46.63393115100077324, 7.208316651077764092 ) ) ;
#68134 = LINE ( 'NONE', #73770, #97430 ) ;
#68133 = CARTESIAN_POINT ( 'NONE',  ( 0.5774900079438590739, 2.647018677488170990, -5.440088680355550821 ) ) ;
#68135 = CARTESIAN_POINT ( 'NONE',  ( 10.00000000000000000, 12.87363466993042138, -12.81628187352647608 ) ) ;
#68136 = ORIENTED_EDGE ( 'NONE', *, *, #95309, .F. ) ;
#68137 = AXIS2_PLACEMENT_3D ( 'NONE', #9558, #17570, #70559 ) ;
#68138 = CARTESIAN_POINT ( 'NONE',  ( 17.96484262340118221, 34.93868534415482685, 7.964842623401181321 ) ) ;
#68139 = CARTESIAN_POINT ( 'NONE',  ( 19.39188664607694434, 15.83703382326399911, -6.500000000000004441 ) ) ;
#68140 = CARTESIAN_POINT ( 'NONE',  ( 20.88017736071110164, 5.355352010821502695, 2.915334737309930979 ) ) ;
#68141 = CARTESIAN_POINT ( 'NONE',  ( 20.88017736071110519, 25.56368534415483751, 2.639326808657452039E-16 ) ) ;
#68142 = CARTESIAN_POINT ( 'NONE',  ( 17.96484262340118221, 64.93868534415483396, 7.964842623401181321 ) ) ;
#68143 = CARTESIAN_POINT ( 'NONE',  ( 24.16423886937410614, 44.51208216824730357, -3.795296366450302550 ) ) ;
#68144 = CARTESIAN_POINT ( 'NONE',  ( 7.361572987183170547, 32.05059781766745175, 9.846743663894590881 ) ) ;
#68145 = CARTESIAN_POINT ( 'NONE',  ( 15.44008868035555793, 41.39701867748817676, -9.422509992056140149 ) ) ;
#68146 = DIRECTION ( 'NONE',  ( 0.000000000000000000, 0.000000000000000000, 1.000000000000000000 ) ) ;
#68147 = AXIS2_PLACEMENT_3D ( 'NONE', #48784, #41319, #25807 ) ;
#68148 = EDGE_CURVE ( 'NONE', #87399, #34693, #1221, .T. ) ;
#68149 = AXIS2_PLACEMENT_3D ( 'NONE', #82442, #28937, #75930 ) ;
#68150 = LINE ( 'NONE', #60131, #16416 ) ;
#68151 = CARTESIAN_POINT ( 'NONE',  ( 10.00000000000000178, 62.25893115100078745, 9.846743663894594434 ) ) ;
#68152 = TOROIDAL_SURFACE ( 'NONE', #34576, 14.49999999999999822, 0.5000000000000000000 ) ;
#68153 = ORIENTED_EDGE ( 'NONE', *, *, #80948, .T. ) ;
#68154 = VERTEX_POINT ( 'NONE', #46020 ) ;
#68155 = CARTESIAN_POINT ( 'NONE',  ( 20.36894250292379382, 18.67874883491397142, 10.36894250292379205 ) ) ;
#68157 = VECTOR ( 'NONE', #31555, 1000.000000000000114 ) ;
#68156 = CARTESIAN_POINT ( 'NONE',  ( 20.36894250292379382, 18.67874883491397142, 10.36894250292379205 ) ) ;
#68158 = CARTESIAN_POINT ( 'NONE',  ( 20.88017736071110164, 55.35535201082149825, 2.915334737309930979 ) ) ;
#68159 = CARTESIAN_POINT ( 'NONE',  ( 2.917880565312948704, 67.63708216824730357, 12.26659068614894643 ) ) ;
#68160 = CARTESIAN_POINT ( 'NONE',  ( 10.00000000000000000, 7.873634669930421381, -12.81628187352647608 ) ) ;
#68161 = CARTESIAN_POINT ( 'NONE',  ( 5.076628168052703671, 46.84226448433412315, 8.527530157486179263 ) ) ;
#68162 = CARTESIAN_POINT ( 'NONE',  ( -11.58061176254664915, -84.07454167686761082, 4.000000000000000000 ) ) ;
#68164 = CARTESIAN_POINT ( 'NONE',  ( 6.565887622018943937, 18.08196800326375708, -12.81628187352647608 ) ) ;
#68163 = CARTESIAN_POINT ( 'NONE',  ( 2.035157376598822676, 52.43868534415483396, -7.964842623401177768 ) ) ;
#68165 = CARTESIAN_POINT ( 'NONE',  ( 6.204703633549690345, 15.76208216824730179, -14.16423886937410259 ) ) ;
#68166 = CARTESIAN_POINT ( 'NONE',  ( 4.559911319644449179, 8.897018677488173211, 9.422509992056141925 ) ) ;
#68167 = CARTESIAN_POINT ( 'NONE',  ( 12.91533473730992121, 29.52201867748817321, 10.88017736071110164 ) ) ;
#68168 =( NAMED_UNIT ( * ) PLANE_ANGLE_UNIT ( ) SI_UNIT ( $, .RADIAN. ) );
#68169 = CARTESIAN_POINT ( 'NONE',  ( 10.00000000000000000, 56.81368534415484106, -10.88017736071110342 ) ) ;
#68170 = CARTESIAN_POINT ( 'NONE',  ( 22.81628187352647785, 46.62363466993041783, 6.195893100308588602E-16 ) ) ;
#68171 = CARTESIAN_POINT ( 'NONE',  ( -4.923371831947302546, -19.82440218233254114, -8.527530157486173934 ) ) ;
#68172 = EDGE_LOOP ( 'NONE', ( #45557, #66754, #96386, #24254 ) ) ;
#68173 = CARTESIAN_POINT ( 'NONE',  ( -46.07478503777810630, 103.8690650836416722, -6.036883934524842843 ) ) ;
#68174 = ORIENTED_EDGE ( 'NONE', *, *, #82620, .T. ) ;
#68175 = CYLINDRICAL_SURFACE ( 'NONE', #15784, 0.2500000000000002220 ) ;
#68176 = ORIENTED_EDGE ( 'NONE', *, *, #73953, .T. ) ;
#68177 = CARTESIAN_POINT ( 'NONE',  ( -0.8217048220046814233, 0.04962895218885818305, 14.73031263975986249 ) ) ;
#68179 = CARTESIAN_POINT ( 'NONE',  ( 6.204703633549690345, 62.84541550158063927, 14.16423886937410082 ) ) ;
#68178 = CARTESIAN_POINT ( 'NONE',  ( 2.917880565312950480, 65.97041550158063217, -12.26659068614894821 ) ) ;
#68181 = CARTESIAN_POINT ( 'NONE',  ( 14.92337183194729988, 64.34226448433412315, -8.527530157486177487 ) ) ;
#68180 = CARTESIAN_POINT ( 'NONE',  ( 14.92337183194729633, 22.67559781766745175, 8.527530157486181039 ) ) ;
#68182 = CARTESIAN_POINT ( 'NONE',  ( 20.15039907845753220, 49.72266099184918176, 6.262539305110078836 ) ) ;
#68183 = CARTESIAN_POINT ( 'NONE',  ( -2.120353041430744323, 15.00000000000000000, 14.34413130794943925 ) ) ;
#68184 = CARTESIAN_POINT ( 'NONE',  ( 7.361572987183169658, -0.03273551566588185635, -9.846743663894592657 ) ) ;
#68185 = CARTESIAN_POINT ( 'NONE',  ( -12.81628187352647608, 19.12363466993041783, 3.903127820947815962E-15 ) ) ;
#68186 = ORIENTED_EDGE ( 'NONE', *, *, #98825, .F. ) ;
#68187 = EDGE_CURVE ( 'NONE', #31750, #79829, #20393, .T. ) ;
#68188 = CARTESIAN_POINT ( 'NONE',  ( 24.16423886937409904, 39.09541550158062506, 3.795296366450317205 ) ) ;
#68189 = EDGE_LOOP ( 'NONE', ( #88664, #61054, #3235 ) ) ;
#68190 = CARTESIAN_POINT ( 'NONE',  ( -4.164238869374099039, 46.80374883491397497, 8.674139862899312516E-16 ) ) ;
#68191 = EDGE_LOOP ( 'NONE', ( #7366, #3623, #47035, #71725, #53030, #78637 ) ) ;
#68192 = CARTESIAN_POINT ( 'NONE',  ( 22.81628187352647785, 56.62363466993042493, 6.195893100308588602E-16 ) ) ;
#68193 = CARTESIAN_POINT ( 'NONE',  ( 0.1532563361054100626, 55.80059781766745175, -2.638427012816831230 ) ) ;
#68194 = CARTESIAN_POINT ( 'NONE',  ( 20.88017736071110875, 20.77201867748816611, -2.915334737309920765 ) ) ;
#68195 = CARTESIAN_POINT ( 'NONE',  ( -2.816281873526473856, 64.33196800326376774, 3.434112377981055619 ) ) ;
#68196 = FACE_OUTER_BOUND ( 'NONE', #26525, .T. ) ;
#68197 = CARTESIAN_POINT ( 'NONE',  ( 17.20831665107776587, 52.88393115100078035, 7.208316651077764980 ) ) ;
#68198 = CARTESIAN_POINT ( 'NONE',  ( 5.076628168052703671, 46.84226448433412315, 8.527530157486179263 ) ) ;
#68199 = ADVANCED_FACE ( 'NONE', ( #76996 ), #54970, .T. ) ;
#68201 = ORIENTED_EDGE ( 'NONE', *, *, #31687, .F. ) ;
#68200 = CARTESIAN_POINT ( 'NONE',  ( 66.76470751278411342, 44.49999999999998579, 10.00000000000000000 ) ) ;
#68202 = LINE ( 'NONE', #7201, #92408 ) ;
#68203 = VERTEX_POINT ( 'NONE', #46985 ) ;
#68204 = EDGE_CURVE ( 'NONE', #34917, #11450, #96998, .T. ) ;
#68205 = TOROIDAL_SURFACE ( 'NONE', #56974, 1.750000000000000888, 0.2500000000000000000 ) ;
#68206 = CARTESIAN_POINT ( 'NONE',  ( -4.249999999999994671, 43.00000000000000711, 6.250000000000000000 ) ) ;
#68207 = CARTESIAN_POINT ( 'NONE',  ( 12.63842701281683034, 27.46726448433411250, 9.846743663894596210 ) ) ;
#68208 = EDGE_CURVE ( 'NONE', #90212, #3379, #13981, .T. ) ;
#68209 = DIRECTION ( 'NONE',  ( 0.000000000000000000, 0.000000000000000000, 1.000000000000000000 ) ) ;
#68210 = CARTESIAN_POINT ( 'NONE',  ( 21.09922568453594849, 36.20696800326375353, 6.408140936763242479 ) ) ;
#68211 = DIRECTION ( 'NONE',  ( 0.000000000000000000, 0.000000000000000000, 1.000000000000000000 ) ) ;
#68212 = CARTESIAN_POINT ( 'NONE',  ( -18.89999999999999503, 98.99999999999998579, -7.750000000000000000 ) ) ;
#68213 = ORIENTED_EDGE ( 'NONE', *, *, #74721, .T. ) ;
#68214 = CARTESIAN_POINT ( 'NONE',  ( 2.791683348922240793, 66.63393115100079456, 7.208316651077764092 ) ) ;
#68215 = CARTESIAN_POINT ( 'NONE',  ( -0.1023957841222447179, 65.13377557478294477, 6.340343622311912952 ) ) ;
#68216 = CARTESIAN_POINT ( 'NONE',  ( 2.791683348922237240, 40.38393115100078035, -7.208316651077763204 ) ) ;
#68217 = CARTESIAN_POINT ( 'NONE',  ( -0.3689425029237881626, 32.42874883491395366, 10.36894250292379027 ) ) ;
#68218 = CARTESIAN_POINT ( 'NONE',  ( 0.1532563361054083140, 46.00893115100079456, 1.131784320476157264E-15 ) ) ;
#68219 = CARTESIAN_POINT ( 'NONE',  ( 6.565887622018943937, 65.16530133659709634, 12.81628187352647430 ) ) ;
#68220 = B_SPLINE_CURVE_WITH_KNOTS ( 'NONE', 3,
 ( #42021, #72485, #49489, #49006, #26499, #17548 ),
 .UNSPECIFIED., .F., .F.,
 ( 4, 2, 4 ),
 ( 0.0002800001862106003543, 0.0006862054174524986287, 0.001092410648694397066 ),
 .UNSPECIFIED. ) ;
#68221 = DIRECTION ( 'NONE',  ( 1.000000000000000000, 0.000000000000000000, 0.000000000000000000 ) ) ;
#68222 = CARTESIAN_POINT ( 'NONE',  ( 17.20831665107776587, 4.133931151000785675, -7.208316651077762316 ) ) ;
#68223 = AXIS2_PLACEMENT_3D ( 'NONE', #72959, #49969, #33475 ) ;
#68224 = CARTESIAN_POINT ( 'NONE',  ( -2.266590686148945544, 6.387082168247300906, -7.082119434687050408 ) ) ;
#68225 = CARTESIAN_POINT ( 'NONE',  ( 0.1532563361054082862, 46.21726448433411605, 2.638427012816831674 ) ) ;
#68226 = CARTESIAN_POINT ( 'NONE',  ( 20.88017736071110519, 50.56368534415484106, 2.639326808657452039E-16 ) ) ;
#68227 = CARTESIAN_POINT ( 'NONE',  ( 2.791683348922240793, 41.63393115100078745, 7.208316651077764092 ) ) ;
#68228 = AXIS2_PLACEMENT_3D ( 'NONE', #34053, #25606, #49551 ) ;
#68229 = CONTEXT_DEPENDENT_SHAPE_REPRESENTATION ( #55155, #71460 ) ;
#68230 = PLANE ( 'NONE',  #23588 ) ;
#68231 = EDGE_CURVE ( 'NONE', #81191, #51046, #55520, .T. ) ;
#68232 = CARTESIAN_POINT ( 'NONE',  ( 20.88017736071110519, 40.56368534415484106, 2.639326808657452039E-16 ) ) ;
#68233 = ORIENTED_EDGE ( 'NONE', *, *, #60838, .T. ) ;
#68234 = CARTESIAN_POINT ( 'NONE',  ( 9.779999999999990479, 20.99999999999999645, 0.000000000000000000 ) ) ;
#68235 = CARTESIAN_POINT ( 'NONE',  ( 15.44008868035555260, 14.73035201082150536, 9.422509992056143702 ) ) ;
#68237 = CARTESIAN_POINT ( 'NONE',  ( 10.00000000000000000, 41.81368534415484106, -10.88017736071110342 ) ) ;
#68236 = CARTESIAN_POINT ( 'NONE',  ( 3.591859063236763294, 3.290301336597087012, -11.09922568453595026 ) ) ;
#68238 = EDGE_CURVE ( 'NONE', #84641, #30081, #9184, .T. ) ;
#68239 = CARTESIAN_POINT ( 'NONE',  ( -7.595945211628415628, 4.258289072137175049E-16, 12.35117874301636398 ) ) ;
#68240 = CARTESIAN_POINT ( 'NONE',  ( 5.963430220938279902, 5.995456701841144209, -10.32896413005680181 ) ) ;
#68242 = DIRECTION ( 'NONE',  ( 0.9970872288863210642, 0.07626964003977958206, 2.765979555393854277E-17 ) ) ;
#68241 = CARTESIAN_POINT ( 'NONE',  ( 0.5774900079438607392, 38.48035201082150536, 5.440088680355550821 ) ) ;
#68243 = CARTESIAN_POINT ( 'NONE',  ( 7.361572987183170547, 17.05059781766745530, 9.846743663894590881 ) ) ;
#68244 = CARTESIAN_POINT ( 'NONE',  ( 19.84674366389459266, 38.71726448433412315, -2.638427012816827677 ) ) ;
#68245 = CARTESIAN_POINT ( 'NONE',  ( 3.795296366450306547, 20.34541550158063572, -14.16423886937410259 ) ) ;
#68246 = CARTESIAN_POINT ( 'NONE',  ( 2.791683348922240793, 61.63393115100079456, 7.208316651077764092 ) ) ;
#68247 = CARTESIAN_POINT ( 'NONE',  ( 2.917880565312948704, 62.63708216824730357, 12.26659068614894643 ) ) ;
#68248 = CARTESIAN_POINT ( 'NONE',  ( -14.88232117145528655, 0.5000000000000004441, -1.875237731503337946 ) ) ;
#68249 = CARTESIAN_POINT ( 'NONE',  ( -0.3689425029237898834, 26.17874883491396432, -10.36894250292378850 ) ) ;
#68250 = CARTESIAN_POINT ( 'NONE',  ( -2.266590686148945544, 46.38708216824730357, -7.082119434687050408 ) ) ;
#68251 = CARTESIAN_POINT ( 'NONE',  ( -0.8801773607111009756, 3.063685344154837509, 1.068504757029289695E-15 ) ) ;
#68252 = ORIENTED_EDGE ( 'NONE', *, *, #23797, .T. ) ;
#68253 = CARTESIAN_POINT ( 'NONE',  ( 2.791683348922237240, 20.38393115100078745, -7.208316651077763204 ) ) ;
#68254 = CARTESIAN_POINT ( 'NONE',  ( 0.5774900079438607392, 33.48035201082150536, 5.440088680355550821 ) ) ;
#68255 = CARTESIAN_POINT ( 'NONE',  ( 12.63842701281683922, 44.55059781766745175, -9.846743663894590881 ) ) ;
#68256 = CARTESIAN_POINT ( 'NONE',  ( 6.204703633549690345, 5.762082168247301794, -14.16423886937410259 ) ) ;
#68257 = DIRECTION ( 'NONE',  ( -0.000000000000000000, -1.000000000000000000, -0.000000000000000000 ) ) ;
#68258 = AXIS2_PLACEMENT_3D ( 'NONE', #77833, #9345, #75877 ) ;
#68259 =( NAMED_UNIT ( * ) PLANE_ANGLE_UNIT ( ) SI_UNIT ( $, .RADIAN. ) );
#68260 = CARTESIAN_POINT ( 'NONE',  ( -2.816281873526473856, 34.12363466993042493, 9.499525473075851096E-16 ) ) ;
#68261 = CARTESIAN_POINT ( 'NONE',  ( 10.00000000000000000, 39.75893115100078745, -9.846743663894594434 ) ) ;
#68262 = ORIENTED_EDGE ( 'NONE', *, *, #78485, .F. ) ;
#68263 = CARTESIAN_POINT ( 'NONE',  ( 19.84674366389459266, 3.300597817667451750, 2.638427012816836559 ) ) ;
#68264 = CARTESIAN_POINT ( 'NONE',  ( 10.93739314626210479, -97.13232482346681707, -3.750000000000000000 ) ) ;
#68265 = CARTESIAN_POINT ( 'NONE',  ( 18.72515096720578853, 60.05509018479938277, 6.499999999999877431 ) ) ;
#68266 = CARTESIAN_POINT ( 'NONE',  ( 17.96484262340118221, 4.938685344154837509, 7.964842623401181321 ) ) ;
#68267 = CARTESIAN_POINT ( 'NONE',  ( 13.79529636645030344, 48.26208216824728936, 14.16423886937410614 ) ) ;
#68268 = CARTESIAN_POINT ( 'NONE',  ( 2.035157376598822676, 42.43868534415483396, -7.964842623401177768 ) ) ;
#68269 = CARTESIAN_POINT ( 'NONE',  ( -46.94000000000001194, 93.00000000000000000, -8.999999999999998224 ) ) ;
#68270 = CARTESIAN_POINT ( 'NONE',  ( 20.24186590665277308, 51.76028685723174760, 6.114288769123050749 ) ) ;
#68271 = CARTESIAN_POINT ( 'NONE',  ( 7.361572987183170547, 32.05059781766745175, 9.846743663894590881 ) ) ;
#68272 = CARTESIAN_POINT ( 'NONE',  ( 15.44008868035555793, 6.397018677488170546, -9.422509992056140149 ) ) ;
#68273 = CARTESIAN_POINT ( 'NONE',  ( 0.1532563361054082862, 36.21726448433410894, 2.638427012816831674 ) ) ;
#68274 = CARTESIAN_POINT ( 'NONE',  ( 0.05299164502591494075, 8.154255672638641206E-15, -4.488953749917677705 ) ) ;
#68275 = CARTESIAN_POINT ( 'NONE',  ( 7.361572987183170547, 57.05059781766744464, 9.846743663894590881 ) ) ;
#68276 = CARTESIAN_POINT ( 'NONE',  ( 12.91533473730993009, 51.60535201082149825, -10.88017736071109987 ) ) ;
#68277 = ORIENTED_EDGE ( 'NONE', *, *, #86509, .F. ) ;
#68278 = VERTEX_POINT ( 'NONE', #8022 ) ;
#68279 = CARTESIAN_POINT ( 'NONE',  ( 10.00000000000000178, 60.37363466993041783, 12.81628187352647608 ) ) ;
#68280 = CARTESIAN_POINT ( 'NONE',  ( -9.159723438033054776, 15.00000000000000000, -10.91613331444555079 ) ) ;
#68281 = CARTESIAN_POINT ( 'NONE',  ( 1.472469842513823179, 11.42559781766745175, 4.923371831947296329 ) ) ;
#68282 = CARTESIAN_POINT ( 'NONE',  ( 13.43411237798105340, 60.58196800326376064, 12.81628187352647963 ) ) ;
#68284 = CARTESIAN_POINT ( 'NONE',  ( 14.92337183194729988, 49.34226448433411605, -8.527530157486177487 ) ) ;
#68283 = CARTESIAN_POINT ( 'NONE',  ( 20.88017736071110164, 5.355352010821503583, 2.915334737309930979 ) ) ;
#68285 =( NAMED_UNIT ( * ) PLANE_ANGLE_UNIT ( ) SI_UNIT ( $, .RADIAN. ) );
#68286 = CARTESIAN_POINT ( 'NONE',  ( 10.00000000000000000, -0.2410688489992152128, -9.846743663894594434 ) ) ;
#68287 = CARTESIAN_POINT ( 'NONE',  ( -2.266590686148945544, 26.38708216824730357, -7.082119434687050408 ) ) ;
#68288 = CARTESIAN_POINT ( 'NONE',  ( 10.00000000000000178, 48.05374883491396787, 14.16423886937410082 ) ) ;
#68289 = CARTESIAN_POINT ( 'NONE',  ( 10.00000000000000000, 54.75893115100078745, -9.846743663894594434 ) ) ;
#68290 = CYLINDRICAL_SURFACE ( 'NONE', #73049, 15.00000000000000000 ) ;
#68291 = CARTESIAN_POINT ( 'NONE',  ( 10.00000000000000178, 54.31368534415484106, 10.88017736071110342 ) ) ;
#68292 = CARTESIAN_POINT ( 'NONE',  ( 2.791683348922240793, 6.633931151000785675, 7.208316651077764092 ) ) ;
#68293 = SURFACE_STYLE_FILL_AREA ( #14306 ) ;
#68294 = ORIENTED_EDGE ( 'NONE', *, *, #59826, .F. ) ;
#68295 = CARTESIAN_POINT ( 'NONE',  ( -2.816281873526473856, 59.33196800326374643, 3.434112377981055619 ) ) ;
#68296 = ORIENTED_EDGE ( 'NONE', *, *, #98268, .F. ) ;
#68297 = CARTESIAN_POINT ( 'NONE',  ( 12.63842701281683922, 14.55059781766744997, -9.846743663894590881 ) ) ;
#68298 = EDGE_LOOP ( 'NONE', ( #7596, #79361, #56652, #43336, #88236, #98188 ) ) ;
#68299 = CARTESIAN_POINT ( 'NONE',  ( 22.26659068614895176, 24.72041550158063572, -7.082119434687042414 ) ) ;
#68300 = CARTESIAN_POINT ( 'NONE',  ( 7.361572987183170547, 7.050597817667451750, 9.846743663894590881 ) ) ;
#68301 = CARTESIAN_POINT ( 'NONE',  ( 4.559911319644449179, 32.23035201082150536, -9.422509992056141925 ) ) ;
#68302 = CARTESIAN_POINT ( 'NONE',  ( -45.24390243902436737, 36.19512195121945553, -8.000000000000000000 ) ) ;
#68303 = ORIENTED_EDGE ( 'NONE', *, *, #13850, .F. ) ;
#68304 = CARTESIAN_POINT ( 'NONE',  ( 12.91533473730992121, 34.52201867748817676, 10.88017736071110164 ) ) ;
#68305 = ORIENTED_EDGE ( 'NONE', *, *, #16957, .T. ) ;
#68306 = FILL_AREA_STYLE_COLOUR ( '', #88819 ) ;
#68307 = ORIENTED_EDGE ( 'NONE', *, *, #37815, .F. ) ;
#68308 = CARTESIAN_POINT ( 'NONE',  ( 21.09922568453595559, 12.04030133659708746, -6.408140936763230044 ) ) ;
#68309 = CARTESIAN_POINT ( 'NONE',  ( 20.88017736071110164, 65.35535201082150536, 2.915334737309930979 ) ) ;
#68310 = DIRECTION ( 'NONE',  ( -0.9935718556765877896, 0.000000000000000000, 0.1132032137679039180 ) ) ;
#68311 = EDGE_CURVE ( 'NONE', #95614, #59664, #68524, .T. ) ;
#68312 = CARTESIAN_POINT ( 'NONE',  ( 9.898881779040660689, -0.03417435944610275333, 10.25059215482582786 ) ) ;
#68313 = CARTESIAN_POINT ( 'NONE',  ( 2.791683348922240793, 11.63393115100078568, 7.208316651077764092 ) ) ;
#68314 = CARTESIAN_POINT ( 'NONE',  ( 20.88017736071110164, 35.35535201082150536, 2.915334737309930979 ) ) ;
#68315 = ADVANCED_FACE ( 'NONE', ( #18347 ), #4418, .T. ) ;
#68316 = VERTEX_POINT ( 'NONE', #30502 ) ;
#68317 = CARTESIAN_POINT ( 'NONE',  ( -8.000343251535921851, 84.06932101904432386, 3.750000000000000000 ) ) ;
#68318 = CARTESIAN_POINT ( 'NONE',  ( 15.44008868035555260, 39.73035201082150536, 9.422509992056143702 ) ) ;
#68319 = LINE ( 'NONE', #60796, #86664 ) ;
#68320 = CARTESIAN_POINT ( 'NONE',  ( 3.591859063236761518, 54.95696800326376064, 11.09922568453594849 ) ) ;
#68321 = CARTESIAN_POINT ( 'NONE',  ( 17.96484262340118221, 59.93868534415484106, 7.964842623401181321 ) ) ;
#68322 = EDGE_CURVE ( 'NONE', #50188, #90286, #60291, .T. ) ;
#68323 = CARTESIAN_POINT ( 'NONE',  ( 16.40814093676324603, 2.456968003263753531, -11.09922568453594671 ) ) ;
#68324 = CARTESIAN_POINT ( 'NONE',  ( 1.377727649040772586E-15, 12.49999999999999112, -11.25000000000000178 ) ) ;
#68325 = CARTESIAN_POINT ( 'NONE',  ( 0.1532563361054082862, 11.21726448433411605, 2.638427012816831674 ) ) ;
#68326 = CARTESIAN_POINT ( 'NONE',  ( -2.816281873526473856, 59.33196800326374643, 3.434112377981055619 ) ) ;
#68327 = CARTESIAN_POINT ( 'NONE',  ( 5.500000000000000000, 61.00000000000000711, -5.000000000000000000 ) ) ;
#68328 = CARTESIAN_POINT ( 'NONE',  ( 5.076628168052703671, 6.842264484334118713, 8.527530157486179263 ) ) ;
#68329 = CARTESIAN_POINT ( 'NONE',  ( 3.591859063236761518, 24.95696800326375353, 11.09922568453594849 ) ) ;
#68331 = CARTESIAN_POINT ( 'NONE',  ( 0.1532563361054083140, 61.00893115100078745, 1.131784320476157264E-15 ) ) ;
#68330 = DIRECTION ( 'NONE',  ( -0.000000000000000000, -0.000000000000000000, 1.000000000000000000 ) ) ;
#68332 = CARTESIAN_POINT ( 'NONE',  ( 17.96484262340118221, 29.93868534415484106, 7.964842623401181321 ) ) ;
#68333 = CARTESIAN_POINT ( 'NONE',  ( 1.472469842513823179, 66.42559781766745175, 4.923371831947296329 ) ) ;
#68334 = LINE ( 'NONE', #38332, #2419 ) ;
#68335 = CARTESIAN_POINT ( 'NONE',  ( 19.84674366389459266, 18.30059781766745175, 2.638427012816836559 ) ) ;
#68336 = CARTESIAN_POINT ( 'NONE',  ( 19.84674366389459266, 13.71726448433411782, -2.638427012816827677 ) ) ;
#68338 = EDGE_LOOP ( 'NONE', ( #98072, #16181, #12196, #45395, #47481 ) ) ;
#68337 = CARTESIAN_POINT ( 'NONE',  ( -2.816281873526473856, 4.123634669930420493, 9.499525473075851096E-16 ) ) ;
#68339 = AXIS2_PLACEMENT_3D ( 'NONE', #94584, #72560, #25616 ) ;
#68340 = CARTESIAN_POINT ( 'NONE',  ( 15.44008868035555793, 6.397018677488170546, -9.422509992056140149 ) ) ;
#68341 = CARTESIAN_POINT ( 'NONE',  ( 2.791683348922237240, 65.38393115100078035, -7.208316651077763204 ) ) ;
#68342 = CARTESIAN_POINT ( 'NONE',  ( 6.655516370393623760, -69.44235516214573067, -2.500000000000000000 ) ) ;
#68343 = CARTESIAN_POINT ( 'NONE',  ( 4.559911319644449179, 8.897018677488173211, 9.422509992056141925 ) ) ;
#68344 = CARTESIAN_POINT ( 'NONE',  ( 5.076628168052703671, 46.84226448433412315, 8.527530157486179263 ) ) ;
#68345 = ORIENTED_EDGE ( 'NONE', *, *, #65812, .F. ) ;
#68346 = DIRECTION ( 'NONE',  ( -0.000000000000000000, 1.000000000000000000, -0.000000000000000000 ) ) ;
#68347 = CARTESIAN_POINT ( 'NONE',  ( 0.5774900079438590739, 7.647018677488171434, -5.440088680355550821 ) ) ;
#68348 = CARTESIAN_POINT ( 'NONE',  ( 0.2751277870542909731, 47.28217586085238366, -6.499999999999992006 ) ) ;
#68349 = EDGE_CURVE ( 'NONE', #66685, #19583, #11836, .T. ) ;
#68350 = B_SPLINE_CURVE_WITH_KNOTS ( 'NONE', 3,
 ( #51898, #20912, #52874, #44872, #67388, #58389 ),
 .UNSPECIFIED., .F., .F.,
 ( 4, 2, 4 ),
 ( 0.0002800039672440407979, 0.0006862092354666064070, 0.001092414503689172070 ),
 .UNSPECIFIED. ) ;
#68351 = CARTESIAN_POINT ( 'NONE',  ( 20.88017736071110519, 30.56368534415484106, 2.639326808657452039E-16 ) ) ;
#68352 = CARTESIAN_POINT ( 'NONE',  ( 22.26659068614894466, 48.88708216824730357, 7.082119434687054849 ) ) ;
#68354 = DIRECTION ( 'NONE',  ( -0.000000000000000000, -0.000000000000000000, -1.000000000000000000 ) ) ;
#68353 = CARTESIAN_POINT ( 'NONE',  ( 10.00000000000000178, 68.05374883491397497, 14.16423886937410082 ) ) ;
#68355 = CARTESIAN_POINT ( 'NONE',  ( 19.84674366389459621, 3.508931151000785231, 7.409399052514197653E-17 ) ) ;
#68356 = CARTESIAN_POINT ( 'NONE',  ( 2.791683348922240793, 31.63393115100078745, 7.208316651077764092 ) ) ;
#68357 = CARTESIAN_POINT ( 'NONE',  ( 22.81628187352647785, 11.41530133659708390, 3.434112377981063169 ) ) ;
#68358 = LINE ( 'NONE', #98876, #18653 ) ;
#68359 =( NAMED_UNIT ( * ) SI_UNIT ( $, .STERADIAN. ) SOLID_ANGLE_UNIT ( ) );
#68360 = CARTESIAN_POINT ( 'NONE',  ( 5.076628168052704559, 60.17559781766745175, -8.527530157486179263 ) ) ;
#68362 = CARTESIAN_POINT ( 'NONE',  ( -12.87930560075664488, 0.04962897030442339763, -7.195887444332561778 ) ) ;
#68361 = COLOUR_RGB ( '', 0.66274510, 0.83137255, 0.94901961) ;
#68363 = EDGE_CURVE ( 'NONE', #55365, #50602, #61004, .T. ) ;
#68364 = VECTOR ( 'NONE', #17745, 1000.000000000000000 ) ;
#68365 = CARTESIAN_POINT ( 'NONE',  ( -10.91025143197891545, -52.91559880499231383, -3.999999999999998224 ) ) ;
#68366 = CARTESIAN_POINT ( 'NONE',  ( 10.00000000000000178, 8.053748834913967869, 14.16423886937410082 ) ) ;
#68367 = CARTESIAN_POINT ( 'NONE',  ( 0.1532563361054083140, 26.00893115100078745, 1.131784320476157264E-15 ) ) ;
#68368 = CARTESIAN_POINT ( 'NONE',  ( 17.08211943468705130, 58.47041550158063927, 12.26659068614894998 ) ) ;
#68369 = CARTESIAN_POINT ( 'NONE',  ( 0.1532563361054082862, 6.217264484334118713, 2.638427012816831674 ) ) ;
#68371 = DIRECTION ( 'NONE',  ( 1.000000000000000000, 0.000000000000000000, -0.000000000000000000 ) ) ;
#68370 = DIRECTION ( 'NONE',  ( 0.000000000000000000, 1.000000000000000000, 0.000000000000000000 ) ) ;
#68372 = CARTESIAN_POINT ( 'NONE',  ( -0.8801773607110991993, 37.85535201082151247, -2.915334737309923874 ) ) ;
#68373 = CARTESIAN_POINT ( 'NONE',  ( 19.38216949554541202, 50.99863466993042493, 9.382169495545424454 ) ) ;
#68374 = CARTESIAN_POINT ( 'NONE',  ( 2.035157376598822676, 2.438685344154837953, -7.964842623401177768 ) ) ;
#68375 = CARTESIAN_POINT ( 'NONE',  ( -1.099225684535947600, 33.70696800326375353, -6.408140936763238038 ) ) ;
#68376 = CARTESIAN_POINT ( 'NONE',  ( 0.1532563361054100626, 0.8005978176674514168, -2.638427012816831230 ) ) ;
#68377 = ORIENTED_EDGE ( 'NONE', *, *, #13215, .T. ) ;
#68378 = LINE ( 'NONE', #22882, #59836 ) ;
#68379 = CARTESIAN_POINT ( 'NONE',  ( -14.62129639376010637, -3.201784540621254098E-15, -0.3552502084987199105 ) ) ;
#68380 = CARTESIAN_POINT ( 'NONE',  ( 22.26659068614894466, 43.88708216824729647, 7.082119434687054849 ) ) ;
#68381 = CARTESIAN_POINT ( 'NONE',  ( 6.204703633549690345, 7.845415501580634832, 14.16423886937410082 ) ) ;
#68382 = CARTESIAN_POINT ( 'NONE',  ( 15.44008868035555793, 41.39701867748817676, -9.422509992056140149 ) ) ;
#68383 = LINE ( 'NONE', #68875, #78269 ) ;
#68384 = PLANE ( 'NONE',  #16046 ) ;
#68385 = CARTESIAN_POINT ( 'NONE',  ( 20.88017736071110875, 55.77201867748816966, -2.915334737309920765 ) ) ;
#68386 = CARTESIAN_POINT ( 'NONE',  ( 2.035157376598824452, 58.68868534415482685, 7.964842623401179544 ) ) ;
#68387 = CARTESIAN_POINT ( 'NONE',  ( 0.6178305044545838731, 29.74863466993042138, 9.382169495545420901 ) ) ;
#68388 = CARTESIAN_POINT ( 'NONE',  ( 5.240693273022541732, 14.95037116783232456, -13.79102773478290622 ) ) ;
#68389 = PLANE ( 'NONE',  #89812 ) ;
#68390 = CARTESIAN_POINT ( 'NONE',  ( 2.791683348922240793, 36.63393115100078035, 7.208316651077764092 ) ) ;
#68391 = CARTESIAN_POINT ( 'NONE',  ( 22.81628187352647785, 16.41530133659708923, 3.434112377981063169 ) ) ;
#68392 = CARTESIAN_POINT ( 'NONE',  ( 19.84674366389459266, 3.300597817667451750, 2.638427012816836559 ) ) ;
#68393 = CARTESIAN_POINT ( 'NONE',  ( 12.91533473730992121, 4.522018677488169658, 10.88017736071110164 ) ) ;
#68394 = CARTESIAN_POINT ( 'NONE',  ( 19.84674366389459266, 43.71726448433410894, -2.638427012816827677 ) ) ;
#68395 = CARTESIAN_POINT ( 'NONE',  ( 10.00000000000000178, 60.37363466993041783, 12.81628187352647608 ) ) ;
#68396 = CARTESIAN_POINT ( 'NONE',  ( 0.1532563361054100626, 20.80059781766744464, -2.638427012816831230 ) ) ;
#68397 = CARTESIAN_POINT ( 'NONE',  ( 10.00000000000000178, 3.053748834913967425, 14.16423886937410082 ) ) ;
#68398 = CARTESIAN_POINT ( 'NONE',  ( 17.39651004071838614, 42.93575266056826933, 6.500000000000032863 ) ) ;
#68399 = CARTESIAN_POINT ( 'NONE',  ( 7.084665262690076126, 27.02201867748817676, -10.88017736071110164 ) ) ;
#68401 = CARTESIAN_POINT ( 'NONE',  ( 6.204703633549690345, 45.76208216824729647, -14.16423886937410259 ) ) ;
#68400 = CARTESIAN_POINT ( 'NONE',  ( 4.559911319644449179, 17.23035201082150536, -9.422509992056141925 ) ) ;
#68402 = CARTESIAN_POINT ( 'NONE',  ( 17.96484262340118221, 29.93868534415484106, 7.964842623401181321 ) ) ;
#68403 = EDGE_CURVE ( 'NONE', #21055, #92145, #88154, .T. ) ;
#68404 = CARTESIAN_POINT ( 'NONE',  ( 20.88017736071110164, 15.35535201082150358, 2.915334737309930979 ) ) ;
#68405 = EDGE_LOOP ( 'NONE', ( #30563, #3247, #45797, #19884, #67693, #47354 ) ) ;
#68406 = CARTESIAN_POINT ( 'NONE',  ( 20.88017736071110164, 25.35535201082150891, 2.915334737309930979 ) ) ;
#68407 = EDGE_CURVE ( 'NONE', #67262, #43658, #23032, .T. ) ;
#68408 = CARTESIAN_POINT ( 'NONE',  ( 3.591859063236763294, 48.29030133659708923, -11.09922568453595026 ) ) ;
#68409 = CARTESIAN_POINT ( 'NONE',  ( 4.559911319644449179, 47.23035201082150536, -9.422509992056141925 ) ) ;
#68411 = CARTESIAN_POINT ( 'NONE',  ( 12.91533473730993009, 51.60535201082149825, -10.88017736071109987 ) ) ;
#68410 = CARTESIAN_POINT ( 'NONE',  ( 1.472469842513823179, 45.59226448433412315, -4.923371831947296329 ) ) ;
#68412 = ORIENTED_EDGE ( 'NONE', *, *, #86386, .F. ) ;
#68413 = CARTESIAN_POINT ( 'NONE',  ( 2.035157376598824452, 48.68868534415483396, 7.964842623401179544 ) ) ;
#68414 = CARTESIAN_POINT ( 'NONE',  ( -5.056330833731841778, 4.586016791640643039E-16, 13.58983143750696421 ) ) ;
#68415 = CARTESIAN_POINT ( 'NONE',  ( 14.62617646268094518, 14.49999999999999112, -3.327906561566873478 ) ) ;
#68416 = CARTESIAN_POINT ( 'NONE',  ( 6.204703633549690345, 42.84541550158063217, 14.16423886937410082 ) ) ;
#68417 = CARTESIAN_POINT ( 'NONE',  ( 17.96484262340118221, 61.18868534415482685, -7.964842623401177768 ) ) ;
#68418 = CARTESIAN_POINT ( 'NONE',  ( 20.15039907845753220, 25.60158574516642815, -6.262539305110077947 ) ) ;
#68419 = CARTESIAN_POINT ( 'NONE',  ( -7.322384435959399696, -84.40865712959146094, -4.000000000000000000 ) ) ;
#68420 = CARTESIAN_POINT ( 'NONE',  ( 1.472469842513823179, 61.42559781766745175, 4.923371831947296329 ) ) ;
#68421 = CARTESIAN_POINT ( 'NONE',  ( -8.000000000000000000, 75.73428692542562146, -2.900000000000000799 ) ) ;
#68422 = CARTESIAN_POINT ( 'NONE',  ( 5.076628168052703671, 31.84226448433412315, 8.527530157486179263 ) ) ;
#68423 = EDGE_LOOP ( 'NONE', ( #90424, #63365, #50467, #70766, #14684, #34059 ) ) ;
#68424 = CARTESIAN_POINT ( 'NONE',  ( 19.84674366389459266, 38.71726448433412315, -2.638427012816827677 ) ) ;
#68425 = CARTESIAN_POINT ( 'NONE',  ( -5.204170427930421283E-15, -2.126365330069574178, -12.81628187352647608 ) ) ;
#68426 = STYLED_ITEM ( 'NONE', ( #91787 ), #14192 ) ;
#68427 = CARTESIAN_POINT ( 'NONE',  ( 17.96484262340118221, 19.93868534415484106, 7.964842623401181321 ) ) ;
#68428 = CARTESIAN_POINT ( 'NONE',  ( 17.20831665107776587, 34.13393115100078745, -7.208316651077762316 ) ) ;
#68429 = CARTESIAN_POINT ( 'NONE',  ( 21.09922568453594849, 26.20696800326375353, 6.408140936763242479 ) ) ;
#68431 = CARTESIAN_POINT ( 'NONE',  ( 19.42250999205614548, 60.98035201082151247, -5.440088680355545492 ) ) ;
#68430 = CYLINDRICAL_SURFACE ( 'NONE', #80262, 0.5000000000000004441 ) ;
#68433 = CARTESIAN_POINT ( 'NONE',  ( -0.8801773607111009756, 3.063685344154837509, 1.068504757029289695E-15 ) ) ;
#68432 = CARTESIAN_POINT ( 'NONE',  ( 10.00000000000000178, 34.31368534415484106, 10.88017736071110342 ) ) ;
#68434 = CARTESIAN_POINT ( 'NONE',  ( 13.79529636645030344, 63.26208216824730357, 14.16423886937410614 ) ) ;
#68435 = VECTOR ( 'NONE', #84271, 1000.000000000000000 ) ;
#68436 = VECTOR ( 'NONE', #39029, 1000.000000000000000 ) ;
#68437 = EDGE_CURVE ( 'NONE', #44632, #26502, #69017, .T. ) ;
#68438 = CARTESIAN_POINT ( 'NONE',  ( 0.6178305044545818747, 18.49863466993041428, -9.382169495545419124 ) ) ;
#68439 = CARTESIAN_POINT ( 'NONE',  ( 6.000000000000000000, 10.49999999999999822, -6.000000000000000000 ) ) ;
#68440 = EDGE_LOOP ( 'NONE', ( #81697, #35937, #14099, #50021 ) ) ;
#68441 = CARTESIAN_POINT ( 'NONE',  ( 10.00000000000000178, 20.37363466993042138, 12.81628187352647608 ) ) ;
#68442 = CARTESIAN_POINT ( 'NONE',  ( 7.084665262690076126, 22.02201867748817321, -10.88017736071110164 ) ) ;
#68443 = ADVANCED_FACE ( 'NONE', ( #15537 ), #548, .F. ) ;
#68444 = CARTESIAN_POINT ( 'NONE',  ( 2.035157376598824452, 48.68868534415483396, 7.964842623401179544 ) ) ;
#68445 = CARTESIAN_POINT ( 'NONE',  ( -33.19000000000001194, 92.00000000000000000, -10.09898361729590199 ) ) ;
#68446 = ORIENTED_EDGE ( 'NONE', *, *, #44284, .F. ) ;
#68447 = CARTESIAN_POINT ( 'NONE',  ( 2.035157376598822676, 62.43868534415483396, -7.964842623401177768 ) ) ;
#68448 = CARTESIAN_POINT ( 'NONE',  ( 18.52753015748617571, 33.09226448433411605, 4.923371831947298993 ) ) ;
#68449 = CARTESIAN_POINT ( 'NONE',  ( 10.00000000000000000, 29.75893115100078745, -9.846743663894594434 ) ) ;
#68450 = CARTESIAN_POINT ( 'NONE',  ( 14.92337183194729988, 19.34226448433411960, -8.527530157486177487 ) ) ;
#68451 = CARTESIAN_POINT ( 'NONE',  ( 20.10493008474206178, 54.71697413083881401, 6.336235997365760042 ) ) ;
#68452 = CARTESIAN_POINT ( 'NONE',  ( 6.565887622018943937, 38.08196800326376064, -12.81628187352647608 ) ) ;
#68454 = CARTESIAN_POINT ( 'NONE',  ( -8.209432707284705089, 14.63595249122789177, -12.55409154915497538 ) ) ;
#68453 = CARTESIAN_POINT ( 'NONE',  ( 12.63842701281683922, 19.55059781766745175, -9.846743663894590881 ) ) ;
#68455 = CARTESIAN_POINT ( 'NONE',  ( 20.24186590665277308, 45.59014588040356841, -6.114288769123051637 ) ) ;
#68457 = VERTEX_POINT ( 'NONE', #11325 ) ;
#68456 = CARTESIAN_POINT ( 'NONE',  ( 17.20831665107776587, 34.13393115100078745, -7.208316651077762316 ) ) ;
#68458 = CARTESIAN_POINT ( 'NONE',  ( 17.75000000000000000, 84.07179676972448590, 12.00000000000000000 ) ) ;
#68459 = CARTESIAN_POINT ( 'NONE',  ( 16.40814093676324603, 17.45696800326375353, -11.09922568453594671 ) ) ;
#68460 = EDGE_CURVE ( 'NONE', #1436, #37674, #3342, .T. ) ;
#68461 = CARTESIAN_POINT ( 'NONE',  ( 20.88017736071110875, 45.77201867748816966, -2.915334737309920765 ) ) ;
#68462 = CARTESIAN_POINT ( 'NONE',  ( 17.08211943468705130, 28.47041550158063572, 12.26659068614894998 ) ) ;
#68463 = UNCERTAINTY_MEASURE_WITH_UNIT (LENGTH_MEASURE( 1.000000000000000082E-05 ), #92308, 'distance_accuracy_value', 'NONE');
#68464 = DIRECTION ( 'NONE',  ( -1.000000000000000000, 0.000000000000000000, 0.000000000000000000 ) ) ;
#68465 = CARTESIAN_POINT ( 'NONE',  ( 6.204703633549690345, 35.76208216824729647, -14.16423886937410259 ) ) ;
#68466 = EDGE_CURVE ( 'NONE', #663, #55728, #10759, .T. ) ;
#68467 = CARTESIAN_POINT ( 'NONE',  ( 13.79529636645030344, 58.26208216824728936, 14.16423886937410614 ) ) ;
#68468 = CARTESIAN_POINT ( 'NONE',  ( -4.164238869374099927, 12.01208216824730357, 3.795296366450308767 ) ) ;
#68470 = CARTESIAN_POINT ( 'NONE',  ( 18.04007052943773104, 33.01528370094807485, 5.767676674365834977 ) ) ;
#68469 = CARTESIAN_POINT ( 'NONE',  ( 13.79529636645030344, 28.26208216824729647, 14.16423886937410614 ) ) ;
#68471 = CARTESIAN_POINT ( 'NONE',  ( 0.5774900079438590739, 47.64701867748817676, -5.440088680355550821 ) ) ;
#68472 = CARTESIAN_POINT ( 'NONE',  ( -4.289191146912808207E-15, 8.868033628982656680, -11.25000000000000178 ) ) ;
#68474 = CARTESIAN_POINT ( 'NONE',  ( 2.791683348922240793, 36.63393115100078035, 7.208316651077764092 ) ) ;
#68473 = CARTESIAN_POINT ( 'NONE',  ( 19.42250999205614548, 65.98035201082151957, -5.440088680355545492 ) ) ;
#68475 = CARTESIAN_POINT ( 'NONE',  ( 19.42250999205614548, 20.98035201082150891, -5.440088680355545492 ) ) ;
#68476 = PLANE ( 'NONE',  #61075 ) ;
#68477 = CARTESIAN_POINT ( 'NONE',  ( 19.84674366389459621, 63.50893115100078745, 7.409399052514197653E-17 ) ) ;
#68478 = CARTESIAN_POINT ( 'NONE',  ( 20.00000000000000711, 82.59735310505368489, -4.636598378016183908 ) ) ;
#68479 = CARTESIAN_POINT ( 'NONE',  ( 19.84674366389459266, 23.71726448433412315, -2.638427012816827677 ) ) ;
#68480 = CARTESIAN_POINT ( 'NONE',  ( 0.6178305044545818747, 53.49863466993041072, -9.382169495545419124 ) ) ;
#68481 = CARTESIAN_POINT ( 'NONE',  ( 3.795296366450306547, -14.65458449841936428, -14.16423886937410259 ) ) ;
#68482 = CARTESIAN_POINT ( 'NONE',  ( 20.88017736071110519, 45.56368534415484106, 2.639326808657452039E-16 ) ) ;
#68483 = CARTESIAN_POINT ( 'NONE',  ( 19.84674366389459621, 48.50893115100078745, 7.409399052514197653E-17 ) ) ;
#68484 = CARTESIAN_POINT ( 'NONE',  ( 6.204703633549690345, 45.76208216824729647, -14.16423886937410259 ) ) ;
#68485 = EDGE_LOOP ( 'NONE', ( #41251, #65391, #77707, #78191, #4201, #61608 ) ) ;
#68486 = CARTESIAN_POINT ( 'NONE',  ( -4.164238869374099927, 2.012082168247300906, 3.795296366450308767 ) ) ;
#68487 = CARTESIAN_POINT ( 'NONE',  ( 4.559911319644449179, 67.23035201082150536, -9.422509992056141925 ) ) ;
#68488 = DIRECTION ( 'NONE',  ( -0.9914448613738093830, 0.000000000000000000, -0.1305261922200583180 ) ) ;
#68489 = CARTESIAN_POINT ( 'NONE',  ( 24.16423886937410614, 59.30374883491397497, 8.672049930838204340E-16 ) ) ;
#68490 = CARTESIAN_POINT ( 'NONE',  ( 0.6178305044545838731, 14.74863466993041783, 9.382169495545420901 ) ) ;
#68491 = LINE ( 'NONE', #44493, #88011 ) ;
#68492 = CARTESIAN_POINT ( 'NONE',  ( 2.035157376598822676, 57.43868534415484106, -7.964842623401177768 ) ) ;
#68493 = DIRECTION ( 'NONE',  ( 0.000000000000000000, 0.000000000000000000, -1.000000000000000000 ) ) ;
#68494 = PRESENTATION_LAYER_ASSIGNMENT (  '', '', ( #22173 ) ) ;
#68495 = CARTESIAN_POINT ( 'NONE',  ( -46.75138744620058873, 100.8579332310653598, -9.074091037931069081 ) ) ;
#68496 = CARTESIAN_POINT ( 'NONE',  ( 0.5774900079438590739, 2.647018677488171434, -5.440088680355550821 ) ) ;
#68497 = CARTESIAN_POINT ( 'NONE',  ( -10.88017736071110164, 32.85535201082151957, -2.915334737309917212 ) ) ;
#68498 = CARTESIAN_POINT ( 'NONE',  ( 20.88017736071110519, 15.56368534415483751, 2.639326808657452039E-16 ) ) ;
#68499 = CARTESIAN_POINT ( 'NONE',  ( 4.559911319644449179, 28.89701867748817321, 9.422509992056141925 ) ) ;
#68500 = CARTESIAN_POINT ( 'NONE',  ( 17.20831665107776587, 62.88393115100078745, 7.208316651077764980 ) ) ;
#68501 = CARTESIAN_POINT ( 'NONE',  ( 10.00000000000000178, 50.37363466993042493, 12.81628187352647608 ) ) ;
#68502 = ORIENTED_EDGE ( 'NONE', *, *, #93027, .F. ) ;
#68503 = CARTESIAN_POINT ( 'NONE',  ( -0.8801773607111009756, 18.06368534415484106, 1.068504757029289695E-15 ) ) ;
#68504 = CARTESIAN_POINT ( 'NONE',  ( 0.6178305044545838731, 24.74863466993042493, 9.382169495545420901 ) ) ;
#68505 = CARTESIAN_POINT ( 'NONE',  ( 56.78206182523731371, 44.99999999999999289, 0.000000000000000000 ) ) ;
#68506 = VECTOR ( 'NONE', #80729, 1000.000000000000000 ) ;
#68507 = CARTESIAN_POINT ( 'NONE',  ( 12.63842701281683922, 54.55059781766745175, -9.846743663894590881 ) ) ;
#68508 = CARTESIAN_POINT ( 'NONE',  ( 10.00000000000000178, 34.31368534415484106, 10.88017736071110342 ) ) ;
#68509 = CARTESIAN_POINT ( 'NONE',  ( 21.09922568453594849, 16.20696800326375353, 6.408140936763242479 ) ) ;
#68511 = DIRECTION ( 'NONE',  ( -0.9995586998285053149, -0.02970531260815256758, 0.000000000000000000 ) ) ;
#68510 = CARTESIAN_POINT ( 'NONE',  ( 10.00000000000000178, 44.31368534415484106, 10.88017736071110342 ) ) ;
#68512 = DIRECTION ( 'NONE',  ( -0.000000000000000000, -0.000000000000000000, -1.000000000000000000 ) ) ;
#68513 = CARTESIAN_POINT ( 'NONE',  ( 13.43411237798106583, 52.66530133659708213, -12.81628187352647252 ) ) ;
#68514 = ORIENTED_EDGE ( 'NONE', *, *, #58254, .T. ) ;
#68515 = CARTESIAN_POINT ( 'NONE',  ( 1.472469842513823179, 66.42559781766745175, 4.923371831947296329 ) ) ;
#68516 = CARTESIAN_POINT ( 'NONE',  ( 0.000000000000000000, 14.49999999999999822, 0.000000000000000000 ) ) ;
#68517 = CARTESIAN_POINT ( 'NONE',  ( 7.084665262690076126, 47.02201867748818387, -10.88017736071110164 ) ) ;
#68518 = CARTESIAN_POINT ( 'NONE',  ( 21.09922568453595559, 32.04030133659708923, -6.408140936763230044 ) ) ;
#68519 = CARTESIAN_POINT ( 'NONE',  ( 17.20831665107776587, 9.133931151000787452, -7.208316651077762316 ) ) ;
#68520 = CARTESIAN_POINT ( 'NONE',  ( 17.08211943468705130, 48.47041550158063927, 12.26659068614894998 ) ) ;
#68521 = CARTESIAN_POINT ( 'NONE',  ( 2.791683348922240793, 66.63393115100079456, 7.208316651077764092 ) ) ;
#68522 = CARTESIAN_POINT ( 'NONE',  ( 17.20831665107776587, 17.88393115100078745, 7.208316651077764980 ) ) ;
#68523 = CARTESIAN_POINT ( 'NONE',  ( 19.84674366389459266, 3.717264484334118713, -2.638427012816827677 ) ) ;
#68524 = LINE ( 'NONE', #91006, #25196 ) ;
#68525 = CARTESIAN_POINT ( 'NONE',  ( 13.79529636645031943, 45.34541550158062506, -14.16423886937409904 ) ) ;
#68526 = DIRECTION ( 'NONE',  ( -0.7604059656000257128, 0.000000000000000000, -0.6494480483301898754 ) ) ;
#68527 = EDGE_CURVE ( 'NONE', #23491, #87709, #11816, .T. ) ;
#68528 = PRESENTATION_LAYER_ASSIGNMENT (  '', '', ( #6280 ) ) ;
#68529 = CARTESIAN_POINT ( 'NONE',  ( -0.8801773607111009756, 8.063685344154837509, 1.068504757029289695E-15 ) ) ;
#68530 = LINE ( 'NONE', #59, #39226 ) ;
#68531 = ORIENTED_EDGE ( 'NONE', *, *, #69799, .F. ) ;
#68532 = CARTESIAN_POINT ( 'NONE',  ( 2.035157376598822676, 7.438685344154837509, -7.964842623401177768 ) ) ;
#68533 = CARTESIAN_POINT ( 'NONE',  ( 2.917880565312948704, 67.63708216824730357, 12.26659068614894643 ) ) ;
#68534 = CARTESIAN_POINT ( 'NONE',  ( 7.361572987183169658, 49.96726448433410894, -9.846743663894592657 ) ) ;
#68535 = CARTESIAN_POINT ( 'NONE',  ( 13.43411237798105340, 45.58196800326374643, 12.81628187352647963 ) ) ;
#68536 = FACE_OUTER_BOUND ( 'NONE', #82131, .T. ) ;
#68538 = CARTESIAN_POINT ( 'NONE',  ( -0.3689425029237881626, 7.428748834913967869, 10.36894250292379027 ) ) ;
#68537 = CARTESIAN_POINT ( 'NONE',  ( -8.051738205446245189, 84.95449735710290895, -3.788866803286884632 ) ) ;
#68539 = CARTESIAN_POINT ( 'NONE',  ( 20.88017736071110875, 20.77201867748816611, -2.915334737309920765 ) ) ;
#68540 = CARTESIAN_POINT ( 'NONE',  ( 15.44008868035555793, 6.397018677488171434, -9.422509992056140149 ) ) ;
#68541 = CARTESIAN_POINT ( 'NONE',  ( 17.20831665107776587, 47.88393115100078745, 7.208316651077764980 ) ) ;
#68542 = SURFACE_STYLE_FILL_AREA ( #38538 ) ;
#68543 = CARTESIAN_POINT ( 'NONE',  ( 5.076628168052704559, 25.17559781766745175, -8.527530157486179263 ) ) ;
#68544 = CARTESIAN_POINT ( 'NONE',  ( 8.527530157486175710, 18.92559781766745175, -4.923371831947298993 ) ) ;
#68545 = VERTEX_POINT ( 'NONE', #50298 ) ;
#68546 = VECTOR ( 'NONE', #25117, 1000.000000000000000 ) ;
#68547 = EDGE_LOOP ( 'NONE', ( #10051, #52288, #30056, #83566 ) ) ;
#68548 = DIRECTION ( 'NONE',  ( -0.000000000000000000, -1.000000000000000000, -0.000000000000000000 ) ) ;
#68549 = ORIENTED_EDGE ( 'NONE', *, *, #7812, .F. ) ;
#68550 = CARTESIAN_POINT ( 'NONE',  ( 19.84674366389459266, 58.71726448433411605, -2.638427012816827677 ) ) ;
#68552 = CARTESIAN_POINT ( 'NONE',  ( 19.42250999205614548, 35.98035201082151247, -5.440088680355545492 ) ) ;
#68551 = CARTESIAN_POINT ( 'NONE',  ( 12.91533473730993009, 36.60535201082151247, -10.88017736071109987 ) ) ;
#68553 = CARTESIAN_POINT ( 'NONE',  ( 3.591859063236761518, 24.95696800326375353, 11.09922568453594849 ) ) ;
#68554 = CARTESIAN_POINT ( 'NONE',  ( 20.36894250292379382, 8.678748834913967869, 10.36894250292379205 ) ) ;
#68555 = CARTESIAN_POINT ( 'NONE',  ( 17.96484262340118221, 66.18868534415483396, -7.964842623401177768 ) ) ;
#68556 = EDGE_CURVE ( 'NONE', #13373, #107, #20082, .T. ) ;
#68557 = CARTESIAN_POINT ( 'NONE',  ( 0.6178305044545838731, 49.74863466993041072, 9.382169495545420901 ) ) ;
#68558 = VERTEX_POINT ( 'NONE', #41844 ) ;
#68559 = CARTESIAN_POINT ( 'NONE',  ( 10.00000000000000000, 44.75893115100078745, -9.846743663894594434 ) ) ;
#68560 = EDGE_CURVE ( 'NONE', #3454, #48192, #58791, .T. ) ;
#68561 = CARTESIAN_POINT ( 'NONE',  ( -0.8801773607111008646, 13.27201867748817321, 2.915334737309923430 ) ) ;
#68562 = ORIENTED_EDGE ( 'NONE', *, *, #69340, .T. ) ;
#68563 = CARTESIAN_POINT ( 'NONE',  ( 7.084665262690076126, 14.10535201082150358, 10.88017736071109987 ) ) ;
#68564 = ORIENTED_EDGE ( 'NONE', *, *, #24297, .T. ) ;
#68565 = CARTESIAN_POINT ( 'NONE',  ( 10.00000000000000178, 54.31368534415484106, 10.88017736071110342 ) ) ;
#68566 = CARTESIAN_POINT ( 'NONE',  ( 15.44008868035555260, 59.73035201082151247, 9.422509992056143702 ) ) ;
#68567 = AXIS2_PLACEMENT_3D ( 'NONE', #84284, #44776, #91769 ) ;
#68568 = FACE_OUTER_BOUND ( 'NONE', #4513, .T. ) ;
#68569 = CARTESIAN_POINT ( 'NONE',  ( 10.00000000000000178, 54.31368534415484106, 10.88017736071110342 ) ) ;
#68570 = CARTESIAN_POINT ( 'NONE',  ( -0.2418659066527703572, 53.09014588040358262, 6.114288769123046308 ) ) ;
#68571 = DIRECTION ( 'NONE',  ( 1.000000000000000000, -0.000000000000000000, -0.000000000000000000 ) ) ;
#68573 = ORIENTED_EDGE ( 'NONE', *, *, #77588, .F. ) ;
#68572 = CARTESIAN_POINT ( 'NONE',  ( 10.85666693323940102, -52.68303261961045081, 4.000000000000000000 ) ) ;
#68574 = CARTESIAN_POINT ( 'NONE',  ( 18.52753015748618282, 43.92559781766745175, -4.923371831947291888 ) ) ;
#68575 = EDGE_LOOP ( 'NONE', ( #28463, #31888, #35807, #44049, #85256, #58732 ) ) ;
#68576 = CARTESIAN_POINT ( 'NONE',  ( 0.1532563361054082862, 66.21726448433413736, 2.638427012816831674 ) ) ;
#68577 = CARTESIAN_POINT ( 'NONE',  ( 20.15039907845753930, 69.92552686551195507, -6.262539305110068177 ) ) ;
#68578 = CIRCLE ( 'NONE', #40034, 14.49999999999999822 ) ;
#68579 = CARTESIAN_POINT ( 'NONE',  ( 13.79529636645030344, 8.262082168247300018, 14.16423886937410614 ) ) ;
#68580 = CARTESIAN_POINT ( 'NONE',  ( -7.750000000000000000, 79.82179676972448590, -6.250000000000000000 ) ) ;
#68582 = CARTESIAN_POINT ( 'NONE',  ( 4.559911319644449179, 63.89701867748817676, 9.422509992056141925 ) ) ;
#68581 = CARTESIAN_POINT ( 'NONE',  ( 20.15039907845753930, 69.92552686551195507, 6.262539305110068177 ) ) ;
#68583 = CARTESIAN_POINT ( 'NONE',  ( 17.96484262340118221, 9.938685344154839285, 7.964842623401181321 ) ) ;
#68584 = CARTESIAN_POINT ( 'NONE',  ( 0.2751277870542909176, 59.36607318730130345, -6.499999999999992006 ) ) ;
#68586 = ORIENTED_EDGE ( 'NONE', *, *, #9939, .T. ) ;
#68585 = CARTESIAN_POINT ( 'NONE',  ( 3.591859063236761518, 39.95696800326375353, 11.09922568453594849 ) ) ;
#68587 = LINE ( 'NONE', #14614, #1830 ) ;
#68588 = CARTESIAN_POINT ( 'NONE',  ( 12.63842701281683034, 42.46726448433412315, 9.846743663894596210 ) ) ;
#68589 = CARTESIAN_POINT ( 'NONE',  ( 5.076628168052703671, 1.842264484334118047, 8.527530157486179263 ) ) ;
#68590 = CARTESIAN_POINT ( 'NONE',  ( 6.565887622018943937, 15.16530133659708568, 12.81628187352647430 ) ) ;
#68592 = EDGE_CURVE ( 'NONE', #30756, #52027, #57070, .T. ) ;
#68591 = CARTESIAN_POINT ( 'NONE',  ( 5.076628168052703671, 26.84226448433411960, 8.527530157486179263 ) ) ;
#68593 = AXIS2_PLACEMENT_3D ( 'NONE', #71944, #87439, #85485 ) ;
#68594 = CARTESIAN_POINT ( 'NONE',  ( -0.2002127540270186579, 69.97534054108130874, -6.181800700215005939 ) ) ;
#68595 = CARTESIAN_POINT ( 'NONE',  ( 22.81628187352647785, 11.62363466993042138, 6.195893100308588602E-16 ) ) ;
#68596 = DIRECTION ( 'NONE',  ( 1.000000000000000000, 0.000000000000000000, 0.000000000000000000 ) ) ;
#68597 = CARTESIAN_POINT ( 'NONE',  ( 2.791683348922240793, 11.63393115100078568, 7.208316651077764092 ) ) ;
#68598 = ORIENTED_EDGE ( 'NONE', *, *, #37160, .F. ) ;
#68599 = VERTEX_POINT ( 'NONE', #49808 ) ;
#68600 = CARTESIAN_POINT ( 'NONE',  ( 10.00000000000000178, 19.31368534415484106, 10.88017736071110342 ) ) ;
#68601 = CARTESIAN_POINT ( 'NONE',  ( 24.16423886937409904, 14.09541550158063217, 3.795296366450317205 ) ) ;
#68602 = CARTESIAN_POINT ( 'NONE',  ( 19.84674366389459266, 38.30059781766745175, 2.638427012816836559 ) ) ;
#68603 = CARTESIAN_POINT ( 'NONE',  ( 7.361572987183169658, 4.967264484334119601, -9.846743663894592657 ) ) ;
#68605 = CARTESIAN_POINT ( 'NONE',  ( -6.445967608602039434, -48.01283281809150338, -3.750000000000000000 ) ) ;
#68604 = CARTESIAN_POINT ( 'NONE',  ( 10.00000000000000000, 42.87363466993042493, -12.81628187352647608 ) ) ;
#68606 = CARTESIAN_POINT ( 'NONE',  ( -0.8801773607111009756, 18.06368534415484106, 1.068504757029289695E-15 ) ) ;
#68607 = FACE_OUTER_BOUND ( 'NONE', #67295, .T. ) ;
#68608 = CARTESIAN_POINT ( 'NONE',  ( 21.09922568453595559, 12.04030133659708746, -6.408140936763230044 ) ) ;
#68609 = CARTESIAN_POINT ( 'NONE',  ( 5.076628168052703671, 31.84226448433412315, 8.527530157486179263 ) ) ;
#68610 = CARTESIAN_POINT ( 'NONE',  ( 10.88017736071110164, -9.644647989178485759, 2.915334737309921209 ) ) ;
#68611 = CARTESIAN_POINT ( 'NONE',  ( 3.591859063236761518, 29.95696800326375708, 11.09922568453594849 ) ) ;
#68612 = CARTESIAN_POINT ( 'NONE',  ( 18.28836319691945889, 24.34492782695771140, 6.499999999999999112 ) ) ;
#68614 = DIRECTION ( 'NONE',  ( -0.5519369853120617009, 0.000000000000000000, 0.8338858220671657717 ) ) ;
#68613 = CARTESIAN_POINT ( 'NONE',  ( 17.96484262340118221, 39.93868534415484106, 7.964842623401181321 ) ) ;
#68615 = VECTOR ( 'NONE', #31337, 1000.000000000000000 ) ;
#68616 = CARTESIAN_POINT ( 'NONE',  ( 13.96552416078066550, 0.04962884865031113452, -4.756200848675081971 ) ) ;
#68617 = CARTESIAN_POINT ( 'NONE',  ( -0.8801773607111009756, 68.06368534415484817, 1.068504757029289695E-15 ) ) ;
#68618 = CARTESIAN_POINT ( 'NONE',  ( 7.084665262690076126, 42.02201867748816966, -10.88017736071110164 ) ) ;
#68619 = CARTESIAN_POINT ( 'NONE',  ( -0.8801773607111008646, 48.27201867748816966, 2.915334737309923430 ) ) ;
#68620 = CARTESIAN_POINT ( 'NONE',  ( 19.89103541497709671, 60.66234555792570404, -6.479102184480829862 ) ) ;
#68621 = CARTESIAN_POINT ( 'NONE',  ( 15.44008868035555793, 66.39701867748817676, -9.422509992056140149 ) ) ;
#68622 = CARTESIAN_POINT ( 'NONE',  ( 7.361572987183169658, 54.96726448433413026, -9.846743663894592657 ) ) ;
#68624 = FACE_OUTER_BOUND ( 'NONE', #58983, .T. ) ;
#68623 = CARTESIAN_POINT ( 'NONE',  ( 4.559911319644449179, 3.897018677488170990, 9.422509992056141925 ) ) ;
#68625 = CARTESIAN_POINT ( 'NONE',  ( 0.6178305044545818747, 18.49863466993041428, -9.382169495545419124 ) ) ;
#68626 = ORIENTED_EDGE ( 'NONE', *, *, #24209, .T. ) ;
#68627 = CARTESIAN_POINT ( 'NONE',  ( 2.035157376598824452, 33.68868534415484106, 7.964842623401179544 ) ) ;
#68629 = CARTESIAN_POINT ( 'NONE',  ( 19.72487221294571214, 15.71833443783937589, -6.500000000000001776 ) ) ;
#68628 = CARTESIAN_POINT ( 'NONE',  ( 7.361572987183169658, 59.96726448433410894, -9.846743663894592657 ) ) ;
#68630 = CARTESIAN_POINT ( 'NONE',  ( 19.42250999205614193, 20.14701867748817321, 5.440088680355555262 ) ) ;
#68631 = CARTESIAN_POINT ( 'NONE',  ( 12.91533473730992121, 24.52201867748816966, 10.88017736071110164 ) ) ;
#68632 = CARTESIAN_POINT ( 'NONE',  ( -2.266590686148945544, 36.38708216824730357, -7.082119434687050408 ) ) ;
#68633 = CARTESIAN_POINT ( 'NONE',  ( 0.1532563361054082862, 21.21726448433412315, 2.638427012816831674 ) ) ;
#68634 = CARTESIAN_POINT ( 'NONE',  ( 20.88017736071110164, 40.35535201082150536, 2.915334737309930979 ) ) ;
#68635 =( NAMED_UNIT ( * ) PLANE_ANGLE_UNIT ( ) SI_UNIT ( $, .RADIAN. ) );
#68636 = CARTESIAN_POINT ( 'NONE',  ( 13.79529636645031943, 5.345415501580634832, -14.16423886937409904 ) ) ;
#68637 = EDGE_CURVE ( 'NONE', #8141, #39290, #23563, .T. ) ;
#68638 = CARTESIAN_POINT ( 'NONE',  ( 2.791683348922240793, 56.63393115100078035, 7.208316651077764092 ) ) ;
#68639 = ORIENTED_EDGE ( 'NONE', *, *, #74061, .T. ) ;
#68640 = ORIENTED_EDGE ( 'NONE', *, *, #51720, .T. ) ;
#68641 = CARTESIAN_POINT ( 'NONE',  ( 24.16423886937410614, 39.30374883491396787, 8.672049930838204340E-16 ) ) ;
#68642 = CARTESIAN_POINT ( 'NONE',  ( 17.08211943468705840, 25.13708216824730357, -12.26659068614894466 ) ) ;
#68643 = CARTESIAN_POINT ( 'NONE',  ( 19.84674366389459266, 3.717264484334118713, -2.638427012816827677 ) ) ;
#68644 = CARTESIAN_POINT ( 'NONE',  ( 18.52753015748617571, 43.09226448433412315, 4.923371831947298993 ) ) ;
#68645 = CARTESIAN_POINT ( 'NONE',  ( -11.35564645740952372, -81.99443000160049166, 4.000000000000000000 ) ) ;
#68647 = CARTESIAN_POINT ( 'NONE',  ( 0.6178305044545818747, 18.49863466993041428, -9.382169495545419124 ) ) ;
#68646 = CARTESIAN_POINT ( 'NONE',  ( 17.96484262340118221, 51.18868534415483396, -7.964842623401177768 ) ) ;
#68648 = CARTESIAN_POINT ( 'NONE',  ( 17.08211943468705840, 35.13708216824730357, -12.26659068614894466 ) ) ;
#68649 = CARTESIAN_POINT ( 'NONE',  ( -0.8801773607111009756, 18.06368534415484106, 1.068504757029289695E-15 ) ) ;
#68650 = CARTESIAN_POINT ( 'NONE',  ( 4.559911319644449179, 28.89701867748817321, 9.422509992056141925 ) ) ;
#68651 =( BOUNDED_SURFACE ( )  B_SPLINE_SURFACE ( 1, 2, ( 
 ( #7434, #61880, #37930, #70885, #2893, #55380, #63359, #10374, #40875, #86860, #10863, #18366, #48846, #33825, #40387, #41864, #72327, #26344, #93368, #78367, #64331, #86372, #11344, #49340, #55873, #48356, #94842, #79839, #78863, #87344, #2403, #24895, #56845, #79356, #17874, #34320, #33343, #56367, #71851, #32861, #71381, #63837, #93862, #18859, #3860, #9886, #85880, #94351, #62871, #32365, #25870, #41384, #3361, #1908, #25390, #17392, #47861, #77205, #38729, #77694, #23742, #45736, #53230, #61222, #23248, #15745, #68735, #24714, #92700, #266, #8710, #40198, #39719, #70706, #54204, #15257, #9206, #39228, #22747, #76235, #17218, #30711, #24224, #76716, #91726, #93187, #85213, #47697, #53723, #54691, #8234, #84239, #55186, #16717, #38244, #7750, #1243, #47190, #78189, #9702, #2223, #46230, #85702, #754, #62687, #84720, #16224, #31205, #32683, #91220, #69229, #70211, #83734, #46705, #61701, #92216, #69717, #31699, #62190, #1730, #32184, #80597, #19595, #14082, #89077, #96600, #97105, #66072, #12095, #51077, #21584, #28576, #35582, #28077, #58575, #74064, #36582, #20590, #21082, #50092, #81568, #67070, #95599, #5596, #13076, #88578, #43569, #51578, #65573, #42597, #89571, #44060, #36075, #27085, #66578, #50590, #59566, #52074, #59066, #73076, #82067, #5093, #4612, #13575, #74567, #6081, #97597, #82568, #90060, #29059, #35073, #44562, #4116, #88084, #34580, #65074, #57587, #96100, #27582, #58074, #20087, #81081, #12584, #43083, #73569, #84052, #92037, #14581, #37575, #68068, #30538, #77034, #91044, #15081, #585, #75559, #91551, #31524, #75060, #16043, #62020, #16545, #83560, #61038, #46531, #98595, #39046, #23566, #7073, #69541, #31029, #92521, #45552, #30044, #38555, #60051, #68559, #76540, #37078, #24046, #83060, #67576, #6567, #1058, #98087, #52556, #46053, #15572, #54034, #45050, #60553, #22572, #23070, #8547, #53043, #76050, #61529, #7580, #53538, #54517, #29545, #85031, #90551, #22081, #38068, #8056, #91, #69050, #84544, #63975, #47517, #41517, #3030, #3508, #55523, #78019, #1557, #64471, #17535, #87482, #47020, #85525, #40525, #77511, #40023, #70526, #94489, #25527, #79498, #2049, #63009, #48497, #32511, #56018, #86517, #33968, #17038, #9028, #71984, #9522, #78510, #93512, #25038, #2546, #32004, #86020, #41018, #10504, #94978, #48002, #33479, #24549, #62508, #56977, #33003, #71024, #71520, #10025, #55008, #94004, #26481, #26007, #63504, #18015, #78999, #56501, #10997, #86992, #18499, #93013, #48990, #39545, #70033, #88962, #80967, #4494, #96482, #66447, #80479, #57473, #5478, #58953, #42971, #11483, #20470 ),
 ( #19481, #42003, #89453, #12954, #57959, #59438, #4979, #58447, #12467, #43450, #73451, #95484, #65955, #36457, #73951, #50463, #35458, #27954, #50957, #51454, #81453, #35952, #34465, #96982, #81943, #72469, #28459, #20969, #34959, #13452, #43938, #11979, #87967, #74437, #5962, #66951, #4001, #97469, #65457, #28933, #18996, #49473, #49973, #79980, #19965, #42480, #64957, #26975, #72963, #95983, #27465, #88463, #53416, #59931, #45932, #83923, #74940, #83435, #91422, #51954, #46416, #97970, #82439, #89940, #53919, #21457, #67449, #60917, #98961, #7937, #29426, #52440, #82938, #45422, #91916, #6948, #29920, #15453, #90419, #7452, #76906, #13963, #30909, #8419, #31396, #98467, #75927, #61407, #14455, #84428, #38433, #21959, #15925, #76423, #38926, #60426, #44927, #44438, #69413, #90919, #6444, #36952, #75434, #14955, #37455, #67943, #22449, #68931, #68441, #23440, #52922, #37949, #22950, #30417, #461, #936, #48864, #31886, #3380, #86875, #62384, #93387, #92889, #1433, #17413, #46897, #24421, #55894, #25407, #79374, #54885, #17891, #39418, #77388, #71869, #47879, #69913, #78383, #10879, #10390, #41403, #24912, #84908, #78879, #9903, #92403, #16420, #18385, #85401, #93880, #47386, #16913, #63855, #86390, #8901, #77888, #70900, #48375, #61896, #23926, #54397, #9400, #94369, #70407, #33360, #55396, #85896, #1925, #25887, #39901, #32383, #40894, #62888, #40406, #2420, #32877, #63375, #71395, #2909, #56386, #51335, #4376, #73335, #58825, #43333, #34841, #96860, #80848, #34343, #65831, #27836, #88840, #43819, #88347, #72347, #73825, #19845, #66325, #64837, #50337, #18877, #87845, #95862, #27345, #4862, #58323, #35338, #96363, #12833, #95356, #81817, #13335, #5358, #56862, #3879, #35837, #42365, #74315, #89333, #11857, #65336, #28335, #20843, #57838, #33843, #26855, #87363, #64352, #20348, #72838, #94860, #12345, #50844, #81336, #57352, #42852, #26363, #19365, #49359, #79861, #49848, #11364, #41883, #80357, #36331, #60312, #44806, #37830, #90804, #74818, #98839, #84315, #22332, #52320, #91297, #37338, #59318, #66826, #6323, #36833, #29312, #82316, #38316, #7329, #67828, #90302, #83313, #53300, #67324, #44317, #22821, #45816, #29803, #97348, #68320, #82813, #61292, #53804, #14837, #97847, #30294, #6822, #59808, #45311, #83808, #98346, #52806, #15815, #91801, #60797, #21837, #15334, #76304, #89817, #75807, #7821, #28819, #23323, #13836, #21338, #5841, #68812, #51828, #14333, #345, #30787, #46301, #75312, #39305, #69797, #32263, #78765, #92775, #16793, #2302, #77276, #93269, #33249, #76788, #17780, #63742, #18266, #85285, #62768, #48255 ) ),
 .UNSPECIFIED., .F., .F., .F. ) 
 B_SPLINE_SURFACE_WITH_KNOTS ( ( 2, 2 ),
 ( 3, 2, 2, 2, 2, 2, 2, 2, 2, 2, 2, 2, 2, 2, 2, 2, 2, 2, 2, 2, 2, 2, 2, 2, 2, 2, 2, 2, 2, 2, 2, 2, 2, 2, 2, 2, 2, 2, 2, 2, 2, 2, 2, 2, 2, 2, 2, 2, 2, 2, 2, 2, 2, 2, 2, 2, 2, 2, 2, 2, 2, 2, 2, 2, 2, 2, 2, 2, 2, 2, 2, 2, 2, 2, 2, 2, 2, 2, 2, 2, 2, 2, 2, 2, 2, 2, 2, 2, 2, 2, 2, 2, 2, 2, 2, 2, 2, 2, 2, 2, 2, 2, 2, 2, 2, 2, 2, 2, 2, 2, 2, 2, 2, 2, 2, 2, 2, 2, 2, 2, 2, 2, 2, 2, 2, 2, 2, 2, 2, 2, 2, 2, 2, 2, 2, 2, 2, 2, 2, 2, 2, 2, 2, 2, 2, 2, 2, 2, 2, 2, 2, 2, 2, 2, 2, 2, 2, 2, 2, 2, 2, 2, 3 ),
 ( 0.000000000000000000, 1.000000000000000000 ),
 ( 0.000000000000000000, 0.005952380952380952051, 0.01190476190476190410, 0.01785714285714285615, 0.02380952380952380820, 0.02976190476190476025, 0.03571428571428571230, 0.04166666666666666435, 0.04761904761904761640, 0.05357142857142856845, 0.05952380952380952051, 0.06547619047619047949, 0.07142857142857142461, 0.07738095238095238360, 0.08333333333333332871, 0.08928571428571428770, 0.09523809523809523281, 0.1011904761904761918, 0.1071428571428571369, 0.1130952380952380959, 0.1190476190476190410, 0.1250000000000000000, 0.1309523809523809590, 0.1369047619047619180, 0.1428571428571428492, 0.1488095238095238082, 0.1547619047619047672, 0.1607142857142857262, 0.1666666666666666574, 0.1726190476190476164, 0.1785714285714285754, 0.1845238095238095344, 0.1904761904761904656, 0.1964285714285714246, 0.2023809523809523836, 0.2083333333333333426, 0.2142857142857142738, 0.2202380952380952328, 0.2261904761904761918, 0.2321428571428571508, 0.2380952380952380820, 0.2440476190476190410, 0.2500000000000000000, 0.2559523809523809312, 0.2619047619047619180, 0.2678571428571428492, 0.2738095238095238360, 0.2797619047619047672, 0.2857142857142856984, 0.2916666666666666852, 0.2976190476190476164, 0.3035714285714285476, 0.3095238095238095344, 0.3154761904761904656, 0.3214285714285714524, 0.3273809523809523836, 0.3333333333333333148, 0.3392857142857143016, 0.3452380952380952328, 0.3511904761904761640, 0.3571428571428571508, 0.3630952380952380820, 0.3690476190476190688, 0.3750000000000000000, 0.3809523809523809312, 0.3869047619047619180, 0.3928571428571428492, 0.3988095238095238360, 0.4047619047619047672, 0.4107142857142856984, 0.4166666666666666852, 0.4226190476190476164, 0.4285714285714285476, 0.4345238095238095344, 0.4404761904761904656, 0.4464285714285714524, 0.4523809523809523836, 0.4583333333333333148, 0.4642857142857143016, 0.4702380952380952328, 0.4761904761904761640, 0.4821428571428571508, 0.4880952380952380820, 0.4940476190476190688, 0.5000000000000000000, 0.5059523809523809312, 0.5119047619047618625, 0.5178571428571429047, 0.5238095238095238360, 0.5297619047619047672, 0.5357142857142856984, 0.5416666666666666297, 0.5476190476190476719, 0.5535714285714286031, 0.5595238095238095344, 0.5654761904761904656, 0.5714285714285713969, 0.5773809523809523281, 0.5833333333333333703, 0.5892857142857143016, 0.5952380952380952328, 0.6011904761904761640, 0.6071428571428570953, 0.6130952380952381375, 0.6190476190476190688, 0.6250000000000000000, 0.6309523809523809312, 0.6369047619047618625, 0.6428571428571429047, 0.6488095238095238360, 0.6547619047619047672, 0.6607142857142856984, 0.6666666666666666297, 0.6726190476190476719, 0.6785714285714286031, 0.6845238095238095344, 0.6904761904761904656, 0.6964285714285713969, 0.7023809523809523281, 0.7083333333333333703, 0.7142857142857143016, 0.7202380952380952328, 0.7261904761904761640, 0.7321428571428570953, 0.7380952380952381375, 0.7440476190476190688, 0.7500000000000000000, 0.7559523809523809312, 0.7619047619047618625, 0.7678571428571429047, 0.7738095238095238360, 0.7797619047619047672, 0.7857142857142856984, 0.7916666666666666297, 0.7976190476190476719, 0.8035714285714286031, 0.8095238095238095344, 0.8154761904761904656, 0.8214285714285713969, 0.8273809523809523281, 0.8333333333333333703, 0.8392857142857143016, 0.8452380952380952328, 0.8511904761904761640, 0.8571428571428570953, 0.8630952380952381375, 0.8690476190476190688, 0.8750000000000000000, 0.8809523809523809312, 0.8869047619047618625, 0.8928571428571429047, 0.8988095238095238360, 0.9047619047619047672, 0.9107142857142856984, 0.9166666666666666297, 0.9226190476190476719, 0.9285714285714286031, 0.9345238095238095344, 0.9404761904761904656, 0.9464285714285713969, 0.9523809523809523281, 0.9583333333333333703, 0.9642857142857143016 ),
 .UNSPECIFIED. ) 
 GEOMETRIC_REPRESENTATION_ITEM ( )  RATIONAL_B_SPLINE_SURFACE ( (
 ( 1.000000000000000000, 0.9659258262890683122, 1.000000000000000000, 0.9659258262890683122, 1.000000000000000000, 0.9659258262890683122, 1.000000000000000000, 0.9659258262890683122, 1.000000000000000000, 0.9659258262890683122, 1.000000000000000000, 0.9659258262890683122, 1.000000000000000000, 0.9659258262890683122, 1.000000000000000000, 0.9659258262890683122, 1.000000000000000000, 0.9659258262890683122, 1.000000000000000000, 0.9659258262890683122, 1.000000000000000000, 0.9659258262890683122, 1.000000000000000000, 0.9659258262890683122, 1.000000000000000000, 0.9659258262890683122, 1.000000000000000000, 0.9659258262890683122, 1.000000000000000000, 0.9659258262890683122, 1.000000000000000000, 0.9659258262890683122, 1.000000000000000000, 0.9659258262890683122, 1.000000000000000000, 0.9659258262890683122, 1.000000000000000000, 0.9659258262890683122, 1.000000000000000000, 0.9659258262890683122, 1.000000000000000000, 0.9659258262890683122, 1.000000000000000000, 0.9659258262890683122, 1.000000000000000000, 0.9659258262890683122, 1.000000000000000000, 0.9659258262890683122, 1.000000000000000000, 0.9659258262890683122, 1.000000000000000000, 0.9659258262890683122, 1.000000000000000000, 0.9659258262890683122, 1.000000000000000000, 0.9659258262890683122, 1.000000000000000000, 0.9659258262890683122, 1.000000000000000000, 0.9659258262890683122, 1.000000000000000000, 0.9659258262890683122, 1.000000000000000000, 0.9659258262890683122, 1.000000000000000000, 0.9659258262890683122, 1.000000000000000000, 0.9659258262890683122, 1.000000000000000000, 0.9659258262890683122, 1.000000000000000000, 0.9659258262890683122, 1.000000000000000000, 0.9659258262890683122, 1.000000000000000000, 0.9659258262890683122, 1.000000000000000000, 0.9659258262890683122, 1.000000000000000000, 0.9659258262890683122, 1.000000000000000000, 0.9659258262890683122, 1.000000000000000000, 0.9659258262890683122, 1.000000000000000000, 0.9659258262890683122, 1.000000000000000000, 0.9659258262890683122, 1.000000000000000000, 0.9659258262890683122, 1.000000000000000000, 0.9659258262890683122, 1.000000000000000000, 0.9659258262890683122, 1.000000000000000000, 0.9659258262890683122, 1.000000000000000000, 0.9659258262890683122, 1.000000000000000000, 0.9659258262890683122, 1.000000000000000000, 0.9659258262890683122, 1.000000000000000000, 0.9659258262890683122, 1.000000000000000000, 0.9659258262890683122, 1.000000000000000000, 0.9659258262890683122, 1.000000000000000000, 0.9659258262890683122, 1.000000000000000000, 0.9659258262890683122, 1.000000000000000000, 0.9659258262890683122, 1.000000000000000000, 0.9659258262890683122, 1.000000000000000000, 0.9659258262890683122, 1.000000000000000000, 0.9659258262890683122, 1.000000000000000000, 0.9659258262890683122, 1.000000000000000000, 0.9659258262890683122, 1.000000000000000000, 0.9659258262890683122, 1.000000000000000000, 0.9659258262890683122, 1.000000000000000000, 0.9659258262890683122, 1.000000000000000000, 0.9659258262890683122, 1.000000000000000000, 0.9659258262890683122, 1.000000000000000000, 0.9659258262890683122, 1.000000000000000000, 0.9659258262890683122, 1.000000000000000000, 0.9659258262890683122, 1.000000000000000000, 0.9659258262890683122, 1.000000000000000000, 0.9659258262890683122, 1.000000000000000000, 0.9659258262890683122, 1.000000000000000000, 0.9659258262890683122, 1.000000000000000000, 0.9659258262890683122, 1.000000000000000000, 0.9659258262890683122, 1.000000000000000000, 0.9659258262890683122, 1.000000000000000000, 0.9659258262890683122, 1.000000000000000000, 0.9659258262890683122, 1.000000000000000000, 0.9659258262890683122, 1.000000000000000000, 0.9659258262890683122, 1.000000000000000000, 0.9659258262890683122, 1.000000000000000000, 0.9659258262890683122, 1.000000000000000000, 0.9659258262890683122, 1.000000000000000000, 0.9659258262890683122, 1.000000000000000000, 0.9659258262890683122, 1.000000000000000000, 0.9659258262890683122, 1.000000000000000000, 0.9659258262890683122, 1.000000000000000000, 0.9659258262890683122, 1.000000000000000000, 0.9659258262890683122, 1.000000000000000000, 0.9659258262890683122, 1.000000000000000000, 0.9659258262890683122, 1.000000000000000000, 0.9659258262890683122, 1.000000000000000000, 0.9659258262890683122, 1.000000000000000000, 0.9659258262890683122, 1.000000000000000000, 0.9659258262890683122, 1.000000000000000000, 0.9659258262890683122, 1.000000000000000000, 0.9659258262890683122, 1.000000000000000000, 0.9659258262890683122, 1.000000000000000000, 0.9659258262890683122, 1.000000000000000000, 0.9659258262890683122, 1.000000000000000000, 0.9659258262890683122, 1.000000000000000000, 0.9659258262890683122, 1.000000000000000000, 0.9659258262890683122, 1.000000000000000000, 0.9659258262890683122, 1.000000000000000000, 0.9659258262890683122, 1.000000000000000000, 0.9659258262890683122, 1.000000000000000000, 0.9659258262890683122, 1.000000000000000000, 0.9659258262890683122, 1.000000000000000000, 0.9659258262890683122, 1.000000000000000000, 0.9659258262890683122, 1.000000000000000000, 0.9659258262890683122, 1.000000000000000000, 0.9659258262890683122, 1.000000000000000000, 0.9659258262890683122, 1.000000000000000000, 0.9659258262890683122, 1.000000000000000000, 0.9659258262890683122, 1.000000000000000000, 0.9659258262890683122, 1.000000000000000000, 0.9659258262890683122, 1.000000000000000000, 0.9659258262890683122, 1.000000000000000000, 0.9659258262890683122, 1.000000000000000000, 0.9659258262890683122, 1.000000000000000000, 0.9659258262890683122, 1.000000000000000000, 0.9659258262890683122, 1.000000000000000000, 0.9659258262890683122, 1.000000000000000000, 0.9659258262890683122, 1.000000000000000000, 0.9659258262890683122, 1.000000000000000000, 0.9659258262890683122, 1.000000000000000000, 0.9659258262890683122, 1.000000000000000000, 0.9659258262890683122, 1.000000000000000000, 0.9659258262890683122, 1.000000000000000000, 0.9659258262890683122, 1.000000000000000000, 0.9659258262890683122, 1.000000000000000000, 0.9659258262890683122, 1.000000000000000000, 0.9659258262890683122, 1.000000000000000000, 0.9659258262890683122, 1.000000000000000000, 0.9659258262890683122, 1.000000000000000000, 0.9659258262890683122, 1.000000000000000000, 0.9659258262890683122, 1.000000000000000000, 0.9659258262890683122, 1.000000000000000000, 0.9659258262890683122, 1.000000000000000000, 0.9659258262890683122, 1.000000000000000000, 0.9659258262890683122, 1.000000000000000000, 0.9659258262890683122, 1.000000000000000000, 0.9659258262890683122, 1.000000000000000000, 0.9659258262890683122, 1.000000000000000000, 0.9659258262890683122, 1.000000000000000000, 0.9659258262890683122, 1.000000000000000000, 0.9659258262890683122, 1.000000000000000000, 0.9659258262890683122, 1.000000000000000000, 0.9659258262890683122, 1.000000000000000000, 0.9659258262890683122, 1.000000000000000000, 0.9659258262890683122, 1.000000000000000000, 0.9659258262890683122, 1.000000000000000000, 0.9659258262890683122, 1.000000000000000000, 0.9659258262890683122, 1.000000000000000000, 0.9659258262890683122, 1.000000000000000000, 0.9659258262890683122, 1.000000000000000000, 0.9659258262890683122, 1.000000000000000000, 0.9659258262890683122, 1.000000000000000000, 0.9659258262890683122, 1.000000000000000000, 0.9659258262890683122, 1.000000000000000000, 0.9659258262890683122, 1.000000000000000000),
 ( 1.000000000000000000, 0.9659258262890683122, 1.000000000000000000, 0.9659258262890683122, 1.000000000000000000, 0.9659258262890683122, 1.000000000000000000, 0.9659258262890683122, 1.000000000000000000, 0.9659258262890683122, 1.000000000000000000, 0.9659258262890683122, 1.000000000000000000, 0.9659258262890683122, 1.000000000000000000, 0.9659258262890683122, 1.000000000000000000, 0.9659258262890683122, 1.000000000000000000, 0.9659258262890683122, 1.000000000000000000, 0.9659258262890683122, 1.000000000000000000, 0.9659258262890683122, 1.000000000000000000, 0.9659258262890683122, 1.000000000000000000, 0.9659258262890683122, 1.000000000000000000, 0.9659258262890683122, 1.000000000000000000, 0.9659258262890683122, 1.000000000000000000, 0.9659258262890683122, 1.000000000000000000, 0.9659258262890683122, 1.000000000000000000, 0.9659258262890683122, 1.000000000000000000, 0.9659258262890683122, 1.000000000000000000, 0.9659258262890683122, 1.000000000000000000, 0.9659258262890683122, 1.000000000000000000, 0.9659258262890683122, 1.000000000000000000, 0.9659258262890683122, 1.000000000000000000, 0.9659258262890683122, 1.000000000000000000, 0.9659258262890683122, 1.000000000000000000, 0.9659258262890683122, 1.000000000000000000, 0.9659258262890683122, 1.000000000000000000, 0.9659258262890683122, 1.000000000000000000, 0.9659258262890683122, 1.000000000000000000, 0.9659258262890683122, 1.000000000000000000, 0.9659258262890683122, 1.000000000000000000, 0.9659258262890683122, 1.000000000000000000, 0.9659258262890683122, 1.000000000000000000, 0.9659258262890683122, 1.000000000000000000, 0.9659258262890683122, 1.000000000000000000, 0.9659258262890683122, 1.000000000000000000, 0.9659258262890683122, 1.000000000000000000, 0.9659258262890683122, 1.000000000000000000, 0.9659258262890683122, 1.000000000000000000, 0.9659258262890683122, 1.000000000000000000, 0.9659258262890683122, 1.000000000000000000, 0.9659258262890683122, 1.000000000000000000, 0.9659258262890683122, 1.000000000000000000, 0.9659258262890683122, 1.000000000000000000, 0.9659258262890683122, 1.000000000000000000, 0.9659258262890683122, 1.000000000000000000, 0.9659258262890683122, 1.000000000000000000, 0.9659258262890683122, 1.000000000000000000, 0.9659258262890683122, 1.000000000000000000, 0.9659258262890683122, 1.000000000000000000, 0.9659258262890683122, 1.000000000000000000, 0.9659258262890683122, 1.000000000000000000, 0.9659258262890683122, 1.000000000000000000, 0.9659258262890683122, 1.000000000000000000, 0.9659258262890683122, 1.000000000000000000, 0.9659258262890683122, 1.000000000000000000, 0.9659258262890683122, 1.000000000000000000, 0.9659258262890683122, 1.000000000000000000, 0.9659258262890683122, 1.000000000000000000, 0.9659258262890683122, 1.000000000000000000, 0.9659258262890683122, 1.000000000000000000, 0.9659258262890683122, 1.000000000000000000, 0.9659258262890683122, 1.000000000000000000, 0.9659258262890683122, 1.000000000000000000, 0.9659258262890683122, 1.000000000000000000, 0.9659258262890683122, 1.000000000000000000, 0.9659258262890683122, 1.000000000000000000, 0.9659258262890683122, 1.000000000000000000, 0.9659258262890683122, 1.000000000000000000, 0.9659258262890683122, 1.000000000000000000, 0.9659258262890683122, 1.000000000000000000, 0.9659258262890683122, 1.000000000000000000, 0.9659258262890683122, 1.000000000000000000, 0.9659258262890683122, 1.000000000000000000, 0.9659258262890683122, 1.000000000000000000, 0.9659258262890683122, 1.000000000000000000, 0.9659258262890683122, 1.000000000000000000, 0.9659258262890683122, 1.000000000000000000, 0.9659258262890683122, 1.000000000000000000, 0.9659258262890683122, 1.000000000000000000, 0.9659258262890683122, 1.000000000000000000, 0.9659258262890683122, 1.000000000000000000, 0.9659258262890683122, 1.000000000000000000, 0.9659258262890683122, 1.000000000000000000, 0.9659258262890683122, 1.000000000000000000, 0.9659258262890683122, 1.000000000000000000, 0.9659258262890683122, 1.000000000000000000, 0.9659258262890683122, 1.000000000000000000, 0.9659258262890683122, 1.000000000000000000, 0.9659258262890683122, 1.000000000000000000, 0.9659258262890683122, 1.000000000000000000, 0.9659258262890683122, 1.000000000000000000, 0.9659258262890683122, 1.000000000000000000, 0.9659258262890683122, 1.000000000000000000, 0.9659258262890683122, 1.000000000000000000, 0.9659258262890683122, 1.000000000000000000, 0.9659258262890683122, 1.000000000000000000, 0.9659258262890683122, 1.000000000000000000, 0.9659258262890683122, 1.000000000000000000, 0.9659258262890683122, 1.000000000000000000, 0.9659258262890683122, 1.000000000000000000, 0.9659258262890683122, 1.000000000000000000, 0.9659258262890683122, 1.000000000000000000, 0.9659258262890683122, 1.000000000000000000, 0.9659258262890683122, 1.000000000000000000, 0.9659258262890683122, 1.000000000000000000, 0.9659258262890683122, 1.000000000000000000, 0.9659258262890683122, 1.000000000000000000, 0.9659258262890683122, 1.000000000000000000, 0.9659258262890683122, 1.000000000000000000, 0.9659258262890683122, 1.000000000000000000, 0.9659258262890683122, 1.000000000000000000, 0.9659258262890683122, 1.000000000000000000, 0.9659258262890683122, 1.000000000000000000, 0.9659258262890683122, 1.000000000000000000, 0.9659258262890683122, 1.000000000000000000, 0.9659258262890683122, 1.000000000000000000, 0.9659258262890683122, 1.000000000000000000, 0.9659258262890683122, 1.000000000000000000, 0.9659258262890683122, 1.000000000000000000, 0.9659258262890683122, 1.000000000000000000, 0.9659258262890683122, 1.000000000000000000, 0.9659258262890683122, 1.000000000000000000, 0.9659258262890683122, 1.000000000000000000, 0.9659258262890683122, 1.000000000000000000, 0.9659258262890683122, 1.000000000000000000, 0.9659258262890683122, 1.000000000000000000, 0.9659258262890683122, 1.000000000000000000, 0.9659258262890683122, 1.000000000000000000, 0.9659258262890683122, 1.000000000000000000, 0.9659258262890683122, 1.000000000000000000, 0.9659258262890683122, 1.000000000000000000, 0.9659258262890683122, 1.000000000000000000, 0.9659258262890683122, 1.000000000000000000, 0.9659258262890683122, 1.000000000000000000, 0.9659258262890683122, 1.000000000000000000, 0.9659258262890683122, 1.000000000000000000, 0.9659258262890683122, 1.000000000000000000, 0.9659258262890683122, 1.000000000000000000, 0.9659258262890683122, 1.000000000000000000, 0.9659258262890683122, 1.000000000000000000, 0.9659258262890683122, 1.000000000000000000, 0.9659258262890683122, 1.000000000000000000, 0.9659258262890683122, 1.000000000000000000, 0.9659258262890683122, 1.000000000000000000, 0.9659258262890683122, 1.000000000000000000, 0.9659258262890683122, 1.000000000000000000, 0.9659258262890683122, 1.000000000000000000, 0.9659258262890683122, 1.000000000000000000, 0.9659258262890683122, 1.000000000000000000, 0.9659258262890683122, 1.000000000000000000, 0.9659258262890683122, 1.000000000000000000, 0.9659258262890683122, 1.000000000000000000, 0.9659258262890683122, 1.000000000000000000, 0.9659258262890683122, 1.000000000000000000, 0.9659258262890683122, 1.000000000000000000, 0.9659258262890683122, 1.000000000000000000, 0.9659258262890683122, 1.000000000000000000, 0.9659258262890683122, 1.000000000000000000, 0.9659258262890683122, 1.000000000000000000, 0.9659258262890683122, 1.000000000000000000) ) ) 
 REPRESENTATION_ITEM ( '' )  SURFACE ( )  );
#68652 = CARTESIAN_POINT ( 'NONE',  ( 18.04007052943771683, 53.01528370094807485, 5.767676674365856293 ) ) ;
#68653 = CARTESIAN_POINT ( 'NONE',  ( 2.035157376598822676, 52.43868534415483396, -7.964842623401177768 ) ) ;
#68654 = AXIS2_PLACEMENT_3D ( 'NONE', #83375, #92349, #98408 ) ;
#68655 = CARTESIAN_POINT ( 'NONE',  ( -4.923371831947302546, -29.82440218233254470, -8.527530157486173934 ) ) ;
#68656 = EDGE_LOOP ( 'NONE', ( #86238, #51876, #73095, #76772 ) ) ;
#68657 = DIRECTION ( 'NONE',  ( 0.000000000000000000, -4.510281037539694659E-14, 1.000000000000000000 ) ) ;
#68658 = ORIENTED_EDGE ( 'NONE', *, *, #49456, .T. ) ;
#68659 = CARTESIAN_POINT ( 'NONE',  ( -0.2418659066527775181, 13.09014588040356841, 6.114288769123032985 ) ) ;
#68660 = DIRECTION ( 'NONE',  ( 0.000000000000000000, -0.000000000000000000, 1.000000000000000000 ) ) ;
#68661 = AXIS2_PLACEMENT_3D ( 'NONE', #83302, #7316, #13327 ) ;
#68662 = EDGE_LOOP ( 'NONE', ( #84780, #330, #43165, #19145 ) ) ;
#68663 = CARTESIAN_POINT ( 'NONE',  ( 0.1129803114748898080, 19.29427333184091609, -6.480634945678687586 ) ) ;
#68665 = CARTESIAN_POINT ( 'NONE',  ( 13.79529636645030344, 63.26208216824730357, 14.16423886937410614 ) ) ;
#68664 = CARTESIAN_POINT ( 'NONE',  ( 20.36894250292379738, 59.92874883491397497, -10.36894250292379027 ) ) ;
#68667 = CARTESIAN_POINT ( 'NONE',  ( 17.20831665107776587, 62.88393115100078745, 7.208316651077764980 ) ) ;
#68666 = CARTESIAN_POINT ( 'NONE',  ( 2.791683348922237240, 20.38393115100078745, -7.208316651077763204 ) ) ;
#68668 = CARTESIAN_POINT ( 'NONE',  ( -0.8801773607111009756, 68.06368534415484817, 1.068504757029289695E-15 ) ) ;
#68669 = DIRECTION ( 'NONE',  ( -0.000000000000000000, -0.000000000000000000, -1.000000000000000000 ) ) ;
#68670 = EDGE_CURVE ( 'NONE', #92829, #98109, #35671, .T. ) ;
#68671 = CARTESIAN_POINT ( 'NONE',  ( 3.434112377981060948, 25.58196800326376419, 12.81628187352647430 ) ) ;
#68672 = ORIENTED_EDGE ( 'NONE', *, *, #1855, .T. ) ;
#68673 = CARTESIAN_POINT ( 'NONE',  ( 13.79529636645030344, 33.26208216824730357, 14.16423886937410614 ) ) ;
#68674 = EDGE_CURVE ( 'NONE', #17007, #39149, #2225, .T. ) ;
#68675 = CARTESIAN_POINT ( 'NONE',  ( 24.16423886937410614, 49.51208216824730357, -3.795296366450302550 ) ) ;
#68676 = VERTEX_POINT ( 'NONE', #27799 ) ;
#68677 = CARTESIAN_POINT ( 'NONE',  ( 22.81628187352647785, 61.41530133659709634, 3.434112377981063169 ) ) ;
#68678 = CARTESIAN_POINT ( 'NONE',  ( -0.8801773607111009756, 28.06368534415484106, 1.068504757029289695E-15 ) ) ;
#68679 = CARTESIAN_POINT ( 'NONE',  ( 17.20831665107776587, 47.88393115100078745, 7.208316651077764980 ) ) ;
#68680 = CARTESIAN_POINT ( 'NONE',  ( 2.035157376598824452, 23.68868534415484461, 7.964842623401179544 ) ) ;
#68681 = DIRECTION ( 'NONE',  ( 0.9996573249755575929, 0.000000000000000000, -0.02617694830786282401 ) ) ;
#68682 = CARTESIAN_POINT ( 'NONE',  ( -6.871316085749032965, -73.24163895400424451, 2.499999999999998224 ) ) ;
#68683 = CARTESIAN_POINT ( 'NONE',  ( 0.1532563361054083140, 61.00893115100078745, 1.131784320476157264E-15 ) ) ;
#68684 = CARTESIAN_POINT ( 'NONE',  ( 10.00000000000000000, 44.75893115100078745, -9.846743663894594434 ) ) ;
#68685 = LINE ( 'NONE', #67202, #36072 ) ;
#68686 = CARTESIAN_POINT ( 'NONE',  ( 0.2751277870542965243, 3.218334437839379891, 6.500000000000000888 ) ) ;
#68687 = CARTESIAN_POINT ( 'NONE',  ( 12.63842701281683034, 2.467264484334118269, 9.846743663894596210 ) ) ;
#68688 = CARTESIAN_POINT ( 'NONE',  ( 18.29284471827479663, 20.40189080397285437, -6.500000000000035527 ) ) ;
#68689 = ORIENTED_EDGE ( 'NONE', *, *, #97764, .F. ) ;
#68690 = CARTESIAN_POINT ( 'NONE',  ( 19.65595514172846947, 85.79709332851908243, 5.361975859778444153 ) ) ;
#68691 = CARTESIAN_POINT ( 'NONE',  ( 7.361572987183170547, 32.05059781766745175, 9.846743663894590881 ) ) ;
#68692 = DIRECTION ( 'NONE',  ( -1.257568779154408793E-17, -1.000000000000000000, 0.000000000000000000 ) ) ;
#68693 = CARTESIAN_POINT ( 'NONE',  ( 22.81628187352647785, 31.62363466993042138, 6.195893100308588602E-16 ) ) ;
#68694 = DIRECTION ( 'NONE',  ( 1.257568779154408793E-17, 1.000000000000000000, -0.000000000000000000 ) ) ;
#68695 = CARTESIAN_POINT ( 'NONE',  ( -3.999999999999999112, 0.2999999999999982125, 0.000000000000000000 ) ) ;
#68696 = VERTEX_POINT ( 'NONE', #50810 ) ;
#68697 = DIRECTION ( 'NONE',  ( 0.000000000000000000, 0.000000000000000000, 1.000000000000000000 ) ) ;
#68698 = DIRECTION ( 'NONE',  ( 0.000000000000000000, 1.000000000000000000, 0.000000000000000000 ) ) ;
#68699 = CARTESIAN_POINT ( 'NONE',  ( 19.84674366389459621, 43.50893115100078745, 7.409399052514197653E-17 ) ) ;
#68700 = CARTESIAN_POINT ( 'NONE',  ( -2.266590686148945544, 32.22041550158063927, 7.082119434687048631 ) ) ;
#68701 = CARTESIAN_POINT ( 'NONE',  ( 0.1532563361054082862, 56.21726448433411605, 2.638427012816831674 ) ) ;
#68702 = CARTESIAN_POINT ( 'NONE',  ( 17.39651004071841811, 2.935752660568277328, 6.500000000000002665 ) ) ;
#68703 = CARTESIAN_POINT ( 'NONE',  ( 19.84674366389459266, 8.717264484334116048, -2.638427012816827677 ) ) ;
#68704 = CARTESIAN_POINT ( 'NONE',  ( -4.164238869374098151, 1.595415501580634388, -3.795296366450310543 ) ) ;
#68705 = CARTESIAN_POINT ( 'NONE',  ( 0.1532563361054100626, 50.80059781766745175, -2.638427012816831230 ) ) ;
#68707 = EDGE_CURVE ( 'NONE', #63596, #3959, #39539, .T. ) ;
#68706 = CARTESIAN_POINT ( 'NONE',  ( 4.559911319644449179, 52.23035201082151247, -9.422509992056141925 ) ) ;
#68708 = CARTESIAN_POINT ( 'NONE',  ( 10.00000000000000000, 44.75893115100078745, -9.846743663894594434 ) ) ;
#68709 = CARTESIAN_POINT ( 'NONE',  ( 0.8217048220045788387, 0.04962895218885213927, -14.73031263975987493 ) ) ;
#68710 = CARTESIAN_POINT ( 'NONE',  ( 2.035157376598822676, 47.43868534415484817, -7.964842623401177768 ) ) ;
#68711 = VERTEX_POINT ( 'NONE', #72797 ) ;
#68712 = DIRECTION ( 'NONE',  ( -0.5905099943842175847, -0.8070303256584298035, 0.000000000000000000 ) ) ;
#68713 = CARTESIAN_POINT ( 'NONE',  ( 4.559911319644449179, 27.23035201082150536, -9.422509992056141925 ) ) ;
#68714 = AXIS2_PLACEMENT_3D ( 'NONE', #55952, #69475, #46955 ) ;
#68716 = CARTESIAN_POINT ( 'NONE',  ( 10.00000000000000178, 59.31368534415484106, 10.88017736071110342 ) ) ;
#68715 = CARTESIAN_POINT ( 'NONE',  ( -2.816281873526473856, -0.8763653300695799508, 9.499525473075851096E-16 ) ) ;
#68717 = DIRECTION ( 'NONE',  ( -0.000000000000000000, -1.000000000000000000, -0.000000000000000000 ) ) ;
#68718 = ADVANCED_FACE ( 'NONE', ( #89298 ), #3841, .F. ) ;
#68719 = CARTESIAN_POINT ( 'NONE',  ( 4.559911319644449179, 68.89701867748817676, 9.422509992056141925 ) ) ;
#68721 = VECTOR ( 'NONE', #15391, 1000.000000000000114 ) ;
#68720 = CARTESIAN_POINT ( 'NONE',  ( 13.14228782657339956, 0.5000000000000004441, -7.230509711182238064 ) ) ;
#68723 = CARTESIAN_POINT ( 'NONE',  ( -46.44000000000001194, 100.8660254037844339, 9.500000000000000000 ) ) ;
#68722 = CARTESIAN_POINT ( 'NONE',  ( 17.96484262340118221, 36.18868534415484106, -7.964842623401177768 ) ) ;
#68724 = CARTESIAN_POINT ( 'NONE',  ( 5.076628168052704559, 15.17559781766745175, -8.527530157486179263 ) ) ;
#68725 = CARTESIAN_POINT ( 'NONE',  ( 14.92337183194729633, 37.67559781766745175, 8.527530157486181039 ) ) ;
#68726 =( NAMED_UNIT ( * ) PLANE_ANGLE_UNIT ( ) SI_UNIT ( $, .RADIAN. ) );
#68727 = CARTESIAN_POINT ( 'NONE',  ( -3.795296366450322534, 15.76208216824730535, -14.16423886937409904 ) ) ;
#68728 = CARTESIAN_POINT ( 'NONE',  ( 3.591859063236761518, -0.04303199673624671928, 11.09922568453594849 ) ) ;
#68729 = VECTOR ( 'NONE', #92165, 1000.000000000000000 ) ;
#68731 = DIRECTION ( 'NONE',  ( -0.000000000000000000, -0.000000000000000000, -1.000000000000000000 ) ) ;
#68730 = CARTESIAN_POINT ( 'NONE',  ( -4.164238869374099039, 61.80374883491397497, 8.674139862899312516E-16 ) ) ;
#68732 = LINE ( 'NONE', #77201, #62803 ) ;
#68733 = CARTESIAN_POINT ( 'NONE',  ( 2.917880565312948704, 22.63708216824730002, 12.26659068614894643 ) ) ;
#68734 = CARTESIAN_POINT ( 'NONE',  ( 24.16423886937409904, 54.09541550158063217, 3.795296366450317205 ) ) ;
#68735 = CARTESIAN_POINT ( 'NONE',  ( 19.84674366389459621, 13.50893115100078568, 7.409399052514197653E-17 ) ) ;
#68736 = CARTESIAN_POINT ( 'NONE',  ( -0.8801773607111008646, 3.272018677488171434, 2.915334737309923430 ) ) ;
#68737 = EDGE_LOOP ( 'NONE', ( #30125, #77645, #55148, #6085 ) ) ;
#68738 = CARTESIAN_POINT ( 'NONE',  ( 1.472469842513823179, 20.59226448433411960, -4.923371831947296329 ) ) ;
#68739 = CARTESIAN_POINT ( 'NONE',  ( 4.559911319644449179, 33.89701867748817676, 9.422509992056141925 ) ) ;
#68740 = CARTESIAN_POINT ( 'NONE',  ( 17.20831665107776587, 47.88393115100078745, 7.208316651077764980 ) ) ;
#68742 = CYLINDRICAL_SURFACE ( 'NONE', #79058, 1.249999999999987121 ) ;
#68741 = CARTESIAN_POINT ( 'NONE',  ( -2.266590686148945544, 12.22041550158063394, 7.082119434687048631 ) ) ;
#68743 = CARTESIAN_POINT ( 'NONE',  ( -1.499999999999998890, 21.83999999999999986, 0.000000000000000000 ) ) ;
#68744 = CARTESIAN_POINT ( 'NONE',  ( 0.1532563361054083140, 6.008931151000784787, 1.131784320476157264E-15 ) ) ;
#68745 = CARTESIAN_POINT ( 'NONE',  ( 6.565887622018943937, 40.16530133659708923, 12.81628187352647430 ) ) ;
#68746 = CARTESIAN_POINT ( 'NONE',  ( 19.84674366389459266, 38.30059781766745175, 2.638427012816836559 ) ) ;
#68747 = ORIENTED_EDGE ( 'NONE', *, *, #97379, .F. ) ;
#68748 = CARTESIAN_POINT ( 'NONE',  ( 19.84674366389459266, 28.30059781766745886, 2.638427012816836559 ) ) ;
#68749 = CARTESIAN_POINT ( 'NONE',  ( 11.13643110663977431, -94.02619357115823107, -4.000000000000000000 ) ) ;
#68750 = DIRECTION ( 'NONE',  ( 8.673617379884027583E-16, 1.000000000000000000, 0.000000000000000000 ) ) ;
#68751 = CARTESIAN_POINT ( 'NONE',  ( -0.3689425029237881626, 57.42874883491397497, 10.36894250292379027 ) ) ;
#68752 = CARTESIAN_POINT ( 'NONE',  ( 12.91533473730993009, 56.60535201082151247, -10.88017736071109987 ) ) ;
#68753 = FILL_AREA_STYLE_COLOUR ( '', #72911 ) ;
#68754 = AXIS2_PLACEMENT_3D ( 'NONE', #85583, #61583, #25097 ) ;
#68755 = CARTESIAN_POINT ( 'NONE',  ( 21.92686044187657046, 52.39664270246083788, -3.195792623639524432 ) ) ;
#68756 = CARTESIAN_POINT ( 'NONE',  ( 12.63842701281683922, 34.55059781766745886, -9.846743663894590881 ) ) ;
#68757 = CARTESIAN_POINT ( 'NONE',  ( 10.00000000000000000, 1.813685344154837731, -10.88017736071110342 ) ) ;
#68758 = CARTESIAN_POINT ( 'NONE',  ( 0.1532563361054083140, 46.00893115100079456, 1.131784320476157264E-15 ) ) ;
#68759 = LINE ( 'NONE', #30736, #9607 ) ;
#68760 = CARTESIAN_POINT ( 'NONE',  ( 14.92337183194729988, 54.34226448433412315, -8.527530157486177487 ) ) ;
#68761 = CARTESIAN_POINT ( 'NONE',  ( 19.42250999205614548, 50.98035201082151247, -5.440088680355545492 ) ) ;
#68762 = EDGE_CURVE ( 'NONE', #39241, #92547, #14259, .T. ) ;
#68763 = ORIENTED_EDGE ( 'NONE', *, *, #46851, .F. ) ;
#68764 = EDGE_LOOP ( 'NONE', ( #1687, #6818, #87427, #38054, #83330, #15304 ) ) ;
#68765 = COLOUR_RGB ( '', 0.66274510, 0.83137255, 0.94901961) ;
#68766 = CARTESIAN_POINT ( 'NONE',  ( -14.61046065509106029, -3.236089374985053262E-15, 0.6655452423541795559 ) ) ;
#68767 = CARTESIAN_POINT ( 'NONE',  ( -3.750000000000000000, 10.25000000000000000, 2.500000000000000000 ) ) ;
#68768 = CARTESIAN_POINT ( 'NONE',  ( 0.1532563361054100626, 5.800597817667452638, -2.638427012816831230 ) ) ;
#68769 = CARTESIAN_POINT ( 'NONE',  ( 6.565887622018943937, 55.16530133659709634, 12.81628187352647430 ) ) ;
#68771 = CARTESIAN_POINT ( 'NONE',  ( 14.92337183194729988, 44.34226448433412315, -8.527530157486177487 ) ) ;
#68770 = CARTESIAN_POINT ( 'NONE',  ( -2.266590686148945544, 66.38708216824730357, -7.082119434687050408 ) ) ;
#68773 = EDGE_CURVE ( 'NONE', #3379, #31285, #94112, .T. ) ;
#68772 = CARTESIAN_POINT ( 'NONE',  ( 20.00000000000000355, 88.21129152568919096, 4.994901225422943902 ) ) ;
#68774 = ADVANCED_FACE ( 'NONE', ( #60763 ), #68290, .T. ) ;
#68775 = CARTESIAN_POINT ( 'NONE',  ( 24.16423886937410614, 29.30374883491396787, 8.672049930838204340E-16 ) ) ;
#68776 = CARTESIAN_POINT ( 'NONE',  ( 10.00000000000000178, 58.05374883491397497, 14.16423886937410082 ) ) ;
#68777 = CARTESIAN_POINT ( 'NONE',  ( 10.00000000000000178, 62.25893115100078745, 9.846743663894594434 ) ) ;
#68778 = CARTESIAN_POINT ( 'NONE',  ( 17.59846011966563850, 33.99402920976537246, 9.945641156544798633 ) ) ;
#68779 = CARTESIAN_POINT ( 'NONE',  ( -0.8801773607111008646, 48.27201867748816966, 2.915334737309923430 ) ) ;
#68780 = CARTESIAN_POINT ( 'NONE',  ( 5.076628168052704559, 0.1755978176674514724, -8.527530157486179263 ) ) ;
#68781 = EDGE_LOOP ( 'NONE', ( #48729, #93919, #80927, #74145 ) ) ;
#68782 = CARTESIAN_POINT ( 'NONE',  ( 19.38216949554541557, 62.24863466993041072, -9.382169495545420901 ) ) ;
#68783 = VERTEX_POINT ( 'NONE', #44282 ) ;
#68784 = EDGE_CURVE ( 'NONE', #11334, #35983, #30890, .T. ) ;
#68785 = CARTESIAN_POINT ( 'NONE',  ( 7.361572987183169658, 4.967264484334119601, -9.846743663894592657 ) ) ;
#68786 = ORIENTED_EDGE ( 'NONE', *, *, #27348, .F. ) ;
#68787 = CARTESIAN_POINT ( 'NONE',  ( 20.36894250292379738, 19.92874883491396787, -10.36894250292379027 ) ) ;
#68788 = CARTESIAN_POINT ( 'NONE',  ( 2.791683348922240793, 21.63393115100078745, 7.208316651077764092 ) ) ;
#68789 = CARTESIAN_POINT ( 'NONE',  ( 20.88017736071110164, 35.35535201082150536, 2.915334737309930979 ) ) ;
#68790 = PRESENTATION_STYLE_ASSIGNMENT (( #37805 ) ) ;
#68791 = EDGE_LOOP ( 'NONE', ( #54554, #62626, #19192, #21588 ) ) ;
#68792 = PRESENTATION_LAYER_ASSIGNMENT (  '', '', ( #1786 ) ) ;
#68793 = CARTESIAN_POINT ( 'NONE',  ( 12.91533473730993009, 26.60535201082150536, -10.88017736071109987 ) ) ;
#68794 = EDGE_LOOP ( 'NONE', ( #85239, #57322, #97874, #43895 ) ) ;
#68795 = AXIS2_PLACEMENT_3D ( 'NONE', #45878, #40346, #31343 ) ;
#68796 = FACE_OUTER_BOUND ( 'NONE', #64554, .T. ) ;
#68797 = VERTEX_POINT ( 'NONE', #52771 ) ;
#68798 = EDGE_CURVE ( 'NONE', #65197, #72511, #44773, .T. ) ;
#68799 = CIRCLE ( 'NONE', #87899, 14.49999999999999822 ) ;
#68800 = ORIENTED_EDGE ( 'NONE', *, *, #72416, .T. ) ;
#68801 = CARTESIAN_POINT ( 'NONE',  ( 6.565887622018943937, 18.08196800326375708, -12.81628187352647608 ) ) ;
#68802 = CARTESIAN_POINT ( 'NONE',  ( 1.472469842513823179, 5.592264484334118713, -4.923371831947296329 ) ) ;
#68803 =( NAMED_UNIT ( * ) SI_UNIT ( $, .STERADIAN. ) SOLID_ANGLE_UNIT ( ) );
#68804 = SURFACE_STYLE_USAGE ( .BOTH. , #37819 ) ;
#68805 = CARTESIAN_POINT ( 'NONE',  ( 1.472469842513823179, 16.42559781766745175, 4.923371831947296329 ) ) ;
#68806 = AXIS2_PLACEMENT_3D ( 'NONE', #74169, #89189, #28192 ) ;
#68807 = CARTESIAN_POINT ( 'NONE',  ( 20.88017736071110519, 25.56368534415483751, 2.639326808657452039E-16 ) ) ;
#68808 = ORIENTED_EDGE ( 'NONE', *, *, #57584, .F. ) ;
#68809 = CARTESIAN_POINT ( 'NONE',  ( -1.099225684535947600, 63.70696800326376774, -6.408140936763238038 ) ) ;
#68810 = CARTESIAN_POINT ( 'NONE',  ( 15.44008868035555260, 59.73035201082151247, 9.422509992056143702 ) ) ;
#68811 = CARTESIAN_POINT ( 'NONE',  ( -8.924603092375777535, 75.06466731010172566, -2.900000000000000799 ) ) ;
#68812 = CARTESIAN_POINT ( 'NONE',  ( 13.43411237798105340, 60.58196800326376064, 12.81628187352647963 ) ) ;
#68813 = CARTESIAN_POINT ( 'NONE',  ( 2.035157376598822676, 57.43868534415484106, -7.964842623401177768 ) ) ;
#68814 = CARTESIAN_POINT ( 'NONE',  ( 19.84674366389459266, 63.71726448433412315, -2.638427012816827677 ) ) ;
#68815 = LINE ( 'NONE', #60316, #30721 ) ;
#68816 = CARTESIAN_POINT ( 'NONE',  ( 2.791683348922240793, 26.63393115100078745, 7.208316651077764092 ) ) ;
#68817 = CARTESIAN_POINT ( 'NONE',  ( 10.00000000000000178, 50.37363466993042493, 12.81628187352647608 ) ) ;
#68818 = CARTESIAN_POINT ( 'NONE',  ( -0.1688089201193209155, 79.91181047996344944, 9.500000000000000000 ) ) ;
#68819 = CARTESIAN_POINT ( 'NONE',  ( 19.84674366389459266, 23.30059781766745530, 2.638427012816836559 ) ) ;
#68820 = CARTESIAN_POINT ( 'NONE',  ( 10.00000000000000178, 15.37363466993042138, 12.81628187352647608 ) ) ;
#68822 = FACE_OUTER_BOUND ( 'NONE', #92535, .T. ) ;
#68821 = SURFACE_STYLE_USAGE ( .BOTH. , #29318 ) ;
#68823 = CARTESIAN_POINT ( 'NONE',  ( 15.44008868035555260, 34.73035201082151247, 9.422509992056143702 ) ) ;
#68824 = CARTESIAN_POINT ( 'NONE',  ( 7.361572987183170547, 62.05059781766745886, 9.846743663894590881 ) ) ;
#68825 = AXIS2_PLACEMENT_3D ( 'NONE', #81864, #79547, #32556 ) ;
#68826 = DIRECTION ( 'NONE',  ( -0.000000000000000000, -1.000000000000000000, -0.000000000000000000 ) ) ;
#68827 = CARTESIAN_POINT ( 'NONE',  ( 14.92337183194729988, 19.34226448433411960, -8.527530157486177487 ) ) ;
#68828 = CARTESIAN_POINT ( 'NONE',  ( 7.361572987183169658, 9.967264484334119601, -9.846743663894592657 ) ) ;
#68830 = ADVANCED_FACE ( 'NONE', ( #22789 ), #37303, .T. ) ;
#68829 = CARTESIAN_POINT ( 'NONE',  ( 10.00000000000000178, 19.31368534415484106, 10.88017736071110342 ) ) ;
#68831 = CARTESIAN_POINT ( 'NONE',  ( -1.099225684535947600, 13.70696800326375353, -6.408140936763238038 ) ) ;
#68832 = CARTESIAN_POINT ( 'NONE',  ( -0.7375392941516148992, 0.3640475087720989045, -14.98185688723471998 ) ) ;
#68833 = AXIS2_PLACEMENT_3D ( 'NONE', #90969, #76473, #7000 ) ;
#68834 = CARTESIAN_POINT ( 'NONE',  ( 4.441081520790487680, -2.684960557614425092, -2.750000000000000444 ) ) ;
#68835 = CARTESIAN_POINT ( 'NONE',  ( 7.084665262690076126, 4.105352010821503583, 10.88017736071109987 ) ) ;
#68836 = CARTESIAN_POINT ( 'NONE',  ( 19.84674366389459621, 48.50893115100078745, 7.409399052514197653E-17 ) ) ;
#68837 = ORIENTED_EDGE ( 'NONE', *, *, #1199, .F. ) ;
#68838 = CARTESIAN_POINT ( 'NONE',  ( 4.920090861810839655, -13.81657824362204678, 2.750000000000000444 ) ) ;
#68839 = CARTESIAN_POINT ( 'NONE',  ( 0.5774900079438607392, 23.48035201082150536, 5.440088680355550821 ) ) ;
#68840 = CARTESIAN_POINT ( 'NONE',  ( 0.5774900079438590739, 12.64701867748817321, -5.440088680355550821 ) ) ;
#68841 = CARTESIAN_POINT ( 'NONE',  ( -0.8801773607110991993, 27.85535201082150181, -2.915334737309923874 ) ) ;
#68843 = DIRECTION ( 'NONE',  ( -0.000000000000000000, -0.000000000000000000, -1.000000000000000000 ) ) ;
#68842 = CARTESIAN_POINT ( 'NONE',  ( 2.035157376598822676, 2.438685344154838397, -7.964842623401177768 ) ) ;
#68844 = CARTESIAN_POINT ( 'NONE',  ( 19.84674366389459266, 3.300597817667451750, 2.638427012816836559 ) ) ;
#68845 = CARTESIAN_POINT ( 'NONE',  ( 18.52753015748618282, 18.92559781766745175, -4.923371831947291888 ) ) ;
#68846 = CARTESIAN_POINT ( 'NONE',  ( 3.591859063236763294, 8.290301336597087456, -11.09922568453595026 ) ) ;
#68847 = DIRECTION ( 'NONE',  ( 6.938893903907221278E-15, -1.000000000000000000, 0.000000000000000000 ) ) ;
#68848 = CARTESIAN_POINT ( 'NONE',  ( 3.591859063236763294, -1.709698663402913210, -11.09922568453595026 ) ) ;
#68849 = DIRECTION ( 'NONE',  ( 1.000000000000000000, -5.818595309480553908E-17, 0.000000000000000000 ) ) ;
#68850 =( BOUNDED_CURVE ( )  B_SPLINE_CURVE ( 2, ( #97758, #30205, #61206, #60708, #7232, #90715, #92203, #37739, #38230 ),
 .UNSPECIFIED., .F., .F. ) 
 B_SPLINE_CURVE_WITH_KNOTS ( ( 3, 2, 2, 2, 3 ),
 ( 0.2972837940830885262, 0.2976190476190476719, 0.3035714285714286031, 0.3095238095238095344, 0.3098590630597686801 ),
 .UNSPECIFIED. ) 
 CURVE ( )  GEOMETRIC_REPRESENTATION_ITEM ( )  RATIONAL_B_SPLINE_CURVE ( ( 0.9963778908391760503, 0.9980808541467920403, 1.000000000000000000, 0.9659258262890682012, 1.000000000000000000, 0.9659258262890682012, 1.000000000000000000, 0.9980808541467920403, 0.9963778908391759392 ) ) 
 REPRESENTATION_ITEM ( '' )  );
#68851 = CARTESIAN_POINT ( 'NONE',  ( -8.000000000000000000, -0.01655697267263257777, -3.750000000000000000 ) ) ;
#68852 = CARTESIAN_POINT ( 'NONE',  ( 6.204703633549690345, 15.76208216824730179, -14.16423886937410259 ) ) ;
#68853 = TOROIDAL_SURFACE ( 'NONE', #22607, 14.49999999999999822, 0.5000000000000000000 ) ;
#68854 = CARTESIAN_POINT ( 'NONE',  ( 19.84674366389459621, 28.50893115100078745, 7.409399052514197653E-17 ) ) ;
#68855 = LINE ( 'NONE', #74355, #11357 ) ;
#68856 = ORIENTED_EDGE ( 'NONE', *, *, #42681, .T. ) ;
#68857 = CARTESIAN_POINT ( 'NONE',  ( 20.36894250292379382, 58.67874883491396076, 10.36894250292379205 ) ) ;
#68858 = CARTESIAN_POINT ( 'NONE',  ( 12.63842701281683034, 12.46726448433411782, 9.846743663894596210 ) ) ;
#68860 = CARTESIAN_POINT ( 'NONE',  ( -7.750000000000000000, 40.99999999999999289, 6.250000000000000000 ) ) ;
#68859 = CARTESIAN_POINT ( 'NONE',  ( 0.2751277870542978565, 12.28217586085238011, -6.500000000000002665 ) ) ;
#68861 = CARTESIAN_POINT ( 'NONE',  ( 2.035157376598824452, 43.68868534415484106, 7.964842623401179544 ) ) ;
#68862 = CARTESIAN_POINT ( 'NONE',  ( 6.565887622018943937, 55.16530133659709634, 12.81628187352647430 ) ) ;
#68863 = CARTESIAN_POINT ( 'NONE',  ( 19.42250999205614193, 15.14701867748817143, 5.440088680355555262 ) ) ;
#68864 = TOROIDAL_SURFACE ( 'NONE', #30581, 9.538348415311009632, 7.000000000000000000 ) ;
#68865 = CARTESIAN_POINT ( 'NONE',  ( 21.09922568453594849, 51.20696800326375353, 6.408140936763242479 ) ) ;
#68866 = CARTESIAN_POINT ( 'NONE',  ( 3.591859063236761518, -0.04303199673624671928, 11.09922568453594849 ) ) ;
#68867 = FILL_AREA_STYLE ('',( #30848 ) ) ;
#68868 = VERTEX_POINT ( 'NONE', #98312 ) ;
#68869 = DIRECTION ( 'NONE',  ( -1.257568779154408793E-17, -1.000000000000000000, 0.000000000000000000 ) ) ;
#68870 = CARTESIAN_POINT ( 'NONE',  ( 1.485411327523655789, 2.210147928482776969, -6.499999999999963585 ) ) ;
#68871 = CARTESIAN_POINT ( 'NONE',  ( 6.204703633549690345, 45.76208216824729647, -14.16423886937410259 ) ) ;
#68872 = CARTESIAN_POINT ( 'NONE',  ( 13.79529636645031943, 10.34541550158063394, -14.16423886937409904 ) ) ;
#68873 = CARTESIAN_POINT ( 'NONE',  ( 7.084665262690076126, 4.105352010821503583, 10.88017736071109987 ) ) ;
#68874 = CARTESIAN_POINT ( 'NONE',  ( -0.8801773607110991993, 32.85535201082151247, -2.915334737309923874 ) ) ;
#68875 = CARTESIAN_POINT ( 'NONE',  ( -9.024359497401759356, 75.07164295747612925, 2.900000000000000355 ) ) ;
#68876 = CARTESIAN_POINT ( 'NONE',  ( 14.97687855664611689, 0.3639309658595352159, -0.8325315005900656429 ) ) ;
#68877 = CARTESIAN_POINT ( 'NONE',  ( 2.035157376598822676, 67.43868534415484817, -7.964842623401177768 ) ) ;
#68878 = CARTESIAN_POINT ( 'NONE',  ( -0.8801773607111009756, 63.06368534415484106, 1.068504757029289695E-15 ) ) ;
#68879 = CARTESIAN_POINT ( 'NONE',  ( 22.81628187352647785, 31.62363466993042138, 6.195893100308588602E-16 ) ) ;
#68880 = DIRECTION ( 'NONE',  ( 0.000000000000000000, 0.000000000000000000, 1.000000000000000000 ) ) ;
#68881 = PLANE ( 'NONE',  #91465 ) ;
#68882 = CARTESIAN_POINT ( 'NONE',  ( 1.472469842513823179, 31.42559781766745530, 4.923371831947296329 ) ) ;
#68883 = CARTESIAN_POINT ( 'NONE',  ( 12.91533473730992121, 19.52201867748816611, 10.88017736071110164 ) ) ;
#68884 = ADVANCED_FACE ( 'NONE', ( #75771 ), #81052, .T. ) ;
#68885 = EDGE_CURVE ( 'NONE', #46257, #39257, #2792, .T. ) ;
#68886 = CARTESIAN_POINT ( 'NONE',  ( 0.6178305044545818747, 23.49863466993041783, -9.382169495545419124 ) ) ;
#68887 = CARTESIAN_POINT ( 'NONE',  ( 2.791683348922237240, 10.38393115100078390, -7.208316651077763204 ) ) ;
#68889 = EDGE_CURVE ( 'NONE', #4994, #89266, #23287, .T. ) ;
#68888 = CARTESIAN_POINT ( 'NONE',  ( -0.8801773607111008646, 13.27201867748817143, 2.915334737309923430 ) ) ;
#68890 = EDGE_CURVE ( 'NONE', #45005, #85730, #31519, .T. ) ;
#68891 = CARTESIAN_POINT ( 'NONE',  ( 14.92337183194729633, 32.67559781766745175, 8.527530157486181039 ) ) ;
#68892 = CARTESIAN_POINT ( 'NONE',  ( 22.81628187352648496, 61.83196800326376774, -3.434112377981050290 ) ) ;
#68894 = CARTESIAN_POINT ( 'NONE',  ( -4.164238869374099927, 2.012082168247300906, 3.795296366450308767 ) ) ;
#68893 = CARTESIAN_POINT ( 'NONE',  ( 17.20831665107776587, 34.13393115100078745, -7.208316651077762316 ) ) ;
#68895 = CARTESIAN_POINT ( 'NONE',  ( 17.08211943468705130, 18.47041550158063572, 12.26659068614894998 ) ) ;
#68896 = CARTESIAN_POINT ( 'NONE',  ( -0.8801773607110991993, 32.85535201082151247, -2.915334737309923874 ) ) ;
#68898 = CARTESIAN_POINT ( 'NONE',  ( 6.204703633549690345, 42.84541550158063217, 14.16423886937410082 ) ) ;
#68897 = CARTESIAN_POINT ( 'NONE',  ( 20.88017736071110519, 10.56368534415483751, 2.639326808657452039E-16 ) ) ;
#68899 = CARTESIAN_POINT ( 'NONE',  ( 7.084665262690076126, 37.02201867748817676, -10.88017736071110164 ) ) ;
#68900 = CARTESIAN_POINT ( 'NONE',  ( 19.42250999205614548, 15.98035201082150714, -5.440088680355545492 ) ) ;
#68901 = ORIENTED_EDGE ( 'NONE', *, *, #70442, .F. ) ;
#68902 = CARTESIAN_POINT ( 'NONE',  ( 10.00000000000000178, 34.31368534415484106, 10.88017736071110342 ) ) ;
#68903 = AXIS2_PLACEMENT_3D ( 'NONE', #57390, #40935, #10916 ) ;
#68904 = CARTESIAN_POINT ( 'NONE',  ( -2.816281873526473856, 64.12363466993042493, 9.499525473075851096E-16 ) ) ;
#68905 = CARTESIAN_POINT ( 'NONE',  ( -0.8801773607110991993, 42.85535201082150536, -2.915334737309923874 ) ) ;
#68906 = CARTESIAN_POINT ( 'NONE',  ( 4.559911319644449179, 53.89701867748817676, 9.422509992056141925 ) ) ;
#68907 = ORIENTED_EDGE ( 'NONE', *, *, #90582, .T. ) ;
#68908 = CARTESIAN_POINT ( 'NONE',  ( 19.42250999205614193, 45.14701867748817676, 5.440088680355555262 ) ) ;
#68909 = CARTESIAN_POINT ( 'NONE',  ( 0.000000000000000000, 0.5000000000000004441, 0.000000000000000000 ) ) ;
#68910 = AXIS2_PLACEMENT_3D ( 'NONE', #62931, #93433, #24955 ) ;
#68911 = CARTESIAN_POINT ( 'NONE',  ( -4.164238869374099927, 42.01208216824728936, 3.795296366450308767 ) ) ;
#68912 = CARTESIAN_POINT ( 'NONE',  ( 20.88017736071110875, 60.77201867748817676, -2.915334737309920765 ) ) ;
#68913 = DIRECTION ( 'NONE',  ( -1.000000000000000000, 5.818595309480552676E-17, 0.000000000000000000 ) ) ;
#68914 = CARTESIAN_POINT ( 'NONE',  ( 18.52753015748617571, 63.09226448433412315, 4.923371831947298993 ) ) ;
#68915 = CARTESIAN_POINT ( 'NONE',  ( 10.19513985507833276, 0.5000000000000004441, -11.00268709613217055 ) ) ;
#68916 = CARTESIAN_POINT ( 'NONE',  ( 10.00000000000000178, 37.25893115100078745, 9.846743663894594434 ) ) ;
#68917 = ORIENTED_EDGE ( 'NONE', *, *, #51664, .F. ) ;
#68918 = EDGE_CURVE ( 'NONE', #50302, #72594, #45951, .T. ) ;
#68919 = CARTESIAN_POINT ( 'NONE',  ( 7.361572987183169658, 39.96726448433411605, -9.846743663894592657 ) ) ;
#68920 = CARTESIAN_POINT ( 'NONE',  ( 7.084665262690076126, 34.10535201082151247, 10.88017736071109987 ) ) ;
#68921 = CARTESIAN_POINT ( 'NONE',  ( 12.63842701281683034, 32.46726448433412315, 9.846743663894596210 ) ) ;
#68922 = CARTESIAN_POINT ( 'NONE',  ( -1.099225684535947600, 23.70696800326375708, -6.408140936763238038 ) ) ;
#68923 = DIRECTION ( 'NONE',  ( 0.000000000000000000, -0.000000000000000000, 1.000000000000000000 ) ) ;
#68925 = CARTESIAN_POINT ( 'NONE',  ( 15.44008868035555793, 6.397018677488170546, -9.422509992056140149 ) ) ;
#68924 = CARTESIAN_POINT ( 'NONE',  ( 7.084665262690076126, 47.02201867748818387, -10.88017736071110164 ) ) ;
#68926 = CARTESIAN_POINT ( 'NONE',  ( 13.79529636645031943, 55.34541550158062506, -14.16423886937409904 ) ) ;
#68927 = VECTOR ( 'NONE', #59416, 1000.000000000000114 ) ;
#68928 = CARTESIAN_POINT ( 'NONE',  ( 19.38216949554541202, 20.99863466993042138, 9.382169495545424454 ) ) ;
#68929 = CYLINDRICAL_SURFACE ( 'NONE', #5157, 0.5000000000000004441 ) ;
#68930 = ORIENTED_EDGE ( 'NONE', *, *, #59162, .T. ) ;
#68931 = CARTESIAN_POINT ( 'NONE',  ( 6.565887622018943937, 20.16530133659708213, 12.81628187352647430 ) ) ;
#68932 = CARTESIAN_POINT ( 'NONE',  ( 20.88017736071110519, 20.56368534415484106, 2.639326808657452039E-16 ) ) ;
#68933 = CARTESIAN_POINT ( 'NONE',  ( 19.42250999205614193, 55.14701867748817676, 5.440088680355555262 ) ) ;
#68934 = COLOUR_RGB ( '', 0.40784314, 0.44705882, 0.49803922) ;
#68935 = ORIENTED_EDGE ( 'NONE', *, *, #88268, .T. ) ;
#68936 = CARTESIAN_POINT ( 'NONE',  ( 0.1532563361054100626, 0.8005978176674514168, -2.638427012816831230 ) ) ;
#68937 = CARTESIAN_POINT ( 'NONE',  ( 0.1532563361054100626, 55.80059781766745175, -2.638427012816831230 ) ) ;
#68938 = CARTESIAN_POINT ( 'NONE',  ( 14.92337183194729633, 32.67559781766745175, 8.527530157486181039 ) ) ;
#68939 = CARTESIAN_POINT ( 'NONE',  ( 5.076628168052703671, 31.84226448433412315, 8.527530157486179263 ) ) ;
#68940 = DIRECTION ( 'NONE',  ( -1.000000000000000000, 0.000000000000000000, 0.000000000000000000 ) ) ;
#68941 = CARTESIAN_POINT ( 'NONE',  ( 11.24699797944280100, 54.09857164847241506, 0.000000000000000000 ) ) ;
#68943 = CARTESIAN_POINT ( 'NONE',  ( 34.56412365047463453, 13.99999999999999645, 10.00000000000000000 ) ) ;
#68942 = CARTESIAN_POINT ( 'NONE',  ( 17.20831665107776587, 12.88393115100078390, 7.208316651077764980 ) ) ;
#68944 = CARTESIAN_POINT ( 'NONE',  ( 4.630000000000003446, 1.019547802438462547, -4.000000000000000000 ) ) ;
#68946 = ORIENTED_EDGE ( 'NONE', *, *, #43284, .F. ) ;
#68945 = CARTESIAN_POINT ( 'NONE',  ( 17.20831665107776587, 44.13393115100078745, -7.208316651077762316 ) ) ;
#68947 = CARTESIAN_POINT ( 'NONE',  ( 19.72487221294571569, 65.71833443783937412, -6.499999999999983125 ) ) ;
#68948 = CARTESIAN_POINT ( 'NONE',  ( 6.565887622018943937, 18.08196800326375708, -12.81628187352647608 ) ) ;
#68949 = ORIENTED_EDGE ( 'NONE', *, *, #54646, .T. ) ;
#68950 = CARTESIAN_POINT ( 'NONE',  ( -0.8801773607111009756, 53.06368534415484106, 1.068504757029289695E-15 ) ) ;
#68951 = CARTESIAN_POINT ( 'NONE',  ( 6.204703633549690345, 35.76208216824729647, -14.16423886937410259 ) ) ;
#68952 = PLANE ( 'NONE',  #72736 ) ;
#68953 = CARTESIAN_POINT ( 'NONE',  ( -4.164238869374099927, 32.01208216824730357, 3.795296366450308767 ) ) ;
#68954 = CARTESIAN_POINT ( 'NONE',  ( 20.36894250292379382, 63.67874883491396787, 10.36894250292379205 ) ) ;
#68955 = CARTESIAN_POINT ( 'NONE',  ( 13.79529636645030344, 13.26208216824729824, 14.16423886937410614 ) ) ;
#68957 = LINE ( 'NONE', #69445, #38211 ) ;
#68956 = CARTESIAN_POINT ( 'NONE',  ( -2.266590686148945544, 31.38708216824730002, -7.082119434687050408 ) ) ;
#68958 = CARTESIAN_POINT ( 'NONE',  ( 15.44008868035555260, 54.73035201082150536, 9.422509992056143702 ) ) ;
#68959 = CARTESIAN_POINT ( 'NONE',  ( 4.380000000000000782, -0.01592157648205478476, -3.750000000000000888 ) ) ;
#68960 = B_SPLINE_CURVE_WITH_KNOTS ( 'NONE', 3,
 ( #22447, #37452, #1431, #52920, #14953, #933 ),
 .UNSPECIFIED., .F., .F.,
 ( 4, 2, 4 ),
 ( 0.0002800289709865070556, 0.0006862344838253337225, 0.001092439996664160444 ),
 .UNSPECIFIED. ) ;
#68962 = CARTESIAN_POINT ( 'NONE',  ( 18.52753015748617571, 38.09226448433412315, 4.923371831947298993 ) ) ;
#68961 = FACE_OUTER_BOUND ( 'NONE', #85270, .T. ) ;
#68963 = CARTESIAN_POINT ( 'NONE',  ( 10.00000000000000000, 21.81368534415484106, -10.88017736071110342 ) ) ;
#68964 = CARTESIAN_POINT ( 'NONE',  ( 21.92686044187656691, 54.95379003517447813, 3.195792623639537755 ) ) ;
#68965 = CARTESIAN_POINT ( 'NONE',  ( 10.00000000000000178, 62.25893115100078745, 9.846743663894594434 ) ) ;
#68966 = EDGE_CURVE ( 'NONE', #71703, #74605, #93900, .T. ) ;
#68967 = CARTESIAN_POINT ( 'NONE',  ( -9.820682251645022731, 14.76930270348881002, -11.26020669458372758 ) ) ;
#68968 = CARTESIAN_POINT ( 'NONE',  ( 2.791683348922237240, 40.38393115100078035, -7.208316651077763204 ) ) ;
#68969 = CARTESIAN_POINT ( 'NONE',  ( 16.40814093676323893, 50.79030133659708923, 11.09922568453595026 ) ) ;
#68970 = CARTESIAN_POINT ( 'NONE',  ( -7.082119434687044190, -7.362917831752691100, 12.26659068614894998 ) ) ;
#68971 = CARTESIAN_POINT ( 'NONE',  ( 19.84674366389459266, 38.30059781766745175, 2.638427012816836559 ) ) ;
#68972 = CARTESIAN_POINT ( 'NONE',  ( 0.1532563361054100626, 50.80059781766745175, -2.638427012816831230 ) ) ;
#68973 = AXIS2_PLACEMENT_3D ( 'NONE', #51776, #26800, #58266 ) ;
#68974 = CARTESIAN_POINT ( 'NONE',  ( 17.08211943468705130, 38.47041550158063217, 12.26659068614894998 ) ) ;
#68975 = ORIENTED_EDGE ( 'NONE', *, *, #5973, .T. ) ;
#68976 = CARTESIAN_POINT ( 'NONE',  ( 2.917880565312948704, 12.63708216824730179, 12.26659068614894643 ) ) ;
#68977 = CARTESIAN_POINT ( 'NONE',  ( 2.035157376598824452, 58.68868534415482685, 7.964842623401179544 ) ) ;
#68978 = CARTESIAN_POINT ( 'NONE',  ( -3.750000000000000000, 37.25000000000000000, -3.750000000000000000 ) ) ;
#68979 = CARTESIAN_POINT ( 'NONE',  ( 6.204703633549690345, 52.84541550158062506, 14.16423886937410082 ) ) ;
#68980 = CARTESIAN_POINT ( 'NONE',  ( -1.099225684535947600, 9.540301336597087456, 6.408140936763237150 ) ) ;
#68981 = CARTESIAN_POINT ( 'NONE',  ( -0.1023957841222405962, 55.13377557478295898, 6.340343622311920058 ) ) ;
#68982 = CARTESIAN_POINT ( 'NONE',  ( 18.52753015748617571, 3.092264484334118269, 4.923371831947298993 ) ) ;
#68983 = CARTESIAN_POINT ( 'NONE',  ( -0.7575892234032817196, 14.76930270348881002, 14.92193396517713033 ) ) ;
#68984 = CARTESIAN_POINT ( 'NONE',  ( -46.94000000000001194, 101.9444105523804893, -6.894162316358291243 ) ) ;
#68985 = CARTESIAN_POINT ( 'NONE',  ( -4.164238869374099927, 57.01208216824731068, 3.795296366450308767 ) ) ;
#68986 = DIRECTION ( 'NONE',  ( 0.000000000000000000, -1.000000000000000000, 0.000000000000000000 ) ) ;
#68987 = CARTESIAN_POINT ( 'NONE',  ( -0.8801773607110991993, 32.85535201082151247, -2.915334737309923874 ) ) ;
#68988 = CARTESIAN_POINT ( 'NONE',  ( 7.084665262690076126, 29.10535201082150181, 10.88017736071109987 ) ) ;
#68989 = CARTESIAN_POINT ( 'NONE',  ( 5.076628168052704559, 50.17559781766745886, -8.527530157486179263 ) ) ;
#68990 = CARTESIAN_POINT ( 'NONE',  ( 5.076628168052704559, 50.17559781766745886, -8.527530157486179263 ) ) ;
#68991 = CARTESIAN_POINT ( 'NONE',  ( 10.00000000000000178, 55.37363466993042493, 12.81628187352647608 ) ) ;
#68992 =( NAMED_UNIT ( * ) PLANE_ANGLE_UNIT ( ) SI_UNIT ( $, .RADIAN. ) );
#68993 = EDGE_LOOP ( 'NONE', ( #5343, #75973, #51370, #62713 ) ) ;
#68994 = CARTESIAN_POINT ( 'NONE',  ( 15.44008868035555260, 14.73035201082150536, 9.422509992056143702 ) ) ;
#68995 = CARTESIAN_POINT ( 'NONE',  ( 0.6178305044545838731, 14.74863466993041783, 9.382169495545420901 ) ) ;
#68996 = CARTESIAN_POINT ( 'NONE',  ( 64.56412365047461321, 11.99999999999999467, 10.00000000000000000 ) ) ;
#68997 = AXIS2_PLACEMENT_3D ( 'NONE', #14215, #67206, #13710 ) ;
#68998 = ADVANCED_FACE ( 'NONE', ( #62236 ), #76286, .T. ) ;
#68999 = CARTESIAN_POINT ( 'NONE',  ( 7.361572987183170547, 47.05059781766745175, 9.846743663894590881 ) ) ;
#69000 = CARTESIAN_POINT ( 'NONE',  ( 19.42250999205614548, 55.98035201082150536, -5.440088680355545492 ) ) ;
#69001 = EDGE_CURVE ( 'NONE', #15586, #73495, #52315, .T. ) ;
#69002 = CARTESIAN_POINT ( 'NONE',  ( 19.38216949554541557, 27.24863466993041783, -9.382169495545420901 ) ) ;
#69004 = CARTESIAN_POINT ( 'NONE',  ( -8.024359497401761132, 75.03672218798435267, 3.000000000000000000 ) ) ;
#69003 = CARTESIAN_POINT ( 'NONE',  ( 4.559911319644449179, 47.23035201082150536, -9.422509992056141925 ) ) ;
#69005 = CARTESIAN_POINT ( 'NONE',  ( 0.5600000000000083800, 105.0000000000000000, -5.000000000000000000 ) ) ;
#69006 =( GEOMETRIC_REPRESENTATION_CONTEXT ( 3 ) GLOBAL_UNCERTAINTY_ASSIGNED_CONTEXT ( ( #83385 ) ) GLOBAL_UNIT_ASSIGNED_CONTEXT ( ( #5455, #21934, #81428 ) ) REPRESENTATION_CONTEXT ( 'NONE', 'WORKASPACE' ) );
#69007 = CARTESIAN_POINT ( 'NONE',  ( -2.816281873526473856, 54.33196800326376064, 3.434112377981055619 ) ) ;
#69008 = ORIENTED_EDGE ( 'NONE', *, *, #83306, .T. ) ;
#69009 = CYLINDRICAL_SURFACE ( 'NONE', #54850, 0.2500000000000002220 ) ;
#69010 = CARTESIAN_POINT ( 'NONE',  ( 20.88017736071110875, 45.77201867748816966, -2.915334737309920765 ) ) ;
#69011 = CARTESIAN_POINT ( 'NONE',  ( 13.43411237798105340, 50.58196800326375353, 12.81628187352647963 ) ) ;
#69012 = CARTESIAN_POINT ( 'NONE',  ( 12.63842701281683922, 4.550597817667451750, -9.846743663894590881 ) ) ;
#69013 = TOROIDAL_SURFACE ( 'NONE', #25891, 14.49999999999999822, 0.5000000000000000000 ) ;
#69014 = CARTESIAN_POINT ( 'NONE',  ( 0.1532563361054100626, 60.80059781766744464, -2.638427012816831230 ) ) ;
#69015 = CARTESIAN_POINT ( 'NONE',  ( 12.63842701281683922, 34.55059781766745886, -9.846743663894590881 ) ) ;
#69016 = CARTESIAN_POINT ( 'NONE',  ( 7.361572987183170547, 2.050597817667451750, 9.846743663894590881 ) ) ;
#69017 = LINE ( 'NONE', #62471, #79422 ) ;
#69018 = CARTESIAN_POINT ( 'NONE',  ( -0.3689425029237881626, 47.42874883491396787, 10.36894250292379027 ) ) ;
#69019 = VECTOR ( 'NONE', #52854, 1000.000000000000000 ) ;
#69020 = CARTESIAN_POINT ( 'NONE',  ( 2.035157376598822676, 2.438685344154837953, -7.964842623401177768 ) ) ;
#69021 = CARTESIAN_POINT ( 'NONE',  ( 2.035157376598824452, 3.688685344154837953, 7.964842623401179544 ) ) ;
#69022 = CARTESIAN_POINT ( 'NONE',  ( -7.080143328636912869, -69.54337233422656084, -3.999999999999999556 ) ) ;
#69023 = ORIENTED_EDGE ( 'NONE', *, *, #75348, .F. ) ;
#69024 = CARTESIAN_POINT ( 'NONE',  ( 20.88017736071110164, 15.35535201082150358, 2.915334737309930979 ) ) ;
#69025 = CARTESIAN_POINT ( 'NONE',  ( 10.00000000000000178, 4.313685344154837509, 10.88017736071110342 ) ) ;
#69026 = CARTESIAN_POINT ( 'NONE',  ( 18.52753015748617571, 43.09226448433412315, 4.923371831947298993 ) ) ;
#69027 = CARTESIAN_POINT ( 'NONE',  ( 16.40814093676323893, 35.79030133659708923, 11.09922568453595026 ) ) ;
#69029 = CARTESIAN_POINT ( 'NONE',  ( -0.3689425029237881626, 12.42874883491396609, 10.36894250292379027 ) ) ;
#69028 = CARTESIAN_POINT ( 'NONE',  ( -14.03351048042399007, 15.00000000000000000, 2.474486531753619989 ) ) ;
#69030 = CARTESIAN_POINT ( 'NONE',  ( 19.42250999205614193, 25.14701867748817321, 5.440088680355555262 ) ) ;
#69031 = CARTESIAN_POINT ( 'NONE',  ( 12.91533473730993009, 6.605352010821504471, -10.88017736071109987 ) ) ;
#69032 = CARTESIAN_POINT ( 'NONE',  ( 17.20831665107776587, 44.13393115100078745, -7.208316651077762316 ) ) ;
#69033 = CARTESIAN_POINT ( 'NONE',  ( 0.4400000000000020006, 1.019547802438468986, -4.000000000000000000 ) ) ;
#69034 = CARTESIAN_POINT ( 'NONE',  ( 19.84674366389459621, 18.50893115100078745, 7.409399052514197653E-17 ) ) ;
#69035 = EDGE_CURVE ( 'NONE', #85150, #17634, #78525, .T. ) ;
#69036 = CARTESIAN_POINT ( 'NONE',  ( 0.8952175423694934686, 32.60160829253884884, -5.990408912944337416 ) ) ;
#69037 = CARTESIAN_POINT ( 'NONE',  ( 3.469446951953614189E-15, -39.62636533006958217, 12.81628187352647608 ) ) ;
#69038 = ORIENTED_EDGE ( 'NONE', *, *, #54183, .F. ) ;
#69039 =( NAMED_UNIT ( * ) PLANE_ANGLE_UNIT ( ) SI_UNIT ( $, .RADIAN. ) );
#69040 = ORIENTED_EDGE ( 'NONE', *, *, #35822, .F. ) ;
#69041 = CARTESIAN_POINT ( 'NONE',  ( 1.472469842513823179, 55.59226448433412315, -4.923371831947296329 ) ) ;
#69043 = CARTESIAN_POINT ( 'NONE',  ( 0.5774900079438607392, 33.48035201082150536, 5.440088680355550821 ) ) ;
#69042 = CARTESIAN_POINT ( 'NONE',  ( 20.88017736071110519, 35.56368534415484106, 2.639326808657452039E-16 ) ) ;
#69045 = CARTESIAN_POINT ( 'NONE',  ( 13.43411237798105340, 30.58196800326374998, 12.81628187352647963 ) ) ;
#69044 = CARTESIAN_POINT ( 'NONE',  ( -0.8801773607111008646, 3.272018677488171434, 2.915334737309923430 ) ) ;
#69046 = CARTESIAN_POINT ( 'NONE',  ( 24.16423886937410614, 14.51208216824730179, -3.795296366450302550 ) ) ;
#69047 = VECTOR ( 'NONE', #6946, 1000.000000000000000 ) ;
#69048 = CARTESIAN_POINT ( 'NONE',  ( 0.6178305044545818747, 48.49863466993042493, -9.382169495545419124 ) ) ;
#69049 = VERTEX_POINT ( 'NONE', #69759 ) ;
#69050 = CARTESIAN_POINT ( 'NONE',  ( 0.1532563361054082862, 51.21726448433412315, 2.638427012816831674 ) ) ;
#69051 = CARTESIAN_POINT ( 'NONE',  ( 19.42250999205614548, 25.98035201082150891, -5.440088680355545492 ) ) ;
#69052 = ORIENTED_EDGE ( 'NONE', *, *, #37290, .F. ) ;
#69053 = CARTESIAN_POINT ( 'NONE',  ( -0.8801773607110991993, 12.85535201082150358, -2.915334737309923874 ) ) ;
#69054 = ORIENTED_EDGE ( 'NONE', *, *, #18993, .T. ) ;
#69055 = CARTESIAN_POINT ( 'NONE',  ( 12.91533473730992121, 54.52201867748816255, 10.88017736071110164 ) ) ;
#69056 = CARTESIAN_POINT ( 'NONE',  ( 7.084665262690076126, 69.10535201082151957, 10.88017736071109987 ) ) ;
#69057 = CARTESIAN_POINT ( 'NONE',  ( 17.96484262340118221, 59.93868534415484106, 7.964842623401181321 ) ) ;
#69058 = CARTESIAN_POINT ( 'NONE',  ( 5.076628168052704559, 15.17559781766745175, -8.527530157486179263 ) ) ;
#69059 = CARTESIAN_POINT ( 'NONE',  ( -0.8801773607111009756, 53.06368534415484106, 1.068504757029289695E-15 ) ) ;
#69060 = CARTESIAN_POINT ( 'NONE',  ( -5.056330833731841778, 15.00000000000000000, 13.58983143750696421 ) ) ;
#69061 = CARTESIAN_POINT ( 'NONE',  ( 0.1532563361054082862, 11.21726448433411782, 2.638427012816831674 ) ) ;
#69064 = ORIENTED_EDGE ( 'NONE', *, *, #19988, .T. ) ;
#69063 = VECTOR ( 'NONE', #75878, 1000.000000000000000 ) ;
#69062 = CARTESIAN_POINT ( 'NONE',  ( 8.134956207566084174, 15.00000000000000000, -13.77315809598639085 ) ) ;
#69065 = CARTESIAN_POINT ( 'NONE',  ( 17.20831665107776587, 42.88393115100077324, 7.208316651077764980 ) ) ;
#69066 = ORIENTED_EDGE ( 'NONE', *, *, #68208, .T. ) ;
#69067 = ORIENTED_EDGE ( 'NONE', *, *, #75307, .T. ) ;
#69068 = CARTESIAN_POINT ( 'NONE',  ( 0.1532563361054100626, 65.80059781766745175, -2.638427012816831230 ) ) ;
#69069 = VECTOR ( 'NONE', #31776, 1000.000000000000114 ) ;
#69070 = AXIS2_PLACEMENT_3D ( 'NONE', #97131, #14104, #14611 ) ;
#69071 = CIRCLE ( 'NONE', #8405, 0.2500000000000002220 ) ;
#69072 = CARTESIAN_POINT ( 'NONE',  ( -0.3689425029237881626, 17.42874883491397142, 10.36894250292379027 ) ) ;
#69073 = CARTESIAN_POINT ( 'NONE',  ( 20.04068437667225311, 29.71974360917721114, 6.396802510829709298 ) ) ;
#69074 = CARTESIAN_POINT ( 'NONE',  ( -3.420591144908684988, 14.49999999999999112, 14.60477854057959313 ) ) ;
#69075 = CARTESIAN_POINT ( 'NONE',  ( 10.00000000000000178, 14.31368534415483929, 10.88017736071110342 ) ) ;
#69077 = ORIENTED_EDGE ( 'NONE', *, *, #19004, .T. ) ;
#69076 = CARTESIAN_POINT ( 'NONE',  ( 6.565887622018943937, 43.08196800326374643, -12.81628187352647608 ) ) ;
#69079 = CIRCLE ( 'NONE', #25970, 11.99999999999999645 ) ;
#69078 =( NAMED_UNIT ( * ) PLANE_ANGLE_UNIT ( ) SI_UNIT ( $, .RADIAN. ) );
#69080 = CARTESIAN_POINT ( 'NONE',  ( 18.52753015748617571, 3.092264484334118269, 4.923371831947298993 ) ) ;
#69081 = CARTESIAN_POINT ( 'NONE',  ( 19.38216949554541557, 37.24863466993041783, -9.382169495545420901 ) ) ;
#69082 = CARTESIAN_POINT ( 'NONE',  ( 18.52753015748617571, 23.09226448433411960, 4.923371831947298993 ) ) ;
#69083 = EDGE_CURVE ( 'NONE', #92042, #20156, #93725, .T. ) ;
#69084 = DIRECTION ( 'NONE',  ( -0.3502073812594621582, 0.000000000000000000, -0.9366721892483996781 ) ) ;
#69085 = CARTESIAN_POINT ( 'NONE',  ( 13.43411237798105340, 20.58196800326374643, 12.81628187352647963 ) ) ;
#69086 = VECTOR ( 'NONE', #58658, 1000.000000000000114 ) ;
#69087 = FACE_OUTER_BOUND ( 'NONE', #14718, .T. ) ;
#69088 = CARTESIAN_POINT ( 'NONE',  ( 18.52753015748618282, 3.925597817667451306, -4.923371831947291888 ) ) ;
#69089 = ORIENTED_EDGE ( 'NONE', *, *, #59238, .T. ) ;
#69090 = ORIENTED_EDGE ( 'NONE', *, *, #47851, .T. ) ;
#69091 = CARTESIAN_POINT ( 'NONE',  ( 0.5774900079438607392, 28.48035201082150891, 5.440088680355550821 ) ) ;
#69092 = CARTESIAN_POINT ( 'NONE',  ( 10.00000000000000000, 20.55374883491396787, -14.16423886937410082 ) ) ;
#69093 = CARTESIAN_POINT ( 'NONE',  ( 1.472469842513823179, 40.59226448433411605, -4.923371831947296329 ) ) ;
#69094 = CARTESIAN_POINT ( 'NONE',  ( 17.96484262340118221, 64.93868534415483396, 7.964842623401181321 ) ) ;
#69096 = CARTESIAN_POINT ( 'NONE',  ( -6.560019409699617832, -50.64698701990471363, -2.750000000000000444 ) ) ;
#69095 = CARTESIAN_POINT ( 'NONE',  ( 22.81628187352647785, 46.62363466993041783, 6.195893100308588602E-16 ) ) ;
#69097 = CARTESIAN_POINT ( 'NONE',  ( 20.88017736071110164, 25.35535201082150891, 2.915334737309930979 ) ) ;
#69098 = CYLINDRICAL_SURFACE ( 'NONE', #7115, 0.1000000000000001166 ) ;
#69099 = AXIS2_PLACEMENT_3D ( 'NONE', #49373, #8917, #77904 ) ;
#69100 = CARTESIAN_POINT ( 'NONE',  ( 22.81628187352648496, 11.83196800326375531, -3.434112377981050290 ) ) ;
#69101 = CARTESIAN_POINT ( 'NONE',  ( 12.63842701281683922, 24.55059781766745175, -9.846743663894590881 ) ) ;
#69102 = CARTESIAN_POINT ( 'NONE',  ( -5.440088680355558814, -12.76964798917849109, -9.422509992056136596 ) ) ;
#69103 = CARTESIAN_POINT ( 'NONE',  ( -2.816281873526471635, 53.91530133659709634, -3.434112377981056508 ) ) ;
#69104 =( LENGTH_UNIT ( ) NAMED_UNIT ( * ) SI_UNIT ( .MILLI., .METRE. ) );
#69106 = CARTESIAN_POINT ( 'NONE',  ( 17.75000000000000711, 43.00000000000000000, 6.500000000000000888 ) ) ;
#69105 = CARTESIAN_POINT ( 'NONE',  ( 2.035157376598822676, 52.43868534415483396, -7.964842623401177768 ) ) ;
#69107 = SURFACE_STYLE_FILL_AREA ( #15133 ) ;
#69108 = CARTESIAN_POINT ( 'NONE',  ( 12.91533473730992121, 44.52201867748816966, 10.88017736071110164 ) ) ;
#69110 = CARTESIAN_POINT ( 'NONE',  ( 0.5774900079438590739, 42.64701867748816966, -5.440088680355550821 ) ) ;
#69109 = VECTOR ( 'NONE', #23321, 1000.000000000000227 ) ;
#69111 = CARTESIAN_POINT ( 'NONE',  ( 14.92337183194729988, 59.34226448433412315, -8.527530157486177487 ) ) ;
#69112 = EDGE_CURVE ( 'NONE', #59804, #45794, #7703, .T. ) ;
#69113 = CARTESIAN_POINT ( 'NONE',  ( 4.559911319644449179, 62.23035201082150536, -9.422509992056141925 ) ) ;
#69114 = UNCERTAINTY_MEASURE_WITH_UNIT (LENGTH_MEASURE( 1.000000000000000082E-05 ), #57296, 'distance_accuracy_value', 'NONE');
#69115 = EDGE_CURVE ( 'NONE', #76088, #6068, #43983, .T. ) ;
#69116 = CARTESIAN_POINT ( 'NONE',  ( 14.92337183194729988, 54.34226448433412315, -8.527530157486177487 ) ) ;
#69118 = DIRECTION ( 'NONE',  ( -1.000000000000000000, 0.000000000000000000, 0.000000000000000000 ) ) ;
#69117 = CARTESIAN_POINT ( 'NONE',  ( 2.035157376598824452, 13.68868534415483751, 7.964842623401179544 ) ) ;
#69119 = CARTESIAN_POINT ( 'NONE',  ( 22.81628187352647785, 11.41530133659708390, 3.434112377981063169 ) ) ;
#69120 = VERTEX_POINT ( 'NONE', #25257 ) ;
#69121 = CARTESIAN_POINT ( 'NONE',  ( 19.42250999205614548, 35.98035201082151247, -5.440088680355545492 ) ) ;
#69123 = CARTESIAN_POINT ( 'NONE',  ( 1.909764518474464046, 0.000000000000000000, -5.107897229450591325 ) ) ;
#69122 = CARTESIAN_POINT ( 'NONE',  ( 13.43411237798106583, 2.665301336597086568, -12.81628187352647252 ) ) ;
#69124 = CARTESIAN_POINT ( 'NONE',  ( 4.559911319644449179, 13.89701867748817143, 9.422509992056141925 ) ) ;
#69125 = CARTESIAN_POINT ( 'NONE',  ( 17.96484262340118221, 24.93868534415484461, 7.964842623401181321 ) ) ;
#69126 = CARTESIAN_POINT ( 'NONE',  ( 10.00000000000000000, 35.55374883491396787, -14.16423886937410082 ) ) ;
#69127 = CARTESIAN_POINT ( 'NONE',  ( 18.52753015748618282, 33.92559781766745886, -4.923371831947291888 ) ) ;
#69128 = CARTESIAN_POINT ( 'NONE',  ( 19.42250999205614548, 40.98035201082150536, -5.440088680355545492 ) ) ;
#69129 = CARTESIAN_POINT ( 'NONE',  ( 0.8217048220044697038, 14.95037104781115467, 14.73031263975989269 ) ) ;
#69130 = CARTESIAN_POINT ( 'NONE',  ( 6.204703633549690345, 7.845415501580634832, 14.16423886937410082 ) ) ;
#69131 = UNCERTAINTY_MEASURE_WITH_UNIT (LENGTH_MEASURE( 1.000000000000000082E-05 ), #47099, 'distance_accuracy_value', 'NONE');
#69132 = AXIS2_PLACEMENT_3D ( 'NONE', #46847, #62335, #15882 ) ;
#69133 = PRESENTATION_STYLE_ASSIGNMENT (( #92605 ) ) ;
#69134 = CARTESIAN_POINT ( 'NONE',  ( 0.1532563361054100626, 60.80059781766744464, -2.638427012816831230 ) ) ;
#69135 = ORIENTED_EDGE ( 'NONE', *, *, #38319, .F. ) ;
#69136 = ORIENTED_EDGE ( 'NONE', *, *, #18083, .T. ) ;
#69137 = CARTESIAN_POINT ( 'NONE',  ( -2.266590686148945544, 41.38708216824729647, -7.082119434687050408 ) ) ;
#69138 = CARTESIAN_POINT ( 'NONE',  ( -0.3689425029237881626, 32.42874883491395366, 10.36894250292379027 ) ) ;
#69139 = CARTESIAN_POINT ( 'NONE',  ( 5.076628168052704559, 5.175597817667451750, -8.527530157486179263 ) ) ;
#69140 = CARTESIAN_POINT ( 'NONE',  ( 18.52753015748617571, 63.09226448433412315, 4.923371831947298993 ) ) ;
#69141 = CARTESIAN_POINT ( 'NONE',  ( -11.58061176244991053, -84.07454167686546498, 3.750000000000000000 ) ) ;
#69143 = CARTESIAN_POINT ( 'NONE',  ( 0.6178305044545838731, 19.74863466993042138, 9.382169495545420901 ) ) ;
#69142 = CARTESIAN_POINT ( 'NONE',  ( 12.91533473730992121, 54.52201867748816255, 10.88017736071110164 ) ) ;
#69144 = CARTESIAN_POINT ( 'NONE',  ( 2.917880565312948704, 32.63708216824730357, 12.26659068614894643 ) ) ;
#69145 = CARTESIAN_POINT ( 'NONE',  ( 20.88017736071110519, 15.56368534415483751, 2.639326808657452039E-16 ) ) ;
#69146 = COLOUR_RGB ( '', 0.66274510, 0.83137255, 0.94901961) ;
#69147 = CARTESIAN_POINT ( 'NONE',  ( 19.42250999205614193, 30.14701867748817321, 5.440088680355555262 ) ) ;
#69148 = VECTOR ( 'NONE', #64383, 1000.000000000000000 ) ;
#69149 = CARTESIAN_POINT ( 'NONE',  ( -35.44000000000001194, 93.50000000000000000, -10.09898361729590199 ) ) ;
#69150 = CARTESIAN_POINT ( 'NONE',  ( -0.8801773607110991993, 52.85535201082151247, -2.915334737309923874 ) ) ;
#69151 = MECHANICAL_DESIGN_GEOMETRIC_PRESENTATION_REPRESENTATION (  '', ( #86700 ), #80416 ) ;
#69152 = CARTESIAN_POINT ( 'NONE',  ( -2.816281873526471635, 48.91530133659708213, -3.434112377981056508 ) ) ;
#69153 = CARTESIAN_POINT ( 'NONE',  ( -7.208316651077756099, -8.366068848999207219, 7.208316651077766757 ) ) ;
#69154 = EDGE_LOOP ( 'NONE', ( #83191, #96939, #69064, #43061, #77423, #38665 ) ) ;
#69155 = SURFACE_STYLE_FILL_AREA ( #38650 ) ;
#69156 = CIRCLE ( 'NONE', #48439, 15.00000000000000000 ) ;
#69157 = ORIENTED_EDGE ( 'NONE', *, *, #30598, .T. ) ;
#69158 = ORIENTED_EDGE ( 'NONE', *, *, #66244, .T. ) ;
#69159 = CARTESIAN_POINT ( 'NONE',  ( 20.36894250292379382, 8.678748834913967869, 10.36894250292379205 ) ) ;
#69161 = CARTESIAN_POINT ( 'NONE',  ( 10.00000000000000000, 1.813685344154838175, -10.88017736071110342 ) ) ;
#69160 = CARTESIAN_POINT ( 'NONE',  ( 24.16423886937410614, 54.51208216824730357, -3.795296366450302550 ) ) ;
#69163 = CARTESIAN_POINT ( 'NONE',  ( 0.1532563361054100626, 55.80059781766745175, -2.638427012816831230 ) ) ;
#69162 = CARTESIAN_POINT ( 'NONE',  ( 10.00000000000000178, 22.25893115100078745, 9.846743663894594434 ) ) ;
#69164 =( LENGTH_UNIT ( ) NAMED_UNIT ( * ) SI_UNIT ( .MILLI., .METRE. ) );
#69165 = CARTESIAN_POINT ( 'NONE',  ( 20.04068437667227798, 49.71974360917720048, 6.396802510829645350 ) ) ;
#69167 = CARTESIAN_POINT ( 'NONE',  ( -1.099225684535947600, 33.70696800326375353, -6.408140936763238038 ) ) ;
#69166 = CARTESIAN_POINT ( 'NONE',  ( -1.099225684535947600, 4.540301336597087456, 6.408140936763237150 ) ) ;
#69168 = CARTESIAN_POINT ( 'NONE',  ( -3.434112377981047626, 25.16530133659708213, 12.81628187352647963 ) ) ;
#69169 = ORIENTED_EDGE ( 'NONE', *, *, #21116, .T. ) ;
#69170 = CARTESIAN_POINT ( 'NONE',  ( 10.00000000000000178, 28.05374883491396787, 14.16423886937410082 ) ) ;
#69171 = ORIENTED_EDGE ( 'NONE', *, *, #85151, .T. ) ;
#69172 = CARTESIAN_POINT ( 'NONE',  ( 2.917880565312950480, 40.97041550158063217, -12.26659068614894821 ) ) ;
#69173 = ORIENTED_EDGE ( 'NONE', *, *, #43710, .T. ) ;
#69174 = CARTESIAN_POINT ( 'NONE',  ( 22.81628187352647785, 51.41530133659708923, 3.434112377981063169 ) ) ;
#69175 = CARTESIAN_POINT ( 'NONE',  ( 2.035157376598824452, 23.68868534415484461, 7.964842623401179544 ) ) ;
#69176 = CARTESIAN_POINT ( 'NONE',  ( 10.00000000000000178, 52.25893115100078745, 9.846743663894594434 ) ) ;
#69177 = CARTESIAN_POINT ( 'NONE',  ( 12.91533473730992121, 24.52201867748816966, 10.88017736071110164 ) ) ;
#69178 = CARTESIAN_POINT ( 'NONE',  ( -6.732636091893173358, -88.11213685669363826, 2.500000000000000000 ) ) ;
#69179 = CARTESIAN_POINT ( 'NONE',  ( 7.361572987183169658, 49.96726448433410894, -9.846743663894592657 ) ) ;
#69180 = CARTESIAN_POINT ( 'NONE',  ( 0.1532563361054100626, 50.80059781766745175, -2.638427012816831230 ) ) ;
#69181 = CIRCLE ( 'NONE', #21284, 0.2499999999999997224 ) ;
#69182 = CARTESIAN_POINT ( 'NONE',  ( -7.551349515323269479, 0.000000000000000000, 12.08468537022900868 ) ) ;
#69183 = AXIS2_PLACEMENT_3D ( 'NONE', #16430, #8915, #39431 ) ;
#69184 = CARTESIAN_POINT ( 'NONE',  ( 0.000000000000000000, 0.000000000000000000, 0.000000000000000000 ) ) ;
#69185 = CARTESIAN_POINT ( 'NONE',  ( 7.361572987183170547, 7.050597817667451750, 9.846743663894590881 ) ) ;
#69186 = CARTESIAN_POINT ( 'NONE',  ( 17.39651004071838969, 59.08210964143329846, -6.500000000000027534 ) ) ;
#69187 = EDGE_LOOP ( 'NONE', ( #55253, #77392, #10247, #7806 ) ) ;
#69188 = CARTESIAN_POINT ( 'NONE',  ( 12.63842701281683922, 34.55059781766745886, -9.846743663894590881 ) ) ;
#69189 = CARTESIAN_POINT ( 'NONE',  ( 12.24319267753454099, 54.01141590572475337, -2.900000000000000799 ) ) ;
#69190 = CARTESIAN_POINT ( 'NONE',  ( 16.40814093676324603, 42.45696800326375353, -11.09922568453594671 ) ) ;
#69191 =( NAMED_UNIT ( * ) SI_UNIT ( $, .STERADIAN. ) SOLID_ANGLE_UNIT ( ) );
#69192 = CARTESIAN_POINT ( 'NONE',  ( -3.500000000000000444, -0.04521315095527938394, 2.750000000000000000 ) ) ;
#69193 = ORIENTED_EDGE ( 'NONE', *, *, #64795, .T. ) ;
#69194 = DIRECTION ( 'NONE',  ( 0.000000000000000000, 1.000000000000000000, 0.000000000000000000 ) ) ;
#69195 = CARTESIAN_POINT ( 'NONE',  ( 2.791683348922240793, 56.63393115100078035, 7.208316651077764092 ) ) ;
#69196 = CARTESIAN_POINT ( 'NONE',  ( -0.3689425029237881626, 37.42874883491396787, 10.36894250292379027 ) ) ;
#69197 = CARTESIAN_POINT ( 'NONE',  ( 10.00000000000000000, 59.75893115100078745, -9.846743663894594434 ) ) ;
#69198 = CARTESIAN_POINT ( 'NONE',  ( 13.82192141328812518, 15.00000000000000000, -4.382292601468683380 ) ) ;
#69199 = CARTESIAN_POINT ( 'NONE',  ( 5.076628168052704559, 25.17559781766745175, -8.527530157486179263 ) ) ;
#69200 = CARTESIAN_POINT ( 'NONE',  ( -1.099225684535947600, 53.70696800326376064, -6.408140936763238038 ) ) ;
#69201 = CARTESIAN_POINT ( 'NONE',  ( 22.26659068614894466, 3.887082168247300906, 7.082119434687054849 ) ) ;
#69202 = CARTESIAN_POINT ( 'NONE',  ( 2.791683348922240793, 61.63393115100079456, 7.208316651077764092 ) ) ;
#69203 = CARTESIAN_POINT ( 'NONE',  ( 2.035157376598822676, 47.43868534415484817, -7.964842623401177768 ) ) ;
#69204 = ADVANCED_FACE ( 'NONE', ( #55743 ), #51411, .T. ) ;
#69205 = CARTESIAN_POINT ( 'NONE',  ( 0.1532563361054082862, 46.21726448433411605, 2.638427012816831674 ) ) ;
#69206 = CARTESIAN_POINT ( 'NONE',  ( -10.32896413005679470, 8.078790035174483464, 5.963430220938290560 ) ) ;
#69207 = CARTESIAN_POINT ( 'NONE',  ( 12.91533473730992121, 59.52201867748816966, 10.88017736071110164 ) ) ;
#69208 = VERTEX_POINT ( 'NONE', #96704 ) ;
#69209 = DIRECTION ( 'NONE',  ( -4.529709940470638685E-14, 0.000000000000000000, 1.000000000000000000 ) ) ;
#69210 = CARTESIAN_POINT ( 'NONE',  ( 17.96484262340118221, 29.93868534415484106, 7.964842623401181321 ) ) ;
#69212 = CARTESIAN_POINT ( 'NONE',  ( 2.035157376598824452, 58.68868534415482685, 7.964842623401179544 ) ) ;
#69211 = CARTESIAN_POINT ( 'NONE',  ( 0.6178305044545818747, 3.498634669930420049, -9.382169495545419124 ) ) ;
#69213 = DIRECTION ( 'NONE',  ( 1.000000000000000000, -0.000000000000000000, -0.000000000000000000 ) ) ;
#69214 = CARTESIAN_POINT ( 'NONE',  ( -27.43587634952537968, 11.50000000000000000, -10.00000000000000000 ) ) ;
#69215 = FILL_AREA_STYLE_COLOUR ( '', #11818 ) ;
#69217 = LINE ( 'NONE', #67741, #20786 ) ;
#69216 = CARTESIAN_POINT ( 'NONE',  ( 10.00000000000000178, 44.31368534415484106, 10.88017736071110342 ) ) ;
#69218 = CARTESIAN_POINT ( 'NONE',  ( 10.00000000000000178, 32.25893115100078745, 9.846743663894594434 ) ) ;
#69219 = DIRECTION ( 'NONE',  ( 0.5547001962252290364, 0.8320502943378437211, 0.000000000000000000 ) ) ;
#69220 = AXIS2_PLACEMENT_3D ( 'NONE', #8798, #63263, #17302 ) ;
#69221 = CARTESIAN_POINT ( 'NONE',  ( 12.26659068614894821, 23.88708216824731068, 7.082119434687044190 ) ) ;
#69222 = CARTESIAN_POINT ( 'NONE',  ( 2.791683348922237240, 60.38393115100078745, -7.208316651077763204 ) ) ;
#69223 = CARTESIAN_POINT ( 'NONE',  ( 0.5774900079438607392, 8.480352010821505360, 5.440088680355550821 ) ) ;
#69224 = CARTESIAN_POINT ( 'NONE',  ( 6.579634127946653699, -87.99828267815712479, 2.750000000000002665 ) ) ;
#69225 = CARTESIAN_POINT ( 'NONE',  ( 17.08211943468705130, 28.47041550158063572, 12.26659068614894998 ) ) ;
#69226 = B_SPLINE_CURVE_WITH_KNOTS ( 'NONE', 3,
 ( #6230, #29210, #66219, #97251, #65227, #89228 ),
 .UNSPECIFIED., .F., .F.,
 ( 4, 2, 4 ),
 ( 3.409110551496067671E-05, 0.0004400426677367857043, 0.0008459942299586107250 ),
 .UNSPECIFIED. ) ;
#69227 = CARTESIAN_POINT ( 'NONE',  ( 22.26659068614894466, 63.88708216824730357, 7.082119434687054849 ) ) ;
#69228 = CARTESIAN_POINT ( 'NONE',  ( 14.92337183194729988, 34.34226448433411605, -8.527530157486177487 ) ) ;
#69229 = CARTESIAN_POINT ( 'NONE',  ( 14.92337183194729633, 22.67559781766745175, 8.527530157486181039 ) ) ;
#69230 = CARTESIAN_POINT ( 'NONE',  ( 15.44008868035555793, 6.397018677488170546, -9.422509992056140149 ) ) ;
#69231 = ORIENTED_EDGE ( 'NONE', *, *, #12330, .F. ) ;
#69232 = CARTESIAN_POINT ( 'NONE',  ( 1.472469842513823179, 26.42559781766745175, 4.923371831947296329 ) ) ;
#69233 = EDGE_CURVE ( 'NONE', #26361, #22285, #50798, .T. ) ;
#69234 = CARTESIAN_POINT ( 'NONE',  ( 19.42250999205614193, 30.14701867748817321, 5.440088680355555262 ) ) ;
#69235 = CARTESIAN_POINT ( 'NONE',  ( 2.791683348922240793, 66.63393115100079456, 7.208316651077764092 ) ) ;
#69237 =( LENGTH_UNIT ( ) NAMED_UNIT ( * ) SI_UNIT ( .MILLI., .METRE. ) );
#69236 = CARTESIAN_POINT ( 'NONE',  ( 24.16423886937410614, 9.512082168247301794, -3.795296366450302550 ) ) ;
#69238 = DIRECTION ( 'NONE',  ( 0.8070303256584298035, -0.5905099943842175847, 0.000000000000000000 ) ) ;
#69239 =( BOUNDED_CURVE ( )  B_SPLINE_CURVE ( 2, ( #56744, #57719, #66206, #42734, #80231, #42246, #4251, #19730, #5239 ),
 .UNSPECIFIED., .F., .F. ) 
 B_SPLINE_CURVE_WITH_KNOTS ( ( 3, 2, 2, 2, 3 ),
 ( 0.2972837940830885262, 0.2976190476190476719, 0.3035714285714286031, 0.3095238095238095344, 0.3098590630597686801 ),
 .UNSPECIFIED. ) 
 CURVE ( )  GEOMETRIC_REPRESENTATION_ITEM ( )  RATIONAL_B_SPLINE_CURVE ( ( 0.9963778908391760503, 0.9980808541467920403, 1.000000000000000000, 0.9659258262890683122, 1.000000000000000000, 0.9659258262890683122, 1.000000000000000000, 0.9980808541467920403, 0.9963778908391759392 ) ) 
 REPRESENTATION_ITEM ( '' )  );
#69240 = CARTESIAN_POINT ( 'NONE',  ( 10.00000000000000178, 7.258931151000785675, 9.846743663894594434 ) ) ;
#69241 = CARTESIAN_POINT ( 'NONE',  ( -1.099225684535947600, 43.70696800326375353, -6.408140936763238038 ) ) ;
#69242 = B_SPLINE_CURVE_WITH_KNOTS ( 'NONE', 3,
 ( #44873, #29378, #45374, #98909, #82886, #75376 ),
 .UNSPECIFIED., .F., .F.,
 ( 4, 2, 4 ),
 ( 3.409110551494644656E-05, 0.0004400426677367928600, 0.0008459942299586393480 ),
 .UNSPECIFIED. ) ;
#69243 = CARTESIAN_POINT ( 'NONE',  ( 7.361572987183169658, 39.96726448433411605, -9.846743663894592657 ) ) ;
#69244 = ORIENTED_EDGE ( 'NONE', *, *, #6804, .T. ) ;
#69245 = CARTESIAN_POINT ( 'NONE',  ( 0.1532563361054083140, 21.00893115100078745, 1.131784320476157264E-15 ) ) ;
#69246 =( NAMED_UNIT ( * ) SI_UNIT ( $, .STERADIAN. ) SOLID_ANGLE_UNIT ( ) );
#69247 = CARTESIAN_POINT ( 'NONE',  ( 14.62617646268092031, 14.63606916781938772, -3.327906561566877919 ) ) ;
#69248 = CARTESIAN_POINT ( 'NONE',  ( 20.36894250292379738, 49.92874883491396787, -10.36894250292379027 ) ) ;
#69249 = CARTESIAN_POINT ( 'NONE',  ( 2.035157376598824452, 53.68868534415484817, 7.964842623401179544 ) ) ;
#69250 = CARTESIAN_POINT ( 'NONE',  ( 10.00000000000000000, 0.5537488349139675359, -14.16423886937410082 ) ) ;
#69251 = CARTESIAN_POINT ( 'NONE',  ( 20.88017736071110875, 60.77201867748817676, -2.915334737309920765 ) ) ;
#69252 = CARTESIAN_POINT ( 'NONE',  ( 19.84674366389459621, 43.50893115100078745, 7.409399052514197653E-17 ) ) ;
#69253 = CARTESIAN_POINT ( 'NONE',  ( 4.559911319644449179, 2.230352010821504471, -9.422509992056141925 ) ) ;
#69254 = CARTESIAN_POINT ( 'NONE',  ( 18.17829156368506105, 39.16792564121896447, 6.500000000000047073 ) ) ;
#69255 = CARTESIAN_POINT ( 'NONE',  ( 12.63842701281683034, 47.46726448433412315, 9.846743663894596210 ) ) ;
#69256 = CARTESIAN_POINT ( 'NONE',  ( 15.44008868035555793, 51.39701867748816966, -9.422509992056140149 ) ) ;
#69257 = CARTESIAN_POINT ( 'NONE',  ( 19.84674366389459621, 3.508931151000785231, 7.409399052514197653E-17 ) ) ;
#69258 = UNCERTAINTY_MEASURE_WITH_UNIT (LENGTH_MEASURE( 1.000000000000000082E-05 ), #21545, 'distance_accuracy_value', 'NONE');
#69259 = ORIENTED_EDGE ( 'NONE', *, *, #67956, .F. ) ;
#69260 = VERTEX_POINT ( 'NONE', #64682 ) ;
#69261 = DIRECTION ( 'NONE',  ( -0.000000000000000000, 1.000000000000000000, -0.000000000000000000 ) ) ;
#69262 = CARTESIAN_POINT ( 'NONE',  ( 14.99999999999997868, 80.07179676972448590, 6.500000000000000888 ) ) ;
#69263 = CARTESIAN_POINT ( 'NONE',  ( 0.1532563361054100626, 15.80059781766745353, -2.638427012816831230 ) ) ;
#69264 = CARTESIAN_POINT ( 'NONE',  ( 21.09922568453595559, 62.04030133659709634, -6.408140936763230044 ) ) ;
#69266 = CARTESIAN_POINT ( 'NONE',  ( 0.1532563361054082862, 46.21726448433411605, 2.638427012816831674 ) ) ;
#69265 = CARTESIAN_POINT ( 'NONE',  ( 19.42250999205614193, 15.14701867748817143, 5.440088680355555262 ) ) ;
#69267 = CARTESIAN_POINT ( 'NONE',  ( 11.35178980618974975, 0.3640475087720984604, -9.804941009311923139 ) ) ;
#69268 = CARTESIAN_POINT ( 'NONE',  ( 2.917880565312950480, 25.97041550158063572, -12.26659068614894821 ) ) ;
#69269 = CARTESIAN_POINT ( 'NONE',  ( -4.164238869374099927, 52.01208216824729647, 3.795296366450308767 ) ) ;
#69270 = CARTESIAN_POINT ( 'NONE',  ( 18.52753015748617571, 53.09226448433412315, 4.923371831947298993 ) ) ;
#69271 = CARTESIAN_POINT ( 'NONE',  ( -12.00809552683947068, 14.63595249122795394, -8.989195838243713155 ) ) ;
#69272 = CARTESIAN_POINT ( 'NONE',  ( 2.035157376598822676, 57.43868534415484106, -7.964842623401177768 ) ) ;
#69273 = CARTESIAN_POINT ( 'NONE',  ( 17.20831665107776587, 17.88393115100078745, 7.208316651077764980 ) ) ;
#69274 = EDGE_CURVE ( 'NONE', #18090, #83143, #50691, .T. ) ;
#69275 = ORIENTED_EDGE ( 'NONE', *, *, #22774, .T. ) ;
#69276 = CARTESIAN_POINT ( 'NONE',  ( 13.82671409943296226, 15.00000000000000000, -3.447387012295225261 ) ) ;
#69277 = CARTESIAN_POINT ( 'NONE',  ( 14.92337183194729633, 12.67559781766745353, 8.527530157486181039 ) ) ;
#69278 = ORIENTED_EDGE ( 'NONE', *, *, #29241, .F. ) ;
#69279 = CARTESIAN_POINT ( 'NONE',  ( 13.79529636645031943, 20.34541550158063572, -14.16423886937409904 ) ) ;
#69280 = CARTESIAN_POINT ( 'NONE',  ( 0.1532563361054100626, 15.80059781766745353, -2.638427012816831230 ) ) ;
#69281 = CARTESIAN_POINT ( 'NONE',  ( 19.42250999205614193, 50.14701867748817676, 5.440088680355555262 ) ) ;
#69282 = ADVANCED_FACE ( 'NONE', ( #80195 ), #98721, .T. ) ;
#69283 = FILL_AREA_STYLE ('',( #80820 ) ) ;
#69284 = ORIENTED_EDGE ( 'NONE', *, *, #66853, .F. ) ;
#69285 = CARTESIAN_POINT ( 'NONE',  ( 19.42250999205614193, 30.14701867748817321, 5.440088680355555262 ) ) ;
#69286 = TOROIDAL_SURFACE ( 'NONE', #48494, 14.49999999999999822, 0.5000000000000000000 ) ;
#69287 = ORIENTED_EDGE ( 'NONE', *, *, #11863, .T. ) ;
#69288 = CARTESIAN_POINT ( 'NONE',  ( 12.91533473730992121, 39.52201867748817676, 10.88017736071110164 ) ) ;
#69289 = VECTOR ( 'NONE', #21131, 1000.000000000000114 ) ;
#69290 = EDGE_CURVE ( 'NONE', #23479, #93500, #53937, .T. ) ;
#69291 = EDGE_LOOP ( 'NONE', ( #90923, #74066, #18238, #73237, #10263, #35769 ) ) ;
#69292 = CARTESIAN_POINT ( 'NONE',  ( 22.81628187352647785, 16.41530133659708923, 3.434112377981063169 ) ) ;
#69293 = CARTESIAN_POINT ( 'NONE',  ( 2.791683348922237240, 15.38393115100078212, -7.208316651077763204 ) ) ;
#69294 = DIRECTION ( 'NONE',  ( -0.000000000000000000, -1.000000000000000000, -0.000000000000000000 ) ) ;
#69295 = CARTESIAN_POINT ( 'NONE',  ( 10.00000000000000000, 19.75893115100078390, -9.846743663894594434 ) ) ;
#69296 = CARTESIAN_POINT ( 'NONE',  ( 17.96484262340118221, 26.18868534415483396, -7.964842623401177768 ) ) ;
#69297 = ORIENTED_EDGE ( 'NONE', *, *, #23694, .F. ) ;
#69298 = CARTESIAN_POINT ( 'NONE',  ( 13.43411237798106583, 62.66530133659708923, -12.81628187352647252 ) ) ;
#69299 = CARTESIAN_POINT ( 'NONE',  ( 12.91533473730993009, 56.60535201082151247, -10.88017736071109987 ) ) ;
#69300 = CARTESIAN_POINT ( 'NONE',  ( -46.48928645636215151, 103.2957187381725248, -6.397878122524185862 ) ) ;
#69301 =( LENGTH_UNIT ( ) NAMED_UNIT ( * ) SI_UNIT ( .MILLI., .METRE. ) );
#69302 = CARTESIAN_POINT ( 'NONE',  ( 12.91533473730993009, 66.60535201082150536, -10.88017736071109987 ) ) ;
#69303 = CARTESIAN_POINT ( 'NONE',  ( 10.00000000000000178, 5.373634669930420493, 12.81628187352647608 ) ) ;
#69304 = CARTESIAN_POINT ( 'NONE',  ( 4.600000000000003197, 98.49999999999998579, 8.000000000000000000 ) ) ;
#69305 = CARTESIAN_POINT ( 'NONE',  ( 1.472469842513823179, 30.59226448433411960, -4.923371831947296329 ) ) ;
#69306 = CARTESIAN_POINT ( 'NONE',  ( -2.816281873526471635, 53.91530133659709634, -3.434112377981056508 ) ) ;
#69307 = CARTESIAN_POINT ( 'NONE',  ( 1.711636803080583080, 36.84492782695769364, -6.500000000000066613 ) ) ;
#69308 = CARTESIAN_POINT ( 'NONE',  ( 1.472469842513823179, 25.59226448433412315, -4.923371831947296329 ) ) ;
#69309 = CARTESIAN_POINT ( 'NONE',  ( 21.09922568453595559, 17.04030133659708923, -6.408140936763230044 ) ) ;
#69311 = CARTESIAN_POINT ( 'NONE',  ( -6.030799524552431734, -39.80423606248630364, -2.750000000000000000 ) ) ;
#69310 = CARTESIAN_POINT ( 'NONE',  ( -2.261421327065682441, 0.000000000000000000, -4.962236210031271355 ) ) ;
#69312 = CARTESIAN_POINT ( 'NONE',  ( 19.42250999205614193, 30.14701867748817321, 5.440088680355555262 ) ) ;
#69313 = CARTESIAN_POINT ( 'NONE',  ( 19.84674366389459266, 58.71726448433411605, -2.638427012816827677 ) ) ;
#69314 = CARTESIAN_POINT ( 'NONE',  ( 1.472469842513823179, 15.59226448433411960, -4.923371831947296329 ) ) ;
#69315 = CARTESIAN_POINT ( 'NONE',  ( 18.52753015748617571, 8.092264484334117824, 4.923371831947298993 ) ) ;
#69316 = CARTESIAN_POINT ( 'NONE',  ( 2.035157376598822676, 7.438685344154837509, -7.964842623401177768 ) ) ;
#69317 = EDGE_CURVE ( 'NONE', #32549, #8076, #42215, .T. ) ;
#69318 = CARTESIAN_POINT ( 'NONE',  ( 19.38216949554541202, 20.99863466993042138, 9.382169495545424454 ) ) ;
#69319 = CARTESIAN_POINT ( 'NONE',  ( 4.559911319644449179, 3.897018677488170990, 9.422509992056141925 ) ) ;
#69320 = SURFACE_STYLE_USAGE ( .BOTH. , #82832 ) ;
#69321 = CARTESIAN_POINT ( 'NONE',  ( 19.84674366389459266, 58.30059781766745886, 2.638427012816836559 ) ) ;
#69322 = CARTESIAN_POINT ( 'NONE',  ( 4.221206346829659672, -3.619822760609359591, -2.500000000000000000 ) ) ;
#69324 = ADVANCED_FACE ( 'NONE', ( #72682 ), #65181, .F. ) ;
#69323 = CARTESIAN_POINT ( 'NONE',  ( 12.91533473730992121, 14.52201867748817143, 10.88017736071110164 ) ) ;
#69325 = CARTESIAN_POINT ( 'NONE',  ( 1.472469842513823179, 41.42559781766745886, 4.923371831947296329 ) ) ;
#69326 = CARTESIAN_POINT ( 'NONE',  ( 4.380000000000002558, 1.019547802438462547, 2.750000000000000000 ) ) ;
#69327 = CARTESIAN_POINT ( 'NONE',  ( 4.559911319644449179, 18.89701867748817321, 9.422509992056141925 ) ) ;
#69328 = CARTESIAN_POINT ( 'NONE',  ( 32.56412365047463453, 26.99999999999998224, 10.00000000000000000 ) ) ;
#69329 = CARTESIAN_POINT ( 'NONE',  ( 19.42250999205614193, 35.14701867748816966, 5.440088680355555262 ) ) ;
#69330 = CARTESIAN_POINT ( 'NONE',  ( -0.3689425029237898834, 66.17874883491396076, -10.36894250292378850 ) ) ;
#69331 = CARTESIAN_POINT ( 'NONE',  ( 14.92337183194729633, 22.67559781766745175, 8.527530157486181039 ) ) ;
#69332 = CARTESIAN_POINT ( 'NONE',  ( 6.565887622018943937, 13.08196800326374998, -12.81628187352647608 ) ) ;
#69333 = CARTESIAN_POINT ( 'NONE',  ( -46.86082856188268408, 103.4709495335575156, 5.834510888469651491 ) ) ;
#69334 = DIRECTION ( 'NONE',  ( 0.000000000000000000, 1.000000000000000000, 0.000000000000000000 ) ) ;
#69335 = DIRECTION ( 'NONE',  ( -1.000000000000000000, 0.000000000000000000, 0.000000000000000000 ) ) ;
#69336 = CARTESIAN_POINT ( 'NONE',  ( -8.647966315087309397, -15.58183027064585779, -4.000000000000000000 ) ) ;
#69337 = CARTESIAN_POINT ( 'NONE',  ( -4.164238869374099927, 17.01208216824730357, 3.795296366450308767 ) ) ;
#69338 = CARTESIAN_POINT ( 'NONE',  ( 2.791683348922237240, 35.38393115100079456, -7.208316651077763204 ) ) ;
#69339 = FACE_OUTER_BOUND ( 'NONE', #1641, .T. ) ;
#69340 = EDGE_CURVE ( 'NONE', #51116, #59690, #60347, .T. ) ;
#69341 = CIRCLE ( 'NONE', #19865, 14.49999999999999822 ) ;
#69342 = CARTESIAN_POINT ( 'NONE',  ( 10.00000000000000000, 50.55374883491396787, -14.16423886937410082 ) ) ;
#69343 = CARTESIAN_POINT ( 'NONE',  ( 14.92337183194729633, 27.67559781766745530, 8.527530157486181039 ) ) ;
#69345 = DIRECTION ( 'NONE',  ( 0.000000000000000000, 0.000000000000000000, -1.000000000000000000 ) ) ;
#69344 = CARTESIAN_POINT ( 'NONE',  ( 5.451370222425311773, 0.000000000000000000, -0.1427491530890097615 ) ) ;
#69346 = CARTESIAN_POINT ( 'NONE',  ( 0.5774900079438607392, 48.48035201082150536, 5.440088680355550821 ) ) ;
#69347 = CARTESIAN_POINT ( 'NONE',  ( -2.816281873526471635, 48.91530133659708213, -3.434112377981056508 ) ) ;
#69348 = CARTESIAN_POINT ( 'NONE',  ( 0.5774900079438590739, 22.64701867748817321, -5.440088680355550821 ) ) ;
#69349 = CARTESIAN_POINT ( 'NONE',  ( 21.09922568453595559, 52.04030133659708923, -6.408140936763230044 ) ) ;
#69350 = CARTESIAN_POINT ( 'NONE',  ( 10.00000000000000178, 0.3736346699304200492, 12.81628187352647608 ) ) ;
#69351 = CARTESIAN_POINT ( 'NONE',  ( 0.1532563361054082862, 6.217264484334118713, 2.638427012816831674 ) ) ;
#69353 = VERTEX_POINT ( 'NONE', #27187 ) ;
#69352 = EDGE_CURVE ( 'NONE', #74689, #55012, #35686, .T. ) ;
#69354 = AXIS2_PLACEMENT_3D ( 'NONE', #75981, #44983, #74996 ) ;
#69355 = CARTESIAN_POINT ( 'NONE',  ( -3.750000000000000000, 10.00000000000000000, 3.750000000000000000 ) ) ;
#69356 = CARTESIAN_POINT ( 'NONE',  ( -14.49440716394873085, 4.311470567659570904E-16, -0.4026921475168178111 ) ) ;
#69357 = CARTESIAN_POINT ( 'NONE',  ( 10.00000000000000000, 60.55374883491397497, -14.16423886937410082 ) ) ;
#69358 = CARTESIAN_POINT ( 'NONE',  ( 2.917880565312950480, 10.97041550158063572, -12.26659068614894821 ) ) ;
#69359 = CARTESIAN_POINT ( 'NONE',  ( 15.44008868035555793, 16.39701867748817321, -9.422509992056140149 ) ) ;
#69360 = CARTESIAN_POINT ( 'NONE',  ( 17.96484262340118221, 39.93868534415484106, 7.964842623401181321 ) ) ;
#69361 = CARTESIAN_POINT ( 'NONE',  ( 10.19513985507833453, 14.63595249122788999, -11.00268709613217943 ) ) ;
#69362 = CARTESIAN_POINT ( 'NONE',  ( -46.51339001641208881, 100.8236536580530895, -9.499999999999998224 ) ) ;
#69363 = CARTESIAN_POINT ( 'NONE',  ( 5.076628168052704559, 0.1755978176674514724, -8.527530157486179263 ) ) ;
#69364 = CARTESIAN_POINT ( 'NONE',  ( 17.96484262340118221, 64.93868534415483396, 7.964842623401181321 ) ) ;
#69365 = CARTESIAN_POINT ( 'NONE',  ( 22.81628187352647785, 26.62363466993042138, 6.195893100308588602E-16 ) ) ;
#69366 = CARTESIAN_POINT ( 'NONE',  ( 17.84635730667657683, 18.63791097397319874, 6.499999999999999112 ) ) ;
#69367 = FILL_AREA_STYLE_COLOUR ( '', #30782 ) ;
#69368 = CARTESIAN_POINT ( 'NONE',  ( 19.84674366389459621, 13.50893115100078568, 7.409399052514197653E-17 ) ) ;
#69369 = CARTESIAN_POINT ( 'NONE',  ( 17.20831665107776587, 42.88393115100077324, 7.208316651077764980 ) ) ;
#69370 = B_SPLINE_CURVE_WITH_KNOTS ( 'NONE', 3,
 ( #19121, #2680, #56633, #80111 ),
 .UNSPECIFIED., .F., .F.,
 ( 4, 4 ),
 ( 0.000000000000000000, 0.002657014572711344572 ),
 .UNSPECIFIED. ) ;
#69371 = CARTESIAN_POINT ( 'NONE',  ( 19.42250999205614548, 15.98035201082150714, -5.440088680355545492 ) ) ;
#69372 = CARTESIAN_POINT ( 'NONE',  ( 3.591859063236763294, 33.29030133659708213, -11.09922568453595026 ) ) ;
#69373 = CARTESIAN_POINT ( 'NONE',  ( 18.52753015748618282, 8.925597817667451750, -4.923371831947291888 ) ) ;
#69374 = LINE ( 'NONE', #896, #64580 ) ;
#69375 = CARTESIAN_POINT ( 'NONE',  ( 18.52753015748617571, 58.09226448433411605, 4.923371831947298993 ) ) ;
#69376 = CARTESIAN_POINT ( 'NONE',  ( 17.20831665107776587, 27.88393115100078390, 7.208316651077764980 ) ) ;
#69377 = CARTESIAN_POINT ( 'NONE',  ( 24.16423886937410614, 14.30374883491396787, 8.672049930838204340E-16 ) ) ;
#69378 = CARTESIAN_POINT ( 'NONE',  ( 17.96484262340118221, 36.18868534415484106, -7.964842623401177768 ) ) ;
#69379 = CARTESIAN_POINT ( 'NONE',  ( 2.035157376598824452, 8.688685344154839285, 7.964842623401179544 ) ) ;
#69380 = CARTESIAN_POINT ( 'NONE',  ( 7.084665262690076126, 32.02201867748816966, -10.88017736071110164 ) ) ;
#69381 = CARTESIAN_POINT ( 'NONE',  ( 12.91533473730992121, 34.52201867748817676, 10.88017736071110164 ) ) ;
#69382 = ORIENTED_EDGE ( 'NONE', *, *, #9140, .F. ) ;
#69383 = CARTESIAN_POINT ( 'NONE',  ( 12.91533473730992121, 34.52201867748817676, 10.88017736071110164 ) ) ;
#69384 = ORIENTED_EDGE ( 'NONE', *, *, #51023, .F. ) ;
#69385 = CIRCLE ( 'NONE', #96734, 8.000000000000007105 ) ;
#69386 = CARTESIAN_POINT ( 'NONE',  ( 10.00000000000000178, 55.37363466993042493, 12.81628187352647608 ) ) ;
#69387 = EDGE_CURVE ( 'NONE', #47240, #81206, #96202, .T. ) ;
#69388 = CARTESIAN_POINT ( 'NONE',  ( 4.559911319644449179, 52.23035201082151247, -9.422509992056141925 ) ) ;
#69389 = ORIENTED_EDGE ( 'NONE', *, *, #25883, .F. ) ;
#69390 = CARTESIAN_POINT ( 'NONE',  ( 20.88017736071110164, 55.35535201082149825, 2.915334737309930979 ) ) ;
#69391 = CARTESIAN_POINT ( 'NONE',  ( 6.757940885659567520, -58.32678904743372073, 3.999999999999999556 ) ) ;
#69392 = SURFACE_SIDE_STYLE ('',( #54866 ) ) ;
#69393 = CARTESIAN_POINT ( 'NONE',  ( 17.08211943468705840, 65.13708216824730357, -12.26659068614894466 ) ) ;
#69394 = CARTESIAN_POINT ( 'NONE',  ( 15.44008868035555793, 61.39701867748817676, -9.422509992056140149 ) ) ;
#69395 = CARTESIAN_POINT ( 'NONE',  ( 0.6076426042653105819, 52.37576471608601736, -6.499999999999992006 ) ) ;
#69396 = CARTESIAN_POINT ( 'NONE',  ( -5.580435433942703582, -28.67474180225207547, -3.999999999999998224 ) ) ;
#69397 = CARTESIAN_POINT ( 'NONE',  ( 4.559911319644449179, 2.230352010821504471, -9.422509992056141925 ) ) ;
#69398 = CARTESIAN_POINT ( 'NONE',  ( 17.20831665107776587, 27.88393115100078390, 7.208316651077764980 ) ) ;
#69399 = ORIENTED_EDGE ( 'NONE', *, *, #76676, .F. ) ;
#69400 = CARTESIAN_POINT ( 'NONE',  ( 0.1532563361054100626, 35.80059781766745175, -2.638427012816831230 ) ) ;
#69401 = MECHANICAL_DESIGN_GEOMETRIC_PRESENTATION_REPRESENTATION (  '', ( #7171 ), #32706 ) ;
#69402 = CARTESIAN_POINT ( 'NONE',  ( 10.00000000000000000, 36.81368534415484106, -10.88017736071110342 ) ) ;
#69403 = CARTESIAN_POINT ( 'NONE',  ( 1.472469842513823179, 35.59226448433412315, -4.923371831947296329 ) ) ;
#69404 = CARTESIAN_POINT ( 'NONE',  ( 22.81628187352647785, 26.41530133659708923, 3.434112377981063169 ) ) ;
#69406 = CARTESIAN_POINT ( 'NONE',  ( 10.00000000000000000, 66.81368534415484817, -10.88017736071110342 ) ) ;
#69405 = CARTESIAN_POINT ( 'NONE',  ( 20.15039907845753930, 2.627771745786128044, -6.262539305110069954 ) ) ;
#69407 = CARTESIAN_POINT ( 'NONE',  ( 19.42250999205614548, 50.98035201082151247, -5.440088680355545492 ) ) ;
#69408 = CARTESIAN_POINT ( 'NONE',  ( -4.164238869374098151, 56.59541550158063927, -3.795296366450310543 ) ) ;
#69409 = CARTESIAN_POINT ( 'NONE',  ( 13.43411237798106583, 27.66530133659708568, -12.81628187352647252 ) ) ;
#69410 = CARTESIAN_POINT ( 'NONE',  ( 17.74999999999999645, 91.00000000000000000, -8.000000000000000000 ) ) ;
#69411 = ORIENTED_EDGE ( 'NONE', *, *, #37450, .F. ) ;
#69412 = VECTOR ( 'NONE', #33406, 1000.000000000000000 ) ;
#69413 = CARTESIAN_POINT ( 'NONE',  ( 3.591859063236763294, 18.29030133659708568, -11.09922568453595026 ) ) ;
#69414 = CARTESIAN_POINT ( 'NONE',  ( 7.084665262690076126, 27.02201867748817676, -10.88017736071110164 ) ) ;
#69415 = CARTESIAN_POINT ( 'NONE',  ( 10.00000000000000000, 66.81368534415484817, -10.88017736071110342 ) ) ;
#69416 = EDGE_CURVE ( 'NONE', #51568, #22305, #95704, .T. ) ;
#69417 = ORIENTED_EDGE ( 'NONE', *, *, #87477, .F. ) ;
#69418 = ORIENTED_EDGE ( 'NONE', *, *, #17393, .T. ) ;
#69419 = CARTESIAN_POINT ( 'NONE',  ( 2.035157376598824452, 68.68868534415484817, 7.964842623401179544 ) ) ;
#69420 =( BOUNDED_CURVE ( )  B_SPLINE_CURVE ( 2, ( #3435, #18432, #48915, #40453, #64880, #41450, #71914, #49403, #26407 ),
 .UNSPECIFIED., .F., .T. ) 
 B_SPLINE_CURVE_WITH_KNOTS ( ( 3, 2, 2, 2, 3 ),
 ( 0.6177146600783226527, 0.6190476190476190688, 0.6250000000000000000, 0.6309523809523809312, 0.6322853399216773473 ),
 .UNSPECIFIED. ) 
 CURVE ( )  GEOMETRIC_REPRESENTATION_ITEM ( )  RATIONAL_B_SPLINE_CURVE ( ( 0.9881565478350733400, 0.9923695281211490915, 1.000000000000000000, 0.9659258262890683122, 1.000000000000000000, 0.9659258262890683122, 1.000000000000000000, 0.9923695281211490915, 0.9881565478350733400 ) ) 
 REPRESENTATION_ITEM ( '' )  );
#69421 = CARTESIAN_POINT ( 'NONE',  ( 12.63842701281683034, 52.46726448433413026, 9.846743663894596210 ) ) ;
#69422 = CARTESIAN_POINT ( 'NONE',  ( 12.63842701281683034, 37.46726448433411605, 9.846743663894596210 ) ) ;
#69423 = FILL_AREA_STYLE ('',( #31405 ) ) ;
#69424 = CARTESIAN_POINT ( 'NONE',  ( 2.791683348922237240, 30.38393115100078390, -7.208316651077763204 ) ) ;
#69425 = CARTESIAN_POINT ( 'NONE',  ( 0.2751277870542911397, 40.30223176428831522, 6.499999999999992006 ) ) ;
#69426 = DIRECTION ( 'NONE',  ( 1.000000000000000000, 0.000000000000000000, 0.000000000000000000 ) ) ;
#69428 = CARTESIAN_POINT ( 'NONE',  ( 20.10421743870887212, 50.60736173766202484, -6.337391062633415117 ) ) ;
#69427 = CARTESIAN_POINT ( 'NONE',  ( 12.63842701281683034, 12.46726448433411782, 9.846743663894596210 ) ) ;
#69429 = CARTESIAN_POINT ( 'NONE',  ( 21.92686044187656691, 44.95379003517448524, 3.195792623639537755 ) ) ;
#69431 = EDGE_LOOP ( 'NONE', ( #37801, #90196, #96948, #33622, #62382, #74077 ) ) ;
#69430 = CARTESIAN_POINT ( 'NONE',  ( 1.472469842513823179, 46.42559781766745175, 4.923371831947296329 ) ) ;
#69432 = CARTESIAN_POINT ( 'NONE',  ( -4.289191146912808207E-15, 3.868033628982651795, -11.25000000000000178 ) ) ;
#69433 = CARTESIAN_POINT ( 'NONE',  ( -2.816281873526471635, 18.91530133659708213, -3.434112377981056508 ) ) ;
#69434 = VECTOR ( 'NONE', #97281, 1000.000000000000000 ) ;
#69435 = EDGE_CURVE ( 'NONE', #1179, #86906, #58316, .T. ) ;
#69436 = CARTESIAN_POINT ( 'NONE',  ( 17.96484262340118221, 51.18868534415483396, -7.964842623401177768 ) ) ;
#69438 = ADVANCED_FACE ( 'NONE', ( #56235 ), #41729, .F. ) ;
#69437 = CARTESIAN_POINT ( 'NONE',  ( -2.266590686148945544, 26.38708216824730357, -7.082119434687050408 ) ) ;
#69439 = CARTESIAN_POINT ( 'NONE',  ( 7.361572987183170547, 2.050597817667451750, 9.846743663894590881 ) ) ;
#69440 = LINE ( 'NONE', #8441, #29628 ) ;
#69441 = CARTESIAN_POINT ( 'NONE',  ( -4.164238869374099039, 41.80374883491397497, 8.674139862899312516E-16 ) ) ;
#69442 = CARTESIAN_POINT ( 'NONE',  ( -2.266590686148945544, 56.38708216824731068, -7.082119434687050408 ) ) ;
#69443 = CARTESIAN_POINT ( 'NONE',  ( 10.00000000000000178, 18.05374883491396787, 14.16423886937410082 ) ) ;
#69445 = CARTESIAN_POINT ( 'NONE',  ( 5.418184704451237899, 0.000000000000000000, 0.6173241701923447566 ) ) ;
#69444 = CARTESIAN_POINT ( 'NONE',  ( 17.08211943468705840, 25.13708216824730357, -12.26659068614894466 ) ) ;
#69446 = CARTESIAN_POINT ( 'NONE',  ( 4.400664535130860422, -1.180071741297640253, -2.750000000000000000 ) ) ;
#69448 = CARTESIAN_POINT ( 'NONE',  ( 14.92337183194729988, 39.34226448433412315, -8.527530157486177487 ) ) ;
#69447 = CARTESIAN_POINT ( 'NONE',  ( 4.471066085529306733, -3.611416924331345868, 2.500000000000000000 ) ) ;
#69449 = ORIENTED_EDGE ( 'NONE', *, *, #64578, .F. ) ;
#69450 = CARTESIAN_POINT ( 'NONE',  ( 19.42250999205614193, 20.14701867748817321, 5.440088680355555262 ) ) ;
#69451 = CARTESIAN_POINT ( 'NONE',  ( 0.000000000000000000, 15.00000000000000000, 14.25000000000000000 ) ) ;
#69452 = CARTESIAN_POINT ( 'NONE',  ( -12.34086200392831678, -0.03417435944610275333, 7.124999999999885425 ) ) ;
#69453 = AXIS2_PLACEMENT_3D ( 'NONE', #59673, #195, #91660 ) ;
#69454 = CARTESIAN_POINT ( 'NONE',  ( 0.000000000000000000, 0.000000000000000000, 0.000000000000000000 ) ) ;
#69455 = CARTESIAN_POINT ( 'NONE',  ( 17.20831665107776587, 34.13393115100078745, -7.208316651077762316 ) ) ;
#69456 = CARTESIAN_POINT ( 'NONE',  ( -1.099225684535947600, 59.54030133659708923, 6.408140936763237150 ) ) ;
#69457 = CARTESIAN_POINT ( 'NONE',  ( 7.082119434687047743, -9.862917831752692877, -12.26659068614894821 ) ) ;
#69458 = CARTESIAN_POINT ( 'NONE',  ( 1.472469842513823179, 46.42559781766745175, 4.923371831947296329 ) ) ;
#69459 = CARTESIAN_POINT ( 'NONE',  ( 18.52753015748618282, 53.92559781766745175, -4.923371831947291888 ) ) ;
#69460 = CARTESIAN_POINT ( 'NONE',  ( 24.16423886937409904, 39.09541550158062506, 3.795296366450317205 ) ) ;
#69461 = ORIENTED_EDGE ( 'NONE', *, *, #66209, .F. ) ;
#69462 = CARTESIAN_POINT ( 'NONE',  ( 13.79529636645031943, 10.34541550158063394, -14.16423886937409904 ) ) ;
#69463 = LINE ( 'NONE', #31931, #66183 ) ;
#69465 = DIRECTION ( 'NONE',  ( 0.8070303256584298035, -0.5905099943842175847, 0.000000000000000000 ) ) ;
#69464 = DIRECTION ( 'NONE',  ( 0.000000000000000000, 0.000000000000000000, -1.000000000000000000 ) ) ;
#69466 = CARTESIAN_POINT ( 'NONE',  ( 4.559911319644449179, 8.897018677488173211, 9.422509992056141925 ) ) ;
#69467 = CARTESIAN_POINT ( 'NONE',  ( 19.38216949554541557, 7.248634669930421381, -9.382169495545420901 ) ) ;
#69468 = CARTESIAN_POINT ( 'NONE',  ( 17.82550711101916008, 78.51652315108729852, 4.000000000000000888 ) ) ;
#69469 = CARTESIAN_POINT ( 'NONE',  ( 19.42250999205614548, 65.98035201082151957, -5.440088680355545492 ) ) ;
#69470 = ADVANCED_FACE ( 'NONE', ( #35178 ), #34688, .T. ) ;
#69471 = CARTESIAN_POINT ( 'NONE',  ( 4.691428608706885051, -2.693193260553968127, -4.000000000000000000 ) ) ;
#69472 = CARTESIAN_POINT ( 'NONE',  ( -0.1503990784575403861, 14.24884699246888964, -6.262539305110056631 ) ) ;
#69473 = DIRECTION ( 'NONE',  ( 0.000000000000000000, 0.000000000000000000, -1.000000000000000000 ) ) ;
#69474 = CARTESIAN_POINT ( 'NONE',  ( 10.00000000000000000, 60.55374883491397497, -14.16423886937410082 ) ) ;
#69475 = DIRECTION ( 'NONE',  ( 0.000000000000000000, 1.000000000000000000, 0.000000000000000000 ) ) ;
#69476 = CARTESIAN_POINT ( 'NONE',  ( 20.88017736071110875, 20.77201867748816611, -2.915334737309920765 ) ) ;
#69477 = CARTESIAN_POINT ( 'NONE',  ( -0.8801773607110991993, 27.85535201082150181, -2.915334737309923874 ) ) ;
#69478 = MECHANICAL_DESIGN_GEOMETRIC_PRESENTATION_REPRESENTATION (  '', ( #56693 ), #93374 ) ;
#69479 = CARTESIAN_POINT ( 'NONE',  ( 18.52753015748617571, 58.09226448433411605, 4.923371831947298993 ) ) ;
#69480 = CARTESIAN_POINT ( 'NONE',  ( 14.92337183194729988, 49.34226448433411605, -8.527530157486177487 ) ) ;
#69481 = CARTESIAN_POINT ( 'NONE',  ( -44.73376486625691939, 105.7482819899384197, -5.219775981216077554 ) ) ;
#69482 = SURFACE_STYLE_USAGE ( .BOTH. , #17474 ) ;
#69483 = ORIENTED_EDGE ( 'NONE', *, *, #76326, .T. ) ;
#69484 = CARTESIAN_POINT ( 'NONE',  ( 0.5774900079438590739, 17.64701867748817321, -5.440088680355550821 ) ) ;
#69485 = CARTESIAN_POINT ( 'NONE',  ( 3.591859063236763294, 18.29030133659708568, -11.09922568453595026 ) ) ;
#69486 = SPHERICAL_SURFACE ( 'NONE', #51285, 0.2500000000000000000 ) ;
#69487 = B_SPLINE_CURVE_WITH_KNOTS ( 'NONE', 3,
 ( #61073, #62052, #68594, #69574 ),
 .UNSPECIFIED., .F., .F.,
 ( 4, 4 ),
 ( 5.143108168158485451E-18, 0.0003153927346766731811 ),
 .UNSPECIFIED. ) ;
#69488 = CARTESIAN_POINT ( 'NONE',  ( 7.361572987183170547, 67.05059781766746596, 9.846743663894590881 ) ) ;
#69489 = B_SPLINE_CURVE_WITH_KNOTS ( 'NONE', 3,
 ( #91357, #98898, #83862, #44863, #30852, #91858 ),
 .UNSPECIFIED., .F., .F.,
 ( 4, 2, 4 ),
 ( 3.409110551461945796E-05, 0.0004400426677364667862, 0.0008459942299583140873 ),
 .UNSPECIFIED. ) ;
#69490 = CARTESIAN_POINT ( 'NONE',  ( 10.00000000000000000, 51.81368534415484106, -10.88017736071110342 ) ) ;
#69491 = VECTOR ( 'NONE', #65844, 1000.000000000000000 ) ;
#69492 = CARTESIAN_POINT ( 'NONE',  ( 21.09922568453595559, 22.04030133659708923, -6.408140936763230044 ) ) ;
#69494 = DIRECTION ( 'NONE',  ( -0.5901017155107530776, -0.8073289077886820486, 0.000000000000000000 ) ) ;
#69493 = CARTESIAN_POINT ( 'NONE',  ( -0.8801773607110991993, 57.85535201082149825, -2.915334737309923874 ) ) ;
#69495 =( LENGTH_UNIT ( ) NAMED_UNIT ( * ) SI_UNIT ( .MILLI., .METRE. ) );
#69496 = CARTESIAN_POINT ( 'NONE',  ( 19.38216949554541557, 62.24863466993041072, -9.382169495545420901 ) ) ;
#69497 = EDGE_LOOP ( 'NONE', ( #92245, #2395, #78816, #65167 ) ) ;
#69498 = CARTESIAN_POINT ( 'NONE',  ( 0.5774900079438590739, 47.64701867748817676, -5.440088680355550821 ) ) ;
#69499 = DIRECTION ( 'NONE',  ( -0.000000000000000000, 1.000000000000000000, 0.000000000000000000 ) ) ;
#69500 = CARTESIAN_POINT ( 'NONE',  ( 4.559911319644449179, 43.89701867748816966, 9.422509992056141925 ) ) ;
#69501 = CARTESIAN_POINT ( 'NONE',  ( 0.6178305044545818747, 53.49863466993041072, -9.382169495545419124 ) ) ;
#69502 = CARTESIAN_POINT ( 'NONE',  ( 14.92337183194729988, 4.342264484334117824, -8.527530157486177487 ) ) ;
#69503 = FILL_AREA_STYLE ('',( #90508 ) ) ;
#69504 = CARTESIAN_POINT ( 'NONE',  ( 12.63842701281683922, 19.55059781766745175, -9.846743663894590881 ) ) ;
#69505 = CARTESIAN_POINT ( 'NONE',  ( 18.72515096720572458, 40.05509018479936145, 6.499999999999964473 ) ) ;
#69506 = CARTESIAN_POINT ( 'NONE',  ( -2.266590686148945544, 57.22041550158063217, 7.082119434687048631 ) ) ;
#69507 = ORIENTED_EDGE ( 'NONE', *, *, #17117, .F. ) ;
#69508 =( NAMED_UNIT ( * ) SI_UNIT ( $, .STERADIAN. ) SOLID_ANGLE_UNIT ( ) );
#69509 = CARTESIAN_POINT ( 'NONE',  ( 10.00000000000000178, 9.313685344154839285, 10.88017736071110342 ) ) ;
#69510 = CARTESIAN_POINT ( 'NONE',  ( -0.1049300847420697458, 7.216974130838790913, -6.336235997365749384 ) ) ;
#69511 = ORIENTED_EDGE ( 'NONE', *, *, #23968, .T. ) ;
#69512 = VERTEX_POINT ( 'NONE', #81184 ) ;
#69513 = CARTESIAN_POINT ( 'NONE',  ( 4.559911319644449179, 8.897018677488173211, 9.422509992056141925 ) ) ;
#69514 = CARTESIAN_POINT ( 'NONE',  ( 7.084665262690076126, 12.02201867748817321, -10.88017736071110164 ) ) ;
#69515 = CARTESIAN_POINT ( 'NONE',  ( 2.791683348922237240, 45.38393115100079456, -7.208316651077763204 ) ) ;
#69516 = PRESENTATION_LAYER_ASSIGNMENT (  '', '', ( #71083 ) ) ;
#69517 = CARTESIAN_POINT ( 'NONE',  ( 22.81628187352647785, 41.62363466993042493, 6.195893100308588602E-16 ) ) ;
#69518 = CARTESIAN_POINT ( 'NONE',  ( -13.34948392230381309, 0.04922511925147153578, 6.279918722514886475 ) ) ;
#69520 = CARTESIAN_POINT ( 'NONE',  ( 17.08211943468705840, 20.13708216824730357, -12.26659068614894466 ) ) ;
#69519 = CARTESIAN_POINT ( 'NONE',  ( -9.524127588832328684, 88.37770237764364367, -5.051303975189256334 ) ) ;
#69521 = CARTESIAN_POINT ( 'NONE',  ( 19.42250999205614548, 20.98035201082150891, -5.440088680355545492 ) ) ;
#69522 = CARTESIAN_POINT ( 'NONE',  ( 0.5774900079438607392, 8.480352010821505360, 5.440088680355550821 ) ) ;
#69523 = CARTESIAN_POINT ( 'NONE',  ( 12.63842701281683922, 44.55059781766745175, -9.846743663894590881 ) ) ;
#69524 = DIRECTION ( 'NONE',  ( 0.2503800040544526539, 0.000000000000000000, -0.9681476403781048568 ) ) ;
#69525 = CARTESIAN_POINT ( 'NONE',  ( 7.361572987183170547, 22.05059781766745530, 9.846743663894590881 ) ) ;
#69526 = CARTESIAN_POINT ( 'NONE',  ( 0.1532563361054082862, 1.217264484334117824, 2.638427012816831674 ) ) ;
#69527 = CARTESIAN_POINT ( 'NONE',  ( -9.382169495545413795, -40.25136533006956796, 9.382169495545428006 ) ) ;
#69528 = ORIENTED_EDGE ( 'NONE', *, *, #43388, .F. ) ;
#69529 = FILL_AREA_STYLE ('',( #17524 ) ) ;
#69530 = ORIENTED_EDGE ( 'NONE', *, *, #36721, .T. ) ;
#69531 = CARTESIAN_POINT ( 'NONE',  ( 18.52753015748617571, 58.09226448433411605, 4.923371831947298993 ) ) ;
#69533 = CARTESIAN_POINT ( 'NONE',  ( -0.8801773607111009756, 43.06368534415484106, 1.068504757029289695E-15 ) ) ;
#69532 = CARTESIAN_POINT ( 'NONE',  ( 12.91533473730992121, 29.52201867748817321, 10.88017736071110164 ) ) ;
#69535 = CARTESIAN_POINT ( 'NONE',  ( 22.81628187352647785, 26.62363466993042138, 6.195893100308588602E-16 ) ) ;
#69534 = CARTESIAN_POINT ( 'NONE',  ( 20.88017736071110164, 5.355352010821502695, 2.915334737309930979 ) ) ;
#69536 = CARTESIAN_POINT ( 'NONE',  ( -2.266590686148945544, 16.38708216824730357, -7.082119434687050408 ) ) ;
#69537 = EDGE_CURVE ( 'NONE', #42048, #80996, #20466, .T. ) ;
#69538 = TOROIDAL_SURFACE ( 'NONE', #26403, 14.49999999999999822, 0.5000000000000000000 ) ;
#69539 = CARTESIAN_POINT ( 'NONE',  ( -2.816281873526471635, 43.91530133659708923, -3.434112377981056508 ) ) ;
#69540 = VERTEX_POINT ( 'NONE', #87203 ) ;
#69541 = CARTESIAN_POINT ( 'NONE',  ( 19.84674366389459266, 43.30059781766744464, 2.638427012816836559 ) ) ;
#69542 = CARTESIAN_POINT ( 'NONE',  ( 10.00000000000000000, 26.81368534415484106, -10.88017736071110342 ) ) ;
#69543 = ORIENTED_EDGE ( 'NONE', *, *, #30955, .T. ) ;
#69544 = CARTESIAN_POINT ( 'NONE',  ( 15.44008868035555793, 16.39701867748817321, -9.422509992056140149 ) ) ;
#69545 = ORIENTED_EDGE ( 'NONE', *, *, #71634, .T. ) ;
#69546 = CARTESIAN_POINT ( 'NONE',  ( 12.91533473730992121, 59.52201867748816966, 10.88017736071110164 ) ) ;
#69547 = FILL_AREA_STYLE_COLOUR ( '', #67895 ) ;
#69548 = DIRECTION ( 'NONE',  ( -0.7253743710122820820, 0.000000000000000000, -0.6883545756937599069 ) ) ;
#69549 = AXIS2_PLACEMENT_3D ( 'NONE', #42505, #26998, #27978 ) ;
#69550 = CARTESIAN_POINT ( 'NONE',  ( 19.84674366389459266, 8.300597817667451750, 2.638427012816836559 ) ) ;
#69551 = EDGE_CURVE ( 'NONE', #38557, #29252, #71515, .T. ) ;
#69552 = CARTESIAN_POINT ( 'NONE',  ( 7.084665262690076126, 64.10535201082150536, 10.88017736071109987 ) ) ;
#69553 = DIRECTION ( 'NONE',  ( -0.000000000000000000, -1.000000000000000000, -0.000000000000000000 ) ) ;
#69554 =( GEOMETRIC_REPRESENTATION_CONTEXT ( 3 ) GLOBAL_UNCERTAINTY_ASSIGNED_CONTEXT ( ( #86464 ) ) GLOBAL_UNIT_ASSIGNED_CONTEXT ( ( #55175, #25209, #87148 ) ) REPRESENTATION_CONTEXT ( 'NONE', 'WORKASPACE' ) );
#69555 = CARTESIAN_POINT ( 'NONE',  ( 17.20831665107776587, 7.883931151000784787, 7.208316651077764980 ) ) ;
#69556 = EDGE_CURVE ( 'NONE', #56832, #51000, #4115, .T. ) ;
#69557 = CARTESIAN_POINT ( 'NONE',  ( 2.791683348922240793, 46.63393115100077324, 7.208316651077764092 ) ) ;
#69558 = VERTEX_POINT ( 'NONE', #89177 ) ;
#69559 = ORIENTED_EDGE ( 'NONE', *, *, #10014, .T. ) ;
#69560 = CARTESIAN_POINT ( 'NONE',  ( 6.880000000000009663, 40.99999999999999289, 6.250000000000000000 ) ) ;
#69562 = EDGE_CURVE ( 'NONE', #91132, #12692, #34155, .T. ) ;
#69561 = CARTESIAN_POINT ( 'NONE',  ( 0.2751277870542909176, 30.30223176428831167, 6.499999999999992006 ) ) ;
#69563 = CARTESIAN_POINT ( 'NONE',  ( 17.08211943468705130, 13.47041550158063572, 12.26659068614894998 ) ) ;
#69564 = CARTESIAN_POINT ( 'NONE',  ( 19.50000000000000355, 70.00000000000000000, 4.500000000000000888 ) ) ;
#69566 = CARTESIAN_POINT ( 'NONE',  ( 12.91533473730993009, 61.60535201082150536, -10.88017736071109987 ) ) ;
#69565 = CARTESIAN_POINT ( 'NONE',  ( 1.983216688680936812, 15.00000000000000000, -14.11131997956737649 ) ) ;
#69567 = CARTESIAN_POINT ( 'NONE',  ( 0.5774900079438590739, 27.64701867748817676, -5.440088680355550821 ) ) ;
#69568 = CARTESIAN_POINT ( 'NONE',  ( 0.1532563361054082862, 66.21726448433412315, 2.638427012816831674 ) ) ;
#69569 = VERTEX_POINT ( 'NONE', #44661 ) ;
#69570 = CARTESIAN_POINT ( 'NONE',  ( 14.92337183194729633, 7.675597817667451750, 8.527530157486181039 ) ) ;
#69571 = CARTESIAN_POINT ( 'NONE',  ( 0.1532563361054082862, 6.217264484334118713, 2.638427012816831674 ) ) ;
#69572 = CARTESIAN_POINT ( 'NONE',  ( 19.38216949554541202, 35.99863466993041072, 9.382169495545424454 ) ) ;
#69573 = CARTESIAN_POINT ( 'NONE',  ( 19.84674366389459266, 28.30059781766745886, 2.638427012816836559 ) ) ;
#69574 = CARTESIAN_POINT ( 'NONE',  ( -0.1503990784575328643, 69.92552686551195507, -6.262539305110068177 ) ) ;
#69575 = CARTESIAN_POINT ( 'NONE',  ( 16.40814093676323893, 15.79030133659708746, 11.09922568453595026 ) ) ;
#69576 = LINE ( 'NONE', #76573, #47350 ) ;
#69577 = AXIS2_PLACEMENT_3D ( 'NONE', #98260, #743, #31196 ) ;
#69578 = CARTESIAN_POINT ( 'NONE',  ( 1.472469842513823179, 5.592264484334118713, -4.923371831947296329 ) ) ;
#69579 = VERTEX_POINT ( 'NONE', #59164 ) ;
#69580 = CARTESIAN_POINT ( 'NONE',  ( 2.035157376598824452, 28.68868534415484106, 7.964842623401179544 ) ) ;
#69581 = CARTESIAN_POINT ( 'NONE',  ( 6.204703633549690345, 35.76208216824729647, -14.16423886937410259 ) ) ;
#69582 = CARTESIAN_POINT ( 'NONE',  ( 0.1532563361054100626, 35.80059781766745175, -2.638427012816831230 ) ) ;
#69583 = CARTESIAN_POINT ( 'NONE',  ( 0.5774900079438590739, 62.64701867748817676, -5.440088680355550821 ) ) ;
#69585 = FACE_OUTER_BOUND ( 'NONE', #51602, .T. ) ;
#69584 = CARTESIAN_POINT ( 'NONE',  ( -1.099225684535947600, 48.70696800326375353, -6.408140936763238038 ) ) ;
#69586 = CARTESIAN_POINT ( 'NONE',  ( 2.035157376598822676, 22.43868534415483396, -7.964842623401177768 ) ) ;
#69587 = ADVANCED_FACE ( 'NONE', ( #44157 ), #58705, .T. ) ;
#69588 = CYLINDRICAL_SURFACE ( 'NONE', #96558, 11.25000000000000178 ) ;
#69589 = CARTESIAN_POINT ( 'NONE',  ( -2.816281873526473856, 9.331968003263753531, 3.434112377981055619 ) ) ;
#69590 = CARTESIAN_POINT ( 'NONE',  ( 5.076628168052704559, 35.17559781766745175, -8.527530157486179263 ) ) ;
#69591 = CARTESIAN_POINT ( 'NONE',  ( 9.422509992056141925, 0.9803520108215141304, -5.440088680355554374 ) ) ;
#69592 = CARTESIAN_POINT ( 'NONE',  ( -2.816281873526473856, 49.12363466993042493, 9.499525473075851096E-16 ) ) ;
#69593 = LINE ( 'NONE', #86567, #38810 ) ;
#69595 = CARTESIAN_POINT ( 'NONE',  ( 0.6076426042653108039, 62.37576471608601025, -6.499999999999992006 ) ) ;
#69594 = CARTESIAN_POINT ( 'NONE',  ( 2.035157376598822676, 57.43868534415484106, -7.964842623401177768 ) ) ;
#69596 = CIRCLE ( 'NONE', #74349, 9.538348415311009632 ) ;
#69598 = EDGE_CURVE ( 'NONE', #36801, #55896, #74666, .T. ) ;
#69597 = CARTESIAN_POINT ( 'NONE',  ( 18.28836319691945889, 29.34492782695770785, 6.499999999999997335 ) ) ;
#69599 = CARTESIAN_POINT ( 'NONE',  ( 17.96484262340118221, 59.93868534415484106, 7.964842623401181321 ) ) ;
#69600 = CARTESIAN_POINT ( 'NONE',  ( 15.44008868035555793, 41.39701867748817676, -9.422509992056140149 ) ) ;
#69601 = CARTESIAN_POINT ( 'NONE',  ( 7.881609424766030436, 15.00000000000000711, -12.32025747423893591 ) ) ;
#69602 = DIRECTION ( 'NONE',  ( -0.000000000000000000, -0.000000000000000000, -1.000000000000000000 ) ) ;
#69603 = AXIS2_PLACEMENT_3D ( 'NONE', #66790, #52766, #59772 ) ;
#69604 = CARTESIAN_POINT ( 'NONE',  ( 7.361572987183169658, 44.96726448433412315, -9.846743663894592657 ) ) ;
#69606 = DIRECTION ( 'NONE',  ( 0.000000000000000000, 0.000000000000000000, 1.000000000000000000 ) ) ;
#69605 = CARTESIAN_POINT ( 'NONE',  ( 2.035157376598824452, 28.68868534415484106, 7.964842623401179544 ) ) ;
#69607 = CARTESIAN_POINT ( 'NONE',  ( 0.6178305044545838731, 29.74863466993042138, 9.382169495545420901 ) ) ;
#69608 = ORIENTED_EDGE ( 'NONE', *, *, #69793, .T. ) ;
#69609 = CARTESIAN_POINT ( 'NONE',  ( 20.88017736071110164, 40.35535201082150536, 2.915334737309930979 ) ) ;
#69610 = CARTESIAN_POINT ( 'NONE',  ( 6.565887622018943937, 5.165301336597086568, 12.81628187352647430 ) ) ;
#69611 = CARTESIAN_POINT ( 'NONE',  ( 19.42250999205614193, 10.14701867748816966, 5.440088680355555262 ) ) ;
#69612 = CARTESIAN_POINT ( 'NONE',  ( 12.91533473730992121, 39.52201867748817676, 10.88017736071110164 ) ) ;
#69613 = CARTESIAN_POINT ( 'NONE',  ( 13.79529636645030344, 33.26208216824730357, 14.16423886937410614 ) ) ;
#69614 = CARTESIAN_POINT ( 'NONE',  ( 19.84674366389459266, 28.71726448433411960, -2.638427012816827677 ) ) ;
#69615 = CARTESIAN_POINT ( 'NONE',  ( 20.88017736071110164, 55.35535201082149825, 2.915334737309930979 ) ) ;
#69616 = DIRECTION ( 'NONE',  ( -6.608470384673550777E-17, -1.000000000000000000, 0.000000000000000000 ) ) ;
#69617 = CARTESIAN_POINT ( 'NONE',  ( 22.26659068614894466, 8.887082168247300018, 7.082119434687054849 ) ) ;
#69618 = VECTOR ( 'NONE', #49867, 1000.000000000000114 ) ;
#69619 = SURFACE_STYLE_USAGE ( .BOTH. , #9112 ) ;
#69620 = CARTESIAN_POINT ( 'NONE',  ( 12.63842701281683922, 64.55059781766745175, -9.846743663894590881 ) ) ;
#69621 = AXIS2_PLACEMENT_3D ( 'NONE', #7175, #6186, #74675 ) ;
#69622 = ORIENTED_EDGE ( 'NONE', *, *, #17077, .F. ) ;
#69623 = ORIENTED_EDGE ( 'NONE', *, *, #36889, .T. ) ;
#69624 = CARTESIAN_POINT ( 'NONE',  ( 22.26659068614894466, 33.88708216824730357, 7.082119434687054849 ) ) ;
#69625 = CARTESIAN_POINT ( 'NONE',  ( -4.164238869374099927, 37.01208216824731068, 3.795296366450308767 ) ) ;
#69626 = CARTESIAN_POINT ( 'NONE',  ( 18.52753015748617571, 8.092264484334117824, 4.923371831947298993 ) ) ;
#69627 = B_SPLINE_CURVE_WITH_KNOTS ( 'NONE', 3,
 ( #59633, #36652, #22642, #53123 ),
 .UNSPECIFIED., .F., .F.,
 ( 4, 4 ),
 ( 7.152448122690996019E-18, 0.002562518741975553654 ),
 .UNSPECIFIED. ) ;
#69628 = CARTESIAN_POINT ( 'NONE',  ( 5.076628168052704559, 65.17559781766745175, -8.527530157486179263 ) ) ;
#69629 = CARTESIAN_POINT ( 'NONE',  ( -7.909656209098489654, -4.175824794483175673, 4.000000000000000000 ) ) ;
#69631 = CARTESIAN_POINT ( 'NONE',  ( 19.38216949554541202, 15.99863466993042138, 9.382169495545424454 ) ) ;
#69630 = CARTESIAN_POINT ( 'NONE',  ( 7.084665262690076126, 64.10535201082150536, 10.88017736071109987 ) ) ;
#69632 = CARTESIAN_POINT ( 'NONE',  ( 24.16423886937409904, 29.09541550158063572, 3.795296366450317205 ) ) ;
#69633 = CARTESIAN_POINT ( 'NONE',  ( 0.5774900079438590739, 32.64701867748816966, -5.440088680355550821 ) ) ;
#69634 = CARTESIAN_POINT ( 'NONE',  ( 7.084665262690076126, 27.02201867748817676, -10.88017736071110164 ) ) ;
#69635 = CARTESIAN_POINT ( 'NONE',  ( 13.55255535720595184, -0.03417435944610275333, -4.403492169842965431 ) ) ;
#69636 = CARTESIAN_POINT ( 'NONE',  ( 10.00000000000000178, 59.31368534415484106, 10.88017736071110342 ) ) ;
#69637 = CARTESIAN_POINT ( 'NONE',  ( -2.638427012816840111, -5.032735515665881287, -9.846743663894590881 ) ) ;
#69638 = EDGE_CURVE ( 'NONE', #19346, #55759, #65115, .T. ) ;
#69639 = ORIENTED_EDGE ( 'NONE', *, *, #86151, .T. ) ;
#69640 = DIRECTION ( 'NONE',  ( 1.000000000000000000, 0.000000000000000000, 0.000000000000000000 ) ) ;
#69641 = VERTEX_POINT ( 'NONE', #22171 ) ;
#69642 = DIRECTION ( 'NONE',  ( 0.000000000000000000, 0.000000000000000000, -1.000000000000000000 ) ) ;
#69643 = ORIENTED_EDGE ( 'NONE', *, *, #95980, .F. ) ;
#69644 = CARTESIAN_POINT ( 'NONE',  ( 24.16423886937410614, 9.303748834913967869, 8.672049930838204340E-16 ) ) ;
#69646 = CARTESIAN_POINT ( 'NONE',  ( -0.8801773607111009756, 3.063685344154838397, 1.068504757029289695E-15 ) ) ;
#69645 = CARTESIAN_POINT ( 'NONE',  ( 17.08211943468705840, 60.13708216824729647, -12.26659068614894466 ) ) ;
#69648 = CARTESIAN_POINT ( 'NONE',  ( 0.1532563361054082862, 66.21726448433413736, 2.638427012816831674 ) ) ;
#69647 = CARTESIAN_POINT ( 'NONE',  ( 12.63842701281683034, 32.46726448433412315, 9.846743663894596210 ) ) ;
#69649 = CARTESIAN_POINT ( 'NONE',  ( 20.24186590665277663, 59.73410085661204505, 6.114288769123047196 ) ) ;
#69650 = EDGE_CURVE ( 'NONE', #30382, #93734, #20690, .T. ) ;
#69651 = CARTESIAN_POINT ( 'NONE',  ( 5.129999999999995453, 43.00000000000000711, 6.500000000000000888 ) ) ;
#69652 = CARTESIAN_POINT ( 'NONE',  ( -2.816281873526473856, 9.123634669930421381, 9.499525473075851096E-16 ) ) ;
#69653 = VERTEX_POINT ( 'NONE', #58678 ) ;
#69654 = CARTESIAN_POINT ( 'NONE',  ( 6.204703633549690345, 40.76208216824731778, -14.16423886937410259 ) ) ;
#69655 = CARTESIAN_POINT ( 'NONE',  ( 17.08211943468705840, 45.13708216824730357, -12.26659068614894466 ) ) ;
#69656 = ORIENTED_EDGE ( 'NONE', *, *, #54907, .T. ) ;
#69657 = CARTESIAN_POINT ( 'NONE',  ( 19.42250999205614193, 15.14701867748817143, 5.440088680355555262 ) ) ;
#69658 = CARTESIAN_POINT ( 'NONE',  ( 6.565887622018943937, 53.08196800326374643, -12.81628187352647608 ) ) ;
#69659 = CARTESIAN_POINT ( 'NONE',  ( 19.42250999205614548, 30.98035201082150536, -5.440088680355545492 ) ) ;
#69660 = CARTESIAN_POINT ( 'NONE',  ( 10.00000000000000000, 44.75893115100078745, -9.846743663894594434 ) ) ;
#69661 = CARTESIAN_POINT ( 'NONE',  ( 20.88017736071110164, 30.35535201082151247, 2.915334737309930979 ) ) ;
#69662 = CARTESIAN_POINT ( 'NONE',  ( -3.521020805652878671, -6.414291667507525219, 2.500000000000000444 ) ) ;
#69663 = CARTESIAN_POINT ( 'NONE',  ( 5.076628168052704559, 60.17559781766745175, -8.527530157486179263 ) ) ;
#69664 = CARTESIAN_POINT ( 'NONE',  ( 20.88017736071110519, 65.56368534415483396, 2.639326808657452039E-16 ) ) ;
#69665 = CARTESIAN_POINT ( 'NONE',  ( 4.559911319644449179, 22.23035201082150536, -9.422509992056141925 ) ) ;
#69666 =( GEOMETRIC_REPRESENTATION_CONTEXT ( 3 ) GLOBAL_UNCERTAINTY_ASSIGNED_CONTEXT ( ( #27289 ) ) GLOBAL_UNIT_ASSIGNED_CONTEXT ( ( #80642, #4160, #74106 ) ) REPRESENTATION_CONTEXT ( 'NONE', 'WORKASPACE' ) );
#69667 = CARTESIAN_POINT ( 'NONE',  ( -3.750000000000000000, 37.00000000000000000, -3.750000000000000000 ) ) ;
#69668 = ADVANCED_FACE ( 'NONE', ( #15171 ), #4491, .T. ) ;
#69669 = DIRECTION ( 'NONE',  ( -0.000000000000000000, -1.000000000000000000, -0.000000000000000000 ) ) ;
#69670 = CARTESIAN_POINT ( 'NONE',  ( -3.271890209819976025, -0.8418601081563239497, 2.500000000000000888 ) ) ;
#69671 = ORIENTED_EDGE ( 'NONE', *, *, #76299, .F. ) ;
#69672 = CARTESIAN_POINT ( 'NONE',  ( 8.955817848464572961, -3.107653060326661887, 4.000000000000000000 ) ) ;
#69673 = CARTESIAN_POINT ( 'NONE',  ( 10.00000000000000000, 34.75893115100078745, -9.846743663894594434 ) ) ;
#69675 = EDGE_CURVE ( 'NONE', #30783, #39614, #48188, .T. ) ;
#69674 = CARTESIAN_POINT ( 'NONE',  ( -23.44000000000001194, 92.00000000000000000, 9.500000000000000000 ) ) ;
#69676 = CARTESIAN_POINT ( 'NONE',  ( 9.779999999999988702, 27.00436609429084811, 3.000000000000000000 ) ) ;
#69677 = CARTESIAN_POINT ( 'NONE',  ( 1.350000000000004086, 98.49999999999998579, -8.525133428036873795 ) ) ;
#69678 = CARTESIAN_POINT ( 'NONE',  ( -0.1503990784575328643, 70.00000000000000000, -6.262539305110068177 ) ) ;
#69679 = LINE ( 'NONE', #83204, #48987 ) ;
#69680 = CARTESIAN_POINT ( 'NONE',  ( 0.1532563361054100626, 60.80059781766744464, -2.638427012816831230 ) ) ;
#69681 = CARTESIAN_POINT ( 'NONE',  ( -4.164238869374099927, 47.01208216824729647, 3.795296366450308767 ) ) ;
#69682 = CARTESIAN_POINT ( 'NONE',  ( 19.84674366389459266, 63.71726448433412315, -2.638427012816827677 ) ) ;
#69683 = CARTESIAN_POINT ( 'NONE',  ( 20.10384461210892582, 41.74302437010792488, 6.337995344473752901 ) ) ;
#69684 = CARTESIAN_POINT ( 'NONE',  ( 17.20831665107776587, 12.88393115100078390, 7.208316651077764980 ) ) ;
#69685 = CARTESIAN_POINT ( 'NONE',  ( 21.09922568453594849, 56.20696800326375353, 6.408140936763242479 ) ) ;
#69686 = CARTESIAN_POINT ( 'NONE',  ( 10.00000000000000000, 59.75893115100078745, -9.846743663894594434 ) ) ;
#69687 = CARTESIAN_POINT ( 'NONE',  ( 12.91533473730992121, 59.52201867748816966, 10.88017736071110164 ) ) ;
#69688 = CARTESIAN_POINT ( 'NONE',  ( 6.934003561272774618, -73.15726776830514666, -2.750000000000000444 ) ) ;
#69689 = AXIS2_PLACEMENT_3D ( 'NONE', #53778, #7306, #29778 ) ;
#69690 = VERTEX_POINT ( 'NONE', #31125 ) ;
#69691 = CARTESIAN_POINT ( 'NONE',  ( 19.42250999205614548, 55.98035201082150536, -5.440088680355545492 ) ) ;
#69692 = EDGE_CURVE ( 'NONE', #84535, #71042, #92139, .T. ) ;
#69693 = AXIS2_PLACEMENT_3D ( 'NONE', #96611, #80609, #96112 ) ;
#69694 = ORIENTED_EDGE ( 'NONE', *, *, #33950, .F. ) ;
#69695 = CARTESIAN_POINT ( 'NONE',  ( -9.898881779040801021, 0.000000000000000000, 10.25059215482569641 ) ) ;
#69696 = CARTESIAN_POINT ( 'NONE',  ( 12.91533473730992121, 34.52201867748817676, 10.88017736071110164 ) ) ;
#69698 = CARTESIAN_POINT ( 'NONE',  ( 20.88017736071110164, 55.35535201082149825, 2.915334737309930979 ) ) ;
#69697 = CARTESIAN_POINT ( 'NONE',  ( 21.09922568453595559, 7.040301336597086568, -6.408140936763230044 ) ) ;
#69699 = DIRECTION ( 'NONE',  ( -0.000000000000000000, -1.000000000000000000, -0.000000000000000000 ) ) ;
#69700 = DIRECTION ( 'NONE',  ( -0.000000000000000000, 0.000000000000000000, 1.000000000000000000 ) ) ;
#69701 = CARTESIAN_POINT ( 'NONE',  ( 8.731067818237038480, 5.787123368507815613, -8.731067818237040257 ) ) ;
#69703 = DIRECTION ( 'NONE',  ( -0.000000000000000000, -1.000000000000000000, -0.000000000000000000 ) ) ;
#69702 = CARTESIAN_POINT ( 'NONE',  ( 15.44008868035555793, 41.39701867748817676, -9.422509992056140149 ) ) ;
#69704 = CARTESIAN_POINT ( 'NONE',  ( 14.92337183194729633, 32.67559781766745175, 8.527530157486181039 ) ) ;
#69705 = CARTESIAN_POINT ( 'NONE',  ( 17.20831665107776587, 4.133931151000785675, -7.208316651077762316 ) ) ;
#69706 = CARTESIAN_POINT ( 'NONE',  ( -14.16423886937410437, 26.59541550158064283, -3.795296366450299885 ) ) ;
#69707 = CARTESIAN_POINT ( 'NONE',  ( -2.816281873526473856, 14.33196800326375531, 3.434112377981055619 ) ) ;
#69709 = PLANE ( 'NONE',  #84045 ) ;
#69708 = CARTESIAN_POINT ( 'NONE',  ( 12.91533473730993009, 16.60535201082150891, -10.88017736071109987 ) ) ;
#69710 = VECTOR ( 'NONE', #57320, 999.9999999999998863 ) ;
#69711 = PRESENTATION_STYLE_ASSIGNMENT (( #47692 ) ) ;
#69712 = CARTESIAN_POINT ( 'NONE',  ( -4.164238869374099927, 22.01208216824730357, 3.795296366450308767 ) ) ;
#69713 = CIRCLE ( 'NONE', #68149, 11.92686044187656513 ) ;
#69714 = CARTESIAN_POINT ( 'NONE',  ( 24.16423886937410614, 64.30374883491396076, 8.672049930838204340E-16 ) ) ;
#69715 = CARTESIAN_POINT ( 'NONE',  ( 7.361572987183169658, 34.96726448433411605, -9.846743663894592657 ) ) ;
#69716 = VECTOR ( 'NONE', #75942, 1000.000000000000000 ) ;
#69717 = CARTESIAN_POINT ( 'NONE',  ( 18.52753015748618282, 23.92559781766745530, -4.923371831947291888 ) ) ;
#69718 = CARTESIAN_POINT ( 'NONE',  ( -0.8801773607110991993, 17.85535201082150536, -2.915334737309923874 ) ) ;
#69719 = ORIENTED_EDGE ( 'NONE', *, *, #67640, .F. ) ;
#69720 = CARTESIAN_POINT ( 'NONE',  ( 0.1532563361054083140, 36.00893115100078745, 1.131784320476157264E-15 ) ) ;
#69721 = CARTESIAN_POINT ( 'NONE',  ( 20.88017736071110875, 30.77201867748816966, -2.915334737309920765 ) ) ;
#69722 = CARTESIAN_POINT ( 'NONE',  ( 1.472469842513823179, 65.59226448433412315, -4.923371831947296329 ) ) ;
#69724 = CARTESIAN_POINT ( 'NONE',  ( 0.000000000000000000, 0.5000000000000004441, 0.000000000000000000 ) ) ;
#69723 = CARTESIAN_POINT ( 'NONE',  ( 17.08211943468705840, 10.13708216824730179, -12.26659068614894466 ) ) ;
#69725 = CARTESIAN_POINT ( 'NONE',  ( 1.274849032794278747, 42.55509018479936856, -6.499999999999960032 ) ) ;
#69726 = CARTESIAN_POINT ( 'NONE',  ( 2.791683348922237240, 15.38393115100078212, -7.208316651077763204 ) ) ;
#69727 = CARTESIAN_POINT ( 'NONE',  ( 13.43411237798106583, 32.66530133659708213, -12.81628187352647252 ) ) ;
#69728 = CARTESIAN_POINT ( 'NONE',  ( 2.791683348922237240, 60.38393115100078745, -7.208316651077763204 ) ) ;
#69729 = ORIENTED_EDGE ( 'NONE', *, *, #57768, .F. ) ;
#69730 = CARTESIAN_POINT ( 'NONE',  ( 17.20831665107776587, 17.88393115100078745, 7.208316651077764980 ) ) ;
#69731 = B_SPLINE_CURVE_WITH_KNOTS ( 'NONE', 3,
 ( #86452, #61465, #39479, #45990, #92945, #91972 ),
 .UNSPECIFIED., .F., .F.,
 ( 4, 2, 4 ),
 ( 0.0002800098398849580313, 0.0006862151655504416300, 0.001092420491215925337 ),
 .UNSPECIFIED. ) ;
#69732 = CARTESIAN_POINT ( 'NONE',  ( 8.862914611804004750, -7.247476534019402727, -4.000000000000000000 ) ) ;
#69733 = CARTESIAN_POINT ( 'NONE',  ( -46.53118954259812057, 102.2886238795329490, -7.275463144368016444 ) ) ;
#69734 = CARTESIAN_POINT ( 'NONE',  ( 13.79529636645031943, 60.34541550158063927, -14.16423886937409904 ) ) ;
#69735 = CARTESIAN_POINT ( 'NONE',  ( 19.42250999205614548, 50.98035201082151247, -5.440088680355545492 ) ) ;
#69736 = CARTESIAN_POINT ( 'NONE',  ( -4.164238869374099927, 2.012082168247300906, 3.795296366450308767 ) ) ;
#69737 = CARTESIAN_POINT ( 'NONE',  ( -0.8801773607111008646, 53.27201867748816966, 2.915334737309923430 ) ) ;
#69738 = CARTESIAN_POINT ( 'NONE',  ( 0.1532563361054082862, 31.21726448433412315, 2.638427012816831674 ) ) ;
#69739 = CARTESIAN_POINT ( 'NONE',  ( 17.96484262340118221, 16.18868534415483396, -7.964842623401177768 ) ) ;
#69740 = FILL_AREA_STYLE ('',( #38753 ) ) ;
#69741 = CARTESIAN_POINT ( 'NONE',  ( 0.1532563361054100626, 50.80059781766745175, -2.638427012816831230 ) ) ;
#69742 = AXIS2_PLACEMENT_3D ( 'NONE', #42197, #5673, #66148 ) ;
#69743 = CARTESIAN_POINT ( 'NONE',  ( 2.035157376598824452, 53.68868534415484817, 7.964842623401179544 ) ) ;
#69744 = CARTESIAN_POINT ( 'NONE',  ( 19.84674366389459266, 3.300597817667451750, 2.638427012816836559 ) ) ;
#69745 = AXIS2_PLACEMENT_3D ( 'NONE', #27092, #19605, #12591 ) ;
#69746 = ORIENTED_EDGE ( 'NONE', *, *, #48337, .T. ) ;
#69747 = ORIENTED_EDGE ( 'NONE', *, *, #42056, .T. ) ;
#69748 = CARTESIAN_POINT ( 'NONE',  ( -0.1503990784575294781, 68.10158574516643171, 6.262539305110072618 ) ) ;
#69749 = CARTESIAN_POINT ( 'NONE',  ( -8.000000000000000000, 1.019547802438466100, 3.750000000000000000 ) ) ;
#69750 = CARTESIAN_POINT ( 'NONE',  ( 7.361572987183170547, 47.05059781766745175, 9.846743663894590881 ) ) ;
#69751 = CARTESIAN_POINT ( 'NONE',  ( 18.52753015748618282, 18.92559781766745175, -4.923371831947291888 ) ) ;
#69752 = CARTESIAN_POINT ( 'NONE',  ( -2.816281873526473856, 59.33196800326374643, 3.434112377981055619 ) ) ;
#69754 = CARTESIAN_POINT ( 'NONE',  ( 12.63842701281683922, 54.55059781766745175, -9.846743663894590881 ) ) ;
#69753 = CARTESIAN_POINT ( 'NONE',  ( -0.8801773607110991993, 22.85535201082150181, -2.915334737309923874 ) ) ;
#69755 = CARTESIAN_POINT ( 'NONE',  ( 2.917880565312948704, 32.63708216824730357, 12.26659068614894643 ) ) ;
#69756 = AXIS2_PLACEMENT_3D ( 'NONE', #26920, #79440, #41948 ) ;
#69757 = CARTESIAN_POINT ( 'NONE',  ( 2.917880565312948704, 62.63708216824730357, 12.26659068614894643 ) ) ;
#69758 = CARTESIAN_POINT ( 'NONE',  ( 7.361572987183170547, 62.05059781766745886, 9.846743663894590881 ) ) ;
#69759 = CARTESIAN_POINT ( 'NONE',  ( -7.750000000000000000, 80.07179676972448590, 4.250000000000000000 ) ) ;
#69760 = CARTESIAN_POINT ( 'NONE',  ( -0.8801773607111009756, 53.06368534415484106, 1.068504757029289695E-15 ) ) ;
#69761 = CARTESIAN_POINT ( 'NONE',  ( 18.52753015748617571, 18.09226448433411960, 4.923371831947298993 ) ) ;
#69762 = DIRECTION ( 'NONE',  ( -0.8320502943378436100, 0.5547001962252291474, -0.000000000000000000 ) ) ;
#69763 = VERTEX_POINT ( 'NONE', #55105 ) ;
#69764 = CARTESIAN_POINT ( 'NONE',  ( -1.326261724322778557, 0.2301504087166175161, -14.88164196614427226 ) ) ;
#69765 = ORIENTED_EDGE ( 'NONE', *, *, #74212, .T. ) ;
#69766 = CARTESIAN_POINT ( 'NONE',  ( 12.63842701281683922, 9.550597817667449974, -9.846743663894590881 ) ) ;
#69767 = VERTEX_POINT ( 'NONE', #16140 ) ;
#69768 = CARTESIAN_POINT ( 'NONE',  ( 22.26659068614894466, 23.88708216824730357, 7.082119434687054849 ) ) ;
#69769 = CARTESIAN_POINT ( 'NONE',  ( 18.52753015748618282, 23.92559781766745530, -4.923371831947291888 ) ) ;
#69770 = CARTESIAN_POINT ( 'NONE',  ( 17.96484262340118221, 44.93868534415483396, 7.964842623401181321 ) ) ;
#69771 = ADVANCED_FACE ( 'NONE', ( #1653 ), #93109, .T. ) ;
#69772 = SURFACE_SIDE_STYLE ('',( #84771 ) ) ;
#69773 = VERTEX_POINT ( 'NONE', #47113 ) ;
#69774 = CARTESIAN_POINT ( 'NONE',  ( -0.8801773607110991993, 37.85535201082151247, -2.915334737309923874 ) ) ;
#69775 = CARTESIAN_POINT ( 'NONE',  ( -0.1503990784575279516, 43.10158574516643171, 6.262539305110076171 ) ) ;
#69776 = EDGE_CURVE ( 'NONE', #86034, #5496, #62110, .T. ) ;
#69777 = AXIS2_PLACEMENT_3D ( 'NONE', #75201, #45697, #22713 ) ;
#69778 = ORIENTED_EDGE ( 'NONE', *, *, #8812, .F. ) ;
#69779 = CARTESIAN_POINT ( 'NONE',  ( 17.96484262340118221, 46.18868534415484106, -7.964842623401177768 ) ) ;
#69780 = CARTESIAN_POINT ( 'NONE',  ( 6.204703633549690345, 12.84541550158063572, 14.16423886937410082 ) ) ;
#69781 = ORIENTED_EDGE ( 'NONE', *, *, #1621, .T. ) ;
#69782 = CARTESIAN_POINT ( 'NONE',  ( -1.099225684535947600, 19.54030133659708568, 6.408140936763237150 ) ) ;
#69783 = FILL_AREA_STYLE ('',( #54755 ) ) ;
#69784 = CARTESIAN_POINT ( 'NONE',  ( 0.1532563361054082862, 16.21726448433411960, 2.638427012816831674 ) ) ;
#69785 = LINE ( 'NONE', #67818, #32227 ) ;
#69786 =( NAMED_UNIT ( * ) PLANE_ANGLE_UNIT ( ) SI_UNIT ( $, .RADIAN. ) );
#69787 = CARTESIAN_POINT ( 'NONE',  ( 1.472469842513823179, 20.59226448433411960, -4.923371831947296329 ) ) ;
#69788 = CARTESIAN_POINT ( 'NONE',  ( -0.8801773607111008646, 33.27201867748817676, 2.915334737309923430 ) ) ;
#69789 = MECHANICAL_DESIGN_GEOMETRIC_PRESENTATION_REPRESENTATION (  '', ( #36227 ), #84138 ) ;
#69790 = CIRCLE ( 'NONE', #66573, 0.2500000000000002220 ) ;
#69791 = ORIENTED_EDGE ( 'NONE', *, *, #26636, .F. ) ;
#69793 = EDGE_CURVE ( 'NONE', #94935, #4865, #33175, .T. ) ;
#69792 = AXIS2_PLACEMENT_3D ( 'NONE', #20508, #5016, #67486 ) ;
#69794 = DIRECTION ( 'NONE',  ( 0.000000000000000000, 1.000000000000000000, 0.000000000000000000 ) ) ;
#69795 = CARTESIAN_POINT ( 'NONE',  ( 15.44008868035555260, 54.73035201082150536, 9.422509992056143702 ) ) ;
#69796 = LINE ( 'NONE', #29802, #69109 ) ;
#69797 = CARTESIAN_POINT ( 'NONE',  ( 19.38216949554541557, 62.24863466993041072, -9.382169495545420901 ) ) ;
#69798 = CARTESIAN_POINT ( 'NONE',  ( 20.88017736071110164, 60.35535201082151957, 2.915334737309930979 ) ) ;
#69799 = EDGE_CURVE ( 'NONE', #23173, #87694, #46148, .T. ) ;
#69800 = CARTESIAN_POINT ( 'NONE',  ( 19.38216949554541557, 17.24863466993041783, -9.382169495545420901 ) ) ;
#69801 = CARTESIAN_POINT ( 'NONE',  ( 12.00809552683956305, 0.3639308727179669245, 8.989195838243638548 ) ) ;
#69802 = CARTESIAN_POINT ( 'NONE',  ( 0.1532563361054100626, 30.80059781766744820, -2.638427012816831230 ) ) ;
#69803 = CARTESIAN_POINT ( 'NONE',  ( 16.40814093676324603, 57.45696800326375353, -11.09922568453594671 ) ) ;
#69804 = CARTESIAN_POINT ( 'NONE',  ( 4.573266373291863474, -6.401889604903887587, -3.750000000000001776 ) ) ;
#69805 = CARTESIAN_POINT ( 'NONE',  ( 14.92337183194729988, 19.34226448433411960, -8.527530157486177487 ) ) ;
#69806 = CARTESIAN_POINT ( 'NONE',  ( 22.81628187352647785, 21.41530133659708923, 3.434112377981063169 ) ) ;
#69809 = STYLED_ITEM ( 'NONE', ( #46834 ), #299 ) ;
#69808 = LINE ( 'NONE', #15824, #94462 ) ;
#69807 =( NAMED_UNIT ( * ) PLANE_ANGLE_UNIT ( ) SI_UNIT ( $, .RADIAN. ) );
#69810 = CARTESIAN_POINT ( 'NONE',  ( 10.00000000000000178, 44.31368534415484106, 10.88017736071110342 ) ) ;
#69811 = CARTESIAN_POINT ( 'NONE',  ( 12.63842701281683922, 64.55059781766745175, -9.846743663894590881 ) ) ;
#69812 = DIRECTION ( 'NONE',  ( 0.000000000000000000, 0.000000000000000000, 1.000000000000000000 ) ) ;
#69813 = CARTESIAN_POINT ( 'NONE',  ( 12.63842701281683034, 17.46726448433411250, 9.846743663894596210 ) ) ;
#69814 = CARTESIAN_POINT ( 'NONE',  ( -0.8801773607111009756, 8.063685344154837509, 1.068504757029289695E-15 ) ) ;
#69815 = CARTESIAN_POINT ( 'NONE',  ( 3.591859063236761518, 9.956968003263753531, 11.09922568453594849 ) ) ;
#69816 = CARTESIAN_POINT ( 'NONE',  ( 15.44008868035555260, 4.730352010821504471, 9.422509992056143702 ) ) ;
#69817 = CARTESIAN_POINT ( 'NONE',  ( -10.89045396206093663, 89.68015320059714668, 6.284968870998880242 ) ) ;
#69818 = CARTESIAN_POINT ( 'NONE',  ( 19.42250999205614548, 25.98035201082150891, -5.440088680355545492 ) ) ;
#69819 = PRESENTATION_LAYER_ASSIGNMENT (  '', '', ( #66596 ) ) ;
#69820 = ORIENTED_EDGE ( 'NONE', *, *, #52075, .F. ) ;
#69821 = CARTESIAN_POINT ( 'NONE',  ( 7.771322705631503069, 15.00000000000000000, -12.24159072199917375 ) ) ;
#69823 = CARTESIAN_POINT ( 'NONE',  ( 20.88017736071110519, 15.56368534415483751, 2.639326808657452039E-16 ) ) ;
#69822 = CARTESIAN_POINT ( 'NONE',  ( 19.84674366389459266, 28.71726448433411960, -2.638427012816827677 ) ) ;
#69824 = CYLINDRICAL_SURFACE ( 'NONE', #24787, 0.2500000000000002220 ) ;
#69825 = CARTESIAN_POINT ( 'NONE',  ( 15.44008868035555793, 26.39701867748817321, -9.422509992056140149 ) ) ;
#69827 = SURFACE_STYLE_FILL_AREA ( #18295 ) ;
#69826 = CARTESIAN_POINT ( 'NONE',  ( 13.79529636645031943, 60.34541550158063927, -14.16423886937409904 ) ) ;
#69828 = CARTESIAN_POINT ( 'NONE',  ( 10.00000000000000178, 2.258931151000784787, 9.846743663894594434 ) ) ;
#69829 = EDGE_CURVE ( 'NONE', #83990, #26974, #45235, .T. ) ;
#69830 = CARTESIAN_POINT ( 'NONE',  ( 18.52753015748618282, 38.92559781766745175, -4.923371831947291888 ) ) ;
#69831 = DIRECTION ( 'NONE',  ( 0.000000000000000000, 1.000000000000000000, -0.000000000000000000 ) ) ;
#69832 = EDGE_CURVE ( 'NONE', #90632, #90778, #181, .T. ) ;
#69833 = CARTESIAN_POINT ( 'NONE',  ( 7.361572987183170547, 62.05059781766745886, 9.846743663894590881 ) ) ;
#69834 = DIRECTION ( 'NONE',  ( 0.000000000000000000, 0.000000000000000000, 1.000000000000000000 ) ) ;
#69835 = CARTESIAN_POINT ( 'NONE',  ( 2.917880565312950480, 25.97041550158063572, -12.26659068614894821 ) ) ;
#69836 = CARTESIAN_POINT ( 'NONE',  ( 1.472469842513823179, 36.42559781766745175, 4.923371831947296329 ) ) ;
#69837 = CARTESIAN_POINT ( 'NONE',  ( -5.171435456984210255, 0.000000000000000000, -1.730338099014048669 ) ) ;
#69838 = ORIENTED_EDGE ( 'NONE', *, *, #20955, .F. ) ;
#69839 = CARTESIAN_POINT ( 'NONE',  ( 17.08211943468705840, 50.13708216824730357, -12.26659068614894466 ) ) ;
#69840 = CARTESIAN_POINT ( 'NONE',  ( 0.1532563361054082862, 21.21726448433412315, 2.638427012816831674 ) ) ;
#69842 = CARTESIAN_POINT ( 'NONE',  ( 13.07964015051220485, 14.76930270348881180, 7.222261988160834534 ) ) ;
#69841 = PRESENTATION_STYLE_ASSIGNMENT (( #7378 ) ) ;
#69843 = CARTESIAN_POINT ( 'NONE',  ( 19.42250999205614548, 50.98035201082151247, -5.440088680355545492 ) ) ;
#69844 = CARTESIAN_POINT ( 'NONE',  ( 6.565887622018943937, 58.08196800326376064, -12.81628187352647608 ) ) ;
#69845 = CARTESIAN_POINT ( 'NONE',  ( 15.44008868035555793, 11.39701867748817143, -9.422509992056140149 ) ) ;
#69846 = CARTESIAN_POINT ( 'NONE',  ( 19.38216949554541557, 52.24863466993041072, -9.382169495545420901 ) ) ;
#69847 = CARTESIAN_POINT ( 'NONE',  ( -2.816281873526473856, -0.6680319967362464695, 3.434112377981055619 ) ) ;
#69848 = CARTESIAN_POINT ( 'NONE',  ( 0.1532563361054083140, 1.008931151000784787, 1.131784320476157264E-15 ) ) ;
#69849 = VERTEX_POINT ( 'NONE', #77614 ) ;
#69850 = CARTESIAN_POINT ( 'NONE',  ( -2.888614318722539487, 15.00000000000000888, 14.33855829812819849 ) ) ;
#69851 = FACE_OUTER_BOUND ( 'NONE', #72027, .T. ) ;
#69852 = CARTESIAN_POINT ( 'NONE',  ( -0.3689425029237881626, 57.42874883491397497, 10.36894250292379027 ) ) ;
#69853 = CARTESIAN_POINT ( 'NONE',  ( 17.08211943468705130, 13.47041550158063572, 12.26659068614894998 ) ) ;
#69854 = CARTESIAN_POINT ( 'NONE',  ( 15.44008868035555260, 14.73035201082150536, 9.422509992056143702 ) ) ;
#69855 = AXIS2_PLACEMENT_3D ( 'NONE', #51592, #82076, #97610 ) ;
#69856 = CARTESIAN_POINT ( 'NONE',  ( 7.084665262690076126, 34.10535201082151247, 10.88017736071109987 ) ) ;
#69857 = LINE ( 'NONE', #1379, #23980 ) ;
#69858 = DIRECTION ( 'NONE',  ( 1.000000000000000000, 0.000000000000000000, 0.000000000000000000 ) ) ;
#69859 = CARTESIAN_POINT ( 'NONE',  ( 7.361572987183169658, -0.03273551566588185635, -9.846743663894592657 ) ) ;
#69860 = DIRECTION ( 'NONE',  ( -0.000000000000000000, -1.000000000000000000, -0.000000000000000000 ) ) ;
#69861 = CARTESIAN_POINT ( 'NONE',  ( 5.076628168052703671, 26.84226448433411960, 8.527530157486179263 ) ) ;
#69862 = DIRECTION ( 'NONE',  ( -0.9862856015372319929, 0.000000000000000000, 0.1650476058606741014 ) ) ;
#69863 = DIRECTION ( 'NONE',  ( -1.000000000000000000, 0.000000000000000000, 0.000000000000000000 ) ) ;
#69864 = CARTESIAN_POINT ( 'NONE',  ( 19.84674366389459266, 8.717264484334116048, -2.638427012816827677 ) ) ;
#69865 = CARTESIAN_POINT ( 'NONE',  ( 1.472469842513823179, 30.59226448433411960, -4.923371831947296329 ) ) ;
#69866 = CARTESIAN_POINT ( 'NONE',  ( 2.035157376598824452, 13.68868534415483751, 7.964842623401179544 ) ) ;
#69867 = AXIS2_PLACEMENT_3D ( 'NONE', #88595, #34110, #4138 ) ;
#69868 = AXIS2_PLACEMENT_3D ( 'NONE', #39011, #8990, #38033 ) ;
#69869 = CARTESIAN_POINT ( 'NONE',  ( -2.816281873526473856, 34.12363466993042493, 9.499525473075851096E-16 ) ) ;
#69870 = CARTESIAN_POINT ( 'NONE',  ( 1.472469842513823179, 10.59226448433411782, -4.923371831947296329 ) ) ;
#69871 = CARTESIAN_POINT ( 'NONE',  ( 9.159723438033203990, 15.00000000000000000, -10.91613331444542645 ) ) ;
#69872 = CARTESIAN_POINT ( 'NONE',  ( 18.52753015748618282, 53.92559781766745175, -4.923371831947291888 ) ) ;
#69874 = CARTESIAN_POINT ( 'NONE',  ( -4.164238869374098151, 1.595415501580634388, -3.795296366450310543 ) ) ;
#69873 = CARTESIAN_POINT ( 'NONE',  ( 7.361572987183170547, 27.05059781766745175, 9.846743663894590881 ) ) ;
#69875 = CARTESIAN_POINT ( 'NONE',  ( 6.204703633549690345, 20.76208216824730357, -14.16423886937410259 ) ) ;
#69876 = CARTESIAN_POINT ( 'NONE',  ( 2.035157376598822676, 42.43868534415483396, -7.964842623401177768 ) ) ;
#69877 = CARTESIAN_POINT ( 'NONE',  ( 17.96484262340118221, 11.18868534415483929, -7.964842623401177768 ) ) ;
#69878 = CARTESIAN_POINT ( 'NONE',  ( 0.5774900079438590739, 42.64701867748816966, -5.440088680355550821 ) ) ;
#69879 = CARTESIAN_POINT ( 'NONE',  ( 10.00000000000000178, 29.31368534415483751, 10.88017736071110342 ) ) ;
#69880 = ORIENTED_EDGE ( 'NONE', *, *, #72374, .F. ) ;
#69881 = CARTESIAN_POINT ( 'NONE',  ( 19.38216949554541202, 30.99863466993042138, 9.382169495545424454 ) ) ;
#69882 = CARTESIAN_POINT ( 'NONE',  ( 19.42250999205614193, 40.14701867748817676, 5.440088680355555262 ) ) ;
#69883 = ORIENTED_EDGE ( 'NONE', *, *, #37217, .T. ) ;
#69884 = CARTESIAN_POINT ( 'NONE',  ( -2.816281873526473856, 54.33196800326376064, 3.434112377981055619 ) ) ;
#69885 = ADVANCED_FACE ( 'NONE', ( #47620 ), #66709, .F. ) ;
#69886 = CARTESIAN_POINT ( 'NONE',  ( 12.91533473730993009, 46.60535201082150536, -10.88017736071109987 ) ) ;
#69887 = ORIENTED_EDGE ( 'NONE', *, *, #43446, .T. ) ;
#69888 = CARTESIAN_POINT ( 'NONE',  ( 0.5774900079438590739, 47.64701867748817676, -5.440088680355550821 ) ) ;
#69889 = CARTESIAN_POINT ( 'NONE',  ( 6.284516029235898138, -36.06297093898795936, 4.000000000000000000 ) ) ;
#69890 = CARTESIAN_POINT ( 'NONE',  ( 19.72487221294571214, 57.80223176428831522, -6.499999999999988454 ) ) ;
#69891 = PRESENTATION_STYLE_ASSIGNMENT (( #16395 ) ) ;
#69892 = CARTESIAN_POINT ( 'NONE',  ( 20.36894250292379382, 63.67874883491396787, 10.36894250292379205 ) ) ;
#69893 = CARTESIAN_POINT ( 'NONE',  ( 10.00000000000000000, 66.81368534415484817, -10.88017736071110342 ) ) ;
#69894 = CARTESIAN_POINT ( 'NONE',  ( 24.16423886937409904, 9.095415501580633943, 3.795296366450317205 ) ) ;
#69895 = SURFACE_SIDE_STYLE ('',( #39402 ) ) ;
#69896 = CARTESIAN_POINT ( 'NONE',  ( 19.42250999205614193, 10.14701867748816966, 5.440088680355555262 ) ) ;
#69897 = CARTESIAN_POINT ( 'NONE',  ( 7.361572987183169658, 49.96726448433410894, -9.846743663894592657 ) ) ;
#69898 = ORIENTED_EDGE ( 'NONE', *, *, #56131, .F. ) ;
#69899 = CARTESIAN_POINT ( 'NONE',  ( 1.472469842513823179, 40.59226448433411605, -4.923371831947296329 ) ) ;
#69900 = TOROIDAL_SURFACE ( 'NONE', #65081, 14.49999999999999822, 0.5000000000000000000 ) ;
#69901 = CARTESIAN_POINT ( 'NONE',  ( 15.44008868035555260, 39.73035201082150536, 9.422509992056143702 ) ) ;
#69902 = CARTESIAN_POINT ( 'NONE',  ( 18.52753015748618282, 43.92559781766745175, -4.923371831947291888 ) ) ;
#69903 = CARTESIAN_POINT ( 'NONE',  ( 6.565887622018943937, 18.08196800326375708, -12.81628187352647608 ) ) ;
#69905 = DIRECTION ( 'NONE',  ( 0.9975640502598243087, -0.06975647374412535795, 0.000000000000000000 ) ) ;
#69904 = DIRECTION ( 'NONE',  ( -0.8320502943378437211, 0.5547001962252290364, 0.000000000000000000 ) ) ;
#69906 = CARTESIAN_POINT ( 'NONE',  ( 2.035157376598822676, 47.43868534415484817, -7.964842623401177768 ) ) ;
#69907 = CARTESIAN_POINT ( 'NONE',  ( -0.3689425029237881626, 57.42874883491397497, 10.36894250292379027 ) ) ;
#69908 = AXIS2_PLACEMENT_3D ( 'NONE', #12070, #33575, #96077 ) ;
#69909 = EDGE_CURVE ( 'NONE', #76829, #16659, #54125, .T. ) ;
#69910 = CARTESIAN_POINT ( 'NONE',  ( 3.591859063236763294, 18.29030133659708568, -11.09922568453595026 ) ) ;
#69911 = CARTESIAN_POINT ( 'NONE',  ( 0.000000000000000000, 15.00000000000000000, 0.000000000000000000 ) ) ;
#69912 = ORIENTED_EDGE ( 'NONE', *, *, #2414, .F. ) ;
#69913 = CARTESIAN_POINT ( 'NONE',  ( 21.09922568453594849, 26.20696800326375353, 6.408140936763242479 ) ) ;
#69914 = CARTESIAN_POINT ( 'NONE',  ( 17.96484262340118221, 19.93868534415484106, 7.964842623401181321 ) ) ;
#69915 = EDGE_CURVE ( 'NONE', #74674, #97132, #18829, .T. ) ;
#69916 = VERTEX_POINT ( 'NONE', #77126 ) ;
#69917 = VECTOR ( 'NONE', #47117, 999.9999999999998863 ) ;
#69918 = CARTESIAN_POINT ( 'NONE',  ( 2.791683348922240793, 46.63393115100077324, 7.208316651077764092 ) ) ;
#69919 = CARTESIAN_POINT ( 'NONE',  ( 2.791683348922240793, 31.63393115100078745, 7.208316651077764092 ) ) ;
#69920 = CARTESIAN_POINT ( 'NONE',  ( -10.86761736821483026, -97.98327470060252153, 3.750000000000000888 ) ) ;
#69921 = DIRECTION ( 'NONE',  ( -0.5807029557109348872, 0.000000000000000000, -0.8141155183563226760 ) ) ;
#69922 = CARTESIAN_POINT ( 'NONE',  ( 17.20831665107776587, 29.13393115100078390, -7.208316651077762316 ) ) ;
#69923 = CARTESIAN_POINT ( 'NONE',  ( 20.24186590665278018, 57.61633188102329228, -6.114288769123040090 ) ) ;
#69924 = CARTESIAN_POINT ( 'NONE',  ( 0.000000000000000000, 81.99999999999992895, 5.000000000000000000 ) ) ;
#69927 = CARTESIAN_POINT ( 'NONE',  ( 0.8218345515128016032, 0.04922511925147077944, 14.72992491912911639 ) ) ;
#69926 = MECHANICAL_DESIGN_GEOMETRIC_PRESENTATION_REPRESENTATION (  '', ( #25273 ), #76284 ) ;
#69925 = CARTESIAN_POINT ( 'NONE',  ( 17.20831665107776587, 7.883931151000784787, 7.208316651077764980 ) ) ;
#69928 = PRESENTATION_STYLE_ASSIGNMENT (( #71409 ) ) ;
#69930 = ORIENTED_EDGE ( 'NONE', *, *, #84695, .T. ) ;
#69929 = CARTESIAN_POINT ( 'NONE',  ( 18.52753015748618282, 43.92559781766745175, -4.923371831947291888 ) ) ;
#69931 = AXIS2_PLACEMENT_3D ( 'NONE', #2149, #76634, #84159 ) ;
#69932 = CARTESIAN_POINT ( 'NONE',  ( 5.624999999999999112, 3.451366962315989717, -9.742785792574936821 ) ) ;
#69933 = CARTESIAN_POINT ( 'NONE',  ( 19.38216949554541202, 15.99863466993042138, 9.382169495545424454 ) ) ;
#69934 = CARTESIAN_POINT ( 'NONE',  ( 15.44008868035555260, 54.73035201082150536, 9.422509992056143702 ) ) ;
#69935 = CARTESIAN_POINT ( 'NONE',  ( 20.36894250292379738, 44.92874883491396787, -10.36894250292379027 ) ) ;
#69936 =( NAMED_UNIT ( * ) PLANE_ANGLE_UNIT ( ) SI_UNIT ( $, .RADIAN. ) );
#69937 = DIRECTION ( 'NONE',  ( -1.000000000000000000, 0.000000000000000000, 0.000000000000000000 ) ) ;
#69938 = CARTESIAN_POINT ( 'NONE',  ( -2.266590686148945544, 47.22041550158063927, 7.082119434687048631 ) ) ;
#69939 = CARTESIAN_POINT ( 'NONE',  ( 17.08211943468705130, 53.47041550158063217, 12.26659068614894998 ) ) ;
#69940 = CARTESIAN_POINT ( 'NONE',  ( 20.36894250292379738, 19.92874883491396787, -10.36894250292379027 ) ) ;
#69942 = CARTESIAN_POINT ( 'NONE',  ( -2.827051895225590972, 14.76984989550149940, -14.67071941139717062 ) ) ;
#69941 = CARTESIAN_POINT ( 'NONE',  ( 2.917880565312948704, 22.63708216824730002, 12.26659068614894643 ) ) ;
#69943 = CARTESIAN_POINT ( 'NONE',  ( 13.82671409943293739, 15.00000000000000000, 3.447387012295318076 ) ) ;
#69945 = CARTESIAN_POINT ( 'NONE',  ( 1.472469842513823179, 46.42559781766745175, 4.923371831947296329 ) ) ;
#69944 = CARTESIAN_POINT ( 'NONE',  ( 5.113979357112576452, -17.50950876262128730, 2.750000000000000000 ) ) ;
#69946 = CARTESIAN_POINT ( 'NONE',  ( 19.42250999205614193, 40.14701867748817676, 5.440088680355555262 ) ) ;
#69947 = CARTESIAN_POINT ( 'NONE',  ( -12.07856007377816887, 4.482427100288500905E-16, -8.022367888855006512 ) ) ;
#69948 = CARTESIAN_POINT ( 'NONE',  ( 20.00000000000000711, 88.18274230950564174, -5.338627755225069826 ) ) ;
#69949 = EDGE_CURVE ( 'NONE', #39693, #40991, #8153, .T. ) ;
#69950 = CARTESIAN_POINT ( 'NONE',  ( 1.472469842513823179, 46.42559781766745175, 4.923371831947296329 ) ) ;
#69951 = CARTESIAN_POINT ( 'NONE',  ( 21.09922568453595559, 62.04030133659709634, -6.408140936763230044 ) ) ;
#69952 = CARTESIAN_POINT ( 'NONE',  ( 12.26659068614894466, -5.279584498419365168, -7.082119434687053960 ) ) ;
#69953 = CARTESIAN_POINT ( 'NONE',  ( 7.361572987183170547, 37.05059781766744464, 9.846743663894590881 ) ) ;
#69954 = CARTESIAN_POINT ( 'NONE',  ( 5.076628168052704559, 60.17559781766745175, -8.527530157486179263 ) ) ;
#69955 = CARTESIAN_POINT ( 'NONE',  ( -4.164238869374099039, 36.80374883491396787, 8.674139862899312516E-16 ) ) ;
#69956 = EDGE_LOOP ( 'NONE', ( #95688, #28602, #10154, #44860, #79415, #73437, #93849, #2067, #27700, #8288, #82647, #39050, #56460, #59977, #14185, #7310, #30173, #81101, #86220, #23521 ) ) ;
#69957 = CARTESIAN_POINT ( 'NONE',  ( 22.26659068614894466, 8.887082168247300018, 7.082119434687054849 ) ) ;
#69958 = CARTESIAN_POINT ( 'NONE',  ( -12.67147417979165525, 14.95037112956503478, -7.555862176155688559 ) ) ;
#69960 = CARTESIAN_POINT ( 'NONE',  ( -3.750000000000000000, 36.75000000000000000, -3.750000000000000000 ) ) ;
#69959 =( NAMED_UNIT ( * ) PLANE_ANGLE_UNIT ( ) SI_UNIT ( $, .RADIAN. ) );
#69961 = CARTESIAN_POINT ( 'NONE',  ( 7.084665262690076126, 12.02201867748817321, -10.88017736071110164 ) ) ;
#69962 = CARTESIAN_POINT ( 'NONE',  ( 22.81628187352647785, 6.623634669930420493, 6.195893100308588602E-16 ) ) ;
#69963 = SPHERICAL_SURFACE ( 'NONE', #75238, 0.2500000000000000000 ) ;
#69964 = CARTESIAN_POINT ( 'NONE',  ( 10.00000000000000000, 66.81368534415484817, -10.88017736071110342 ) ) ;
#69965 = CARTESIAN_POINT ( 'NONE',  ( 20.24186590665276597, 41.76028685723173339, 6.114288769123062295 ) ) ;
#69966 = CARTESIAN_POINT ( 'NONE',  ( -7.750355510519348456, 84.07179676972448590, -3.750000000000000000 ) ) ;
#69967 = CARTESIAN_POINT ( 'NONE',  ( -8.099999999999999645, 75.73428692542562146, -3.000000000000000000 ) ) ;
#69968 = CARTESIAN_POINT ( 'NONE',  ( 10.00000000000000000, 1.813685344154838175, -10.88017736071110342 ) ) ;
#69969 = DIRECTION ( 'NONE',  ( 0.7604059656000385914, 0.000000000000000000, -0.6494480483301746654 ) ) ;
#69970 = CARTESIAN_POINT ( 'NONE',  ( -0.8801773607111009756, 33.06368534415484106, 1.068504757029289695E-15 ) ) ;
#69971 = CARTESIAN_POINT ( 'NONE',  ( 0.5774900079438607392, 23.48035201082150536, 5.440088680355550821 ) ) ;
#69972 = CARTESIAN_POINT ( 'NONE',  ( 10.00000000000000178, 5.373634669930420493, 12.81628187352647608 ) ) ;
#69973 = CARTESIAN_POINT ( 'NONE',  ( 7.361572987183169658, 49.96726448433410894, -9.846743663894592657 ) ) ;
#69974 = CARTESIAN_POINT ( 'NONE',  ( -1.099225684535947600, 64.54030133659709634, 6.408140936763237150 ) ) ;
#69975 = CARTESIAN_POINT ( 'NONE',  ( 10.00000000000000000, -0.2410688489992152128, -9.846743663894594434 ) ) ;
#69976 = ORIENTED_EDGE ( 'NONE', *, *, #67635, .F. ) ;
#69977 = CARTESIAN_POINT ( 'NONE',  ( -0.8801773607110991993, 27.85535201082150181, -2.915334737309923874 ) ) ;
#69978 = CARTESIAN_POINT ( 'NONE',  ( 0.6178305044545838731, 29.74863466993042138, 9.382169495545420901 ) ) ;
#69979 = CARTESIAN_POINT ( 'NONE',  ( 13.99999999999999822, 61.00000000000000711, 6.500000000000000888 ) ) ;
#69980 = AXIS2_PLACEMENT_3D ( 'NONE', #562, #61504, #95960 ) ;
#69981 = CARTESIAN_POINT ( 'NONE',  ( 2.791683348922237240, 55.38393115100078745, -7.208316651077763204 ) ) ;
#69982 = CARTESIAN_POINT ( 'NONE',  ( 15.44008868035555793, 51.39701867748816966, -9.422509992056140149 ) ) ;
#69983 = CARTESIAN_POINT ( 'NONE',  ( 18.52753015748617571, 13.09226448433411960, 4.923371831947298993 ) ) ;
#69984 = CARTESIAN_POINT ( 'NONE',  ( 22.81628187352647785, 21.41530133659708923, 3.434112377981063169 ) ) ;
#69986 = DIRECTION ( 'NONE',  ( 0.000000000000000000, 0.000000000000000000, -1.000000000000000000 ) ) ;
#69985 = CARTESIAN_POINT ( 'NONE',  ( 17.96484262340118221, 64.93868534415483396, 7.964842623401181321 ) ) ;
#69987 = EDGE_LOOP ( 'NONE', ( #39118, #61110, #94045, #46195 ) ) ;
#69988 = CARTESIAN_POINT ( 'NONE',  ( 3.897244926436124857, 3.990182060915936250E-16, 13.96644127841333294 ) ) ;
#69989 = DIRECTION ( 'NONE',  ( -0.000000000000000000, -0.000000000000000000, 1.000000000000000000 ) ) ;
#69990 = CARTESIAN_POINT ( 'NONE',  ( 2.035157376598824452, 48.68868534415483396, 7.964842623401179544 ) ) ;
#69992 = CARTESIAN_POINT ( 'NONE',  ( 17.08211943468705840, 15.13708216824730179, -12.26659068614894466 ) ) ;
#69991 = CARTESIAN_POINT ( 'NONE',  ( 0.6178305044545818747, 48.49863466993042493, -9.382169495545419124 ) ) ;
#69993 = CARTESIAN_POINT ( 'NONE',  ( 19.84674366389459621, 23.50893115100078390, 7.409399052514197653E-17 ) ) ;
#69994 = VECTOR ( 'NONE', #98735, 1000.000000000000000 ) ;
#69995 = CARTESIAN_POINT ( 'NONE',  ( 10.00000000000000000, 11.81368534415483751, -10.88017736071110342 ) ) ;
#69996 = CARTESIAN_POINT ( 'NONE',  ( 12.63842701281683922, 24.55059781766745175, -9.846743663894590881 ) ) ;
#69997 = CARTESIAN_POINT ( 'NONE',  ( 5.129999999999990123, 76.07179676972444327, 6.250000000000000000 ) ) ;
#69998 = CARTESIAN_POINT ( 'NONE',  ( 10.00000000000000178, 58.05374883491397497, 14.16423886937410082 ) ) ;
#69999 = ORIENTED_EDGE ( 'NONE', *, *, #14598, .F. ) ;
#70000 = DIRECTION ( 'NONE',  ( 0.000000000000000000, 0.000000000000000000, 1.000000000000000000 ) ) ;
#70001 = VECTOR ( 'NONE', #88299, 1000.000000000000000 ) ;
#70002 = EDGE_CURVE ( 'NONE', #1078, #87032, #95481, .T. ) ;
#70003 = CARTESIAN_POINT ( 'NONE',  ( 12.91533473730993009, 6.605352010821504471, -10.88017736071109987 ) ) ;
#70004 = CARTESIAN_POINT ( 'NONE',  ( 0.1532563361054100626, 15.80059781766745353, -2.638427012816831230 ) ) ;
#70005 = AXIS2_PLACEMENT_3D ( 'NONE', #1039, #53522, #24530 ) ;
#70006 = ORIENTED_EDGE ( 'NONE', *, *, #33124, .F. ) ;
#70007 = CARTESIAN_POINT ( 'NONE',  ( 2.035157376598822676, 2.438685344154838397, -7.964842623401177768 ) ) ;
#70008 = CARTESIAN_POINT ( 'NONE',  ( 12.91533473730993009, 6.605352010821504471, -10.88017736071109987 ) ) ;
#70009 = CARTESIAN_POINT ( 'NONE',  ( 14.92337183194729988, 44.34226448433412315, -8.527530157486177487 ) ) ;
#70010 = CARTESIAN_POINT ( 'NONE',  ( -2.816281873526473856, 49.12363466993042493, 9.499525473075851096E-16 ) ) ;
#70011 = CARTESIAN_POINT ( 'NONE',  ( -42.94000000000001194, 92.00000000000000000, 9.000000000000000000 ) ) ;
#70012 = CARTESIAN_POINT ( 'NONE',  ( 6.204703633549690345, 25.76208216824730712, -14.16423886937410259 ) ) ;
#70013 = CARTESIAN_POINT ( 'NONE',  ( 4.559911319644449179, 23.89701867748817321, 9.422509992056141925 ) ) ;
#70014 = CARTESIAN_POINT ( 'NONE',  ( 6.204703633549690345, 67.84541550158060375, 14.16423886937410082 ) ) ;
#70015 = ADVANCED_FACE ( 'NONE', ( #10122 ), #61138, .F. ) ;
#70016 = ADVANCED_FACE ( 'NONE', ( #92620 ), #73191, .F. ) ;
#70017 = CARTESIAN_POINT ( 'NONE',  ( 0.1532563361054082862, 46.21726448433411605, 2.638427012816831674 ) ) ;
#70018 = DIRECTION ( 'NONE',  ( -0.000000000000000000, 0.000000000000000000, 1.000000000000000000 ) ) ;
#70019 = CARTESIAN_POINT ( 'NONE',  ( 14.92337183194729633, 32.67559781766745175, 8.527530157486181039 ) ) ;
#70020 = CARTESIAN_POINT ( 'NONE',  ( -46.44000000000001194, 93.00000000000000000, -9.500000000000000000 ) ) ;
#70021 = CARTESIAN_POINT ( 'NONE',  ( 2.638427012816829897, 29.55059781766745530, -9.846743663894592657 ) ) ;
#70022 = VERTEX_POINT ( 'NONE', #56600 ) ;
#70023 = CARTESIAN_POINT ( 'NONE',  ( 4.559911319644449179, 67.23035201082150536, -9.422509992056141925 ) ) ;
#70024 = EDGE_CURVE ( 'NONE', #1559, #23534, #54006, .T. ) ;
#70025 = CARTESIAN_POINT ( 'NONE',  ( 19.84674366389459621, 58.50893115100078745, 7.409399052514197653E-17 ) ) ;
#70026 = CARTESIAN_POINT ( 'NONE',  ( -0.8801773607110991993, 42.85535201082150536, -2.915334737309923874 ) ) ;
#70028 = CARTESIAN_POINT ( 'NONE',  ( 10.00000000000000178, 30.37363466993042138, 12.81628187352647608 ) ) ;
#70027 = CARTESIAN_POINT ( 'NONE',  ( 17.96484262340118221, 4.938685344154837509, 7.964842623401181321 ) ) ;
#70029 = CARTESIAN_POINT ( 'NONE',  ( -4.164238869374098151, 16.59541550158063927, -3.795296366450310543 ) ) ;
#70030 = ADVANCED_FACE ( 'NONE', ( #19089, #27069 ), #34071, .F. ) ;
#70031 = CARTESIAN_POINT ( 'NONE',  ( 13.43411237798106583, 47.66530133659709634, -12.81628187352647252 ) ) ;
#70032 = ORIENTED_EDGE ( 'NONE', *, *, #40605, .F. ) ;
#70033 = CARTESIAN_POINT ( 'NONE',  ( 10.00000000000000000, 64.75893115100078035, -9.846743663894594434 ) ) ;
#70034 = CARTESIAN_POINT ( 'NONE',  ( 20.88017736071110519, 15.56368534415483751, 2.639326808657452039E-16 ) ) ;
#70035 = ORIENTED_EDGE ( 'NONE', *, *, #12967, .F. ) ;
#70036 = ADVANCED_FACE ( 'NONE', ( #49094 ), #41615, .T. ) ;
#70037 = CARTESIAN_POINT ( 'NONE',  ( 7.084665262690076126, 32.02201867748816966, -10.88017736071110164 ) ) ;
#70038 = ORIENTED_EDGE ( 'NONE', *, *, #79708, .F. ) ;
#70039 = CARTESIAN_POINT ( 'NONE',  ( 19.42250999205614193, 65.14701867748817676, 5.440088680355555262 ) ) ;
#70040 = CARTESIAN_POINT ( 'NONE',  ( 20.88017736071110875, 65.77201867748817676, -2.915334737309920765 ) ) ;
#70041 = CARTESIAN_POINT ( 'NONE',  ( 0.000000000000000000, 14.49999999999999822, 0.000000000000000000 ) ) ;
#70042 = CARTESIAN_POINT ( 'NONE',  ( 10.00000000000000178, 12.25893115100078568, 9.846743663894594434 ) ) ;
#70043 = CARTESIAN_POINT ( 'NONE',  ( 7.084665262690076126, 69.10535201082151957, 10.88017736071109987 ) ) ;
#70044 = CARTESIAN_POINT ( 'NONE',  ( -46.52365679472261206, 102.3054413859459828, 7.234551493516248932 ) ) ;
#70047 = ORIENTED_EDGE ( 'NONE', *, *, #68885, .T. ) ;
#70046 = VECTOR ( 'NONE', #98938, 1000.000000000000114 ) ;
#70045 = CARTESIAN_POINT ( 'NONE',  ( 10.00000000000000178, 2.258931151000784787, 9.846743663894594434 ) ) ;
#70048 = CARTESIAN_POINT ( 'NONE',  ( 19.84674366389459266, 38.30059781766745175, 2.638427012816836559 ) ) ;
#70049 = ORIENTED_EDGE ( 'NONE', *, *, #10726, .F. ) ;
#70050 = ORIENTED_EDGE ( 'NONE', *, *, #71461, .T. ) ;
#70051 = FACE_OUTER_BOUND ( 'NONE', #54132, .T. ) ;
#70052 = CARTESIAN_POINT ( 'NONE',  ( 20.36894250292379382, 8.678748834913967869, 10.36894250292379205 ) ) ;
#70053 = CARTESIAN_POINT ( 'NONE',  ( 10.00000000000000000, 62.87363466993042493, -12.81628187352647608 ) ) ;
#70054 = SURFACE_SIDE_STYLE ('',( #56525 ) ) ;
#70055 = CARTESIAN_POINT ( 'NONE',  ( 17.08211943468705130, 18.47041550158063572, 12.26659068614894998 ) ) ;
#70056 = CIRCLE ( 'NONE', #34923, 19.99999999999999645 ) ;
#70057 = DIRECTION ( 'NONE',  ( 0.000000000000000000, -1.000000000000000000, 0.000000000000000000 ) ) ;
#70059 = CARTESIAN_POINT ( 'NONE',  ( -0.8801773607111009756, 63.06368534415484106, 1.068504757029289695E-15 ) ) ;
#70058 = DIRECTION ( 'NONE',  ( 0.000000000000000000, -1.000000000000000000, 0.000000000000000000 ) ) ;
#70060 = CARTESIAN_POINT ( 'NONE',  ( -0.8801773607110991993, 22.85535201082150181, -2.915334737309923874 ) ) ;
#70061 = CARTESIAN_POINT ( 'NONE',  ( 5.800000000000003375, 99.99999999999998579, 8.000000000000000000 ) ) ;
#70062 = EDGE_LOOP ( 'NONE', ( #53648, #28187, #75575, #96830 ) ) ;
#70063 = CARTESIAN_POINT ( 'NONE',  ( 14.92337183194729988, 9.342264484334119601, -8.527530157486177487 ) ) ;
#70064 = CARTESIAN_POINT ( 'NONE',  ( 19.84674366389459266, 8.717264484334116048, -2.638427012816827677 ) ) ;
#70065 = CARTESIAN_POINT ( 'NONE',  ( 13.43411237798105340, 35.58196800326375353, 12.81628187352647963 ) ) ;
#70066 = CARTESIAN_POINT ( 'NONE',  ( 10.00000000000000178, 27.25893115100078390, 9.846743663894594434 ) ) ;
#70067 = MECHANICAL_DESIGN_GEOMETRIC_PRESENTATION_REPRESENTATION (  '', ( #71635 ), #1428 ) ;
#70068 =( NAMED_UNIT ( * ) SI_UNIT ( $, .STERADIAN. ) SOLID_ANGLE_UNIT ( ) );
#70069 = EDGE_CURVE ( 'NONE', #44471, #81942, #72083, .T. ) ;
#70070 = CARTESIAN_POINT ( 'NONE',  ( 13.43411237798106583, 17.66530133659708923, -12.81628187352647252 ) ) ;
#70071 = AXIS2_PLACEMENT_3D ( 'NONE', #70291, #70785, #39791 ) ;
#70072 = DIRECTION ( 'NONE',  ( 0.000000000000000000, 0.000000000000000000, 1.000000000000000000 ) ) ;
#70073 = CARTESIAN_POINT ( 'NONE',  ( 2.791683348922240793, 6.633931151000785675, 7.208316651077764092 ) ) ;
#70074 = ORIENTED_EDGE ( 'NONE', *, *, #49530, .T. ) ;
#70075 = ORIENTED_EDGE ( 'NONE', *, *, #2981, .F. ) ;
#70076 = CARTESIAN_POINT ( 'NONE',  ( -0.8801773607110991993, 42.85535201082150536, -2.915334737309923874 ) ) ;
#70077 = CARTESIAN_POINT ( 'NONE',  ( -4.164238869374099927, 32.01208216824730357, 3.795296366450308767 ) ) ;
#70078 = CARTESIAN_POINT ( 'NONE',  ( 2.791683348922240793, 36.63393115100078035, 7.208316651077764092 ) ) ;
#70079 = CARTESIAN_POINT ( 'NONE',  ( 17.20831665107776587, 4.133931151000785675, -7.208316651077762316 ) ) ;
#70081 = DIRECTION ( 'NONE',  ( -1.000000000000000000, 0.000000000000000000, 0.000000000000000000 ) ) ;
#70080 = CARTESIAN_POINT ( 'NONE',  ( 3.591859063236761518, 59.95696800326375353, 11.09922568453594849 ) ) ;
#70082 = CARTESIAN_POINT ( 'NONE',  ( 12.91533473730993009, 21.60535201082150536, -10.88017736071109987 ) ) ;
#70083 = CARTESIAN_POINT ( 'NONE',  ( 3.591859063236761518, 24.95696800326375353, 11.09922568453594849 ) ) ;
#70084 = CARTESIAN_POINT ( 'NONE',  ( 0.1532563361054082862, 41.21726448433411605, 2.638427012816831674 ) ) ;
#70085 = CARTESIAN_POINT ( 'NONE',  ( -5.204170427930421283E-15, -3.186314655845158494, -10.88017736071110342 ) ) ;
#70086 = CARTESIAN_POINT ( 'NONE',  ( 10.00000000000000178, 55.37363466993042493, 12.81628187352647608 ) ) ;
#70087 = PLANE ( 'NONE',  #2151 ) ;
#70089 = CARTESIAN_POINT ( 'NONE',  ( 0.000000000000000000, 0.5000000000000004441, 0.000000000000000000 ) ) ;
#70088 = CARTESIAN_POINT ( 'NONE',  ( 4.559911319644449179, 53.89701867748817676, 9.422509992056141925 ) ) ;
#70090 = AXIS2_PLACEMENT_3D ( 'NONE', #87, #13571, #30534 ) ;
#70091 = DIRECTION ( 'NONE',  ( 0.000000000000000000, 0.000000000000000000, 1.000000000000000000 ) ) ;
#70092 = DIRECTION ( 'NONE',  ( -0.000000000000000000, -1.000000000000000000, -0.000000000000000000 ) ) ;
#70093 =( BOUNDED_SURFACE ( )  B_SPLINE_SURFACE ( 1, 2, ( 
 ( #89378, #41448, #5406, #18925, #66373, #96907, #58876, #51380, #33892, #64879, #79902, #26902, #83360, #14382, #43864, #29356, #74866, #6365, #82361, #53850, #59859, #91849, #37876, #59364, #15377, #82867, #76350, #60353, #13883, #60846, #67368, #68369, #37382, #67872, #51879, #22872, #98393, #44367, #91345, #7865, #89867, #97392, #90346, #98888, #53343, #30339, #14883, #45352, #83851, #28860, #97898, #66875, #21884, #21382, #36380, #45859, #7377, #36879, #52362, #38361, #30840, #68858, #390, #44851, #61338, #75357, #6871, #23365, #13380, #29850, #74359, #90847, #52853, #5888, #22378, #75857, #16838, #39346, #55819, #10316, #54322, #867, #47311, #76831, #15859, #39828, #24349, #17337, #70334, #84836, #78307, #63782, #1850, #77810, #9826, #54812, #25814, #32308, #24834, #2344, #46826, #92819, #9325, #69840, #86314, #40817, #16344, #31326, #62813, #8346, #46344, #93311, #85323, #47806, #55316, #77318, #40327, #94291, #85823, #70831, #8832, #32800, #84358, #38854, #1364, #31815, #62312, #61826, #17817, #63295, #92334, #93806, #33291, #25335, #69343, #48299, #78806, #71316, #2834, #23857, #48790, #26285, #87281, #56786, #96784, #56310, #73263, #5285, #80280, #57276, #49772, #12269, #43260, #12762, #35761, #86806, #87770, #71798, #42779, #19285, #11781, #64763, #88764, #79785, #95275, #3304, #27266, #42288, #18308, #72275, #18802, #49286, #11288, #79298, #3805, #66250, #80776, #33766, #58246, #26778, #20275, #4295, #41807, #4786, #34261, #35261, #72760, #34769, #94785, #65758, #65257, #95785, #96283, #50772, #64273, #41325, #57765, #27762, #81263, #73754, #88269, #19772, #10807, #50259, #82244, #81744, #6260, #74239, #51260, #52736, #22262, #28753, #13758, #83243, #45742, #68255, #53234, #59742, #60728, #59245, #13260, #98775, #36763, #67256, #30223, #37269, #14766, #20770, #97279, #89744, #21262, #68740, #28259, #45239, #76238, #52249, #29245, #21770, #75736, #15261, #83739, #7755, #58755, #90237, #43752, #7255, #82744, #14264, #97780, #91227, #51759, #44741, #5772, #98275, #75242, #89259, #44245, #74749, #6752, #67756, #36260, #29732, #38249, #37759, #66756, #22751, #60240, #90735, #47197, #759, #47702, #54208, #24719, #24230, #54696, #38734, #9707, #85218, #31210, #78194, #93690, #76721, #84245, #77210, #55192, #40205, #85709, #70217, #1736, #70711, #15749, #84725, #53728, #8716, #46235, #23253, #17223, #93192, #61706, #16230, #2229, #17712, #32688, #25224, #31704, #63183, #92220, #8240, #55704, #86200, #39234, #40699, #16722, #39724, #48184, #23748, #69722, #62197, #46710, #78696, #10206, #69235, #1248, #92705, #91731 ),
 ( #77700, #9211, #32190, #62692, #272, #30717, #61226, #59508, #14025, #79676, #26665, #44004, #64157, #36525, #88149, #19661, #21524, #49174, #11173, #74506, #80158, #65145, #63672, #41206, #3197, #71686, #71202, #2725, #51518, #52018, #95156, #72163, #64645, #27150, #90004, #28998, #82509, #33179, #3690, #86691, #57652, #34151, #57159, #41693, #6028, #94675, #87657, #18196, #42181, #19170, #94176, #87165, #33661, #26184, #56676, #25707, #18691, #56199, #95665, #48676, #67017, #49650, #97538, #11668, #72645, #82012, #4178, #13522, #34649, #79179, #10694, #53981, #30481, #75501, #23511, #38993, #22026, #29487, #22516, #530, #84490, #68995, #15517, #45999, #15992, #59996, #98537, #98032, #52988, #90489, #67514, #30977, #38501, #44994, #29989, #61475, #61967, #46480, #69485, #75992, #76975, #7013, #52498, #8488, #91981, #83504, #84971, #60981, #83993, #1004, #37518, #15021, #7521, #60496, #31465, #92466, #14525, #83008, #38012, #37016, #75005, #35, #45491, #76489, #91494, #68010, #23994, #54466, #23015, #68504, #90985, #53482, #44505, #6510, #8003, #85470, #47460, #31950, #2976, #2491, #62452, #47946, #56453, #70971, #17960, #55467, #85969, #86939, #94437, #63446, #24489, #55963, #93953, #69978, #17479, #32945, #77459, #25950, #92954, #8972, #16490, #33426, #46965, #16982, #25479, #86462, #10456, #77961, #39970, #70471, #40473, #18451, #48933, #32457, #78453, #9967, #48446, #39489, #1500, #54953, #9468, #1991, #78946, #63924, #62953, #40964, #93457, #24982, #71463, #58784, #44766, #73783, #82271, #80804, #58277, #20303, #88795, #29758, #88302, #6287, #37295, #13289, #89290, #81774, #44273, #75271, #6781, #67782, #19800, #20800, #4817, #74778, #51289, #43777, #96814, #21795, #12788, #28290, #35291, #59276, #74268, #50291, #5313, #50803, #81292, #43288, #12301, #35791, #98304, #13786, #65784, #90262, #5799, #52275, #36289, #66279, #36790, #66787, #67284, #97306, #28778, #27792, #97812, #89775, #21292, #29273, #82774, #96317, #73293, #51785, #59769, #14294, #42809, #31237, #61732, #39263, #75763, #15289, #14795, #38276, #7284, #83271, #84753, #54240, #60755, #45771, #16258, #77728, #1280, #85244, #91757, #30251, #46262, #30745, #76264, #68769, #784, #7781, #62229, #39751, #83766, #301, #98803, #46740, #61252, #91255, #92250, #8742, #23280, #53756, #70248, #16750, #23775, #22781, #77238, #69752, #45268, #84274, #31733, #22290, #47225, #68282, #52763, #60266, #24260, #90765, #37785, #92736, #69264, #54724, #53260, #15773, #76747, #8264, #9240, #1764, #38764, #2752, #56227, #48705, #87685, #32220, #72192, #19199, #72675 ) ),
 .UNSPECIFIED., .F., .F., .F. ) 
 B_SPLINE_SURFACE_WITH_KNOTS ( ( 2, 2 ),
 ( 3, 2, 2, 2, 2, 2, 2, 2, 2, 2, 2, 2, 2, 2, 2, 2, 2, 2, 2, 2, 2, 2, 2, 2, 2, 2, 2, 2, 2, 2, 2, 2, 2, 2, 2, 2, 2, 2, 2, 2, 2, 2, 2, 2, 2, 2, 2, 2, 2, 2, 2, 2, 2, 2, 2, 2, 2, 2, 2, 2, 2, 2, 2, 2, 2, 2, 2, 2, 2, 2, 2, 2, 2, 2, 2, 2, 2, 2, 2, 2, 2, 2, 2, 2, 2, 2, 2, 2, 2, 2, 2, 2, 2, 2, 2, 2, 2, 2, 2, 2, 2, 2, 2, 2, 2, 2, 2, 2, 2, 2, 2, 2, 2, 2, 2, 2, 2, 2, 2, 2, 2, 2, 2, 2, 2, 2, 2, 2, 2, 2, 2, 2, 2, 2, 2, 2, 2, 2, 2, 2, 2, 2, 2, 2, 2, 2, 2, 2, 2, 2, 2, 2, 2, 2, 2, 2, 2, 2, 2, 2, 2, 2, 3 ),
 ( 0.000000000000000000, 1.000000000000000000 ),
 ( 0.000000000000000000, 0.005952380952380952051, 0.01190476190476190410, 0.01785714285714285615, 0.02380952380952380820, 0.02976190476190476025, 0.03571428571428571230, 0.04166666666666666435, 0.04761904761904761640, 0.05357142857142856845, 0.05952380952380952051, 0.06547619047619047949, 0.07142857142857142461, 0.07738095238095238360, 0.08333333333333332871, 0.08928571428571428770, 0.09523809523809523281, 0.1011904761904761918, 0.1071428571428571369, 0.1130952380952380959, 0.1190476190476190410, 0.1250000000000000000, 0.1309523809523809590, 0.1369047619047619180, 0.1428571428571428492, 0.1488095238095238082, 0.1547619047619047672, 0.1607142857142857262, 0.1666666666666666574, 0.1726190476190476164, 0.1785714285714285754, 0.1845238095238095344, 0.1904761904761904656, 0.1964285714285714246, 0.2023809523809523836, 0.2083333333333333426, 0.2142857142857142738, 0.2202380952380952328, 0.2261904761904761918, 0.2321428571428571508, 0.2380952380952380820, 0.2440476190476190410, 0.2500000000000000000, 0.2559523809523809312, 0.2619047619047619180, 0.2678571428571428492, 0.2738095238095238360, 0.2797619047619047672, 0.2857142857142856984, 0.2916666666666666852, 0.2976190476190476164, 0.3035714285714285476, 0.3095238095238095344, 0.3154761904761904656, 0.3214285714285714524, 0.3273809523809523836, 0.3333333333333333148, 0.3392857142857143016, 0.3452380952380952328, 0.3511904761904761640, 0.3571428571428571508, 0.3630952380952380820, 0.3690476190476190688, 0.3750000000000000000, 0.3809523809523809312, 0.3869047619047619180, 0.3928571428571428492, 0.3988095238095238360, 0.4047619047619047672, 0.4107142857142856984, 0.4166666666666666852, 0.4226190476190476164, 0.4285714285714285476, 0.4345238095238095344, 0.4404761904761904656, 0.4464285714285714524, 0.4523809523809523836, 0.4583333333333333148, 0.4642857142857143016, 0.4702380952380952328, 0.4761904761904761640, 0.4821428571428571508, 0.4880952380952380820, 0.4940476190476190688, 0.5000000000000000000, 0.5059523809523809312, 0.5119047619047618625, 0.5178571428571429047, 0.5238095238095238360, 0.5297619047619047672, 0.5357142857142856984, 0.5416666666666666297, 0.5476190476190476719, 0.5535714285714286031, 0.5595238095238095344, 0.5654761904761904656, 0.5714285714285713969, 0.5773809523809523281, 0.5833333333333333703, 0.5892857142857143016, 0.5952380952380952328, 0.6011904761904761640, 0.6071428571428570953, 0.6130952380952381375, 0.6190476190476190688, 0.6250000000000000000, 0.6309523809523809312, 0.6369047619047618625, 0.6428571428571429047, 0.6488095238095238360, 0.6547619047619047672, 0.6607142857142856984, 0.6666666666666666297, 0.6726190476190476719, 0.6785714285714286031, 0.6845238095238095344, 0.6904761904761904656, 0.6964285714285713969, 0.7023809523809523281, 0.7083333333333333703, 0.7142857142857143016, 0.7202380952380952328, 0.7261904761904761640, 0.7321428571428570953, 0.7380952380952381375, 0.7440476190476190688, 0.7500000000000000000, 0.7559523809523809312, 0.7619047619047618625, 0.7678571428571429047, 0.7738095238095238360, 0.7797619047619047672, 0.7857142857142856984, 0.7916666666666666297, 0.7976190476190476719, 0.8035714285714286031, 0.8095238095238095344, 0.8154761904761904656, 0.8214285714285713969, 0.8273809523809523281, 0.8333333333333333703, 0.8392857142857143016, 0.8452380952380952328, 0.8511904761904761640, 0.8571428571428570953, 0.8630952380952381375, 0.8690476190476190688, 0.8750000000000000000, 0.8809523809523809312, 0.8869047619047618625, 0.8928571428571429047, 0.8988095238095238360, 0.9047619047619047672, 0.9107142857142856984, 0.9166666666666666297, 0.9226190476190476719, 0.9285714285714286031, 0.9345238095238095344, 0.9404761904761904656, 0.9464285714285713969, 0.9523809523809523281, 0.9583333333333333703, 0.9642857142857143016 ),
 .UNSPECIFIED. ) 
 GEOMETRIC_REPRESENTATION_ITEM ( )  RATIONAL_B_SPLINE_SURFACE ( (
 ( 1.000000000000000000, 0.9659258262890683122, 1.000000000000000000, 0.9659258262890683122, 1.000000000000000000, 0.9659258262890683122, 1.000000000000000000, 0.9659258262890683122, 1.000000000000000000, 0.9659258262890683122, 1.000000000000000000, 0.9659258262890683122, 1.000000000000000000, 0.9659258262890683122, 1.000000000000000000, 0.9659258262890683122, 1.000000000000000000, 0.9659258262890683122, 1.000000000000000000, 0.9659258262890683122, 1.000000000000000000, 0.9659258262890683122, 1.000000000000000000, 0.9659258262890683122, 1.000000000000000000, 0.9659258262890683122, 1.000000000000000000, 0.9659258262890683122, 1.000000000000000000, 0.9659258262890683122, 1.000000000000000000, 0.9659258262890683122, 1.000000000000000000, 0.9659258262890683122, 1.000000000000000000, 0.9659258262890683122, 1.000000000000000000, 0.9659258262890683122, 1.000000000000000000, 0.9659258262890683122, 1.000000000000000000, 0.9659258262890683122, 1.000000000000000000, 0.9659258262890683122, 1.000000000000000000, 0.9659258262890683122, 1.000000000000000000, 0.9659258262890683122, 1.000000000000000000, 0.9659258262890683122, 1.000000000000000000, 0.9659258262890683122, 1.000000000000000000, 0.9659258262890683122, 1.000000000000000000, 0.9659258262890683122, 1.000000000000000000, 0.9659258262890683122, 1.000000000000000000, 0.9659258262890683122, 1.000000000000000000, 0.9659258262890683122, 1.000000000000000000, 0.9659258262890683122, 1.000000000000000000, 0.9659258262890683122, 1.000000000000000000, 0.9659258262890683122, 1.000000000000000000, 0.9659258262890683122, 1.000000000000000000, 0.9659258262890683122, 1.000000000000000000, 0.9659258262890683122, 1.000000000000000000, 0.9659258262890683122, 1.000000000000000000, 0.9659258262890683122, 1.000000000000000000, 0.9659258262890683122, 1.000000000000000000, 0.9659258262890683122, 1.000000000000000000, 0.9659258262890683122, 1.000000000000000000, 0.9659258262890683122, 1.000000000000000000, 0.9659258262890683122, 1.000000000000000000, 0.9659258262890683122, 1.000000000000000000, 0.9659258262890683122, 1.000000000000000000, 0.9659258262890683122, 1.000000000000000000, 0.9659258262890683122, 1.000000000000000000, 0.9659258262890683122, 1.000000000000000000, 0.9659258262890683122, 1.000000000000000000, 0.9659258262890683122, 1.000000000000000000, 0.9659258262890683122, 1.000000000000000000, 0.9659258262890683122, 1.000000000000000000, 0.9659258262890683122, 1.000000000000000000, 0.9659258262890683122, 1.000000000000000000, 0.9659258262890683122, 1.000000000000000000, 0.9659258262890683122, 1.000000000000000000, 0.9659258262890683122, 1.000000000000000000, 0.9659258262890683122, 1.000000000000000000, 0.9659258262890683122, 1.000000000000000000, 0.9659258262890683122, 1.000000000000000000, 0.9659258262890683122, 1.000000000000000000, 0.9659258262890683122, 1.000000000000000000, 0.9659258262890683122, 1.000000000000000000, 0.9659258262890683122, 1.000000000000000000, 0.9659258262890683122, 1.000000000000000000, 0.9659258262890683122, 1.000000000000000000, 0.9659258262890683122, 1.000000000000000000, 0.9659258262890683122, 1.000000000000000000, 0.9659258262890683122, 1.000000000000000000, 0.9659258262890683122, 1.000000000000000000, 0.9659258262890683122, 1.000000000000000000, 0.9659258262890683122, 1.000000000000000000, 0.9659258262890683122, 1.000000000000000000, 0.9659258262890683122, 1.000000000000000000, 0.9659258262890683122, 1.000000000000000000, 0.9659258262890683122, 1.000000000000000000, 0.9659258262890683122, 1.000000000000000000, 0.9659258262890683122, 1.000000000000000000, 0.9659258262890683122, 1.000000000000000000, 0.9659258262890683122, 1.000000000000000000, 0.9659258262890683122, 1.000000000000000000, 0.9659258262890683122, 1.000000000000000000, 0.9659258262890683122, 1.000000000000000000, 0.9659258262890683122, 1.000000000000000000, 0.9659258262890683122, 1.000000000000000000, 0.9659258262890683122, 1.000000000000000000, 0.9659258262890683122, 1.000000000000000000, 0.9659258262890683122, 1.000000000000000000, 0.9659258262890683122, 1.000000000000000000, 0.9659258262890683122, 1.000000000000000000, 0.9659258262890683122, 1.000000000000000000, 0.9659258262890683122, 1.000000000000000000, 0.9659258262890683122, 1.000000000000000000, 0.9659258262890683122, 1.000000000000000000, 0.9659258262890683122, 1.000000000000000000, 0.9659258262890683122, 1.000000000000000000, 0.9659258262890683122, 1.000000000000000000, 0.9659258262890683122, 1.000000000000000000, 0.9659258262890683122, 1.000000000000000000, 0.9659258262890683122, 1.000000000000000000, 0.9659258262890683122, 1.000000000000000000, 0.9659258262890683122, 1.000000000000000000, 0.9659258262890683122, 1.000000000000000000, 0.9659258262890683122, 1.000000000000000000, 0.9659258262890683122, 1.000000000000000000, 0.9659258262890683122, 1.000000000000000000, 0.9659258262890683122, 1.000000000000000000, 0.9659258262890683122, 1.000000000000000000, 0.9659258262890683122, 1.000000000000000000, 0.9659258262890683122, 1.000000000000000000, 0.9659258262890683122, 1.000000000000000000, 0.9659258262890683122, 1.000000000000000000, 0.9659258262890683122, 1.000000000000000000, 0.9659258262890683122, 1.000000000000000000, 0.9659258262890683122, 1.000000000000000000, 0.9659258262890683122, 1.000000000000000000, 0.9659258262890683122, 1.000000000000000000, 0.9659258262890683122, 1.000000000000000000, 0.9659258262890683122, 1.000000000000000000, 0.9659258262890683122, 1.000000000000000000, 0.9659258262890683122, 1.000000000000000000, 0.9659258262890683122, 1.000000000000000000, 0.9659258262890683122, 1.000000000000000000, 0.9659258262890683122, 1.000000000000000000, 0.9659258262890683122, 1.000000000000000000, 0.9659258262890683122, 1.000000000000000000, 0.9659258262890683122, 1.000000000000000000, 0.9659258262890683122, 1.000000000000000000, 0.9659258262890683122, 1.000000000000000000, 0.9659258262890683122, 1.000000000000000000, 0.9659258262890683122, 1.000000000000000000, 0.9659258262890683122, 1.000000000000000000, 0.9659258262890683122, 1.000000000000000000, 0.9659258262890683122, 1.000000000000000000, 0.9659258262890683122, 1.000000000000000000, 0.9659258262890683122, 1.000000000000000000, 0.9659258262890683122, 1.000000000000000000, 0.9659258262890683122, 1.000000000000000000, 0.9659258262890683122, 1.000000000000000000, 0.9659258262890683122, 1.000000000000000000, 0.9659258262890683122, 1.000000000000000000, 0.9659258262890683122, 1.000000000000000000, 0.9659258262890683122, 1.000000000000000000, 0.9659258262890683122, 1.000000000000000000, 0.9659258262890683122, 1.000000000000000000, 0.9659258262890683122, 1.000000000000000000, 0.9659258262890683122, 1.000000000000000000, 0.9659258262890683122, 1.000000000000000000, 0.9659258262890683122, 1.000000000000000000, 0.9659258262890683122, 1.000000000000000000, 0.9659258262890683122, 1.000000000000000000, 0.9659258262890683122, 1.000000000000000000, 0.9659258262890683122, 1.000000000000000000, 0.9659258262890683122, 1.000000000000000000, 0.9659258262890683122, 1.000000000000000000, 0.9659258262890683122, 1.000000000000000000, 0.9659258262890683122, 1.000000000000000000, 0.9659258262890683122, 1.000000000000000000, 0.9659258262890683122, 1.000000000000000000, 0.9659258262890683122, 1.000000000000000000, 0.9659258262890683122, 1.000000000000000000),
 ( 1.000000000000000000, 0.9659258262890683122, 1.000000000000000000, 0.9659258262890683122, 1.000000000000000000, 0.9659258262890683122, 1.000000000000000000, 0.9659258262890683122, 1.000000000000000000, 0.9659258262890683122, 1.000000000000000000, 0.9659258262890683122, 1.000000000000000000, 0.9659258262890683122, 1.000000000000000000, 0.9659258262890683122, 1.000000000000000000, 0.9659258262890683122, 1.000000000000000000, 0.9659258262890683122, 1.000000000000000000, 0.9659258262890683122, 1.000000000000000000, 0.9659258262890683122, 1.000000000000000000, 0.9659258262890683122, 1.000000000000000000, 0.9659258262890683122, 1.000000000000000000, 0.9659258262890683122, 1.000000000000000000, 0.9659258262890683122, 1.000000000000000000, 0.9659258262890683122, 1.000000000000000000, 0.9659258262890683122, 1.000000000000000000, 0.9659258262890683122, 1.000000000000000000, 0.9659258262890683122, 1.000000000000000000, 0.9659258262890683122, 1.000000000000000000, 0.9659258262890683122, 1.000000000000000000, 0.9659258262890683122, 1.000000000000000000, 0.9659258262890683122, 1.000000000000000000, 0.9659258262890683122, 1.000000000000000000, 0.9659258262890683122, 1.000000000000000000, 0.9659258262890683122, 1.000000000000000000, 0.9659258262890683122, 1.000000000000000000, 0.9659258262890683122, 1.000000000000000000, 0.9659258262890683122, 1.000000000000000000, 0.9659258262890683122, 1.000000000000000000, 0.9659258262890683122, 1.000000000000000000, 0.9659258262890683122, 1.000000000000000000, 0.9659258262890683122, 1.000000000000000000, 0.9659258262890683122, 1.000000000000000000, 0.9659258262890683122, 1.000000000000000000, 0.9659258262890683122, 1.000000000000000000, 0.9659258262890683122, 1.000000000000000000, 0.9659258262890683122, 1.000000000000000000, 0.9659258262890683122, 1.000000000000000000, 0.9659258262890683122, 1.000000000000000000, 0.9659258262890683122, 1.000000000000000000, 0.9659258262890683122, 1.000000000000000000, 0.9659258262890683122, 1.000000000000000000, 0.9659258262890683122, 1.000000000000000000, 0.9659258262890683122, 1.000000000000000000, 0.9659258262890683122, 1.000000000000000000, 0.9659258262890683122, 1.000000000000000000, 0.9659258262890683122, 1.000000000000000000, 0.9659258262890683122, 1.000000000000000000, 0.9659258262890683122, 1.000000000000000000, 0.9659258262890683122, 1.000000000000000000, 0.9659258262890683122, 1.000000000000000000, 0.9659258262890683122, 1.000000000000000000, 0.9659258262890683122, 1.000000000000000000, 0.9659258262890683122, 1.000000000000000000, 0.9659258262890683122, 1.000000000000000000, 0.9659258262890683122, 1.000000000000000000, 0.9659258262890683122, 1.000000000000000000, 0.9659258262890683122, 1.000000000000000000, 0.9659258262890683122, 1.000000000000000000, 0.9659258262890683122, 1.000000000000000000, 0.9659258262890683122, 1.000000000000000000, 0.9659258262890683122, 1.000000000000000000, 0.9659258262890683122, 1.000000000000000000, 0.9659258262890683122, 1.000000000000000000, 0.9659258262890683122, 1.000000000000000000, 0.9659258262890683122, 1.000000000000000000, 0.9659258262890683122, 1.000000000000000000, 0.9659258262890683122, 1.000000000000000000, 0.9659258262890683122, 1.000000000000000000, 0.9659258262890683122, 1.000000000000000000, 0.9659258262890683122, 1.000000000000000000, 0.9659258262890683122, 1.000000000000000000, 0.9659258262890683122, 1.000000000000000000, 0.9659258262890683122, 1.000000000000000000, 0.9659258262890683122, 1.000000000000000000, 0.9659258262890683122, 1.000000000000000000, 0.9659258262890683122, 1.000000000000000000, 0.9659258262890683122, 1.000000000000000000, 0.9659258262890683122, 1.000000000000000000, 0.9659258262890683122, 1.000000000000000000, 0.9659258262890683122, 1.000000000000000000, 0.9659258262890683122, 1.000000000000000000, 0.9659258262890683122, 1.000000000000000000, 0.9659258262890683122, 1.000000000000000000, 0.9659258262890683122, 1.000000000000000000, 0.9659258262890683122, 1.000000000000000000, 0.9659258262890683122, 1.000000000000000000, 0.9659258262890683122, 1.000000000000000000, 0.9659258262890683122, 1.000000000000000000, 0.9659258262890683122, 1.000000000000000000, 0.9659258262890683122, 1.000000000000000000, 0.9659258262890683122, 1.000000000000000000, 0.9659258262890683122, 1.000000000000000000, 0.9659258262890683122, 1.000000000000000000, 0.9659258262890683122, 1.000000000000000000, 0.9659258262890683122, 1.000000000000000000, 0.9659258262890683122, 1.000000000000000000, 0.9659258262890683122, 1.000000000000000000, 0.9659258262890683122, 1.000000000000000000, 0.9659258262890683122, 1.000000000000000000, 0.9659258262890683122, 1.000000000000000000, 0.9659258262890683122, 1.000000000000000000, 0.9659258262890683122, 1.000000000000000000, 0.9659258262890683122, 1.000000000000000000, 0.9659258262890683122, 1.000000000000000000, 0.9659258262890683122, 1.000000000000000000, 0.9659258262890683122, 1.000000000000000000, 0.9659258262890683122, 1.000000000000000000, 0.9659258262890683122, 1.000000000000000000, 0.9659258262890683122, 1.000000000000000000, 0.9659258262890683122, 1.000000000000000000, 0.9659258262890683122, 1.000000000000000000, 0.9659258262890683122, 1.000000000000000000, 0.9659258262890683122, 1.000000000000000000, 0.9659258262890683122, 1.000000000000000000, 0.9659258262890683122, 1.000000000000000000, 0.9659258262890683122, 1.000000000000000000, 0.9659258262890683122, 1.000000000000000000, 0.9659258262890683122, 1.000000000000000000, 0.9659258262890683122, 1.000000000000000000, 0.9659258262890683122, 1.000000000000000000, 0.9659258262890683122, 1.000000000000000000, 0.9659258262890683122, 1.000000000000000000, 0.9659258262890683122, 1.000000000000000000, 0.9659258262890683122, 1.000000000000000000, 0.9659258262890683122, 1.000000000000000000, 0.9659258262890683122, 1.000000000000000000, 0.9659258262890683122, 1.000000000000000000, 0.9659258262890683122, 1.000000000000000000, 0.9659258262890683122, 1.000000000000000000, 0.9659258262890683122, 1.000000000000000000, 0.9659258262890683122, 1.000000000000000000, 0.9659258262890683122, 1.000000000000000000, 0.9659258262890683122, 1.000000000000000000, 0.9659258262890683122, 1.000000000000000000, 0.9659258262890683122, 1.000000000000000000, 0.9659258262890683122, 1.000000000000000000, 0.9659258262890683122, 1.000000000000000000, 0.9659258262890683122, 1.000000000000000000, 0.9659258262890683122, 1.000000000000000000, 0.9659258262890683122, 1.000000000000000000, 0.9659258262890683122, 1.000000000000000000, 0.9659258262890683122, 1.000000000000000000, 0.9659258262890683122, 1.000000000000000000, 0.9659258262890683122, 1.000000000000000000, 0.9659258262890683122, 1.000000000000000000, 0.9659258262890683122, 1.000000000000000000, 0.9659258262890683122, 1.000000000000000000, 0.9659258262890683122, 1.000000000000000000, 0.9659258262890683122, 1.000000000000000000, 0.9659258262890683122, 1.000000000000000000, 0.9659258262890683122, 1.000000000000000000, 0.9659258262890683122, 1.000000000000000000, 0.9659258262890683122, 1.000000000000000000, 0.9659258262890683122, 1.000000000000000000, 0.9659258262890683122, 1.000000000000000000, 0.9659258262890683122, 1.000000000000000000, 0.9659258262890683122, 1.000000000000000000, 0.9659258262890683122, 1.000000000000000000, 0.9659258262890683122, 1.000000000000000000) ) ) 
 REPRESENTATION_ITEM ( '' )  SURFACE ( )  );
#70094 = CARTESIAN_POINT ( 'NONE',  ( 15.44008868035555260, 49.73035201082150536, 9.422509992056143702 ) ) ;
#70095 = CARTESIAN_POINT ( 'NONE',  ( -0.8801773607111009756, 53.06368534415484106, 1.068504757029289695E-15 ) ) ;
#70096 = CARTESIAN_POINT ( 'NONE',  ( 14.17193700899790265, -0.03417435944610275333, -1.489530601564018175 ) ) ;
#70097 = CARTESIAN_POINT ( 'NONE',  ( 10.32896413005680181, 11.77164270246085209, 5.963430220938278126 ) ) ;
#70098 = CARTESIAN_POINT ( 'NONE',  ( 19.42250999205614193, 10.14701867748816966, 5.440088680355555262 ) ) ;
#70099 = CARTESIAN_POINT ( 'NONE',  ( 12.63842701281683034, 47.46726448433412315, 9.846743663894596210 ) ) ;
#70101 = CARTESIAN_POINT ( 'NONE',  ( 19.84674366389459266, 23.71726448433412315, -2.638427012816827677 ) ) ;
#70100 = CARTESIAN_POINT ( 'NONE',  ( 10.00000000000000000, 16.81368534415483751, -10.88017736071110342 ) ) ;
#70102 = CARTESIAN_POINT ( 'NONE',  ( 10.00000000000000178, 25.37363466993041783, 12.81628187352647608 ) ) ;
#70103 = ORIENTED_EDGE ( 'NONE', *, *, #2386, .T. ) ;
#70104 = CARTESIAN_POINT ( 'NONE',  ( 2.035157376598822676, 42.43868534415483396, -7.964842623401177768 ) ) ;
#70106 = CARTESIAN_POINT ( 'NONE',  ( -12.79413655343702239, 0.2301508429231322317, 7.715718893782787191 ) ) ;
#70105 = CARTESIAN_POINT ( 'NONE',  ( 16.40814093676324603, 12.45696800326375353, -11.09922568453594671 ) ) ;
#70107 = CARTESIAN_POINT ( 'NONE',  ( 17.96484262340118221, 11.18868534415483929, -7.964842623401177768 ) ) ;
#70108 = CARTESIAN_POINT ( 'NONE',  ( 7.084665262690076126, 44.10535201082151247, 10.88017736071109987 ) ) ;
#70109 = CARTESIAN_POINT ( 'NONE',  ( -0.3689425029237881626, 57.42874883491397497, 10.36894250292379027 ) ) ;
#70110 = CARTESIAN_POINT ( 'NONE',  ( 2.791683348922237240, 25.38393115100078390, -7.208316651077763204 ) ) ;
#70111 = CARTESIAN_POINT ( 'NONE',  ( 20.88017736071110164, 60.35535201082151957, 2.915334737309930979 ) ) ;
#70112 = CARTESIAN_POINT ( 'NONE',  ( -9.024359497401759356, 75.07164295747612925, 2.900000000000000355 ) ) ;
#70113 = CARTESIAN_POINT ( 'NONE',  ( 13.79529636645031943, 10.34541550158063394, -14.16423886937409904 ) ) ;
#70114 = EDGE_CURVE ( 'NONE', #10914, #89676, #87577, .T. ) ;
#70115 = UNCERTAINTY_MEASURE_WITH_UNIT (LENGTH_MEASURE( 1.000000000000000082E-05 ), #15972, 'distance_accuracy_value', 'NONE');
#70116 = FILL_AREA_STYLE_COLOUR ( '', #33936 ) ;
#70117 = LINE ( 'NONE', #18104, #34414 ) ;
#70119 = EDGE_LOOP ( 'NONE', ( #74126, #62356, #24547, #55399 ) ) ;
#70118 = EDGE_CURVE ( 'NONE', #42348, #24535, #49222, .T. ) ;
#70120 = CARTESIAN_POINT ( 'NONE',  ( 6.204703633549690345, 40.76208216824731778, -14.16423886937410259 ) ) ;
#70121 = CARTESIAN_POINT ( 'NONE',  ( 6.204703633549690345, 35.76208216824729647, -14.16423886937410259 ) ) ;
#70122 = CARTESIAN_POINT ( 'NONE',  ( -0.8801773607110991993, 67.85535201082151957, -2.915334737309923874 ) ) ;
#70123 = CARTESIAN_POINT ( 'NONE',  ( 0.1532563361054082862, 66.21726448433413736, 2.638427012816831674 ) ) ;
#70124 = CYLINDRICAL_SURFACE ( 'NONE', #84990, 0.5000000000000004441 ) ;
#70126 = CARTESIAN_POINT ( 'NONE',  ( 21.09922568453595559, 37.04030133659708923, -6.408140936763230044 ) ) ;
#70125 = CARTESIAN_POINT ( 'NONE',  ( 19.42250999205614548, 60.98035201082151247, -5.440088680355545492 ) ) ;
#70127 = CARTESIAN_POINT ( 'NONE',  ( 17.08211943468705130, 28.47041550158063572, 12.26659068614894998 ) ) ;
#70129 = EDGE_CURVE ( 'NONE', #243, #67764, #41531, .T. ) ;
#70128 = B_SPLINE_CURVE_WITH_KNOTS ( 'NONE', 3,
 ( #78073, #85581, #55578, #17095, #40078, #1114 ),
 .UNSPECIFIED., .F., .F.,
 ( 4, 2, 4 ),
 ( 3.409110551496212006E-05, 0.0004400426677368009373, 0.0008459942299586397816 ),
 .UNSPECIFIED. ) ;
#70130 = CARTESIAN_POINT ( 'NONE',  ( 19.42250999205614548, 30.98035201082150536, -5.440088680355545492 ) ) ;
#70131 = EDGE_CURVE ( 'NONE', #69579, #13031, #58128, .T. ) ;
#70132 = CARTESIAN_POINT ( 'NONE',  ( 17.96484262340118221, 29.93868534415484106, 7.964842623401181321 ) ) ;
#70133 = DIRECTION ( 'NONE',  ( -0.000000000000000000, -0.000000000000000000, 1.000000000000000000 ) ) ;
#70134 = CARTESIAN_POINT ( 'NONE',  ( 2.791683348922237240, 0.3839311510007847872, -7.208316651077763204 ) ) ;
#70135 = PRESENTATION_LAYER_ASSIGNMENT (  '', '', ( #14244 ) ) ;
#70136 = CARTESIAN_POINT ( 'NONE',  ( 2.638427012816835227, -12.53273551566588395, 9.846743663894590881 ) ) ;
#70137 = ORIENTED_EDGE ( 'NONE', *, *, #8919, .F. ) ;
#70138 = CARTESIAN_POINT ( 'NONE',  ( -13.82192141328807011, 3.982798640990670655E-16, -4.382292601468863680 ) ) ;
#70139 = VERTEX_POINT ( 'NONE', #73059 ) ;
#70140 = LINE ( 'NONE', #63598, #33282 ) ;
#70141 = ORIENTED_EDGE ( 'NONE', *, *, #9036, .T. ) ;
#70142 = CARTESIAN_POINT ( 'NONE',  ( 2.917880565312948704, 2.637082168247300906, 12.26659068614894643 ) ) ;
#70144 = CARTESIAN_POINT ( 'NONE',  ( 7.084665262690076126, 7.022018677488170546, -10.88017736071110164 ) ) ;
#70143 = CARTESIAN_POINT ( 'NONE',  ( 24.16423886937410614, 64.30374883491396076, 8.672049930838204340E-16 ) ) ;
#70146 = CARTESIAN_POINT ( 'NONE',  ( 1.472469842513823179, 60.59226448433412315, -4.923371831947296329 ) ) ;
#70145 = CARTESIAN_POINT ( 'NONE',  ( 7.361572987183169658, 39.96726448433411605, -9.846743663894592657 ) ) ;
#70147 = EDGE_CURVE ( 'NONE', #79425, #41646, #96081, .T. ) ;
#70148 =( NAMED_UNIT ( * ) PLANE_ANGLE_UNIT ( ) SI_UNIT ( $, .RADIAN. ) );
#70149 = COLOUR_RGB ( '', 0.40784314, 0.44705882, 0.49803922) ;
#70150 = CARTESIAN_POINT ( 'NONE',  ( 34.56412365047464874, 29.50000000000000000, 10.00000000000000000 ) ) ;
#70151 = CARTESIAN_POINT ( 'NONE',  ( 22.81628187352648496, 1.831968003263753753, -3.434112377981050290 ) ) ;
#70152 = ORIENTED_EDGE ( 'NONE', *, *, #2197, .T. ) ;
#70153 = CARTESIAN_POINT ( 'NONE',  ( 13.79529636645030344, 48.26208216824728936, 14.16423886937410614 ) ) ;
#70154 = ORIENTED_EDGE ( 'NONE', *, *, #18708, .F. ) ;
#70155 = EDGE_CURVE ( 'NONE', #31263, #24281, #3259, .T. ) ;
#70156 = CARTESIAN_POINT ( 'NONE',  ( 20.36894250292379738, 39.92874883491396787, -10.36894250292379027 ) ) ;
#70157 = ORIENTED_EDGE ( 'NONE', *, *, #14925, .F. ) ;
#70158 = CARTESIAN_POINT ( 'NONE',  ( -0.8801773607110991993, 17.85535201082150536, -2.915334737309923874 ) ) ;
#70159 = CARTESIAN_POINT ( 'NONE',  ( 18.72515096720568195, 21.07228050351032422, -6.500000000000018652 ) ) ;
#70160 = CARTESIAN_POINT ( 'NONE',  ( 4.559911319644449179, 43.89701867748816966, 9.422509992056141925 ) ) ;
#70161 = CARTESIAN_POINT ( 'NONE',  ( 5.076628168052704559, 55.17559781766745175, -8.527530157486179263 ) ) ;
#70162 = CARTESIAN_POINT ( 'NONE',  ( 4.559911319644449179, 37.23035201082150536, -9.422509992056141925 ) ) ;
#70163 = CARTESIAN_POINT ( 'NONE',  ( -0.3289641300568005855, 64.27164270246085209, -5.963430220938281678 ) ) ;
#70164 = CARTESIAN_POINT ( 'NONE',  ( 7.084665262690076126, 67.02201867748817676, -10.88017736071110164 ) ) ;
#70165 = CARTESIAN_POINT ( 'NONE',  ( -0.8801773607111009756, 33.06368534415484106, 1.068504757029289695E-15 ) ) ;
#70166 = TOROIDAL_SURFACE ( 'NONE', #19114, 14.49999999999999822, 0.5000000000000000000 ) ;
#70168 = ORIENTED_EDGE ( 'NONE', *, *, #94080, .T. ) ;
#70167 = CYLINDRICAL_SURFACE ( 'NONE', #74459, 15.00000000000000000 ) ;
#70169 = CARTESIAN_POINT ( 'NONE',  ( 0.1532563361054083140, 6.008931151000784787, 1.131784320476157264E-15 ) ) ;
#70170 = CARTESIAN_POINT ( 'NONE',  ( -3.521809513897764532, -0.8352226969157688918, 2.749999999999798828 ) ) ;
#70171 = VERTEX_POINT ( 'NONE', #63593 ) ;
#70172 = CARTESIAN_POINT ( 'NONE',  ( 19.84674366389459266, 48.30059781766745175, 2.638427012816836559 ) ) ;
#70173 = SURFACE_STYLE_FILL_AREA ( #47661 ) ;
#70174 = DIRECTION ( 'NONE',  ( 0.000000000000000000, 0.000000000000000000, -1.000000000000000000 ) ) ;
#70175 = VECTOR ( 'NONE', #93085, 1000.000000000000000 ) ;
#70176 = CARTESIAN_POINT ( 'NONE',  ( 12.63842701281683922, 64.55059781766745175, -9.846743663894590881 ) ) ;
#70177 = CARTESIAN_POINT ( 'NONE',  ( -0.8801773607111009756, 53.06368534415484106, 1.068504757029289695E-15 ) ) ;
#70178 = CARTESIAN_POINT ( 'NONE',  ( 2.791683348922240793, 51.63393115100078745, 7.208316651077764092 ) ) ;
#70179 = CARTESIAN_POINT ( 'NONE',  ( 10.00000000000000000, 50.55374883491396787, -14.16423886937410082 ) ) ;
#70180 = CARTESIAN_POINT ( 'NONE',  ( 10.00000000000000000, 54.75893115100078745, -9.846743663894594434 ) ) ;
#70181 = ORIENTED_EDGE ( 'NONE', *, *, #82084, .T. ) ;
#70182 = CARTESIAN_POINT ( 'NONE',  ( 1.816707512666851931, 5.102906685120229824, -6.499999999999991118 ) ) ;
#70183 = CARTESIAN_POINT ( 'NONE',  ( 0.1532563361054083140, 26.00893115100078745, 1.131784320476157264E-15 ) ) ;
#70184 = CARTESIAN_POINT ( 'NONE',  ( -1.099225684535947600, 49.54030133659708923, 6.408140936763237150 ) ) ;
#70185 = CARTESIAN_POINT ( 'NONE',  ( 18.52753015748618282, 63.92559781766745886, -4.923371831947291888 ) ) ;
#70186 = CARTESIAN_POINT ( 'NONE',  ( -0.8801773607111008646, 53.27201867748816966, 2.915334737309923430 ) ) ;
#70187 = CARTESIAN_POINT ( 'NONE',  ( 6.574847571008442415, -50.89175608690136698, -2.750000000000000888 ) ) ;
#70188 = ORIENTED_EDGE ( 'NONE', *, *, #34546, .T. ) ;
#70189 = CARTESIAN_POINT ( 'NONE',  ( 6.204703633549690345, 62.84541550158063927, 14.16423886937410082 ) ) ;
#70190 = CARTESIAN_POINT ( 'NONE',  ( 2.035157376598822676, 27.43868534415483396, -7.964842623401177768 ) ) ;
#70192 = CARTESIAN_POINT ( 'NONE',  ( 0.5774900079438607392, 63.48035201082149825, 5.440088680355550821 ) ) ;
#70191 = CARTESIAN_POINT ( 'NONE',  ( 3.591859063236761518, 9.956968003263753531, 11.09922568453594849 ) ) ;
#70193 = DIRECTION ( 'NONE',  ( -0.000000000000000000, -1.000000000000000000, -0.000000000000000000 ) ) ;
#70194 = SURFACE_STYLE_FILL_AREA ( #78177 ) ;
#70195 = CARTESIAN_POINT ( 'NONE',  ( 19.72487221294571569, 45.71833443783938122, -6.499999999999989342 ) ) ;
#70197 = DIRECTION ( 'NONE',  ( -1.000000000000000000, 0.000000000000000000, -0.000000000000000000 ) ) ;
#70196 = CARTESIAN_POINT ( 'NONE',  ( -0.8801773607111008646, 48.27201867748816966, 2.915334737309923430 ) ) ;
#70198 = EDGE_CURVE ( 'NONE', #47627, #51188, #82064, .T. ) ;
#70199 = CARTESIAN_POINT ( 'NONE',  ( 14.92337183194729988, 39.34226448433412315, -8.527530157486177487 ) ) ;
#70200 = CARTESIAN_POINT ( 'NONE',  ( 14.92337183194729988, 4.342264484334117824, -8.527530157486177487 ) ) ;
#70201 = CARTESIAN_POINT ( 'NONE',  ( -2.915334737309917656, -35.89464798917849464, 10.88017736071110164 ) ) ;
#70202 = CARTESIAN_POINT ( 'NONE',  ( 19.38216949554541202, 5.998634669930420493, 9.382169495545424454 ) ) ;
#70204 = CARTESIAN_POINT ( 'NONE',  ( -20.19000000000001194, 92.00000000000000000, -10.09898361729590199 ) ) ;
#70203 = CARTESIAN_POINT ( 'NONE',  ( 2.035157376598822676, 17.43868534415483751, -7.964842623401177768 ) ) ;
#70205 = DIRECTION ( 'NONE',  ( -0.000000000000000000, 0.000000000000000000, 1.000000000000000000 ) ) ;
#70206 = EDGE_CURVE ( 'NONE', #76154, #62128, #61679, .T. ) ;
#70207 = CARTESIAN_POINT ( 'NONE',  ( 22.26659068614895176, 39.72041550158063217, -7.082119434687042414 ) ) ;
#70208 = CARTESIAN_POINT ( 'NONE',  ( 2.917880565312950480, 25.97041550158063572, -12.26659068614894821 ) ) ;
#70209 = CARTESIAN_POINT ( 'NONE',  ( -4.164238869374098151, 66.59541550158060375, -3.795296366450310543 ) ) ;
#70210 = CARTESIAN_POINT ( 'NONE',  ( 2.791683348922240793, 31.63393115100078745, 7.208316651077764092 ) ) ;
#70211 = CARTESIAN_POINT ( 'NONE',  ( 17.20831665107776587, 22.88393115100078745, 7.208316651077764980 ) ) ;
#70212 = CARTESIAN_POINT ( 'NONE',  ( 10.00000000000000178, 19.31368534415484106, 10.88017736071110342 ) ) ;
#70213 = B_SPLINE_CURVE_WITH_KNOTS ( 'NONE', 3,
 ( #36849, #66340, #96878, #67340, #13853, #5856 ),
 .UNSPECIFIED., .F., .F.,
 ( 4, 2, 4 ),
 ( 3.409110551496207940E-05, 0.0004400426677368021299, 0.0008459942299586421669 ),
 .UNSPECIFIED. ) ;
#70214 = ORIENTED_EDGE ( 'NONE', *, *, #36318, .T. ) ;
#70215 = CARTESIAN_POINT ( 'NONE',  ( 0.1532563361054100626, 40.80059781766745886, -2.638427012816831230 ) ) ;
#70216 = CARTESIAN_POINT ( 'NONE',  ( 0.5774900079438607392, 28.48035201082150891, 5.440088680355550821 ) ) ;
#70217 = CARTESIAN_POINT ( 'NONE',  ( 12.63842701281683922, 59.55059781766744464, -9.846743663894590881 ) ) ;
#70219 = CARTESIAN_POINT ( 'NONE',  ( -1.926860441876564023, 17.87045670184113533, 3.195792623639529761 ) ) ;
#70218 = CARTESIAN_POINT ( 'NONE',  ( 10.00000000000000000, 15.55374883491396787, -14.16423886937410082 ) ) ;
#70220 = LINE ( 'NONE', #55195, #32755 ) ;
#70221 = UNCERTAINTY_MEASURE_WITH_UNIT (LENGTH_MEASURE( 1.000000000000000082E-05 ), #39650, 'distance_accuracy_value', 'NONE');
#70222 = CARTESIAN_POINT ( 'NONE',  ( 19.84674366389459621, 8.508931151000785675, 7.409399052514197653E-17 ) ) ;
#70223 = CARTESIAN_POINT ( 'NONE',  ( 3.591859063236761518, 44.95696800326376064, 11.09922568453594849 ) ) ;
#70224 = CARTESIAN_POINT ( 'NONE',  ( 1.472469842513823179, 51.42559781766745886, 4.923371831947296329 ) ) ;
#70225 = ORIENTED_EDGE ( 'NONE', *, *, #87350, .F. ) ;
#70226 = CARTESIAN_POINT ( 'NONE',  ( 8.991946320728366970, -4.139779132962734032, -3.750000000000000000 ) ) ;
#70227 = CIRCLE ( 'NONE', #74997, 0.2500000000000002220 ) ;
#70228 = CARTESIAN_POINT ( 'NONE',  ( 19.42250999205614548, 5.980352010821504471, -5.440088680355545492 ) ) ;
#70229 = CARTESIAN_POINT ( 'NONE',  ( 20.88017736071110164, 50.35535201082151247, 2.915334737309930979 ) ) ;
#70230 = CARTESIAN_POINT ( 'NONE',  ( -4.164238869374099039, 16.80374883491396787, 8.674139862899312516E-16 ) ) ;
#70231 = CARTESIAN_POINT ( 'NONE',  ( 2.035157376598822676, 62.43868534415483396, -7.964842623401177768 ) ) ;
#70232 = CARTESIAN_POINT ( 'NONE',  ( 18.52753015748617571, 33.09226448433411605, 4.923371831947298993 ) ) ;
#70233 = CARTESIAN_POINT ( 'NONE',  ( -0.8801773607110991993, 22.85535201082150181, -2.915334737309923874 ) ) ;
#70234 = DIRECTION ( 'NONE',  ( 1.000000000000000000, 0.000000000000000000, 0.000000000000000000 ) ) ;
#70235 = CARTESIAN_POINT ( 'NONE',  ( 19.84674366389459266, 58.71726448433411605, -2.638427012816827677 ) ) ;
#70236 = STYLED_ITEM ( 'NONE', ( #74306 ), #22494 ) ;
#70237 = AXIS2_PLACEMENT_3D ( 'NONE', #19952, #25990, #27451 ) ;
#70238 = CARTESIAN_POINT ( 'NONE',  ( 17.39651004071841456, 7.935752660568278216, 6.500000000000003553 ) ) ;
#70239 = UNCERTAINTY_MEASURE_WITH_UNIT (LENGTH_MEASURE( 1.000000000000000082E-05 ), #33948, 'distance_accuracy_value', 'NONE');
#70241 = ORIENTED_EDGE ( 'NONE', *, *, #44876, .T. ) ;
#70240 = ADVANCED_FACE ( 'NONE', ( #14561 ), #6064, .F. ) ;
#70242 = EDGE_LOOP ( 'NONE', ( #44165, #44911, #88499, #53283 ) ) ;
#70243 = CARTESIAN_POINT ( 'NONE',  ( 0.2751277870542909731, 62.28217586085237656, -6.499999999999992006 ) ) ;
#70244 = CARTESIAN_POINT ( 'NONE',  ( 8.880000000000020322, 80.32179676972448590, -4.000000000000000000 ) ) ;
#70245 = CARTESIAN_POINT ( 'NONE',  ( 2.917880565312950480, 0.9704155015806342766, -12.26659068614894821 ) ) ;
#70246 = CARTESIAN_POINT ( 'NONE',  ( 5.076628168052703671, 46.84226448433412315, 8.527530157486179263 ) ) ;
#70247 = CARTESIAN_POINT ( 'NONE',  ( 5.076628168052703671, 16.84226448433411960, 8.527530157486179263 ) ) ;
#70248 = CARTESIAN_POINT ( 'NONE',  ( 3.591859063236763294, 58.29030133659708923, -11.09922568453595026 ) ) ;
#70250 = CARTESIAN_POINT ( 'NONE',  ( 12.63842701281683922, 44.55059781766745175, -9.846743663894590881 ) ) ;
#70249 = CARTESIAN_POINT ( 'NONE',  ( 12.91533473730992121, 24.52201867748816966, 10.88017736071110164 ) ) ;
#70251 = FACE_OUTER_BOUND ( 'NONE', #15180, .T. ) ;
#70252 = CARTESIAN_POINT ( 'NONE',  ( -4.164238869374098151, 36.59541550158063217, -3.795296366450310543 ) ) ;
#70253 = EDGE_CURVE ( 'NONE', #85496, #49230, #42871, .T. ) ;
#70254 = CARTESIAN_POINT ( 'NONE',  ( 6.204703633549690345, 57.84541550158063927, 14.16423886937410082 ) ) ;
#70255 = CARTESIAN_POINT ( 'NONE',  ( -3.750000000000000000, 36.75000000000000000, 2.750000000000000000 ) ) ;
#70256 = CARTESIAN_POINT ( 'NONE',  ( -10.97221242069369218, 14.99999999999805844, 9.670525607395029866 ) ) ;
#70257 = CARTESIAN_POINT ( 'NONE',  ( 20.88017736071110875, 55.77201867748816966, -2.915334737309920765 ) ) ;
#70258 = CARTESIAN_POINT ( 'NONE',  ( 2.791683348922237240, 20.38393115100078745, -7.208316651077763204 ) ) ;
#70259 = CARTESIAN_POINT ( 'NONE',  ( -4.537879770860196338, -17.56524742836564101, 3.750000000002418954 ) ) ;
#70260 = ORIENTED_EDGE ( 'NONE', *, *, #97473, .T. ) ;
#70261 = DIRECTION ( 'NONE',  ( 0.9998643952135762847, -0.01646788341559294114, 2.168110298962930704E-16 ) ) ;
#70262 = ORIENTED_EDGE ( 'NONE', *, *, #13781, .T. ) ;
#70263 = CARTESIAN_POINT ( 'NONE',  ( 0.1532563361054100626, 10.80059781766745175, -2.638427012816831230 ) ) ;
#70264 = ORIENTED_EDGE ( 'NONE', *, *, #22055, .F. ) ;
#70265 = CARTESIAN_POINT ( 'NONE',  ( 6.204703633549690345, 20.76208216824730357, -14.16423886937410259 ) ) ;
#70266 = CARTESIAN_POINT ( 'NONE',  ( 12.63842701281683922, 24.55059781766745175, -9.846743663894590881 ) ) ;
#70267 = CARTESIAN_POINT ( 'NONE',  ( 17.96484262340118221, 39.93868534415484106, 7.964842623401181321 ) ) ;
#70268 = CARTESIAN_POINT ( 'NONE',  ( 14.37657372141816481, 1.111307226797641650E-15, 2.693041920167452918 ) ) ;
#70269 = VERTEX_POINT ( 'NONE', #5076 ) ;
#70270 = CARTESIAN_POINT ( 'NONE',  ( 4.559911319644449179, 38.89701867748817676, 9.422509992056141925 ) ) ;
#70271 = CARTESIAN_POINT ( 'NONE',  ( 14.62129639376010815, -3.239901023247697614E-15, 0.3552502084986245423 ) ) ;
#70272 = CARTESIAN_POINT ( 'NONE',  ( 3.469446951953614189E-15, 0.3736346699304282648, 12.81628187352647608 ) ) ;
#70273 = VERTEX_POINT ( 'NONE', #35563 ) ;
#70274 = CARTESIAN_POINT ( 'NONE',  ( 4.559911319644449179, 42.23035201082151247, -9.422509992056141925 ) ) ;
#70275 = CARTESIAN_POINT ( 'NONE',  ( 24.16423886937410614, 9.303748834913967869, 8.672049930838204340E-16 ) ) ;
#70276 = EDGE_LOOP ( 'NONE', ( #5598, #8125, #21186, #6443 ) ) ;
#70277 = EDGE_CURVE ( 'NONE', #339, #33071, #31653, .T. ) ;
#70278 = VERTEX_POINT ( 'NONE', #13057 ) ;
#70279 = CARTESIAN_POINT ( 'NONE',  ( 22.81628187352647785, 26.41530133659708923, 3.434112377981063169 ) ) ;
#70280 = CARTESIAN_POINT ( 'NONE',  ( 7.361572987183170547, 12.05059781766744997, 9.846743663894590881 ) ) ;
#70281 = CARTESIAN_POINT ( 'NONE',  ( 10.00000000000000000, 1.813685344154837731, -10.88017736071110342 ) ) ;
#70282 = CARTESIAN_POINT ( 'NONE',  ( 6.565887622018943937, 43.08196800326374643, -12.81628187352647608 ) ) ;
#70283 = DIRECTION ( 'NONE',  ( -0.000000000000000000, 1.000000000000000000, -0.000000000000000000 ) ) ;
#70284 = CARTESIAN_POINT ( 'NONE',  ( 5.076628168052703671, 11.84226448433411960, 8.527530157486179263 ) ) ;
#70285 = CARTESIAN_POINT ( 'NONE',  ( 20.88017736071110875, 25.77201867748816966, -2.915334737309920765 ) ) ;
#70286 = B_SPLINE_CURVE_WITH_KNOTS ( 'NONE', 3,
 ( #52485, #18, #53467, #82496 ),
 .UNSPECIFIED., .F., .F.,
 ( 4, 4 ),
 ( 0.000000000000000000, 0.002657014572711347607 ),
 .UNSPECIFIED. ) ;
#70287 = VERTEX_POINT ( 'NONE', #37557 ) ;
#70288 = CARTESIAN_POINT ( 'NONE',  ( 0.000000000000000000, 0.000000000000000000, 0.000000000000000000 ) ) ;
#70289 = CARTESIAN_POINT ( 'NONE',  ( 2.035157376598822676, 62.43868534415483396, -7.964842623401177768 ) ) ;
#70290 = CARTESIAN_POINT ( 'NONE',  ( 2.393480905993059515, 14.63595249122789177, 14.80781041047753632 ) ) ;
#70291 = CARTESIAN_POINT ( 'NONE',  ( 0.000000000000000000, 0.000000000000000000, 0.000000000000000000 ) ) ;
#70292 = CARTESIAN_POINT ( 'NONE',  ( 7.084665262690076126, 59.10535201082150536, 10.88017736071109987 ) ) ;
#70293 = CARTESIAN_POINT ( 'NONE',  ( 10.00000000000000000, 7.873634669930421381, -12.81628187352647608 ) ) ;
#70294 = LINE ( 'NONE', #40281, #78634 ) ;
#70295 = AXIS2_PLACEMENT_3D ( 'NONE', #93575, #54095, #92591 ) ;
#70296 = CARTESIAN_POINT ( 'NONE',  ( 10.00000000000000178, 32.25893115100078745, 9.846743663894594434 ) ) ;
#70297 = CARTESIAN_POINT ( 'NONE',  ( 21.09922568453594849, 61.20696800326376064, 6.408140936763242479 ) ) ;
#70298 = CARTESIAN_POINT ( 'NONE',  ( -2.266590686148945544, 1.387082168247301128, -7.082119434687050408 ) ) ;
#70299 = CARTESIAN_POINT ( 'NONE',  ( 1.472469842513823179, 16.42559781766745175, 4.923371831947296329 ) ) ;
#70300 =( BOUNDED_CURVE ( )  B_SPLINE_CURVE ( 2, ( #28852, #36871, #21877, #14375, #35873, #13875, #44843, #44357, #35381 ),
 .UNSPECIFIED., .F., .F. ) 
 B_SPLINE_CURVE_WITH_KNOTS ( ( 3, 2, 2, 2, 3 ),
 ( 0.5784801414667655184, 0.5833333333333333703, 0.5888888888888889062, 0.5944444444444444420, 0.5999999999999999778 ),
 .UNSPECIFIED. ) 
 CURVE ( )  GEOMETRIC_REPRESENTATION_ITEM ( )  RATIONAL_B_SPLINE_CURVE ( ( 0.9924735557117673190, 0.9702336695114960330, 1.000000000000000000, 0.9659258262890683122, 1.000000000000000000, 0.9659258262890683122, 1.000000000000000000, 0.9659258262890683122, 1.000000000000000000 ) ) 
 REPRESENTATION_ITEM ( '' )  );
#70301 = CARTESIAN_POINT ( 'NONE',  ( -2.816281873526473856, 19.12363466993042138, 9.499525473075851096E-16 ) ) ;
#70302 = CARTESIAN_POINT ( 'NONE',  ( -7.121361048738320321, -73.24645952185287001, -2.750000000000000444 ) ) ;
#70303 = CARTESIAN_POINT ( 'NONE',  ( 19.42250999205614193, 55.14701867748817676, 5.440088680355555262 ) ) ;
#70304 = AXIS2_PLACEMENT_3D ( 'NONE', #96231, #88213, #27710 ) ;
#70305 = CARTESIAN_POINT ( 'NONE',  ( 10.00000000000000000, 59.75893115100078745, -9.846743663894594434 ) ) ;
#70306 = CARTESIAN_POINT ( 'NONE',  ( -0.1503990784575242878, 29.24884699246888786, -6.262539305110083276 ) ) ;
#70307 = CARTESIAN_POINT ( 'NONE',  ( 19.84674366389459266, 28.71726448433411960, -2.638427012816827677 ) ) ;
#70308 = CARTESIAN_POINT ( 'NONE',  ( 18.52753015748617571, 28.09226448433411960, 4.923371831947298993 ) ) ;
#70309 = CARTESIAN_POINT ( 'NONE',  ( 4.559911319644449179, 17.23035201082150536, -9.422509992056141925 ) ) ;
#70310 = CARTESIAN_POINT ( 'NONE',  ( 19.38216949554541202, 10.99863466993042138, 9.382169495545424454 ) ) ;
#70311 = CARTESIAN_POINT ( 'NONE',  ( 19.84674366389459266, 28.30059781766745886, 2.638427012816836559 ) ) ;
#70312 = SURFACE_STYLE_FILL_AREA ( #63275 ) ;
#70313 = CARTESIAN_POINT ( 'NONE',  ( -8.860528122731230027, 87.38741345285838236, 4.488970891313635470 ) ) ;
#70314 = CARTESIAN_POINT ( 'NONE',  ( 10.00000000000000178, 19.31368534415484106, 10.88017736071110342 ) ) ;
#70315 = DIRECTION ( 'NONE',  ( 0.2211055276381909129, 0.9752498888222635998, -0.000000000000000000 ) ) ;
#70317 = CARTESIAN_POINT ( 'NONE',  ( 10.00000000000000000, 21.81368534415484106, -10.88017736071110342 ) ) ;
#70316 = CARTESIAN_POINT ( 'NONE',  ( 7.361572987183169658, 39.96726448433411605, -9.846743663894592657 ) ) ;
#70318 = CARTESIAN_POINT ( 'NONE',  ( 10.14667048435145169, 4.379817243679289018E-16, -10.35833375027041292 ) ) ;
#70319 = B_SPLINE_CURVE_WITH_KNOTS ( 'NONE', 3,
 ( #39427, #93395, #33368, #78391, #1441, #8910 ),
 .UNSPECIFIED., .F., .F.,
 ( 4, 2, 4 ),
 ( 0.0002800206007755258637, 0.0006862260317143902954, 0.001092431462653254727 ),
 .UNSPECIFIED. ) ;
#70320 = CARTESIAN_POINT ( 'NONE',  ( 10.00000000000000000, 26.81368534415484106, -10.88017736071110342 ) ) ;
#70322 = CARTESIAN_POINT ( 'NONE',  ( -0.1503990784575328643, 20.12777174578613071, 6.262539305110068177 ) ) ;
#70321 = CARTESIAN_POINT ( 'NONE',  ( 0.5774900079438607392, 18.48035201082150536, 5.440088680355550821 ) ) ;
#70323 = CARTESIAN_POINT ( 'NONE',  ( 1.472469842513823179, 20.59226448433411960, -4.923371831947296329 ) ) ;
#70324 = CARTESIAN_POINT ( 'NONE',  ( 10.00000000000000178, 37.25893115100078745, 9.846743663894594434 ) ) ;
#70325 = DIRECTION ( 'NONE',  ( -0.9975640502598243087, 0.06975647374412535795, -0.000000000000000000 ) ) ;
#70326 = CARTESIAN_POINT ( 'NONE',  ( 1.383448333479223358, 7.377183271974286249, -6.499999999999965361 ) ) ;
#70327 = EDGE_CURVE ( 'NONE', #50256, #47024, #47651, .T. ) ;
#70328 = CARTESIAN_POINT ( 'NONE',  ( 2.791683348922237240, 65.38393115100078035, -7.208316651077763204 ) ) ;
#70329 = CARTESIAN_POINT ( 'NONE',  ( 20.36894250292379738, 29.92874883491396432, -10.36894250292379027 ) ) ;
#70330 = CARTESIAN_POINT ( 'NONE',  ( 5.076628168052703671, 41.84226448433411605, 8.527530157486179263 ) ) ;
#70331 = DIRECTION ( 'NONE',  ( 0.000000000000000000, 1.000000000000000000, 0.000000000000000000 ) ) ;
#70332 = ORIENTED_EDGE ( 'NONE', *, *, #90328, .F. ) ;
#70333 = CARTESIAN_POINT ( 'NONE',  ( 2.917880565312948704, 57.63708216824731068, 12.26659068614894643 ) ) ;
#70334 = CARTESIAN_POINT ( 'NONE',  ( 18.52753015748617571, 18.09226448433411960, 4.923371831947298993 ) ) ;
#70336 = CARTESIAN_POINT ( 'NONE',  ( -9.538220187641574199, 88.39559135149089286, -5.063080553068876277 ) ) ;
#70335 = CARTESIAN_POINT ( 'NONE',  ( 2.603489959281590771, 66.58210964143327715, 6.500000000000003553 ) ) ;
#70337 = CARTESIAN_POINT ( 'NONE',  ( 12.91533473730993009, 41.60535201082149825, -10.88017736071109987 ) ) ;
#70338 = CARTESIAN_POINT ( 'NONE',  ( 34.56412365047464874, 11.49999999999999645, 9.500000000000000000 ) ) ;
#70339 = CARTESIAN_POINT ( 'NONE',  ( 7.084665262690076126, 17.02201867748817676, -10.88017736071110164 ) ) ;
#70340 = CARTESIAN_POINT ( 'NONE',  ( 13.43411237798106583, 47.66530133659709634, -12.81628187352647252 ) ) ;
#70341 = CARTESIAN_POINT ( 'NONE',  ( 16.40814093676324603, 12.45696800326375353, -11.09922568453594671 ) ) ;
#70342 = CARTESIAN_POINT ( 'NONE',  ( 2.791683348922237240, 20.38393115100078745, -7.208316651077763204 ) ) ;
#70343 = VERTEX_POINT ( 'NONE', #66054 ) ;
#70344 = CARTESIAN_POINT ( 'NONE',  ( 2.781662917646512463E-16, 22.11937003968011695, 0.000000000000000000 ) ) ;
#70345 = CARTESIAN_POINT ( 'NONE',  ( 1.274849032794305170, 17.55509018479936145, -6.499999999999995559 ) ) ;
#70346 = CARTESIAN_POINT ( 'NONE',  ( 20.36894250292379382, 48.67874883491396076, 10.36894250292379205 ) ) ;
#70347 = CARTESIAN_POINT ( 'NONE',  ( 17.08211943468705840, 30.13708216824730357, -12.26659068614894466 ) ) ;
#70348 = CARTESIAN_POINT ( 'NONE',  ( 20.88017736071110519, 20.56368534415484106, 2.639326808657452039E-16 ) ) ;
#70349 = CARTESIAN_POINT ( 'NONE',  ( 12.91533473730992121, 39.52201867748817676, 10.88017736071110164 ) ) ;
#70350 = CARTESIAN_POINT ( 'NONE',  ( 10.00000000000000178, 70.00000000000000000, 0.000000000000000000 ) ) ;
#70351 = DIRECTION ( 'NONE',  ( -0.000000000000000000, 0.000000000000000000, 1.000000000000000000 ) ) ;
#70352 = CARTESIAN_POINT ( 'NONE',  ( 7.084665262690076126, 69.10535201082151957, 10.88017736071109987 ) ) ;
#70353 = CARTESIAN_POINT ( 'NONE',  ( 19.84674366389459266, 23.30059781766745530, 2.638427012816836559 ) ) ;
#70354 = CARTESIAN_POINT ( 'NONE',  ( -41.94000000000001194, 93.50000000000000000, 9.500000000000000000 ) ) ;
#70355 = CARTESIAN_POINT ( 'NONE',  ( 0.000000000000000000, 0.5000000000000004441, 0.000000000000000000 ) ) ;
#70356 = CARTESIAN_POINT ( 'NONE',  ( 2.791683348922237240, 15.38393115100078212, -7.208316651077763204 ) ) ;
#70357 = CARTESIAN_POINT ( 'NONE',  ( 0.1532563361054100626, 40.80059781766745886, -2.638427012816831230 ) ) ;
#70358 = CARTESIAN_POINT ( 'NONE',  ( -0.8801773607110991993, 7.855352010821504471, -2.915334737309923874 ) ) ;
#70359 = UNCERTAINTY_MEASURE_WITH_UNIT (LENGTH_MEASURE( 1.000000000000000082E-05 ), #48522, 'distance_accuracy_value', 'NONE');
#70360 = AXIS2_PLACEMENT_3D ( 'NONE', #31226, #54227, #39739 ) ;
#70361 = EDGE_CURVE ( 'NONE', #79695, #69512, #40272, .T. ) ;
#70362 = CARTESIAN_POINT ( 'NONE',  ( 10.00000000000000000, 27.87363466993042138, -12.81628187352647608 ) ) ;
#70363 = CARTESIAN_POINT ( 'NONE',  ( 7.084665262690076126, 59.10535201082150536, 10.88017736071109987 ) ) ;
#70365 = CARTESIAN_POINT ( 'NONE',  ( 7.361572987183169658, 4.967264484334119601, -9.846743663894592657 ) ) ;
#70364 = CARTESIAN_POINT ( 'NONE',  ( -2.266590686148945544, 52.22041550158064638, 7.082119434687048631 ) ) ;
#70366 = DIRECTION ( 'NONE',  ( 0.000000000000000000, 0.000000000000000000, 1.000000000000000000 ) ) ;
#70367 = CARTESIAN_POINT ( 'NONE',  ( 19.84674366389459621, 48.50893115100078745, 7.409399052514197653E-17 ) ) ;
#70368 = CARTESIAN_POINT ( 'NONE',  ( 0.1532563361054083140, 36.00893115100078745, 1.131784320476157264E-15 ) ) ;
#70369 = EDGE_CURVE ( 'NONE', #73524, #68154, #26873, .T. ) ;
#70370 = CARTESIAN_POINT ( 'NONE',  ( -4.164238869374099039, 11.80374883491396965, 8.674139862899312516E-16 ) ) ;
#70371 = AXIS2_PLACEMENT_3D ( 'NONE', #44868, #89392, #6380 ) ;
#70372 = CARTESIAN_POINT ( 'NONE',  ( 10.00000000000000000, 41.81368534415484106, -10.88017736071110342 ) ) ;
#70373 = CARTESIAN_POINT ( 'NONE',  ( 15.44008868035555260, 14.73035201082150536, 9.422509992056143702 ) ) ;
#70374 = TOROIDAL_SURFACE ( 'NONE', #35215, 2.900000000000001243, 0.1000000000000000056 ) ;
#70375 = CARTESIAN_POINT ( 'NONE',  ( 4.559911319644449179, 42.23035201082151247, -9.422509992056141925 ) ) ;
#70376 = CARTESIAN_POINT ( 'NONE',  ( 0.5774900079438590739, 27.64701867748817676, -5.440088680355550821 ) ) ;
#70377 = VERTEX_POINT ( 'NONE', #21565 ) ;
#70378 = CARTESIAN_POINT ( 'NONE',  ( 17.96484262340118221, 36.18868534415484106, -7.964842623401177768 ) ) ;
#70379 = VERTEX_POINT ( 'NONE', #52054 ) ;
#70380 = CARTESIAN_POINT ( 'NONE',  ( -1.099225684535947600, 63.70696800326376774, -6.408140936763238038 ) ) ;
#70381 = CARTESIAN_POINT ( 'NONE',  ( 4.559911319644449179, 47.23035201082150536, -9.422509992056141925 ) ) ;
#70382 = EDGE_LOOP ( 'NONE', ( #12619, #54740, #45688, #10852, #83544, #59784, #58952, #5080, #45622, #30162, #14601, #23106, #96181, #81190 ) ) ;
#70383 = CARTESIAN_POINT ( 'NONE',  ( 19.42250999205614548, 50.98035201082151247, -5.440088680355545492 ) ) ;
#70384 = FILL_AREA_STYLE_COLOUR ( '', #40243 ) ;
#70385 = CYLINDRICAL_SURFACE ( 'NONE', #86732, 11.92686044187656513 ) ;
#70386 = CARTESIAN_POINT ( 'NONE',  ( 13.55255535720595184, 0.000000000000000000, -4.403492169842965431 ) ) ;
#70387 = CARTESIAN_POINT ( 'NONE',  ( 17.08211943468705130, 58.47041550158063927, 12.26659068614894998 ) ) ;
#70388 = CARTESIAN_POINT ( 'NONE',  ( 0.1532563361054083140, 1.008931151000784787, 1.131784320476157264E-15 ) ) ;
#70389 = CARTESIAN_POINT ( 'NONE',  ( -7.117803565204842364, -58.38168516195393920, -4.000000000000000888 ) ) ;
#70390 = CARTESIAN_POINT ( 'NONE',  ( -0.8801773607111009756, 8.063685344154837509, 1.068504757029289695E-15 ) ) ;
#70391 = CARTESIAN_POINT ( 'NONE',  ( 2.791683348922240793, 46.63393115100077324, 7.208316651077764092 ) ) ;
#70392 = VERTEX_POINT ( 'NONE', #82547 ) ;
#70393 = CARTESIAN_POINT ( 'NONE',  ( 7.361572987183170547, 42.05059781766745886, 9.846743663894590881 ) ) ;
#70394 = CARTESIAN_POINT ( 'NONE',  ( 4.559911319644449179, 63.89701867748817676, 9.422509992056141925 ) ) ;
#70395 = CARTESIAN_POINT ( 'NONE',  ( 10.00000000000000178, 39.31368534415484106, 10.88017736071110342 ) ) ;
#70396 = CARTESIAN_POINT ( 'NONE',  ( 0.1532563361054082862, 51.21726448433412315, 2.638427012816831674 ) ) ;
#70398 = CARTESIAN_POINT ( 'NONE',  ( -0.8801773607110991993, 67.85535201082151957, -2.915334737309923874 ) ) ;
#70397 = SURFACE_STYLE_FILL_AREA ( #33833 ) ;
#70399 = CARTESIAN_POINT ( 'NONE',  ( 12.91533473730992121, 49.52201867748817676, 10.88017736071110164 ) ) ;
#70400 = CARTESIAN_POINT ( 'NONE',  ( 24.16423886937410614, 54.30374883491396787, 8.672049930838204340E-16 ) ) ;
#70401 = CIRCLE ( 'NONE', #68825, 0.2500000000000002220 ) ;
#70402 = EDGE_CURVE ( 'NONE', #25656, #93854, #82767, .T. ) ;
#70403 = TOROIDAL_SURFACE ( 'NONE', #76743, 4.250000000000001776, 0.2500000000000000000 ) ;
#70404 = CARTESIAN_POINT ( 'NONE',  ( 6.565887622018943937, 25.16530133659708213, 12.81628187352647430 ) ) ;
#70405 = DIRECTION ( 'NONE',  ( -1.000000000000000000, 0.000000000000000000, 0.000000000000000000 ) ) ;
#70406 = EDGE_LOOP ( 'NONE', ( #35505, #63012, #69656, #6801, #97210, #6405 ) ) ;
#70407 = CARTESIAN_POINT ( 'NONE',  ( 22.81628187352648496, 31.83196800326375353, -3.434112377981050290 ) ) ;
#70408 = CARTESIAN_POINT ( 'NONE',  ( 19.42250999205614548, 15.98035201082150714, -5.440088680355545492 ) ) ;
#70409 = EDGE_LOOP ( 'NONE', ( #3349, #93652, #24117, #17573, #57958 ) ) ;
#70410 = ORIENTED_EDGE ( 'NONE', *, *, #29805, .F. ) ;
#70411 = CARTESIAN_POINT ( 'NONE',  ( 18.52753015748617571, 48.09226448433412315, 4.923371831947298993 ) ) ;
#70413 = CARTESIAN_POINT ( 'NONE',  ( 7.361572987183169658, 34.96726448433411605, -9.846743663894592657 ) ) ;
#70412 = CARTESIAN_POINT ( 'NONE',  ( 5.076628168052703671, 6.842264484334118713, 8.527530157486179263 ) ) ;
#70414 = CARTESIAN_POINT ( 'NONE',  ( -10.79817015753363840, -44.62824817291426882, 3.750000000000000888 ) ) ;
#70415 = SURFACE_SIDE_STYLE ('',( #9410 ) ) ;
#70416 = CARTESIAN_POINT ( 'NONE',  ( 2.791683348922237240, 25.38393115100078390, -7.208316651077763204 ) ) ;
#70417 = DIRECTION ( 'NONE',  ( 0.000000000000000000, 0.000000000000000000, -1.000000000000000000 ) ) ;
#70418 = DIRECTION ( 'NONE',  ( 1.000000000000000000, 0.000000000000000000, 0.000000000000000000 ) ) ;
#70420 = SURFACE_SIDE_STYLE ('',( #41418 ) ) ;
#70419 = CARTESIAN_POINT ( 'NONE',  ( 12.63842701281683922, 29.55059781766745175, -9.846743663894590881 ) ) ;
#70421 = DIRECTION ( 'NONE',  ( 1.257568779154408793E-17, 1.000000000000000000, -0.000000000000000000 ) ) ;
#70423 = ORIENTED_EDGE ( 'NONE', *, *, #98139, .T. ) ;
#70422 = CARTESIAN_POINT ( 'NONE',  ( 0.1532563361054083140, 41.00893115100078745, 1.131784320476157264E-15 ) ) ;
#70424 = AXIS2_PLACEMENT_3D ( 'NONE', #22133, #15628, #22630 ) ;
#70425 = CARTESIAN_POINT ( 'NONE',  ( 19.38216949554541557, 32.24863466993041783, -9.382169495545420901 ) ) ;
#70426 = CARTESIAN_POINT ( 'NONE',  ( -13.78592789153091225, 90.90750312509719322, 7.843642351634943388 ) ) ;
#70427 = CARTESIAN_POINT ( 'NONE',  ( -2.266590686148945544, 46.38708216824730357, -7.082119434687050408 ) ) ;
#70428 = CARTESIAN_POINT ( 'NONE',  ( 17.20831665107776587, 24.13393115100078035, -7.208316651077762316 ) ) ;
#70430 = CARTESIAN_POINT ( 'NONE',  ( 19.84674366389459266, 3.717264484334118713, -2.638427012816827677 ) ) ;
#70429 = AXIS2_PLACEMENT_3D ( 'NONE', #23382, #70351, #69858 ) ;
#70431 = DIRECTION ( 'NONE',  ( -0.000000000000000000, -1.000000000000000000, -0.000000000000000000 ) ) ;
#70432 = CARTESIAN_POINT ( 'NONE',  ( 22.26659068614894466, 43.88708216824729647, 7.082119434687054849 ) ) ;
#70433 = CARTESIAN_POINT ( 'NONE',  ( 5.076628168052704559, 65.17559781766745175, -8.527530157486179263 ) ) ;
#70434 = CARTESIAN_POINT ( 'NONE',  ( 24.16423886937410614, 54.51208216824730357, -3.795296366450302550 ) ) ;
#70435 = CARTESIAN_POINT ( 'NONE',  ( -2.266590686148945544, 21.38708216824730357, -7.082119434687050408 ) ) ;
#70436 = CARTESIAN_POINT ( 'NONE',  ( 2.917880565312950480, 25.97041550158063572, -12.26659068614894821 ) ) ;
#70437 = CARTESIAN_POINT ( 'NONE',  ( 0.000000000000000000, 0.5000000000000004441, 0.000000000000000000 ) ) ;
#70438 = CARTESIAN_POINT ( 'NONE',  ( 5.076628168052703671, 61.84226448433412315, 8.527530157486179263 ) ) ;
#70439 = CARTESIAN_POINT ( 'NONE',  ( 17.96484262340118221, 34.93868534415482685, 7.964842623401181321 ) ) ;
#70440 = CARTESIAN_POINT ( 'NONE',  ( 13.99999999999999822, 61.50000000000000711, 6.000000000000000000 ) ) ;
#70441 = CARTESIAN_POINT ( 'NONE',  ( 20.00000000000000711, 98.59912998021081876, -4.500000000000000000 ) ) ;
#70442 = EDGE_CURVE ( 'NONE', #2021, #40706, #90759, .T. ) ;
#70443 = CARTESIAN_POINT ( 'NONE',  ( 0.1532563361054100626, 40.80059781766745886, -2.638427012816831230 ) ) ;
#70444 = CARTESIAN_POINT ( 'NONE',  ( 22.81628187352647785, 56.62363466993042493, 6.195893100308588602E-16 ) ) ;
#70445 = CARTESIAN_POINT ( 'NONE',  ( 12.26659068614894466, -10.27958449841935540, -7.082119434687053960 ) ) ;
#70446 = CARTESIAN_POINT ( 'NONE',  ( 14.92337183194729633, 47.67559781766745175, 8.527530157486181039 ) ) ;
#70447 = FACE_OUTER_BOUND ( 'NONE', #68485, .T. ) ;
#70448 = VERTEX_POINT ( 'NONE', #21064 ) ;
#70449 = CARTESIAN_POINT ( 'NONE',  ( -2.266590686148945544, 17.22041550158063572, 7.082119434687048631 ) ) ;
#70450 = DIRECTION ( 'NONE',  ( 0.000000000000000000, 1.000000000000000000, 0.000000000000000000 ) ) ;
#70452 = DIRECTION ( 'NONE',  ( 1.000000000000000000, 0.000000000000000000, 0.000000000000000000 ) ) ;
#70451 = DIRECTION ( 'NONE',  ( -1.000000000000000000, -0.000000000000000000, -0.000000000000000000 ) ) ;
#70453 = CARTESIAN_POINT ( 'NONE',  ( 0.5774900079438590739, 12.64701867748817321, -5.440088680355550821 ) ) ;
#70454 = CARTESIAN_POINT ( 'NONE',  ( -2.816281873526471635, 8.915301336597083903, -3.434112377981056508 ) ) ;
#70455 = CARTESIAN_POINT ( 'NONE',  ( 21.92686044187656691, 2.188309369127507953, 4.562052436263911564E-16 ) ) ;
#70456 = CARTESIAN_POINT ( 'NONE',  ( 15.44008868035555260, 64.73035201082151957, 9.422509992056143702 ) ) ;
#70457 = DIRECTION ( 'NONE',  ( 1.000000000000000000, 0.000000000000000000, 0.000000000000000000 ) ) ;
#70458 = CARTESIAN_POINT ( 'NONE',  ( 1.472469842513823179, 31.42559781766745530, 4.923371831947296329 ) ) ;
#70459 = CARTESIAN_POINT ( 'NONE',  ( 24.16423886937410614, 64.30374883491396076, 8.672049930838204340E-16 ) ) ;
#70460 = CARTESIAN_POINT ( 'NONE',  ( -8.099999999999999645, 80.99999999999994316, 3.000000000000000000 ) ) ;
#70461 = CARTESIAN_POINT ( 'NONE',  ( 10.00000000000000178, 29.31368534415483751, 10.88017736071110342 ) ) ;
#70462 = CARTESIAN_POINT ( 'NONE',  ( 4.559911319644449179, 37.23035201082150536, -9.422509992056141925 ) ) ;
#70463 = CARTESIAN_POINT ( 'NONE',  ( 5.076628168052704559, 65.17559781766745175, -8.527530157486179263 ) ) ;
#70464 = CARTESIAN_POINT ( 'NONE',  ( 14.92337183194729988, 59.34226448433412315, -8.527530157486177487 ) ) ;
#70465 = CARTESIAN_POINT ( 'NONE',  ( 10.00000000000000000, 57.87363466993042493, -12.81628187352647608 ) ) ;
#70466 = CARTESIAN_POINT ( 'NONE',  ( 2.791683348922240793, 1.633931151000784565, 7.208316651077764092 ) ) ;
#70467 = ORIENTED_EDGE ( 'NONE', *, *, #58707, .T. ) ;
#70468 = CIRCLE ( 'NONE', #19357, 15.00000000000000000 ) ;
#70469 = AXIS2_PLACEMENT_3D ( 'NONE', #20389, #96897, #57875 ) ;
#70470 = CARTESIAN_POINT ( 'NONE',  ( 20.88017736071110164, 25.35535201082150891, 2.915334737309930979 ) ) ;
#70471 = CARTESIAN_POINT ( 'NONE',  ( 6.565887622018943937, 33.08196800326374643, -12.81628187352647608 ) ) ;
#70472 = FACE_OUTER_BOUND ( 'NONE', #24274, .T. ) ;
#70473 = EDGE_CURVE ( 'NONE', #1302, #81942, #14063, .T. ) ;
#70474 = CARTESIAN_POINT ( 'NONE',  ( 10.00000000000000000, -2.126365330069579951, -12.81628187352647608 ) ) ;
#70475 = CARTESIAN_POINT ( 'NONE',  ( 4.559911319644449179, 43.89701867748816966, 9.422509992056141925 ) ) ;
#70476 = CARTESIAN_POINT ( 'NONE',  ( 0.1532563361054100626, 10.80059781766745175, -2.638427012816831230 ) ) ;
#70477 = CARTESIAN_POINT ( 'NONE',  ( 22.81628187352647785, 31.41530133659709279, 3.434112377981063169 ) ) ;
#70479 = CARTESIAN_POINT ( 'NONE',  ( -20.19000000000001194, 92.00000000000000000, 9.500000000000000000 ) ) ;
#70478 = CARTESIAN_POINT ( 'NONE',  ( 12.91533473730993009, 66.60535201082150536, -10.88017736071109987 ) ) ;
#70480 = CARTESIAN_POINT ( 'NONE',  ( 18.39792806157253224, 54.52224192338642439, 6.499999999999920952 ) ) ;
#70481 = CARTESIAN_POINT ( 'NONE',  ( 0.6178305044545838731, 64.74863466993043914, 9.382169495545420901 ) ) ;
#70482 = ORIENTED_EDGE ( 'NONE', *, *, #73156, .F. ) ;
#70483 = CARTESIAN_POINT ( 'NONE',  ( 0.000000000000000000, 0.000000000000000000, 10.00000000000000000 ) ) ;
#70484 = PRESENTATION_STYLE_ASSIGNMENT (( #33436 ) ) ;
#70485 = EDGE_CURVE ( 'NONE', #34672, #86489, #68047, .T. ) ;
#70486 = CARTESIAN_POINT ( 'NONE',  ( -0.8801773607111008646, 8.272018677488171434, 2.915334737309923430 ) ) ;
#70488 = CARTESIAN_POINT ( 'NONE',  ( 22.26659068614895176, 14.72041550158063572, -7.082119434687042414 ) ) ;
#70487 = CARTESIAN_POINT ( 'NONE',  ( 22.81628187352647785, 51.41530133659708923, 3.434112377981063169 ) ) ;
#70489 = CARTESIAN_POINT ( 'NONE',  ( 14.92337183194729988, 14.34226448433411782, -8.527530157486177487 ) ) ;
#70490 = CARTESIAN_POINT ( 'NONE',  ( 10.00000000000000178, 4.313685344154837509, 10.88017736071110342 ) ) ;
#70491 = CARTESIAN_POINT ( 'NONE',  ( 10.00000000000000000, 19.75893115100078390, -9.846743663894594434 ) ) ;
#70492 = CARTESIAN_POINT ( 'NONE',  ( 13.79529636645031943, 50.34541550158064638, -14.16423886937409904 ) ) ;
#70493 = EDGE_LOOP ( 'NONE', ( #64582, #13658, #79296, #97535 ) ) ;
#70494 = MECHANICAL_DESIGN_GEOMETRIC_PRESENTATION_REPRESENTATION (  '', ( #95972 ), #83187 ) ;
#70495 = CARTESIAN_POINT ( 'NONE',  ( -0.8801773607111009756, 3.063685344154837509, 1.068504757029289695E-15 ) ) ;
#70496 = CARTESIAN_POINT ( 'NONE',  ( 10.00000000000000000, 16.81368534415483751, -10.88017736071110342 ) ) ;
#70497 = FACE_OUTER_BOUND ( 'NONE', #5332, .T. ) ;
#70498 = VECTOR ( 'NONE', #84799, 1000.000000000000114 ) ;
#70499 = VERTEX_POINT ( 'NONE', #6547 ) ;
#70500 = CARTESIAN_POINT ( 'NONE',  ( 20.88017736071110519, 15.56368534415483751, 2.639326808657452039E-16 ) ) ;
#70501 = CARTESIAN_POINT ( 'NONE',  ( 17.96484262340118221, 14.93868534415484106, 7.964842623401181321 ) ) ;
#70502 = CARTESIAN_POINT ( 'NONE',  ( 12.63842701281683034, 52.46726448433413026, 9.846743663894596210 ) ) ;
#70503 = CARTESIAN_POINT ( 'NONE',  ( -13.61464873478171533, 0.5000000000000004441, 6.296136897217742501 ) ) ;
#70504 = CARTESIAN_POINT ( 'NONE',  ( 6.204703633549690345, 15.76208216824730179, -14.16423886937410259 ) ) ;
#70505 = CARTESIAN_POINT ( 'NONE',  ( 10.00000000000000000, 31.81368534415483751, -10.88017736071110342 ) ) ;
#70506 = CARTESIAN_POINT ( 'NONE',  ( 22.26659068614895176, 64.72041550158064638, -7.082119434687042414 ) ) ;
#70507 = CARTESIAN_POINT ( 'NONE',  ( 10.00000000000000000, 54.75893115100078745, -9.846743663894594434 ) ) ;
#70508 = CARTESIAN_POINT ( 'NONE',  ( 18.50749283717773253, 44.69955587570481015, 6.500000000000077272 ) ) ;
#70509 = CARTESIAN_POINT ( 'NONE',  ( 17.20831665107776587, 42.88393115100077324, 7.208316651077764980 ) ) ;
#70510 = CYLINDRICAL_SURFACE ( 'NONE', #25560, 19.99999999999999645 ) ;
#70511 = CARTESIAN_POINT ( 'NONE',  ( 19.84674366389459266, 8.300597817667451750, 2.638427012816836559 ) ) ;
#70512 = CARTESIAN_POINT ( 'NONE',  ( 7.208316651077762316, 24.13393115100078745, -7.208316651077764980 ) ) ;
#70513 = ORIENTED_EDGE ( 'NONE', *, *, #65210, .T. ) ;
#70514 = EDGE_CURVE ( 'NONE', #72554, #5105, #51073, .T. ) ;
#70515 = MECHANICAL_DESIGN_GEOMETRIC_PRESENTATION_REPRESENTATION (  '', ( #51304 ), #76854 ) ;
#70516 = CARTESIAN_POINT ( 'NONE',  ( 10.00000000000000178, 4.313685344154837509, 10.88017736071110342 ) ) ;
#70517 = CARTESIAN_POINT ( 'NONE',  ( 7.361572987183170547, 2.050597817667451750, 9.846743663894590881 ) ) ;
#70519 = CARTESIAN_POINT ( 'NONE',  ( 12.91533473730993009, 46.60535201082150536, -10.88017736071109987 ) ) ;
#70518 = CARTESIAN_POINT ( 'NONE',  ( 7.084665262690076126, 49.10535201082149825, 10.88017736071109987 ) ) ;
#70521 = CARTESIAN_POINT ( 'NONE',  ( 22.81628187352647785, 46.41530133659708213, 3.434112377981063169 ) ) ;
#70520 = CARTESIAN_POINT ( 'NONE',  ( 0.5774900079438590739, 12.64701867748817143, -5.440088680355550821 ) ) ;
#70522 = CARTESIAN_POINT ( 'NONE',  ( 6.204703633549690345, 22.84541550158062861, 14.16423886937410082 ) ) ;
#70523 = ADVANCED_FACE ( 'NONE', ( #67556 ), #1542, .T. ) ;
#70524 = CARTESIAN_POINT ( 'NONE',  ( -2.816281873526473856, 44.12363466993042493, 9.499525473075851096E-16 ) ) ;
#70525 = ORIENTED_EDGE ( 'NONE', *, *, #2782, .F. ) ;
#70526 = CARTESIAN_POINT ( 'NONE',  ( 7.361572987183169658, 54.96726448433413026, -9.846743663894592657 ) ) ;
#70527 = CARTESIAN_POINT ( 'NONE',  ( 7.084665262690076126, 17.02201867748817676, -10.88017736071110164 ) ) ;
#70528 = CARTESIAN_POINT ( 'NONE',  ( 12.91533473730993009, 31.60535201082150891, -10.88017736071109987 ) ) ;
#70529 = EDGE_CURVE ( 'NONE', #57542, #17879, #62003, .T. ) ;
#70530 = ORIENTED_EDGE ( 'NONE', *, *, #89951, .F. ) ;
#70531 = CARTESIAN_POINT ( 'NONE',  ( 0.1532563361054100626, 10.80059781766745175, -2.638427012816831230 ) ) ;
#70532 = CARTESIAN_POINT ( 'NONE',  ( 10.00000000000000000, 66.81368534415484817, -10.88017736071110342 ) ) ;
#70533 = DIRECTION ( 'NONE',  ( 0.000000000000000000, 0.000000000000000000, 1.000000000000000000 ) ) ;
#70534 = CARTESIAN_POINT ( 'NONE',  ( 2.791683348922240793, 6.633931151000785675, 7.208316651077764092 ) ) ;
#70535 = CARTESIAN_POINT ( 'NONE',  ( -0.8801773607111008646, 68.27201867748817676, 2.915334737309923430 ) ) ;
#70536 = CARTESIAN_POINT ( 'NONE',  ( -10.17198128013128589, 0.2306972965111904195, -10.94389562857679898 ) ) ;
#70538 = SURFACE_STYLE_USAGE ( .BOTH. , #93024 ) ;
#70537 = CARTESIAN_POINT ( 'NONE',  ( 20.88017736071110875, 55.77201867748816966, -2.915334737309920765 ) ) ;
#70539 = CARTESIAN_POINT ( 'NONE',  ( 4.559911319644449179, 68.89701867748817676, 9.422509992056141925 ) ) ;
#70541 = ORIENTED_EDGE ( 'NONE', *, *, #28143, .F. ) ;
#70540 = CARTESIAN_POINT ( 'NONE',  ( 1.472469842513823179, 1.425597817667451528, 4.923371831947296329 ) ) ;
#70542 = CARTESIAN_POINT ( 'NONE',  ( 19.84674366389459266, 53.71726448433411605, -2.638427012816827677 ) ) ;
#70543 = ORIENTED_EDGE ( 'NONE', *, *, #53059, .F. ) ;
#70544 = ORIENTED_EDGE ( 'NONE', *, *, #74961, .F. ) ;
#70545 = CARTESIAN_POINT ( 'NONE',  ( 17.08211943468705840, 10.13708216824730179, -12.26659068614894466 ) ) ;
#70546 = CARTESIAN_POINT ( 'NONE',  ( -2.816281873526471635, 53.91530133659709634, -3.434112377981056508 ) ) ;
#70547 = CARTESIAN_POINT ( 'NONE',  ( 10.00000000000000178, 23.05374883491397142, 14.16423886937410082 ) ) ;
#70548 = CARTESIAN_POINT ( 'NONE',  ( 17.39651004071841101, 57.93575266056827644, 6.500000000000005329 ) ) ;
#70549 = CARTESIAN_POINT ( 'NONE',  ( 14.62617646268092209, 14.49999999999999112, 3.327906561566971622 ) ) ;
#70550 = CARTESIAN_POINT ( 'NONE',  ( 10.00000000000000000, 21.81368534415484106, -10.88017736071110342 ) ) ;
#70551 = VERTEX_POINT ( 'NONE', #85015 ) ;
#70552 = CARTESIAN_POINT ( 'NONE',  ( 2.791683348922237240, 0.3839311510007847872, -7.208316651077763204 ) ) ;
#70553 = CARTESIAN_POINT ( 'NONE',  ( 17.20831665107776587, 9.133931151000787452, -7.208316651077762316 ) ) ;
#70554 = CARTESIAN_POINT ( 'NONE',  ( -2.816281873526473856, 34.33196800326376064, 3.434112377981055619 ) ) ;
#70555 = CARTESIAN_POINT ( 'NONE',  ( 14.92337183194729633, 32.67559781766745175, 8.527530157486181039 ) ) ;
#70556 = DIRECTION ( 'NONE',  ( -0.000000000000000000, -1.000000000000000000, -0.000000000000000000 ) ) ;
#70557 = EDGE_CURVE ( 'NONE', #95164, #48237, #31986, .T. ) ;
#70558 = CARTESIAN_POINT ( 'NONE',  ( -1.099225684535947600, 9.540301336597087456, 6.408140936763237150 ) ) ;
#70559 = DIRECTION ( 'NONE',  ( -0.04361938736533987893, 0.000000000000000000, 0.9990482215818576872 ) ) ;
#70560 = AXIS2_PLACEMENT_3D ( 'NONE', #93071, #19539, #97046 ) ;
#70561 = CARTESIAN_POINT ( 'NONE',  ( 1.472469842513823179, 31.42559781766745530, 4.923371831947296329 ) ) ;
#70562 = CARTESIAN_POINT ( 'NONE',  ( 14.92337183194729988, 4.342264484334117824, -8.527530157486177487 ) ) ;
#70563 = ORIENTED_EDGE ( 'NONE', *, *, #41553, .T. ) ;
#70564 = ADVANCED_FACE ( 'NONE', ( #47496 ), #40006, .T. ) ;
#70565 = VERTEX_POINT ( 'NONE', #92502 ) ;
#70566 = CARTESIAN_POINT ( 'NONE',  ( 4.559911319644449179, 37.23035201082150536, -9.422509992056141925 ) ) ;
#70567 = CARTESIAN_POINT ( 'NONE',  ( 20.36894250292379382, 38.67874883491396076, 10.36894250292379205 ) ) ;
#70568 = CARTESIAN_POINT ( 'NONE',  ( 14.92337183194729988, 39.34226448433412315, -8.527530157486177487 ) ) ;
#70569 = CARTESIAN_POINT ( 'NONE',  ( 12.63842701281683922, 14.55059781766744997, -9.846743663894590881 ) ) ;
#70570 = STYLED_ITEM ( 'NONE', ( #89427 ), #47084 ) ;
#70572 = FACE_OUTER_BOUND ( 'NONE', #41546, .T. ) ;
#70571 = CARTESIAN_POINT ( 'NONE',  ( 13.43411237798105340, 55.58196800326374643, 12.81628187352647963 ) ) ;
#70573 = CARTESIAN_POINT ( 'NONE',  ( 17.96484262340118221, 26.18868534415483396, -7.964842623401177768 ) ) ;
#70574 = SURFACE_STYLE_FILL_AREA ( #16589 ) ;
#70575 = CARTESIAN_POINT ( 'NONE',  ( -1.099225684535947600, 18.70696800326375353, -6.408140936763238038 ) ) ;
#70576 = CARTESIAN_POINT ( 'NONE',  ( 19.84674366389459621, 38.50893115100078745, 7.409399052514197653E-17 ) ) ;
#70577 = CARTESIAN_POINT ( 'NONE',  ( 2.915334737309928315, -0.4779813225118263453, 10.88017736071109987 ) ) ;
#70578 = CARTESIAN_POINT ( 'NONE',  ( 3.591859063236761518, 44.95696800326376064, 11.09922568453594849 ) ) ;
#70579 = DIRECTION ( 'NONE',  ( -0.000000000000000000, 1.000000000000000000, 0.000000000000000000 ) ) ;
#70580 = AXIS2_PLACEMENT_3D ( 'NONE', #56159, #86652, #41165 ) ;
#70582 = DIRECTION ( 'NONE',  ( -0.000000000000000000, -0.000000000000000000, -1.000000000000000000 ) ) ;
#70581 = CARTESIAN_POINT ( 'NONE',  ( 19.42250999205614193, 60.14701867748817676, 5.440088680355555262 ) ) ;
#70583 = CARTESIAN_POINT ( 'NONE',  ( -13.55101055326446513, 0.2301500585724586545, -6.292244619294828922 ) ) ;
#70584 = DIRECTION ( 'NONE',  ( -0.4924235601034707144, 0.000000000000000000, 0.8703556959398975890 ) ) ;
#70585 = CARTESIAN_POINT ( 'NONE',  ( -0.8801773607110991993, 47.85535201082150536, -2.915334737309923874 ) ) ;
#70586 = CARTESIAN_POINT ( 'NONE',  ( 0.5774900079438607392, 53.48035201082151247, 5.440088680355550821 ) ) ;
#70587 = CARTESIAN_POINT ( 'NONE',  ( -45.94000000000001194, 92.50000000000000000, 9.000000000000000000 ) ) ;
#70589 = EDGE_CURVE ( 'NONE', #62099, #95614, #568, .T. ) ;
#70588 = CARTESIAN_POINT ( 'NONE',  ( 0.000000000000000000, 15.00000000000000000, 0.000000000000000000 ) ) ;
#70590 = CARTESIAN_POINT ( 'NONE',  ( 2.035157376598824452, 13.68868534415483751, 7.964842623401179544 ) ) ;
#70591 = CARTESIAN_POINT ( 'NONE',  ( 3.591859063236763294, -1.709698663402913210, -11.09922568453595026 ) ) ;
#70593 = CYLINDRICAL_SURFACE ( 'NONE', #84639, 10.90000000000026326 ) ;
#70592 = CARTESIAN_POINT ( 'NONE',  ( -0.8801773607111009756, 18.06368534415484106, 1.068504757029289695E-15 ) ) ;
#70594 = CARTESIAN_POINT ( 'NONE',  ( 0.000000000000000000, 0.5000000000000004441, 0.000000000000000000 ) ) ;
#70595 = CARTESIAN_POINT ( 'NONE',  ( 22.81628187352647785, 26.62363466993042138, 6.195893100308588602E-16 ) ) ;
#70596 = EDGE_LOOP ( 'NONE', ( #64572, #20475, #72666, #42777, #78170, #70721 ) ) ;
#70597 = CARTESIAN_POINT ( 'NONE',  ( 15.44008868035555260, 54.73035201082150536, 9.422509992056143702 ) ) ;
#70598 = EDGE_CURVE ( 'NONE', #65919, #97109, #62492, .T. ) ;
#70599 = CARTESIAN_POINT ( 'NONE',  ( 19.84674366389459266, 38.71726448433412315, -2.638427012816827677 ) ) ;
#70600 = CARTESIAN_POINT ( 'NONE',  ( 21.09922568453594849, 1.206968003263753531, 6.408140936763242479 ) ) ;
#70601 = CARTESIAN_POINT ( 'NONE',  ( 4.559911319644449179, 18.89701867748817321, 9.422509992056141925 ) ) ;
#70602 = CARTESIAN_POINT ( 'NONE',  ( -0.8801773607110991993, 37.85535201082151247, -2.915334737309923874 ) ) ;
#70603 = CARTESIAN_POINT ( 'NONE',  ( -4.164238869374098151, 46.59541550158063927, -3.795296366450310543 ) ) ;
#70604 = CARTESIAN_POINT ( 'NONE',  ( 17.20831665107776587, 42.88393115100077324, 7.208316651077764980 ) ) ;
#70605 = CARTESIAN_POINT ( 'NONE',  ( -0.8801773607111008646, 58.27201867748816966, 2.915334737309923430 ) ) ;
#70606 = DIRECTION ( 'NONE',  ( 0.000000000000000000, 0.000000000000000000, -1.000000000000000000 ) ) ;
#70607 = CARTESIAN_POINT ( 'NONE',  ( 17.08211943468705130, 13.47041550158063572, 12.26659068614894998 ) ) ;
#70608 = DIRECTION ( 'NONE',  ( -1.000000000000000000, 0.000000000000000000, 0.000000000000000000 ) ) ;
#70609 = DIRECTION ( 'NONE',  ( -0.000000000000000000, 0.000000000000000000, 1.000000000000000000 ) ) ;
#70610 = ORIENTED_EDGE ( 'NONE', *, *, #94697, .T. ) ;
#70611 = VERTEX_POINT ( 'NONE', #76523 ) ;
#70612 = AXIS2_PLACEMENT_3D ( 'NONE', #24034, #85017, #77498 ) ;
#70613 = CARTESIAN_POINT ( 'NONE',  ( 2.917880565312948704, 32.63708216824730357, 12.26659068614894643 ) ) ;
#70614 = CARTESIAN_POINT ( 'NONE',  ( 17.08211943468705840, 40.13708216824731068, -12.26659068614894466 ) ) ;
#70615 = CARTESIAN_POINT ( 'NONE',  ( 10.00000000000000000, -0.2410688489992152128, -9.846743663894594434 ) ) ;
#70616 = CARTESIAN_POINT ( 'NONE',  ( 21.09922568453594849, 21.20696800326375353, 6.408140936763242479 ) ) ;
#70617 = CARTESIAN_POINT ( 'NONE',  ( 19.84674366389459621, 63.50893115100078745, 7.409399052514197653E-17 ) ) ;
#70618 = CARTESIAN_POINT ( 'NONE',  ( -16.94999999999999574, 99.99999999999998579, -8.525133428036873795 ) ) ;
#70620 = CARTESIAN_POINT ( 'NONE',  ( 10.00000000000000000, 37.87363466993041783, -12.81628187352647608 ) ) ;
#70619 = CARTESIAN_POINT ( 'NONE',  ( 0.5774900079438607392, 58.48035201082151247, 5.440088680355550821 ) ) ;
#70621 = CARTESIAN_POINT ( 'NONE',  ( 20.36894250292379382, 23.67874883491397142, 10.36894250292379205 ) ) ;
#70622 = CARTESIAN_POINT ( 'NONE',  ( -0.8801773607110991993, 27.85535201082150181, -2.915334737309923874 ) ) ;
#70623 = DIRECTION ( 'NONE',  ( 1.000000000000000000, 0.000000000000000000, 0.000000000000000000 ) ) ;
#70624 = CARTESIAN_POINT ( 'NONE',  ( 7.361572987183169658, -0.03273551566588185635, -9.846743663894592657 ) ) ;
#70625 = CARTESIAN_POINT ( 'NONE',  ( -9.846743663894594434, -8.991068848999208996, 3.469446951953614189E-15 ) ) ;
#70626 = CARTESIAN_POINT ( 'NONE',  ( 18.52753015748617571, 8.092264484334117824, 4.923371831947298993 ) ) ;
#70627 = ORIENTED_EDGE ( 'NONE', *, *, #16954, .F. ) ;
#70628 = PLANE ( 'NONE',  #74691 ) ;
#70629 = ORIENTED_EDGE ( 'NONE', *, *, #47660, .F. ) ;
#70630 = CARTESIAN_POINT ( 'NONE',  ( 0.000000000000000000, 15.00000000000000000, 0.000000000000000000 ) ) ;
#70631 = EDGE_LOOP ( 'NONE', ( #78878, #29291, #61824, #79997 ) ) ;
#70632 = CARTESIAN_POINT ( 'NONE',  ( 10.00000000000000178, 8.053748834913967869, 14.16423886937410082 ) ) ;
#70634 = CARTESIAN_POINT ( 'NONE',  ( 17.96484262340118221, 11.18868534415484106, -7.964842623401177768 ) ) ;
#70633 = CARTESIAN_POINT ( 'NONE',  ( 10.00000000000000178, 4.313685344154837509, 10.88017736071110342 ) ) ;
#70636 = CARTESIAN_POINT ( 'NONE',  ( -2.816281873526473856, 9.331968003263753531, 3.434112377981055619 ) ) ;
#70635 = CARTESIAN_POINT ( 'NONE',  ( 18.52753015748618282, 38.92559781766745175, -4.923371831947291888 ) ) ;
#70637 = DIRECTION ( 'NONE',  ( 1.000000000000000000, 1.927470528863119542E-16, -0.000000000000000000 ) ) ;
#70638 = FACE_OUTER_BOUND ( 'NONE', #25679, .T. ) ;
#70639 = EDGE_CURVE ( 'NONE', #8299, #93746, #89190, .T. ) ;
#70640 = VECTOR ( 'NONE', #83193, 1000.000000000000000 ) ;
#70641 = CARTESIAN_POINT ( 'NONE',  ( -1.099225684535947600, -1.293031996736246469, -6.408140936763238038 ) ) ;
#70642 = ORIENTED_EDGE ( 'NONE', *, *, #63145, .T. ) ;
#70643 = VECTOR ( 'NONE', #76307, 1000.000000000000000 ) ;
#70644 = AXIS2_PLACEMENT_3D ( 'NONE', #33621, #19132, #80120 ) ;
#70645 = CARTESIAN_POINT ( 'NONE',  ( 24.16423886937410614, 49.51208216824730357, -3.795296366450302550 ) ) ;
#70646 = ORIENTED_EDGE ( 'NONE', *, *, #80880, .T. ) ;
#70647 = VECTOR ( 'NONE', #5191, 999.9999999999998863 ) ;
#70648 = CARTESIAN_POINT ( 'NONE',  ( 13.79529636645030344, 63.26208216824730357, 14.16423886937410614 ) ) ;
#70649 = VERTEX_POINT ( 'NONE', #62990 ) ;
#70650 = CARTESIAN_POINT ( 'NONE',  ( 17.96484262340118221, 39.93868534415484106, 7.964842623401181321 ) ) ;
#70651 = CARTESIAN_POINT ( 'NONE',  ( -0.8801773607111009756, 33.06368534415484106, 1.068504757029289695E-15 ) ) ;
#70652 = CARTESIAN_POINT ( 'NONE',  ( 12.63842701281683922, 59.55059781766744464, -9.846743663894590881 ) ) ;
#70653 = CARTESIAN_POINT ( 'NONE',  ( 10.00000000000000000, 41.81368534415484106, -10.88017736071110342 ) ) ;
#70654 = AXIS2_PLACEMENT_3D ( 'NONE', #29357, #50886, #67873 ) ;
#70655 = CARTESIAN_POINT ( 'NONE',  ( 10.00000000000000178, 69.31368534415484817, 10.88017736071110342 ) ) ;
#70656 = CARTESIAN_POINT ( 'NONE',  ( 0.5774900079438607392, 23.48035201082150536, 5.440088680355550821 ) ) ;
#70657 = B_SPLINE_CURVE_WITH_KNOTS ( 'NONE', 3,
 ( #57563, #88061, #10602, #11093, #19573, #12563, #50070, #80574, #65550, #5072, #3118, #71606 ),
 .UNSPECIFIED., .F., .F.,
 ( 4, 2, 2, 2, 2, 4 ),
 ( 0.000000000000000000, 0.0003464182178352352313, 0.0005196273267528502991, 0.0006062318812116581582, 0.0006495341584410644188, 0.0006928364356704708963 ),
 .UNSPECIFIED. ) ;
#70658 = COLOUR_RGB ( '', 0.08235294, 0.09019608, 0.10196078) ;
#70659 = DIRECTION ( 'NONE',  ( 0.000000000000000000, 0.000000000000000000, 1.000000000000000000 ) ) ;
#70660 = CARTESIAN_POINT ( 'NONE',  ( 0.1532563361054082862, 21.21726448433412315, 2.638427012816831674 ) ) ;
#70661 = CARTESIAN_POINT ( 'NONE',  ( -3.638343494402940248, -8.270261767329087021, 2.500000000000001332 ) ) ;
#70662 = VERTEX_POINT ( 'NONE', #31502 ) ;
#70663 = DIRECTION ( 'NONE',  ( 0.000000000000000000, 0.000000000000000000, 1.000000000000000000 ) ) ;
#70664 = CARTESIAN_POINT ( 'NONE',  ( 14.92337183194729988, 44.34226448433412315, -8.527530157486177487 ) ) ;
#70665 = CARTESIAN_POINT ( 'NONE',  ( 13.99999999999999822, 11.50000000000000000, 5.000000000000000000 ) ) ;
#70666 = SURFACE_STYLE_USAGE ( .BOTH. , #85171 ) ;
#70667 = VECTOR ( 'NONE', #93401, 1000.000000000000000 ) ;
#70668 = CARTESIAN_POINT ( 'NONE',  ( 5.817157072110708427, 14.49999999999999112, 13.82608706751097749 ) ) ;
#70669 = CARTESIAN_POINT ( 'NONE',  ( -46.46849503609698218, 103.9079590269317066, 5.994465626573347805 ) ) ;
#70670 = CARTESIAN_POINT ( 'NONE',  ( 7.881609424765942506, -3.117928278843078365E-15, 12.32025747423898920 ) ) ;
#70671 = CARTESIAN_POINT ( 'NONE',  ( 1.472469842513823179, 55.59226448433412315, -4.923371831947296329 ) ) ;
#70672 = CARTESIAN_POINT ( 'NONE',  ( 13.79529636645030344, 43.26208216824730357, 14.16423886937410614 ) ) ;
#70673 = CARTESIAN_POINT ( 'NONE',  ( 17.20831665107776587, 59.13393115100078745, -7.208316651077762316 ) ) ;
#70674 = VERTEX_POINT ( 'NONE', #92996 ) ;
#70675 = CARTESIAN_POINT ( 'NONE',  ( 0.000000000000000000, 35.00000000000000000, -11.92686044187656513 ) ) ;
#70676 = CARTESIAN_POINT ( 'NONE',  ( 1.472469842513823179, 25.59226448433412315, -4.923371831947296329 ) ) ;
#70677 = CARTESIAN_POINT ( 'NONE',  ( 3.591859063236761518, 54.95696800326376064, 11.09922568453594849 ) ) ;
#70678 = CARTESIAN_POINT ( 'NONE',  ( 5.076628168052703671, 66.84226448433412315, 8.527530157486179263 ) ) ;
#70679 = CARTESIAN_POINT ( 'NONE',  ( 4.559911319644449179, 63.89701867748817676, 9.422509992056141925 ) ) ;
#70680 = CARTESIAN_POINT ( 'NONE',  ( 6.829574850505127692, -88.00372650098204019, -2.750000000000000444 ) ) ;
#70681 = CIRCLE ( 'NONE', #16372, 15.00000000000000000 ) ;
#70682 = EDGE_CURVE ( 'NONE', #38225, #55365, #77986, .T. ) ;
#70683 = EDGE_CURVE ( 'NONE', #87096, #44552, #77496, .T. ) ;
#70684 = ORIENTED_EDGE ( 'NONE', *, *, #62760, .T. ) ;
#70685 = CARTESIAN_POINT ( 'NONE',  ( -4.164238869374099039, 56.80374883491397497, 8.674139862899312516E-16 ) ) ;
#70686 = SURFACE_STYLE_USAGE ( .BOTH. , #40179 ) ;
#70687 = CARTESIAN_POINT ( 'NONE',  ( 10.00000000000000000, 31.81368534415483751, -10.88017736071110342 ) ) ;
#70689 = CARTESIAN_POINT ( 'NONE',  ( 17.96484262340118221, 59.93868534415484106, 7.964842623401181321 ) ) ;
#70688 = CARTESIAN_POINT ( 'NONE',  ( 13.43411237798105340, 15.58196800326374998, 12.81628187352647963 ) ) ;
#70690 = CARTESIAN_POINT ( 'NONE',  ( -1.926860441876563801, 62.66212336850780673, 1.004413902775740978E-15 ) ) ;
#70691 = CARTESIAN_POINT ( 'NONE',  ( -3.881909499400522989, -2.713893563002777498E-15, 14.10103859407592353 ) ) ;
#70692 = DIRECTION ( 'NONE',  ( 1.000000000000000000, 0.000000000000000000, 0.000000000000000000 ) ) ;
#70693 = CYLINDRICAL_SURFACE ( 'NONE', #79126, 15.00000000000000000 ) ;
#70694 = CARTESIAN_POINT ( 'NONE',  ( 7.361572987183170547, 57.05059781766744464, 9.846743663894590881 ) ) ;
#70695 = CARTESIAN_POINT ( 'NONE',  ( 14.92337183194729633, 2.675597817667451750, 8.527530157486181039 ) ) ;
#70696 = CARTESIAN_POINT ( 'NONE',  ( -5.204170427930421283E-15, 30.55374883491396432, -14.16423886937410082 ) ) ;
#70697 = CARTESIAN_POINT ( 'NONE',  ( -1.099225684535947600, 8.706968003263753531, -6.408140936763238038 ) ) ;
#70699 = CARTESIAN_POINT ( 'NONE',  ( 2.377183314880000786, 65.78593319516822646, -6.500000000000057732 ) ) ;
#70698 = CARTESIAN_POINT ( 'NONE',  ( 2.035157376598824452, 8.688685344154839285, 7.964842623401179544 ) ) ;
#70700 = FILL_AREA_STYLE ('',( #55179 ) ) ;
#70701 = CARTESIAN_POINT ( 'NONE',  ( 2.917880565312948704, 32.63708216824730357, 12.26659068614894643 ) ) ;
#70702 = CARTESIAN_POINT ( 'NONE',  ( 24.16423886937409904, 29.09541550158063572, 3.795296366450317205 ) ) ;
#70703 = CARTESIAN_POINT ( 'NONE',  ( 7.084665262690076126, 4.105352010821503583, 10.88017736071109987 ) ) ;
#70704 = VECTOR ( 'NONE', #82381, 999.9999999999998863 ) ;
#70705 = CARTESIAN_POINT ( 'NONE',  ( 14.92337183194729633, 32.67559781766745175, 8.527530157486181039 ) ) ;
#70706 = CARTESIAN_POINT ( 'NONE',  ( 7.361572987183169658, 14.96726448433411960, -9.846743663894592657 ) ) ;
#70707 = CARTESIAN_POINT ( 'NONE',  ( 20.88017736071110519, 20.56368534415484106, 2.639326808657452039E-16 ) ) ;
#70708 = ORIENTED_EDGE ( 'NONE', *, *, #68238, .F. ) ;
#70709 = CARTESIAN_POINT ( 'NONE',  ( 1.472469842513823179, 36.42559781766745175, 4.923371831947296329 ) ) ;
#70710 = CARTESIAN_POINT ( 'NONE',  ( 12.91533473730993009, 46.60535201082150536, -10.88017736071109987 ) ) ;
#70711 = CARTESIAN_POINT ( 'NONE',  ( 7.361572987183169658, 59.96726448433410894, -9.846743663894592657 ) ) ;
#70713 = CARTESIAN_POINT ( 'NONE',  ( -5.279540384298767819, 0.000000000000000000, -1.365381980696781294 ) ) ;
#70712 = CARTESIAN_POINT ( 'NONE',  ( -2.266590686148945544, 21.38708216824730357, -7.082119434687050408 ) ) ;
#70714 = DIRECTION ( 'NONE',  ( 0.6246950475544237324, 0.7808688094430306093, 0.000000000000000000 ) ) ;
#70715 = AXIS2_PLACEMENT_3D ( 'NONE', #36621, #15110, #29097 ) ;
#70716 = VECTOR ( 'NONE', #68694, 1000.000000000000000 ) ;
#70717 = STYLED_ITEM ( 'NONE', ( #50005 ), #48558 ) ;
#70718 = CARTESIAN_POINT ( 'NONE',  ( 18.52753015748618282, 8.925597817667451750, -4.923371831947291888 ) ) ;
#70719 = CARTESIAN_POINT ( 'NONE',  ( 10.00000000000000178, 45.37363466993041783, 12.81628187352647608 ) ) ;
#70720 = CARTESIAN_POINT ( 'NONE',  ( 14.92337183194729988, 49.34226448433411605, -8.527530157486177487 ) ) ;
#70721 = ORIENTED_EDGE ( 'NONE', *, *, #42814, .F. ) ;
#70722 = EDGE_CURVE ( 'NONE', #1078, #9131, #9008, .T. ) ;
#70723 = MECHANICAL_DESIGN_GEOMETRIC_PRESENTATION_REPRESENTATION (  '', ( #73832 ), #2073 ) ;
#70724 = FACE_OUTER_BOUND ( 'NONE', #71935, .T. ) ;
#70725 = CARTESIAN_POINT ( 'NONE',  ( -46.54653926366209760, 102.0639713352970404, -7.520849704105015299 ) ) ;
#70726 = CARTESIAN_POINT ( 'NONE',  ( 6.204703633549690345, 65.76208216824731778, -14.16423886937410259 ) ) ;
#70727 = CARTESIAN_POINT ( 'NONE',  ( -0.3689425029237881626, 7.428748834913967869, 10.36894250292379027 ) ) ;
#70728 = CARTESIAN_POINT ( 'NONE',  ( 17.20831665107776587, 2.883931151000785231, 7.208316651077764980 ) ) ;
#70729 = CARTESIAN_POINT ( 'NONE',  ( 10.00000000000000000, 44.75893115100078745, -9.846743663894594434 ) ) ;
#70730 = CARTESIAN_POINT ( 'NONE',  ( 4.559911319644449179, 17.23035201082150536, -9.422509992056141925 ) ) ;
#70731 = AXIS2_PLACEMENT_3D ( 'NONE', #89260, #6261, #27763 ) ;
#70732 = CARTESIAN_POINT ( 'NONE',  ( 32.56412365047463453, 14.00000000000001066, 9.500000000000000000 ) ) ;
#70733 = CARTESIAN_POINT ( 'NONE',  ( 7.361572987183170547, 62.05059781766745886, 9.846743663894590881 ) ) ;
#70734 = FILL_AREA_STYLE ('',( #54232 ) ) ;
#70735 = CARTESIAN_POINT ( 'NONE',  ( -7.881609424771932382, 14.99999999999799982, 12.32025747424302864 ) ) ;
#70736 = ORIENTED_EDGE ( 'NONE', *, *, #51539, .F. ) ;
#70737 = EDGE_LOOP ( 'NONE', ( #77376, #94730, #5220, #50830 ) ) ;
#70738 = LINE ( 'NONE', #55730, #27790 ) ;
#70739 = DIRECTION ( 'NONE',  ( -0.000000000000000000, -1.000000000000000000, -0.000000000000000000 ) ) ;
#70740 =( NAMED_UNIT ( * ) SI_UNIT ( $, .STERADIAN. ) SOLID_ANGLE_UNIT ( ) );
#70741 = CARTESIAN_POINT ( 'NONE',  ( 22.26659068614895176, 39.72041550158063217, -7.082119434687042414 ) ) ;
#70742 = CARTESIAN_POINT ( 'NONE',  ( 1.472469842513823179, 56.42559781766745886, 4.923371831947296329 ) ) ;
#70743 = CARTESIAN_POINT ( 'NONE',  ( 12.63842701281683922, 19.55059781766745175, -9.846743663894590881 ) ) ;
#70744 = PRESENTATION_STYLE_ASSIGNMENT (( #86721 ) ) ;
#70746 = CARTESIAN_POINT ( 'NONE',  ( 7.361572987183170547, 67.05059781766746596, 9.846743663894590881 ) ) ;
#70745 = CARTESIAN_POINT ( 'NONE',  ( 17.96484262340118221, 21.18868534415483396, -7.964842623401177768 ) ) ;
#70747 = CARTESIAN_POINT ( 'NONE',  ( -1.926860441876562025, 34.47997603579417358, -3.195792623639529761 ) ) ;
#70748 = B_SPLINE_CURVE_WITH_KNOTS ( 'NONE', 3,
 ( #65648, #96171, #66140, #73640, #79683, #58141 ),
 .UNSPECIFIED., .F., .F.,
 ( 4, 2, 4 ),
 ( 0.000000000000000000, 0.0002092266038752941626, 0.0004184532077505883252 ),
 .UNSPECIFIED. ) ;
#70749 = B_SPLINE_CURVE_WITH_KNOTS ( 'NONE', 3,
 ( #83669, #15679, #77140, #69165, #1174, #53656 ),
 .UNSPECIFIED., .F., .F.,
 ( 4, 2, 4 ),
 ( 0.000000000000000000, 0.0002565770811490990710, 0.0005131541622981981420 ),
 .UNSPECIFIED. ) ;
#70750 = CARTESIAN_POINT ( 'NONE',  ( 10.00000000000000178, 38.05374883491396787, 14.16423886937410082 ) ) ;
#70751 = CARTESIAN_POINT ( 'NONE',  ( 13.79529636645031943, 60.34541550158063927, -14.16423886937409904 ) ) ;
#70752 = CARTESIAN_POINT ( 'NONE',  ( 0.1532563361054083140, 66.00893115100079456, 1.131784320476157264E-15 ) ) ;
#70753 = CARTESIAN_POINT ( 'NONE',  ( -11.10175276308059722, 14.95037105032149150, 9.716398248526216364 ) ) ;
#70754 = CARTESIAN_POINT ( 'NONE',  ( 20.88017736071110519, 65.56368534415483396, 2.639326808657452039E-16 ) ) ;
#70755 = CARTESIAN_POINT ( 'NONE',  ( 0.1532563361054100626, 10.80059781766745175, -2.638427012816831230 ) ) ;
#70756 = CARTESIAN_POINT ( 'NONE',  ( -7.116171662429844780, -80.69120418497929847, 3.999999999999194422 ) ) ;
#70757 = EDGE_LOOP ( 'NONE', ( #35182, #65200, #32249, #27310 ) ) ;
#70758 = CARTESIAN_POINT ( 'NONE',  ( -1.175037534397030736, -2.805373121306241934E-15, -14.57833316477038110 ) ) ;
#70759 = VERTEX_POINT ( 'NONE', #39524 ) ;
#70760 = CARTESIAN_POINT ( 'NONE',  ( 17.20831665107776587, 22.88393115100078745, 7.208316651077764980 ) ) ;
#70761 = ORIENTED_EDGE ( 'NONE', *, *, #13694, .F. ) ;
#70762 = CARTESIAN_POINT ( 'NONE',  ( 17.08211943468705840, 30.13708216824730357, -12.26659068614894466 ) ) ;
#70763 = CARTESIAN_POINT ( 'NONE',  ( 14.92337183194729988, 24.34226448433411960, -8.527530157486177487 ) ) ;
#70764 = CARTESIAN_POINT ( 'NONE',  ( 0.5774900079438590739, 47.64701867748817676, -5.440088680355550821 ) ) ;
#70765 = CARTESIAN_POINT ( 'NONE',  ( -3.749999999999994671, 43.00000000000000711, -4.250000000000000000 ) ) ;
#70766 = ORIENTED_EDGE ( 'NONE', *, *, #52091, .T. ) ;
#70767 = CARTESIAN_POINT ( 'NONE',  ( 20.88017736071110519, 40.56368534415484106, 2.639326808657452039E-16 ) ) ;
#70768 = CIRCLE ( 'NONE', #65952, 1.499999999999999112 ) ;
#70769 = CARTESIAN_POINT ( 'NONE',  ( 3.469446951953614189E-15, -9.626365330069580395, 12.81628187352647608 ) ) ;
#70770 = ORIENTED_EDGE ( 'NONE', *, *, #21840, .T. ) ;
#70771 = CARTESIAN_POINT ( 'NONE',  ( 24.16423886937410614, 9.512082168247301794, -3.795296366450302550 ) ) ;
#70772 = ORIENTED_EDGE ( 'NONE', *, *, #39660, .T. ) ;
#70773 = ORIENTED_EDGE ( 'NONE', *, *, #83094, .T. ) ;
#70774 = CARTESIAN_POINT ( 'NONE',  ( 19.38216949554541557, 32.24863466993041783, -9.382169495545420901 ) ) ;
#70775 = CARTESIAN_POINT ( 'NONE',  ( -45.94000000000000483, 92.00000000000000000, -9.500000000000000000 ) ) ;
#70776 = CARTESIAN_POINT ( 'NONE',  ( 19.84674366389459266, 8.717264484334116048, -2.638427012816827677 ) ) ;
#70777 =( NAMED_UNIT ( * ) SI_UNIT ( $, .STERADIAN. ) SOLID_ANGLE_UNIT ( ) );
#70778 = CARTESIAN_POINT ( 'NONE',  ( -1.899999999999997247, 98.49999999999998579, -8.000000000000000000 ) ) ;
#70779 = CARTESIAN_POINT ( 'NONE',  ( 0.1532563361054100626, 25.80059781766744820, -2.638427012816831230 ) ) ;
#70780 = EDGE_CURVE ( 'NONE', #42155, #36998, #41259, .T. ) ;
#70781 = ORIENTED_EDGE ( 'NONE', *, *, #6837, .F. ) ;
#70782 = CARTESIAN_POINT ( 'NONE',  ( 2.153642693323417845, 46.13791097397317742, -6.499999999999926281 ) ) ;
#70783 = CARTESIAN_POINT ( 'NONE',  ( 12.91533473730993009, 61.60535201082150536, -10.88017736071109987 ) ) ;
#70784 = CARTESIAN_POINT ( 'NONE',  ( -14.56089864659471544, 15.00000000000000533, 1.374314915485193245 ) ) ;
#70785 = DIRECTION ( 'NONE',  ( -0.000000000000000000, -1.000000000000000000, -0.000000000000000000 ) ) ;
#70786 = CARTESIAN_POINT ( 'NONE',  ( 10.00000000000000000, 9.758931151000785675, -9.846743663894594434 ) ) ;
#70787 = VECTOR ( 'NONE', #63626, 1000.000000000000000 ) ;
#70788 = CARTESIAN_POINT ( 'NONE',  ( 19.38216949554541202, 10.99863466993042138, 9.382169495545424454 ) ) ;
#70790 = DIRECTION ( 'NONE',  ( 0.9170600743851238246, 0.000000000000000000, -0.3987490689252466969 ) ) ;
#70789 = VECTOR ( 'NONE', #37134, 1000.000000000000000 ) ;
#70791 = CARTESIAN_POINT ( 'NONE',  ( 10.00000000000000000, 24.75893115100078745, -9.846743663894594434 ) ) ;
#70792 = CARTESIAN_POINT ( 'NONE',  ( 3.591859063236763294, 63.29030133659708923, -11.09922568453595026 ) ) ;
#70793 = CARTESIAN_POINT ( 'NONE',  ( 22.26659068614895176, 9.720415501580633943, -7.082119434687042414 ) ) ;
#70794 = CARTESIAN_POINT ( 'NONE',  ( 10.00000000000000000, 14.75893115100078568, -9.846743663894594434 ) ) ;
#70795 = CARTESIAN_POINT ( 'NONE',  ( 22.81628187352647785, 36.62363466993041783, 6.195893100308588602E-16 ) ) ;
#70797 = DIRECTION ( 'NONE',  ( 0.7353630527936759753, 0.6776733583268310657, -0.000000000000000000 ) ) ;
#70796 = CARTESIAN_POINT ( 'NONE',  ( -8.000000000000000000, 80.99999999999994316, -2.900000000000000799 ) ) ;
#70798 = CARTESIAN_POINT ( 'NONE',  ( 4.559911319644449179, 43.89701867748816966, 9.422509992056141925 ) ) ;
#70799 = EDGE_CURVE ( 'NONE', #97286, #13047, #15554, .T. ) ;
#70800 = CARTESIAN_POINT ( 'NONE',  ( 13.43411237798105340, 10.58196800326375353, 12.81628187352647963 ) ) ;
#70801 = DIRECTION ( 'NONE',  ( -1.000000000000000000, 0.000000000000000000, 0.000000000000000000 ) ) ;
#70802 = CARTESIAN_POINT ( 'NONE',  ( 17.20831665107776587, 32.88393115100078745, 7.208316651077764980 ) ) ;
#70803 = CARTESIAN_POINT ( 'NONE',  ( 2.791683348922237240, 15.38393115100078212, -7.208316651077763204 ) ) ;
#70804 = CARTESIAN_POINT ( 'NONE',  ( 0.5774900079438590739, 7.647018677488171434, -5.440088680355550821 ) ) ;
#70805 = CARTESIAN_POINT ( 'NONE',  ( 10.00000000000000000, 22.87363466993042138, -12.81628187352647608 ) ) ;
#70806 = CARTESIAN_POINT ( 'NONE',  ( 0.1532563361054083140, 21.00893115100078745, 1.131784320476157264E-15 ) ) ;
#70807 = CARTESIAN_POINT ( 'NONE',  ( -8.051923691749143686, 84.95650211105896688, 3.789018682291705797 ) ) ;
#70808 = EDGE_CURVE ( 'NONE', #89305, #74710, #66469, .T. ) ;
#70809 = CARTESIAN_POINT ( 'NONE',  ( 7.084665262690076126, 17.02201867748817676, -10.88017736071110164 ) ) ;
#70810 = ADVANCED_FACE ( 'NONE', ( #25019 ), #23547, .F. ) ;
#70811 = CARTESIAN_POINT ( 'NONE',  ( -0.8801773607111009756, 58.06368534415484106, 1.068504757029289695E-15 ) ) ;
#70812 = DIRECTION ( 'NONE',  ( 0.000000000000000000, -0.000000000000000000, -1.000000000000000000 ) ) ;
#70814 = CARTESIAN_POINT ( 'NONE',  ( 17.96484262340118221, 19.93868534415484106, 7.964842623401181321 ) ) ;
#70813 = CARTESIAN_POINT ( 'NONE',  ( 10.00000000000000000, 49.75893115100078745, -9.846743663894594434 ) ) ;
#70815 = SURFACE_STYLE_USAGE ( .BOTH. , #71781 ) ;
#70816 = CARTESIAN_POINT ( 'NONE',  ( 15.44008868035555260, 44.73035201082151247, 9.422509992056143702 ) ) ;
#70818 = DIRECTION ( 'NONE',  ( -1.257568779154408793E-17, -1.000000000000000000, 0.000000000000000000 ) ) ;
#70817 = CARTESIAN_POINT ( 'NONE',  ( 12.91533473730993009, 16.60535201082150891, -10.88017736071109987 ) ) ;
#70819 = CARTESIAN_POINT ( 'NONE',  ( 18.52753015748618282, 13.92559781766745175, -4.923371831947291888 ) ) ;
#70820 = CARTESIAN_POINT ( 'NONE',  ( 2.791683348922240793, 41.63393115100078745, 7.208316651077764092 ) ) ;
#70821 = CARTESIAN_POINT ( 'NONE',  ( 17.99999999999999645, 78.65116497101854520, -3.750000000000000888 ) ) ;
#70822 = DIRECTION ( 'NONE',  ( 0.000000000000000000, -1.000000000000000000, 0.000000000000000000 ) ) ;
#70823 = CARTESIAN_POINT ( 'NONE',  ( -2.816281873526473856, -0.6680319967362464695, 3.434112377981055619 ) ) ;
#70824 = FACE_OUTER_BOUND ( 'NONE', #54050, .T. ) ;
#70825 = CARTESIAN_POINT ( 'NONE',  ( -0.3689425029237881626, 22.42874883491397142, 10.36894250292379027 ) ) ;
#70826 = CIRCLE ( 'NONE', #30834, 0.1000000000000001166 ) ;
#70827 = CARTESIAN_POINT ( 'NONE',  ( 17.20831665107776587, 42.88393115100077324, 7.208316651077764980 ) ) ;
#70828 = CARTESIAN_POINT ( 'NONE',  ( 2.897438467171757030E-16, 23.03999999999999915, 0.000000000000000000 ) ) ;
#70829 = ORIENTED_EDGE ( 'NONE', *, *, #54653, .T. ) ;
#70830 = CARTESIAN_POINT ( 'NONE',  ( 15.44008868035555793, 6.397018677488171434, -9.422509992056140149 ) ) ;
#70831 = CARTESIAN_POINT ( 'NONE',  ( 12.63842701281683922, 24.55059781766745175, -9.846743663894590881 ) ) ;
#70833 = FILL_AREA_STYLE ('',( #78808 ) ) ;
#70832 = CARTESIAN_POINT ( 'NONE',  ( -3.750000000000000000, 37.00000000000000000, -2.750000000000000000 ) ) ;
#70834 = CARTESIAN_POINT ( 'NONE',  ( 15.44008868035555260, 39.73035201082150536, 9.422509992056143702 ) ) ;
#70835 = CARTESIAN_POINT ( 'NONE',  ( 21.09922568453594849, 61.20696800326376064, 6.408140936763242479 ) ) ;
#70836 = CARTESIAN_POINT ( 'NONE',  ( 20.88017736071110875, 15.77201867748817143, -2.915334737309920765 ) ) ;
#70837 = CARTESIAN_POINT ( 'NONE',  ( 6.565887622018943937, 48.08196800326375353, -12.81628187352647608 ) ) ;
#70838 = CARTESIAN_POINT ( 'NONE',  ( -1.099225684535947600, 13.70696800326375353, -6.408140936763238038 ) ) ;
#70839 = CARTESIAN_POINT ( 'NONE',  ( 0.1532563361054100626, 20.80059781766744464, -2.638427012816831230 ) ) ;
#70840 = ORIENTED_EDGE ( 'NONE', *, *, #15254, .T. ) ;
#70841 = PRESENTATION_STYLE_ASSIGNMENT (( #9837 ) ) ;
#70842 = EDGE_CURVE ( 'NONE', #31369, #17262, #23652, .T. ) ;
#70843 = CARTESIAN_POINT ( 'NONE',  ( -4.164238869374098151, 56.59541550158063927, -3.795296366450310543 ) ) ;
#70844 = CARTESIAN_POINT ( 'NONE',  ( -2.266590686148945544, 27.22041550158063572, 7.082119434687048631 ) ) ;
#70845 = CARTESIAN_POINT ( 'NONE',  ( 7.084665262690076126, 24.10535201082150181, 10.88017736071109987 ) ) ;
#70846 = CARTESIAN_POINT ( 'NONE',  ( -0.8801773607111008646, 53.27201867748816966, 2.915334737309923430 ) ) ;
#70847 =( NAMED_UNIT ( * ) SI_UNIT ( $, .STERADIAN. ) SOLID_ANGLE_UNIT ( ) );
#70848 = CARTESIAN_POINT ( 'NONE',  ( 0.000000000000000000, 14.49999999999999822, 0.000000000000000000 ) ) ;
#70849 = CARTESIAN_POINT ( 'NONE',  ( 0.5774900079438590739, 62.64701867748817676, -5.440088680355550821 ) ) ;
#70850 = PLANE ( 'NONE',  #32186 ) ;
#70851 = CARTESIAN_POINT ( 'NONE',  ( 1.472469842513823179, 15.59226448433411960, -4.923371831947296329 ) ) ;
#70852 = CARTESIAN_POINT ( 'NONE',  ( 18.52753015748617571, 28.09226448433411960, 4.923371831947298993 ) ) ;
#70853 = CARTESIAN_POINT ( 'NONE',  ( 7.361572987183169658, 49.96726448433410894, -9.846743663894592657 ) ) ;
#70854 = CARTESIAN_POINT ( 'NONE',  ( 15.44008868035555260, 19.73035201082150536, 9.422509992056143702 ) ) ;
#70855 = CARTESIAN_POINT ( 'NONE',  ( -1.099225684535947600, 33.70696800326375353, -6.408140936763238038 ) ) ;
#70856 = MECHANICAL_DESIGN_GEOMETRIC_PRESENTATION_REPRESENTATION (  '', ( #93165 ), #94962 ) ;
#70857 = CARTESIAN_POINT ( 'NONE',  ( 2.035157376598824452, 48.68868534415483396, 7.964842623401179544 ) ) ;
#70858 = CARTESIAN_POINT ( 'NONE',  ( 17.20831665107776587, 34.13393115100078745, -7.208316651077762316 ) ) ;
#70860 = CARTESIAN_POINT ( 'NONE',  ( 18.52753015748618282, 18.92559781766745175, -4.923371831947291888 ) ) ;
#70859 = CARTESIAN_POINT ( 'NONE',  ( 24.16423886937410614, 49.30374883491396787, 8.672049930838204340E-16 ) ) ;
#70861 = CARTESIAN_POINT ( 'NONE',  ( 9.879999999999988347, 26.99999999999999645, 3.000000000000000000 ) ) ;
#70862 = CARTESIAN_POINT ( 'NONE',  ( 1.472469842513823179, 55.59226448433412315, -4.923371831947296329 ) ) ;
#70864 = CARTESIAN_POINT ( 'NONE',  ( 20.36894250292379738, 14.92874883491396432, -10.36894250292379027 ) ) ;
#70863 = CARTESIAN_POINT ( 'NONE',  ( 1.472469842513823179, 26.42559781766745175, 4.923371831947296329 ) ) ;
#70865 = CARTESIAN_POINT ( 'NONE',  ( 20.36894250292379738, 14.92874883491396432, -10.36894250292379027 ) ) ;
#70866 = CARTESIAN_POINT ( 'NONE',  ( 1.472469842513823179, 36.42559781766745175, 4.923371831947296329 ) ) ;
#70867 = CARTESIAN_POINT ( 'NONE',  ( 10.00000000000000000, 46.81368534415484106, -10.88017736071110342 ) ) ;
#70868 = CARTESIAN_POINT ( 'NONE',  ( 12.91533473730993009, 21.60535201082150536, -10.88017736071109987 ) ) ;
#70869 = STYLED_ITEM ( 'NONE', ( #62463 ), #93184 ) ;
#70870 = CARTESIAN_POINT ( 'NONE',  ( 17.96484262340118221, 39.93868534415484106, 7.964842623401181321 ) ) ;
#70871 = CARTESIAN_POINT ( 'NONE',  ( 7.084665262690076126, 27.02201867748817676, -10.88017736071110164 ) ) ;
#70872 = ORIENTED_EDGE ( 'NONE', *, *, #57176, .T. ) ;
#70873 = CARTESIAN_POINT ( 'NONE',  ( 22.81628187352647785, 36.62363466993041783, 6.195893100308588602E-16 ) ) ;
#70874 = CARTESIAN_POINT ( 'NONE',  ( 17.96484262340118221, 39.93868534415484106, 7.964842623401181321 ) ) ;
#70875 = ORIENTED_EDGE ( 'NONE', *, *, #29122, .F. ) ;
#70876 = CARTESIAN_POINT ( 'NONE',  ( 3.591859063236763294, 58.29030133659708923, -11.09922568453595026 ) ) ;
#70877 = CARTESIAN_POINT ( 'NONE',  ( 19.42250999205614193, 65.14701867748817676, 5.440088680355555262 ) ) ;
#70878 = VERTEX_POINT ( 'NONE', #17517 ) ;
#70879 = CARTESIAN_POINT ( 'NONE',  ( 7.084665262690076126, 67.02201867748817676, -10.88017736071110164 ) ) ;
#70880 = CARTESIAN_POINT ( 'NONE',  ( 5.817157072110800797, 15.00000000000000000, -13.82608706751086558 ) ) ;
#70881 = B_SPLINE_CURVE_WITH_KNOTS ( 'NONE', 3,
 ( #91118, #159, #21655, #8614 ),
 .UNSPECIFIED., .F., .F.,
 ( 4, 4 ),
 ( 9.320633277890009387E-17, 0.001060528352562005667 ),
 .UNSPECIFIED. ) ;
#70882 = CARTESIAN_POINT ( 'NONE',  ( 2.917880565312950480, 65.97041550158063217, -12.26659068614894821 ) ) ;
#70883 = CARTESIAN_POINT ( 'NONE',  ( 14.92337183194729988, 14.34226448433411782, -8.527530157486177487 ) ) ;
#70884 = CARTESIAN_POINT ( 'NONE',  ( -2.266590686148945544, 2.220415501580634388, 7.082119434687048631 ) ) ;
#70885 = CARTESIAN_POINT ( 'NONE',  ( 2.791683348922237240, 0.3839311510007847872, -7.208316651077763204 ) ) ;
#70886 = CARTESIAN_POINT ( 'NONE',  ( 15.44008868035555793, 6.397018677488170546, -9.422509992056140149 ) ) ;
#70887 = CARTESIAN_POINT ( 'NONE',  ( 5.076628168052703671, 41.84226448433411605, 8.527530157486179263 ) ) ;
#70888 = VERTEX_POINT ( 'NONE', #41499 ) ;
#70889 = CARTESIAN_POINT ( 'NONE',  ( 7.361572987183170547, 47.05059781766745175, 9.846743663894590881 ) ) ;
#70890 = DIRECTION ( 'NONE',  ( 0.000000000000000000, 0.000000000000000000, 1.000000000000000000 ) ) ;
#70891 = CARTESIAN_POINT ( 'NONE',  ( 4.559911319644449179, 42.23035201082151247, -9.422509992056141925 ) ) ;
#70892 = CARTESIAN_POINT ( 'NONE',  ( 17.20831665107776587, 47.88393115100078745, 7.208316651077764980 ) ) ;
#70893 = CARTESIAN_POINT ( 'NONE',  ( 13.43411237798105340, 30.58196800326374998, 12.81628187352647963 ) ) ;
#70894 = DIRECTION ( 'NONE',  ( 1.000000000000000000, 0.000000000000000000, 1.224646799147353207E-16 ) ) ;
#70895 = CARTESIAN_POINT ( 'NONE',  ( 20.88017736071110519, 50.56368534415484106, 2.639326808657452039E-16 ) ) ;
#70896 = CARTESIAN_POINT ( 'NONE',  ( -0.8801773607110991993, 7.855352010821506248, -2.915334737309923874 ) ) ;
#70897 = EDGE_CURVE ( 'NONE', #40528, #85153, #71968, .T. ) ;
#70898 = CARTESIAN_POINT ( 'NONE',  ( -1.099225684535947600, 39.54030133659708923, 6.408140936763237150 ) ) ;
#70899 = ORIENTED_EDGE ( 'NONE', *, *, #55426, .F. ) ;
#70900 = CARTESIAN_POINT ( 'NONE',  ( 10.00000000000000178, 30.37363466993042138, 12.81628187352647608 ) ) ;
#70901 = CARTESIAN_POINT ( 'NONE',  ( 15.44008868035555793, 31.39701867748817676, -9.422509992056140149 ) ) ;
#70902 = VERTEX_POINT ( 'NONE', #64939 ) ;
#70903 = DIRECTION ( 'NONE',  ( 0.000000000000000000, 1.000000000000000000, 0.000000000000000000 ) ) ;
#70904 = B_SPLINE_CURVE_WITH_KNOTS ( 'NONE', 3,
 ( #35351, #88359, #45694, #37710, #19855, #38209 ),
 .UNSPECIFIED., .F., .F.,
 ( 4, 2, 4 ),
 ( 5.870982294470536311E-18, 0.0002626113303185901855, 0.0005252226606371745163 ),
 .UNSPECIFIED. ) ;
#70905 = CARTESIAN_POINT ( 'NONE',  ( 10.00000000000000178, 2.258931151000784787, 9.846743663894594434 ) ) ;
#70906 = CARTESIAN_POINT ( 'NONE',  ( 7.361572987183169658, 54.96726448433413026, -9.846743663894592657 ) ) ;
#70908 = CARTESIAN_POINT ( 'NONE',  ( 0.1532563361054083140, 36.00893115100078745, 1.131784320476157264E-15 ) ) ;
#70907 = CARTESIAN_POINT ( 'NONE',  ( 19.84674366389459266, 13.30059781766745353, 2.638427012816836559 ) ) ;
#70909 = CARTESIAN_POINT ( 'NONE',  ( -5.795997163830251431, 15.00000000000000000, 13.01802277140702024 ) ) ;
#70910 = CARTESIAN_POINT ( 'NONE',  ( -13.48255862861919852, 3.931018169630358772E-16, -5.335786055104346559 ) ) ;
#70911 = CARTESIAN_POINT ( 'NONE',  ( 1.472469842513823179, 30.59226448433411960, -4.923371831947296329 ) ) ;
#70912 = CARTESIAN_POINT ( 'NONE',  ( 15.08495336817614607, 15.00000000000000000, -5.321802168063438643 ) ) ;
#70913 = CARTESIAN_POINT ( 'NONE',  ( 17.39651004071838969, 59.08210964143329846, -6.500000000000027534 ) ) ;
#70915 = CARTESIAN_POINT ( 'NONE',  ( 0.7375392941517235901, 0.5000000000000004441, 14.98185688723471110 ) ) ;
#70914 = CARTESIAN_POINT ( 'NONE',  ( 7.361572987183170547, 32.05059781766745175, 9.846743663894590881 ) ) ;
#70916 = DIRECTION ( 'NONE',  ( 0.000000000000000000, 0.000000000000000000, 1.000000000000000000 ) ) ;
#70918 = ORIENTED_EDGE ( 'NONE', *, *, #47881, .T. ) ;
#70917 = CARTESIAN_POINT ( 'NONE',  ( 7.361572987183169658, 49.96726448433410894, -9.846743663894592657 ) ) ;
#70919 = B_SPLINE_CURVE_WITH_KNOTS ( 'NONE', 3,
 ( #97563, #21550, #6534, #25974, #69510, #10477 ),
 .UNSPECIFIED., .F., .F.,
 ( 4, 2, 4 ),
 ( 0.000000000000000000, 0.0002565770811490999926, 0.0005131541622981999852 ),
 .UNSPECIFIED. ) ;
#70920 = CARTESIAN_POINT ( 'NONE',  ( -0.8801773607111009756, 8.063685344154837509, 1.068504757029289695E-15 ) ) ;
#70921 = EDGE_CURVE ( 'NONE', #30230, #41646, #2929, .T. ) ;
#70922 = CARTESIAN_POINT ( 'NONE',  ( 22.81628187352647785, 26.62363466993042138, 6.195893100308588602E-16 ) ) ;
#70923 = DIRECTION ( 'NONE',  ( 0.6225146366376183016, 0.000000000000000000, -0.7826081568524148047 ) ) ;
#70924 = CARTESIAN_POINT ( 'NONE',  ( 24.16423886937410614, 44.30374883491397497, 8.672049930838204340E-16 ) ) ;
#70925 = CARTESIAN_POINT ( 'NONE',  ( 2.791683348922240793, 21.63393115100078745, 7.208316651077764092 ) ) ;
#70926 = B_SPLINE_CURVE_WITH_KNOTS ( 'NONE', 3,
 ( #62249, #76766, #15308, #90785, #45288, #75783 ),
 .UNSPECIFIED., .F., .F.,
 ( 4, 2, 4 ),
 ( 0.0002800671705680555569, 0.0006862730573397291499, 0.001092478944111402797 ),
 .UNSPECIFIED. ) ;
#70927 = EDGE_CURVE ( 'NONE', #98371, #28728, #18853, .T. ) ;
#70928 = CARTESIAN_POINT ( 'NONE',  ( 14.92337183194729988, 4.342264484334117824, -8.527530157486177487 ) ) ;
#70929 = DIRECTION ( 'NONE',  ( 0.9975640502598243087, -0.06975647374412535795, 0.000000000000000000 ) ) ;
#70930 = AXIS2_PLACEMENT_3D ( 'NONE', #16703, #2211, #87145 ) ;
#70931 = CARTESIAN_POINT ( 'NONE',  ( 17.08211943468705130, 43.47041550158063927, 12.26659068614894998 ) ) ;
#70932 = CARTESIAN_POINT ( 'NONE',  ( 17.20831665107776587, 54.13393115100079456, -7.208316651077762316 ) ) ;
#70933 = CARTESIAN_POINT ( 'NONE',  ( 4.559911319644449179, 12.23035201082150714, -9.422509992056141925 ) ) ;
#70934 = CARTESIAN_POINT ( 'NONE',  ( -4.164238869374099039, 21.80374883491396787, 8.674139862899312516E-16 ) ) ;
#70935 = CARTESIAN_POINT ( 'NONE',  ( 20.36894250292379738, 39.92874883491396787, -10.36894250292379027 ) ) ;
#70936 = CYLINDRICAL_SURFACE ( 'NONE', #10045, 2.999999999999999112 ) ;
#70937 = PRODUCT_DEFINITION ( 'UNKNOWN', '', #77461, #88487 ) ;
#70939 = CARTESIAN_POINT ( 'NONE',  ( 7.361572987183169658, 49.96726448433410894, -9.846743663894592657 ) ) ;
#70938 = CARTESIAN_POINT ( 'NONE',  ( 4.406185888756865232, -8.255243720450049949, 2.500000000000000000 ) ) ;
#70940 = ORIENTED_EDGE ( 'NONE', *, *, #87122, .F. ) ;
#70941 = CARTESIAN_POINT ( 'NONE',  ( 12.91533473730993009, 36.60535201082151247, -10.88017736071109987 ) ) ;
#70942 = CARTESIAN_POINT ( 'NONE',  ( 0.000000000000000000, 14.49999999999999822, 0.000000000000000000 ) ) ;
#70943 = CARTESIAN_POINT ( 'NONE',  ( 1.816707512666846824, 65.10290668512024581, -6.499999999999958256 ) ) ;
#70944 = CARTESIAN_POINT ( 'NONE',  ( 19.84674366389459266, 38.30059781766745175, 2.638427012816836559 ) ) ;
#70945 = CARTESIAN_POINT ( 'NONE',  ( 0.6178305044545818747, 63.49863466993043204, -9.382169495545419124 ) ) ;
#70946 = CARTESIAN_POINT ( 'NONE',  ( -10.36894250292378317, 12.42874883491396432, 10.36894250292379560 ) ) ;
#70947 = CARTESIAN_POINT ( 'NONE',  ( 10.00000000000000178, 47.25893115100078745, 9.846743663894594434 ) ) ;
#70948 = CARTESIAN_POINT ( 'NONE',  ( 14.92337183194729988, 64.34226448433412315, -8.527530157486177487 ) ) ;
#70949 = EDGE_LOOP ( 'NONE', ( #16719, #68008, #35316, #40860 ) ) ;
#70950 = CARTESIAN_POINT ( 'NONE',  ( 22.26659068614894466, 13.88708216824730179, 7.082119434687054849 ) ) ;
#70951 = CARTESIAN_POINT ( 'NONE',  ( -5.991992585808451288, 3.888230080364882544E-16, -13.20401548210303311 ) ) ;
#70952 = FILL_AREA_STYLE_COLOUR ( '', #14787 ) ;
#70953 = CARTESIAN_POINT ( 'NONE',  ( -0.8801773607110991993, 2.855352010821504471, -2.915334737309923874 ) ) ;
#70954 = CARTESIAN_POINT ( 'NONE',  ( 10.00000000000000000, 22.87363466993042138, -12.81628187352647608 ) ) ;
#70955 = LINE ( 'NONE', #39952, #9801 ) ;
#70956 = CARTESIAN_POINT ( 'NONE',  ( 2.035157376598824452, 63.68868534415484106, 7.964842623401179544 ) ) ;
#70957 = SURFACE_STYLE_USAGE ( .BOTH. , #77947 ) ;
#70958 = PRESENTATION_STYLE_ASSIGNMENT (( #40460 ) ) ;
#70959 = CARTESIAN_POINT ( 'NONE',  ( -8.900000000000000355, 75.73428692542562146, 2.900000000000000355 ) ) ;
#70960 = CARTESIAN_POINT ( 'NONE',  ( 10.00000000000000178, 9.313685344154839285, 10.88017736071110342 ) ) ;
#70961 = DIRECTION ( 'NONE',  ( 0.000000000000000000, 0.000000000000000000, 1.000000000000000000 ) ) ;
#70962 = CARTESIAN_POINT ( 'NONE',  ( 5.500000000000000000, 60.50000000000000000, -6.000000000000000000 ) ) ;
#70963 = CARTESIAN_POINT ( 'NONE',  ( 7.084665262690076126, 29.10535201082150181, 10.88017736071109987 ) ) ;
#70964 = CARTESIAN_POINT ( 'NONE',  ( 10.00000000000000178, 39.31368534415484106, 10.88017736071110342 ) ) ;
#70965 = CARTESIAN_POINT ( 'NONE',  ( 16.40814093676324603, 2.456968003263753531, -11.09922568453594671 ) ) ;
#70966 = FACE_OUTER_BOUND ( 'NONE', #97184, .T. ) ;
#70967 = CARTESIAN_POINT ( 'NONE',  ( 13.43411237798106583, 57.66530133659708923, -12.81628187352647252 ) ) ;
#70968 = CARTESIAN_POINT ( 'NONE',  ( 14.92337183194729633, 7.675597817667451750, 8.527530157486181039 ) ) ;
#70969 = ORIENTED_EDGE ( 'NONE', *, *, #19427, .F. ) ;
#70970 = CARTESIAN_POINT ( 'NONE',  ( 20.88017736071110519, 25.56368534415483751, 2.639326808657452039E-16 ) ) ;
#70971 = CARTESIAN_POINT ( 'NONE',  ( 13.43411237798106583, 27.66530133659708568, -12.81628187352647252 ) ) ;
#70972 = CARTESIAN_POINT ( 'NONE',  ( -6.581680125707232598, -88.31141629936868753, 2.500000000000000000 ) ) ;
#70973 = CARTESIAN_POINT ( 'NONE',  ( -1.099225684535947600, -1.293031996736246469, -6.408140936763238038 ) ) ;
#70974 = CARTESIAN_POINT ( 'NONE',  ( 19.42250999205614548, 45.98035201082150536, -5.440088680355545492 ) ) ;
#70975 = CARTESIAN_POINT ( 'NONE',  ( 14.92337183194729988, 9.342264484334119601, -8.527530157486177487 ) ) ;
#70976 = CARTESIAN_POINT ( 'NONE',  ( 13.43411237798105340, 40.58196800326375353, 12.81628187352647963 ) ) ;
#70978 = CARTESIAN_POINT ( 'NONE',  ( -5.817157072110618721, 14.63606918420059877, -13.82608706751098815 ) ) ;
#70977 = CARTESIAN_POINT ( 'NONE',  ( 2.035157376598824452, 63.68868534415484106, 7.964842623401179544 ) ) ;
#70979 = CARTESIAN_POINT ( 'NONE',  ( 18.17829156368510723, 54.16792564121899289, 6.499999999999959144 ) ) ;
#70980 = CARTESIAN_POINT ( 'NONE',  ( 6.565887622018943937, 60.16530133659707502, 12.81628187352647430 ) ) ;
#70981 = ORIENTED_EDGE ( 'NONE', *, *, #14605, .F. ) ;
#70982 = CARTESIAN_POINT ( 'NONE',  ( 17.75000000000000000, 84.07179676972448590, -12.00000000000000000 ) ) ;
#70983 = CARTESIAN_POINT ( 'NONE',  ( 15.44008868035555260, 9.730352010821505360, 9.422509992056143702 ) ) ;
#70985 = CARTESIAN_POINT ( 'NONE',  ( 10.00000000000000000, 15.55374883491396787, -14.16423886937410082 ) ) ;
#70984 = CARTESIAN_POINT ( 'NONE',  ( -1.099225684535947600, 48.70696800326375353, -6.408140936763238038 ) ) ;
#70986 = CARTESIAN_POINT ( 'NONE',  ( 0.1532563361054082862, 21.21726448433412315, 2.638427012816831674 ) ) ;
#70987 = CARTESIAN_POINT ( 'NONE',  ( 4.559911319644449179, 3.897018677488170990, 9.422509992056141925 ) ) ;
#70988 = CARTESIAN_POINT ( 'NONE',  ( 5.076628168052704559, 20.17559781766745175, -8.527530157486179263 ) ) ;
#70989 = CARTESIAN_POINT ( 'NONE',  ( -0.3689425029237898834, 51.17874883491397497, -10.36894250292378850 ) ) ;
#70990 = VERTEX_POINT ( 'NONE', #64453 ) ;
#70991 = CARTESIAN_POINT ( 'NONE',  ( 4.559911319644449179, 23.89701867748817321, 9.422509992056141925 ) ) ;
#70992 = DIRECTION ( 'NONE',  ( 0.000000000000000000, 0.000000000000000000, 1.000000000000000000 ) ) ;
#70993 = VERTEX_POINT ( 'NONE', #26957 ) ;
#70994 = ORIENTED_EDGE ( 'NONE', *, *, #27789, .T. ) ;
#70995 = CARTESIAN_POINT ( 'NONE',  ( 2.035157376598824452, 13.68868534415483751, 7.964842623401179544 ) ) ;
#70996 = CARTESIAN_POINT ( 'NONE',  ( 19.84674366389459266, 53.71726448433411605, -2.638427012816827677 ) ) ;
#70997 = CARTESIAN_POINT ( 'NONE',  ( 21.09922568453595559, 52.04030133659708923, -6.408140936763230044 ) ) ;
#70998 = CARTESIAN_POINT ( 'NONE',  ( -0.2418659066527782397, 5.116331881023271855, 6.114288769123032985 ) ) ;
#71001 = CARTESIAN_POINT ( 'NONE',  ( 24.16423886937410614, 19.51208216824729647, -3.795296366450302550 ) ) ;
#71000 = CARTESIAN_POINT ( 'NONE',  ( 10.19513985507825637, 0.5000000000000004441, 11.00268709613223983 ) ) ;
#70999 = CIRCLE ( 'NONE', #8667, 14.49999999999999822 ) ;
#71002 = CARTESIAN_POINT ( 'NONE',  ( 20.88017736071110164, 40.35535201082150536, 2.915334737309930979 ) ) ;
#71003 = CARTESIAN_POINT ( 'NONE',  ( 2.035157376598822676, 22.43868534415483396, -7.964842623401177768 ) ) ;
#71004 = CARTESIAN_POINT ( 'NONE',  ( 0.1532563361054100626, 55.80059781766745175, -2.638427012816831230 ) ) ;
#71005 = COLOUR_RGB ( '', 0.31764706, 0.68627451, 0.89019608) ;
#71006 = DIRECTION ( 'NONE',  ( -0.000000000000000000, 0.000000000000000000, 1.000000000000000000 ) ) ;
#71007 = CARTESIAN_POINT ( 'NONE',  ( 19.84674366389459621, 38.50893115100078745, 7.409399052514197653E-17 ) ) ;
#71008 = CIRCLE ( 'NONE', #10325, 0.2500000000000002220 ) ;
#71009 = CARTESIAN_POINT ( 'NONE',  ( 5.076628168052704559, 5.175597817667451750, -8.527530157486179263 ) ) ;
#71010 = CARTESIAN_POINT ( 'NONE',  ( -2.638427012816840111, 29.96726448433413381, -9.846743663894590881 ) ) ;
#71011 = VERTEX_POINT ( 'NONE', #57457 ) ;
#71012 = CARTESIAN_POINT ( 'NONE',  ( -19.89999999999999858, 92.00000000000000000, -7.750000000000000000 ) ) ;
#71013 = CARTESIAN_POINT ( 'NONE',  ( 12.63842701281683034, 17.46726448433411250, 9.846743663894596210 ) ) ;
#71014 = CARTESIAN_POINT ( 'NONE',  ( 10.00000000000000178, 5.373634669930420493, 12.81628187352647608 ) ) ;
#71015 = CARTESIAN_POINT ( 'NONE',  ( 20.88017736071110519, 45.56368534415484106, 2.639326808657452039E-16 ) ) ;
#71017 = CARTESIAN_POINT ( 'NONE',  ( -2.816281873526473856, 44.12363466993042493, 9.499525473075851096E-16 ) ) ;
#71016 = CARTESIAN_POINT ( 'NONE',  ( 4.559911319644449179, 2.230352010821504471, -9.422509992056141925 ) ) ;
#71018 = CARTESIAN_POINT ( 'NONE',  ( 13.79529636645030344, 33.26208216824730357, 14.16423886937410614 ) ) ;
#71019 = EDGE_CURVE ( 'NONE', #76182, #80952, #41984, .T. ) ;
#71020 = CIRCLE ( 'NONE', #31094, 1.249999999999987121 ) ;
#71021 = CARTESIAN_POINT ( 'NONE',  ( -2.816281873526473856, 54.33196800326376064, 3.434112377981055619 ) ) ;
#71022 = ORIENTED_EDGE ( 'NONE', *, *, #88542, .F. ) ;
#71023 =( BOUNDED_CURVE ( )  B_SPLINE_CURVE ( 2, ( #4898, #19886, #89369, #72879, #4414, #50378, #28376, #80397, #43855 ),
 .UNSPECIFIED., .F., .F. ) 
 B_SPLINE_CURVE_WITH_KNOTS ( ( 3, 2, 2, 2, 3 ),
 ( 0.2248575172211797479, 0.2261904761904761918, 0.2321428571428571508, 0.2380952380952380820, 0.2394281970645344149 ),
 .UNSPECIFIED. ) 
 CURVE ( )  GEOMETRIC_REPRESENTATION_ITEM ( )  RATIONAL_B_SPLINE_CURVE ( ( 0.9881565478350731180, 0.9923695281211489805, 1.000000000000000000, 0.9659258262890683122, 1.000000000000000000, 0.9659258262890683122, 1.000000000000000000, 0.9923695281211495356, 0.9881565478350737841 ) ) 
 REPRESENTATION_ITEM ( '' )  );
#71024 = CARTESIAN_POINT ( 'NONE',  ( 0.1532563361054082862, 61.21726448433412315, 2.638427012816831674 ) ) ;
#71025 = CARTESIAN_POINT ( 'NONE',  ( 0.5774900079438590739, 22.64701867748817321, -5.440088680355550821 ) ) ;
#71026 = ORIENTED_EDGE ( 'NONE', *, *, #67589, .F. ) ;
#71027 = CARTESIAN_POINT ( 'NONE',  ( 7.084665262690076126, 69.10535201082151957, 10.88017736071109987 ) ) ;
#71028 = DIRECTION ( 'NONE',  ( 0.000000000000000000, 0.000000000000000000, 1.000000000000000000 ) ) ;
#71029 = CARTESIAN_POINT ( 'NONE',  ( 19.84674366389459266, 3.717264484334118713, -2.638427012816827677 ) ) ;
#71030 = CARTESIAN_POINT ( 'NONE',  ( 7.361572987183170547, 2.050597817667451750, 9.846743663894590881 ) ) ;
#71031 =( NAMED_UNIT ( * ) PLANE_ANGLE_UNIT ( ) SI_UNIT ( $, .RADIAN. ) );
#71032 = COLOUR_RGB ( '', 0.09019608, 0.27058824, 0.51372549) ;
#71034 = PRESENTATION_STYLE_ASSIGNMENT (( #70538 ) ) ;
#71033 = CARTESIAN_POINT ( 'NONE',  ( 17.96484262340118221, 59.93868534415484106, 7.964842623401181321 ) ) ;
#71035 = CARTESIAN_POINT ( 'NONE',  ( 2.035157376598824452, 68.68868534415484817, 7.964842623401179544 ) ) ;
#71037 = ORIENTED_EDGE ( 'NONE', *, *, #29663, .F. ) ;
#71036 = CARTESIAN_POINT ( 'NONE',  ( 17.20831665107776587, 9.133931151000787452, -7.208316651077762316 ) ) ;
#71038 = CARTESIAN_POINT ( 'NONE',  ( 14.22792531055119092, -2.184074454495212635E-15, 3.387425595041200665 ) ) ;
#71039 = EDGE_CURVE ( 'NONE', #8055, #55012, #67730, .T. ) ;
#71040 = CARTESIAN_POINT ( 'NONE',  ( 0.1532563361054082862, 51.21726448433412315, 2.638427012816831674 ) ) ;
#71041 = ORIENTED_EDGE ( 'NONE', *, *, #73190, .T. ) ;
#71042 = VERTEX_POINT ( 'NONE', #88943 ) ;
#71043 = CARTESIAN_POINT ( 'NONE',  ( -7.750000000000000000, 80.32179676972448590, 4.250000000000000000 ) ) ;
#71044 = CARTESIAN_POINT ( 'NONE',  ( 2.917880565312950480, 5.970415501580634832, -12.26659068614894821 ) ) ;
#71045 = CARTESIAN_POINT ( 'NONE',  ( -2.816281873526473856, 54.33196800326376064, 3.434112377981055619 ) ) ;
#71046 = CARTESIAN_POINT ( 'NONE',  ( 2.917880565312950480, 5.970415501580634832, -12.26659068614894821 ) ) ;
#71047 = CARTESIAN_POINT ( 'NONE',  ( 24.16423886937410614, 39.30374883491396787, 8.672049930838204340E-16 ) ) ;
#71048 = LINE ( 'NONE', #3538, #29022 ) ;
#71049 = CARTESIAN_POINT ( 'NONE',  ( 20.88017736071110875, 25.77201867748816966, -2.915334737309920765 ) ) ;
#71050 = DIRECTION ( 'NONE',  ( 1.000000000000000000, 0.000000000000000000, -0.000000000000000000 ) ) ;
#71051 = ORIENTED_EDGE ( 'NONE', *, *, #3851, .F. ) ;
#71052 = CARTESIAN_POINT ( 'NONE',  ( 17.20831665107776587, 2.883931151000785231, 7.208316651077764980 ) ) ;
#71053 = CARTESIAN_POINT ( 'NONE',  ( 14.92337183194729633, 12.67559781766745353, 8.527530157486181039 ) ) ;
#71054 = CARTESIAN_POINT ( 'NONE',  ( 10.00000000000000000, 32.87363466993042493, -12.81628187352647608 ) ) ;
#71055 = CARTESIAN_POINT ( 'NONE',  ( 5.076628168052703671, 41.84226448433411605, 8.527530157486179263 ) ) ;
#71056 = DIRECTION ( 'NONE',  ( 1.000000000000000000, 0.000000000000000000, 0.000000000000000000 ) ) ;
#71057 = CARTESIAN_POINT ( 'NONE',  ( 13.43411237798105340, 30.58196800326374998, 12.81628187352647963 ) ) ;
#71058 = CARTESIAN_POINT ( 'NONE',  ( 20.03932841506541251, 40.62161441960500952, -6.397827110479001433 ) ) ;
#71059 = CARTESIAN_POINT ( 'NONE',  ( 10.00000000000000178, 32.25893115100078745, 9.846743663894594434 ) ) ;
#71060 = CARTESIAN_POINT ( 'NONE',  ( 24.16423886937410614, 19.51208216824729647, -3.795296366450302550 ) ) ;
#71061 = ORIENTED_EDGE ( 'NONE', *, *, #9519, .T. ) ;
#71062 = CARTESIAN_POINT ( 'NONE',  ( 10.00000000000000000, 31.81368534415483751, -10.88017736071110342 ) ) ;
#71063 = CARTESIAN_POINT ( 'NONE',  ( 2.917880565312950480, 25.97041550158063572, -12.26659068614894821 ) ) ;
#71064 = CARTESIAN_POINT ( 'NONE',  ( 19.84674366389459266, 48.30059781766745175, 2.638427012816836559 ) ) ;
#71065 = CARTESIAN_POINT ( 'NONE',  ( 17.20831665107776587, 17.88393115100078745, 7.208316651077764980 ) ) ;
#71067 = CYLINDRICAL_SURFACE ( 'NONE', #95948, 11.92686044187656513 ) ;
#71066 = CARTESIAN_POINT ( 'NONE',  ( -1.099225684535947600, 54.54030133659708923, 6.408140936763237150 ) ) ;
#71068 = CARTESIAN_POINT ( 'NONE',  ( 7.084665262690076126, 34.10535201082151247, 10.88017736071109987 ) ) ;
#71069 = CARTESIAN_POINT ( 'NONE',  ( 20.15039907845753220, 22.62777174578612716, -6.262539305110077947 ) ) ;
#71070 = EDGE_CURVE ( 'NONE', #32615, #94433, #51935, .T. ) ;
#71071 = CARTESIAN_POINT ( 'NONE',  ( -2.816281873526473856, 24.12363466993042138, 9.499525473075851096E-16 ) ) ;
#71072 = CARTESIAN_POINT ( 'NONE',  ( 17.20831665107776587, 42.88393115100077324, 7.208316651077764980 ) ) ;
#71073 = CARTESIAN_POINT ( 'NONE',  ( 10.88017736071109987, 5.772018677488179428, -2.915334737309928315 ) ) ;
#71074 = CARTESIAN_POINT ( 'NONE',  ( 0.6178305044545818747, 43.49863466993042493, -9.382169495545419124 ) ) ;
#71076 = CARTESIAN_POINT ( 'NONE',  ( 13.82192141328809676, 4.465570197798056962E-16, 4.382292601468775750 ) ) ;
#71075 = CARTESIAN_POINT ( 'NONE',  ( 19.42250999205614193, 50.14701867748817676, 5.440088680355555262 ) ) ;
#71077 = ADVANCED_FACE ( 'NONE', ( #50444 ), #66431, .F. ) ;
#71078 = CARTESIAN_POINT ( 'NONE',  ( -11.05191079938453491, -57.06817940849906989, 4.000000000000000000 ) ) ;
#71079 =( NAMED_UNIT ( * ) SI_UNIT ( $, .STERADIAN. ) SOLID_ANGLE_UNIT ( ) );
#71080 = CARTESIAN_POINT ( 'NONE',  ( 0.5774900079438590739, 52.64701867748817676, -5.440088680355550821 ) ) ;
#71081 = CARTESIAN_POINT ( 'NONE',  ( 7.084665262690076126, 52.02201867748816255, -10.88017736071110164 ) ) ;
#71082 = DIRECTION ( 'NONE',  ( -0.000000000000000000, -1.000000000000000000, -0.000000000000000000 ) ) ;
#71083 = STYLED_ITEM ( 'NONE', ( #98277 ), #7689 ) ;
#71084 = CARTESIAN_POINT ( 'NONE',  ( -13.69999999999999751, 99.99999999999998579, 8.000000000000000000 ) ) ;
#71085 = CARTESIAN_POINT ( 'NONE',  ( 0.5774900079438607392, 3.480352010821504916, 5.440088680355550821 ) ) ;
#71086 = CARTESIAN_POINT ( 'NONE',  ( 3.591859063236761518, -0.04303199673624671928, 11.09922568453594849 ) ) ;
#71088 = DIRECTION ( 'NONE',  ( 0.000000000000000000, -0.000000000000000000, -1.000000000000000000 ) ) ;
#71087 = CARTESIAN_POINT ( 'NONE',  ( 12.91533473730993009, 26.60535201082150536, -10.88017736071109987 ) ) ;
#71089 = CARTESIAN_POINT ( 'NONE',  ( -2.816281873526473856, 29.33196800326376064, 3.434112377981055619 ) ) ;
#71090 = ORIENTED_EDGE ( 'NONE', *, *, #90955, .F. ) ;
#71091 = CARTESIAN_POINT ( 'NONE',  ( 20.88017736071110519, 50.56368534415484106, 2.639326808657452039E-16 ) ) ;
#71092 = CARTESIAN_POINT ( 'NONE',  ( 2.791683348922240793, 36.63393115100078035, 7.208316651077764092 ) ) ;
#71094 = CARTESIAN_POINT ( 'NONE',  ( -12.83294900548068895, 0.5000000000000004441, 7.766300266068274283 ) ) ;
#71093 = CARTESIAN_POINT ( 'NONE',  ( -1.099225684535947600, 3.706968003263753531, -6.408140936763238038 ) ) ;
#71095 = CARTESIAN_POINT ( 'NONE',  ( 20.88017736071110164, 30.35535201082151247, 2.915334737309930979 ) ) ;
#71096 = CARTESIAN_POINT ( 'NONE',  ( 15.44008868035555260, 39.73035201082150536, 9.422509992056143702 ) ) ;
#71097 = CARTESIAN_POINT ( 'NONE',  ( 24.16423886937410614, 54.30374883491396787, 8.672049930838204340E-16 ) ) ;
#71098 = CARTESIAN_POINT ( 'NONE',  ( 2.791683348922240793, 36.63393115100078035, 7.208316651077764092 ) ) ;
#71099 = CARTESIAN_POINT ( 'NONE',  ( 2.035157376598822676, 62.43868534415483396, -7.964842623401177768 ) ) ;
#71100 = LINE ( 'NONE', #50060, #10687 ) ;
#71101 = CARTESIAN_POINT ( 'NONE',  ( 24.16423886937409904, 14.09541550158063217, 3.795296366450317205 ) ) ;
#71102 =( GEOMETRIC_REPRESENTATION_CONTEXT ( 3 ) GLOBAL_UNCERTAINTY_ASSIGNED_CONTEXT ( ( #81287 ) ) GLOBAL_UNIT_ASSIGNED_CONTEXT ( ( #85310, #9808, #40309 ) ) REPRESENTATION_CONTEXT ( 'NONE', 'WORKASPACE' ) );
#71103 = LINE ( 'NONE', #25128, #19393 ) ;
#71104 = CARTESIAN_POINT ( 'NONE',  ( 0.000000000000000000, 0.5000000000000004441, 0.000000000000000000 ) ) ;
#71105 = B_SPLINE_CURVE_WITH_KNOTS ( 'NONE', 3,
 ( #42257, #94757, #79756, #48756, #35224, #41772 ),
 .UNSPECIFIED., .F., .F.,
 ( 4, 2, 4 ),
 ( 5.553824967135426632E-18, 0.0002605067024380912301, 0.0005210134048761769308 ),
 .UNSPECIFIED. ) ;
#71106 = ORIENTED_EDGE ( 'NONE', *, *, #5216, .F. ) ;
#71107 = CARTESIAN_POINT ( 'NONE',  ( 17.08211943468705840, 55.13708216824731068, -12.26659068614894466 ) ) ;
#71108 = CARTESIAN_POINT ( 'NONE',  ( 17.08211943468705130, 33.47041550158063927, 12.26659068614894998 ) ) ;
#71109 = CARTESIAN_POINT ( 'NONE',  ( 19.84674366389459266, 23.30059781766745530, 2.638427012816836559 ) ) ;
#71111 = CARTESIAN_POINT ( 'NONE',  ( 3.591859063236763294, 13.29030133659708746, -11.09922568453595026 ) ) ;
#71110 = VECTOR ( 'NONE', #66253, 1000.000000000000000 ) ;
#71112 = CARTESIAN_POINT ( 'NONE',  ( 0.1532563361054082862, 61.21726448433412315, 2.638427012816831674 ) ) ;
#71113 = DIRECTION ( 'NONE',  ( 0.000000000000000000, 0.000000000000000000, -1.000000000000000000 ) ) ;
#71115 = CARTESIAN_POINT ( 'NONE',  ( 3.591859063236761518, 29.95696800326375708, 11.09922568453594849 ) ) ;
#71114 = CARTESIAN_POINT ( 'NONE',  ( 15.44008868035555260, 59.73035201082151247, 9.422509992056143702 ) ) ;
#71116 = CARTESIAN_POINT ( 'NONE',  ( 17.08211943468705130, 43.47041550158063927, 12.26659068614894998 ) ) ;
#71117 = CARTESIAN_POINT ( 'NONE',  ( 19.42250999205614548, 25.98035201082150891, -5.440088680355545492 ) ) ;
#71118 = CARTESIAN_POINT ( 'NONE',  ( 4.547378612396755670, 0.000000000000000000, 3.009844244835539584 ) ) ;
#71119 = FILL_AREA_STYLE ('',( #41122 ) ) ;
#71120 = CARTESIAN_POINT ( 'NONE',  ( 8.527530157486179263, -6.907735515665875958, 4.923371831947292776 ) ) ;
#71121 = CARTESIAN_POINT ( 'NONE',  ( 10.00000000000000178, 7.258931151000785675, 9.846743663894594434 ) ) ;
#71122 = ORIENTED_EDGE ( 'NONE', *, *, #17117, .T. ) ;
#71123 = VECTOR ( 'NONE', #65979, 1000.000000000000114 ) ;
#71124 = CARTESIAN_POINT ( 'NONE',  ( 3.969999999999999751, 10.25000000000000000, 2.500000000000000000 ) ) ;
#71125 = DIRECTION ( 'NONE',  ( 0.9970872288863208421, 0.07626964003977952655, 0.000000000000000000 ) ) ;
#71126 = ORIENTED_EDGE ( 'NONE', *, *, #52183, .T. ) ;
#71128 = CARTESIAN_POINT ( 'NONE',  ( 20.88017736071110875, 5.772018677488170546, -2.915334737309920765 ) ) ;
#71127 = CARTESIAN_POINT ( 'NONE',  ( 19.42250999205614193, 10.14701867748816966, 5.440088680355555262 ) ) ;
#71130 = CARTESIAN_POINT ( 'NONE',  ( 13.43411237798105340, 10.58196800326375353, 12.81628187352647963 ) ) ;
#71129 = CARTESIAN_POINT ( 'NONE',  ( 1.472469842513823179, 36.42559781766745175, 4.923371831947296329 ) ) ;
#71131 = DIRECTION ( 'NONE',  ( -3.552713678800500929E-14, 0.000000000000000000, 1.000000000000000000 ) ) ;
#71132 = ADVANCED_FACE ( 'NONE', ( #28437 ), #88449, .T. ) ;
#71134 = CARTESIAN_POINT ( 'NONE',  ( 22.81628187352648496, 16.83196800326374998, -3.434112377981050290 ) ) ;
#71133 = AXIS2_PLACEMENT_3D ( 'NONE', #12730, #5253, #95753 ) ;
#71135 = ORIENTED_EDGE ( 'NONE', *, *, #89073, .T. ) ;
#71136 = CARTESIAN_POINT ( 'NONE',  ( 13.79529636645031943, 40.34541550158063217, -14.16423886937409904 ) ) ;
#71137 = VERTEX_POINT ( 'NONE', #36935 ) ;
#71138 = CARTESIAN_POINT ( 'NONE',  ( 24.16423886937409904, 54.09541550158063217, 3.795296366450317205 ) ) ;
#71139 = VERTEX_POINT ( 'NONE', #96465 ) ;
#71140 = CARTESIAN_POINT ( 'NONE',  ( 20.88017736071110519, 30.56368534415484106, 2.639326808657452039E-16 ) ) ;
#71141 = CARTESIAN_POINT ( 'NONE',  ( 20.88017736071110519, 40.56368534415484106, 2.639326808657452039E-16 ) ) ;
#71142 = CARTESIAN_POINT ( 'NONE',  ( 10.00000000000000178, 39.31368534415484106, 10.88017736071110342 ) ) ;
#71143 = CARTESIAN_POINT ( 'NONE',  ( 12.91533473730992121, 59.52201867748816966, 10.88017736071110164 ) ) ;
#71144 = CARTESIAN_POINT ( 'NONE',  ( 20.88017736071110164, 30.35535201082151247, 2.915334737309930979 ) ) ;
#71146 = ORIENTED_EDGE ( 'NONE', *, *, #98339, .T. ) ;
#71145 = LINE ( 'NONE', #93638, #36139 ) ;
#71147 = AXIS2_PLACEMENT_3D ( 'NONE', #84955, #77441, #39470 ) ;
#71148 = EDGE_CURVE ( 'NONE', #34811, #52108, #63692, .T. ) ;
#71149 = CARTESIAN_POINT ( 'NONE',  ( 17.20831665107776587, 12.88393115100078390, 7.208316651077764980 ) ) ;
#71150 = CARTESIAN_POINT ( 'NONE',  ( -5.328486666281220252, -28.65465727419596931, 2.499999999998389288 ) ) ;
#71151 = EDGE_LOOP ( 'NONE', ( #56117, #81570, #73075, #37865 ) ) ;
#71152 = CARTESIAN_POINT ( 'NONE',  ( -6.732636091893168029, -88.11213685669366669, 3.250000000000000000 ) ) ;
#71153 = CARTESIAN_POINT ( 'NONE',  ( 12.63842701281683034, 42.46726448433412315, 9.846743663894596210 ) ) ;
#71154 = DIRECTION ( 'NONE',  ( -0.000000000000000000, -1.000000000000000000, -0.000000000000000000 ) ) ;
#71155 = ADVANCED_FACE ( 'NONE', ( #21437 ), #20948, .F. ) ;
#71156 = FACE_OUTER_BOUND ( 'NONE', #94219, .T. ) ;
#71157 = ORIENTED_EDGE ( 'NONE', *, *, #26397, .F. ) ;
#71158 = CARTESIAN_POINT ( 'NONE',  ( -1.796645268984514487, 0.2306972965111897533, -14.83273813124061036 ) ) ;
#71159 = FACE_OUTER_BOUND ( 'NONE', #85003, .T. ) ;
#71160 = CARTESIAN_POINT ( 'NONE',  ( 0.1532563361054083140, 61.00893115100078745, 1.131784320476157264E-15 ) ) ;
#71161 = CARTESIAN_POINT ( 'NONE',  ( 17.08211943468705130, 48.47041550158063927, 12.26659068614894998 ) ) ;
#71162 = SPHERICAL_SURFACE ( 'NONE', #45071, 0.5000000000000000000 ) ;
#71163 = ORIENTED_EDGE ( 'NONE', *, *, #82772, .T. ) ;
#71164 = DIRECTION ( 'NONE',  ( 0.000000000000000000, -1.000000000000000000, 0.000000000000000000 ) ) ;
#71165 = CARTESIAN_POINT ( 'NONE',  ( 12.63842701281683922, 24.55059781766745175, -9.846743663894590881 ) ) ;
#71166 = PLANE ( 'NONE',  #57906 ) ;
#71167 = MECHANICAL_DESIGN_GEOMETRIC_PRESENTATION_REPRESENTATION (  '', ( #66296 ), #12060 ) ;
#71168 = CARTESIAN_POINT ( 'NONE',  ( 19.84674366389459621, 63.50893115100078745, 7.409399052514197653E-17 ) ) ;
#71169 = CARTESIAN_POINT ( 'NONE',  ( 7.361572987183169658, -0.03273551566588185635, -9.846743663894592657 ) ) ;
#71170 = CYLINDRICAL_SURFACE ( 'NONE', #92054, 0.5000000000000004441 ) ;
#71171 = CARTESIAN_POINT ( 'NONE',  ( 18.52753015748617571, 43.09226448433412315, 4.923371831947298993 ) ) ;
#71172 = PLANE ( 'NONE',  #58444 ) ;
#71173 = CIRCLE ( 'NONE', #35832, 15.00000000000000000 ) ;
#71174 = ORIENTED_EDGE ( 'NONE', *, *, #93367, .F. ) ;
#71175 = CARTESIAN_POINT ( 'NONE',  ( 13.79529636645030344, 63.26208216824730357, 14.16423886937410614 ) ) ;
#71176 = CARTESIAN_POINT ( 'NONE',  ( 9.159723438033203990, 15.00000000000000000, -10.91613331444542645 ) ) ;
#71177 = CARTESIAN_POINT ( 'NONE',  ( -0.8801773607111008646, 43.27201867748817676, 2.915334737309923430 ) ) ;
#71179 = CARTESIAN_POINT ( 'NONE',  ( 1.379999999999981908, 20.99999999999999645, 0.000000000000000000 ) ) ;
#71178 = CARTESIAN_POINT ( 'NONE',  ( 13.43411237798106583, 7.665301336597086568, -12.81628187352647252 ) ) ;
#71180 = CARTESIAN_POINT ( 'NONE',  ( -0.1503990784575247319, 62.22266099184918176, -6.262539305110083276 ) ) ;
#71181 = LINE ( 'NONE', #57518, #4489 ) ;
#71182 = CARTESIAN_POINT ( 'NONE',  ( -15.99538290524656503, -0.03417435944610275333, -0.1584996864330918964 ) ) ;
#71183 = CARTESIAN_POINT ( 'NONE',  ( -0.1049300847420627930, 62.21697413083880690, -6.336235997365760042 ) ) ;
#71184 = CARTESIAN_POINT ( 'NONE',  ( 2.791683348922237240, 55.38393115100078745, -7.208316651077763204 ) ) ;
#71185 = CARTESIAN_POINT ( 'NONE',  ( 5.076628168052704559, 0.1755978176674514724, -8.527530157486179263 ) ) ;
#71186 = CARTESIAN_POINT ( 'NONE',  ( -12.26659068614895354, 31.38708216824731423, -7.082119434687038861 ) ) ;
#71187 = CARTESIAN_POINT ( 'NONE',  ( 10.00000000000000178, 5.373634669930420493, 12.81628187352647608 ) ) ;
#71189 = LINE ( 'NONE', #94166, #72877 ) ;
#71188 = CARTESIAN_POINT ( 'NONE',  ( 19.42250999205614193, 10.14701867748816966, 5.440088680355555262 ) ) ;
#71190 = FACE_OUTER_BOUND ( 'NONE', #10731, .T. ) ;
#71191 = CARTESIAN_POINT ( 'NONE',  ( -4.164238869374098151, 31.59541550158063927, -3.795296366450310543 ) ) ;
#71192 = ADVANCED_FACE ( 'NONE', ( #58430 ), #44907, .T. ) ;
#71193 = CARTESIAN_POINT ( 'NONE',  ( 2.917880565312948704, 32.63708216824730357, 12.26659068614894643 ) ) ;
#71194 = CARTESIAN_POINT ( 'NONE',  ( -2.266590686148945544, 61.38708216824730357, -7.082119434687050408 ) ) ;
#71195 = CARTESIAN_POINT ( 'NONE',  ( 19.84674366389459266, 33.30059781766744464, 2.638427012816836559 ) ) ;
#71196 = CARTESIAN_POINT ( 'NONE',  ( 13.43411237798106583, 42.66530133659707502, -12.81628187352647252 ) ) ;
#71197 = CARTESIAN_POINT ( 'NONE',  ( 0.5774900079438590739, 17.64701867748817321, -5.440088680355550821 ) ) ;
#71198 = VECTOR ( 'NONE', #96337, 1000.000000000000000 ) ;
#71199 = VERTEX_POINT ( 'NONE', #4961 ) ;
#71200 = CARTESIAN_POINT ( 'NONE',  ( 18.52753015748618282, 38.92559781766745175, -4.923371831947291888 ) ) ;
#71201 = CARTESIAN_POINT ( 'NONE',  ( 19.42250999205614193, 40.14701867748817676, 5.440088680355555262 ) ) ;
#71202 = CARTESIAN_POINT ( 'NONE',  ( 3.591859063236763294, 3.290301336597087012, -11.09922568453595026 ) ) ;
#71204 = DIRECTION ( 'NONE',  ( 0.2503800040544526539, 0.000000000000000000, -0.9681476403781048568 ) ) ;
#71203 = CARTESIAN_POINT ( 'NONE',  ( 2.917880565312948704, 27.63708216824730357, 12.26659068614894643 ) ) ;
#71205 = CARTESIAN_POINT ( 'NONE',  ( -13.78891971893199830, 15.00000000000000000, -5.904717858191724567 ) ) ;
#71206 = UNCERTAINTY_MEASURE_WITH_UNIT (LENGTH_MEASURE( 1.000000000000000082E-05 ), #33757, 'distance_accuracy_value', 'NONE');
#71207 = CARTESIAN_POINT ( 'NONE',  ( 1.472469842513823179, 25.59226448433412315, -4.923371831947296329 ) ) ;
#71208 = CARTESIAN_POINT ( 'NONE',  ( 3.591859063236761518, 49.95696800326375353, 11.09922568453594849 ) ) ;
#71209 = CARTESIAN_POINT ( 'NONE',  ( 12.63842701281683922, 54.55059781766745175, -9.846743663894590881 ) ) ;
#71210 = ORIENTED_EDGE ( 'NONE', *, *, #38127, .F. ) ;
#71211 = CARTESIAN_POINT ( 'NONE',  ( 1.274849032794131976, 13.57228050351029403, 6.499999999999760192 ) ) ;
#71212 = CARTESIAN_POINT ( 'NONE',  ( -5.419894505350723257, 14.49999999999999112, 13.98659156302460183 ) ) ;
#71213 = CARTESIAN_POINT ( 'NONE',  ( -4.164238869374098151, 66.59541550158060375, -3.795296366450310543 ) ) ;
#71214 = CARTESIAN_POINT ( 'NONE',  ( -0.3689425029237898834, 16.17874883491396076, -10.36894250292378850 ) ) ;
#71215 = CARTESIAN_POINT ( 'NONE',  ( 0.5774900079438607392, 68.48035201082150536, 5.440088680355550821 ) ) ;
#71216 = CARTESIAN_POINT ( 'NONE',  ( 12.63842701281683034, 47.46726448433412315, 9.846743663894596210 ) ) ;
#71217 = CARTESIAN_POINT ( 'NONE',  ( 17.96484262340118221, 26.18868534415483396, -7.964842623401177768 ) ) ;
#71218 = LINE ( 'NONE', #80175, #84694 ) ;
#71219 = DIRECTION ( 'NONE',  ( -0.000000000000000000, -0.000000000000000000, 1.000000000000000000 ) ) ;
#71220 = DIRECTION ( 'NONE',  ( 0.000000000000000000, -1.000000000000000000, 0.000000000000000000 ) ) ;
#71221 = ORIENTED_EDGE ( 'NONE', *, *, #88945, .T. ) ;
#71222 = ORIENTED_EDGE ( 'NONE', *, *, #45945, .T. ) ;
#71223 = DIRECTION ( 'NONE',  ( 0.8320502943378436100, -0.5547001962252291474, 0.000000000000000000 ) ) ;
#71224 = CARTESIAN_POINT ( 'NONE',  ( 24.16423886937410614, 14.51208216824730179, -3.795296366450302550 ) ) ;
#71225 = FILL_AREA_STYLE ('',( #77234 ) ) ;
#71226 = CARTESIAN_POINT ( 'NONE',  ( 22.26659068614894466, 43.88708216824729647, 7.082119434687054849 ) ) ;
#71227 = CARTESIAN_POINT ( 'NONE',  ( 19.84674366389459621, 53.50893115100078745, 7.409399052514197653E-17 ) ) ;
#71228 = CARTESIAN_POINT ( 'NONE',  ( 1.472469842513823179, 26.42559781766745175, 4.923371831947296329 ) ) ;
#71229 = DIRECTION ( 'NONE',  ( 1.000000000000000000, 0.000000000000000000, 0.000000000000000000 ) ) ;
#71231 = CARTESIAN_POINT ( 'NONE',  ( 12.63842701281683922, 64.55059781766745175, -9.846743663894590881 ) ) ;
#71230 = CARTESIAN_POINT ( 'NONE',  ( 15.44008868035555260, 19.73035201082150536, 9.422509992056143702 ) ) ;
#71232 = CARTESIAN_POINT ( 'NONE',  ( 11.29222593019777499, 0.2306972965111881713, -9.783848334571253247 ) ) ;
#71233 = CARTESIAN_POINT ( 'NONE',  ( 17.08211943468705840, 35.13708216824730357, -12.26659068614894466 ) ) ;
#71234 = CARTESIAN_POINT ( 'NONE',  ( 0.5774900079438590739, 7.647018677488171434, -5.440088680355550821 ) ) ;
#71235 = CARTESIAN_POINT ( 'NONE',  ( 2.791683348922240793, 66.63393115100079456, 7.208316651077764092 ) ) ;
#71236 = EDGE_CURVE ( 'NONE', #69773, #41505, #66930, .T. ) ;
#71237 = CARTESIAN_POINT ( 'NONE',  ( -11.48952521350009448, 15.00000000000000000, -8.845383562533896793 ) ) ;
#71238 = CARTESIAN_POINT ( 'NONE',  ( 7.084665262690076126, 62.02201867748816966, -10.88017736071110164 ) ) ;
#71239 = CARTESIAN_POINT ( 'NONE',  ( 14.92337183194729988, 9.342264484334119601, -8.527530157486177487 ) ) ;
#71240 = CARTESIAN_POINT ( 'NONE',  ( 20.00000000000000355, 70.00000000000000000, -4.500000000000002665 ) ) ;
#71241 = ORIENTED_EDGE ( 'NONE', *, *, #4005, .F. ) ;
#71242 = DIRECTION ( 'NONE',  ( -0.000000000000000000, -1.000000000000000000, -0.000000000000000000 ) ) ;
#71243 = ORIENTED_EDGE ( 'NONE', *, *, #89428, .F. ) ;
#71244 = CARTESIAN_POINT ( 'NONE',  ( 0.1532563361054100626, 25.80059781766744820, -2.638427012816831230 ) ) ;
#71245 = ORIENTED_EDGE ( 'NONE', *, *, #83698, .F. ) ;
#71246 = AXIS2_PLACEMENT_3D ( 'NONE', #46904, #85409, #32886 ) ;
#71247 = CARTESIAN_POINT ( 'NONE',  ( -2.266590686148945544, 32.22041550158063927, 7.082119434687048631 ) ) ;
#71248 = CARTESIAN_POINT ( 'NONE',  ( 17.20831665107776587, 29.13393115100078390, -7.208316651077762316 ) ) ;
#71249 = CARTESIAN_POINT ( 'NONE',  ( 10.00000000000000178, 44.31368534415484106, 10.88017736071110342 ) ) ;
#71250 = LINE ( 'NONE', #2279, #79247 ) ;
#71251 = EDGE_CURVE ( 'NONE', #53769, #70273, #39744, .T. ) ;
#71252 = ORIENTED_EDGE ( 'NONE', *, *, #16957, .F. ) ;
#71253 = CARTESIAN_POINT ( 'NONE',  ( -0.8801773607111008646, 38.27201867748816255, 2.915334737309923430 ) ) ;
#71254 = EDGE_CURVE ( 'NONE', #29582, #46734, #57941, .T. ) ;
#71255 = CARTESIAN_POINT ( 'NONE',  ( 12.81628187352647252, -8.168031996736246469, -3.434112377981059172 ) ) ;
#71256 = ORIENTED_EDGE ( 'NONE', *, *, #30883, .T. ) ;
#71257 = CARTESIAN_POINT ( 'NONE',  ( -2.266590686148945544, 11.38708216824730179, -7.082119434687050408 ) ) ;
#71258 = ORIENTED_EDGE ( 'NONE', *, *, #27705, .F. ) ;
#71259 = ORIENTED_EDGE ( 'NONE', *, *, #96875, .F. ) ;
#71260 = CARTESIAN_POINT ( 'NONE',  ( 19.38216949554541557, 37.24863466993041783, -9.382169495545420901 ) ) ;
#71261 = CARTESIAN_POINT ( 'NONE',  ( 2.917880565312950480, 0.9704155015806342766, -12.26659068614894821 ) ) ;
#71262 = CARTESIAN_POINT ( 'NONE',  ( 14.92337183194729633, 17.67559781766745175, 8.527530157486181039 ) ) ;
#71263 = DIRECTION ( 'NONE',  ( -0.000000000000000000, -1.000000000000000000, -0.000000000000000000 ) ) ;
#71264 = CARTESIAN_POINT ( 'NONE',  ( 7.361572987183169658, 29.96726448433411960, -9.846743663894592657 ) ) ;
#71265 =( GEOMETRIC_REPRESENTATION_CONTEXT ( 3 ) GLOBAL_UNCERTAINTY_ASSIGNED_CONTEXT ( ( #15139 ) ) GLOBAL_UNIT_ASSIGNED_CONTEXT ( ( #11881, #14355, #54301 ) ) REPRESENTATION_CONTEXT ( 'NONE', 'WORKASPACE' ) );
#71267 = CIRCLE ( 'NONE', #23394, 15.00000000000000000 ) ;
#71266 = CARTESIAN_POINT ( 'NONE',  ( 20.88017736071110164, 60.35535201082151957, 2.915334737309930979 ) ) ;
#71268 = EDGE_CURVE ( 'NONE', #27691, #94289, #73256, .T. ) ;
#71269 = CARTESIAN_POINT ( 'NONE',  ( 20.32896413005680714, 65.57879003517447813, -5.963430220938276349 ) ) ;
#71270 = CARTESIAN_POINT ( 'NONE',  ( 14.49120296996857959, 14.95077488074853456, -2.766068805437525757 ) ) ;
#71271 = CARTESIAN_POINT ( 'NONE',  ( -15.96747533562963994, 15.00000000000000000, 0.9576679184939570488 ) ) ;
#71272 = CARTESIAN_POINT ( 'NONE',  ( 2.603489959281581889, 20.43575266056827999, -6.499999999999995559 ) ) ;
#71273 = AXIS2_PLACEMENT_3D ( 'NONE', #74075, #18632, #51091 ) ;
#71274 = CARTESIAN_POINT ( 'NONE',  ( 15.00000000000000000, 77.07179676972447169, -4.250000000000000000 ) ) ;
#71275 = CARTESIAN_POINT ( 'NONE',  ( 7.361572987183170547, 7.050597817667451750, 9.846743663894590881 ) ) ;
#71276 = EDGE_CURVE ( 'NONE', #51412, #70611, #89329, .T. ) ;
#71277 = DIRECTION ( 'NONE',  ( 0.5547001962252290364, 0.8320502943378437211, 0.000000000000000000 ) ) ;
#71278 = CARTESIAN_POINT ( 'NONE',  ( 0.1532563361054083140, 51.00893115100078745, 1.131784320476157264E-15 ) ) ;
#71279 = CARTESIAN_POINT ( 'NONE',  ( 20.88017736071110519, 35.56368534415484106, 2.639326808657452039E-16 ) ) ;
#71280 = CARTESIAN_POINT ( 'NONE',  ( -0.3689425029237898834, 6.178748834913968757, -10.36894250292378850 ) ) ;
#71281 = CARTESIAN_POINT ( 'NONE',  ( 5.076628168052704559, 30.17559781766745175, -8.527530157486179263 ) ) ;
#71282 = CARTESIAN_POINT ( 'NONE',  ( -1.099225684535947600, 33.70696800326375353, -6.408140936763238038 ) ) ;
#71283 = SURFACE_STYLE_USAGE ( .BOTH. , #65223 ) ;
#71284 = CARTESIAN_POINT ( 'NONE',  ( 12.91533473730992121, 49.52201867748817676, 10.88017736071110164 ) ) ;
#71285 = CARTESIAN_POINT ( 'NONE',  ( 0.6178305044545818747, 3.498634669930420049, -9.382169495545419124 ) ) ;
#71286 = CARTESIAN_POINT ( 'NONE',  ( 4.838527690343521925, 14.63606918327236706, 14.19819177887734263 ) ) ;
#71287 = CARTESIAN_POINT ( 'NONE',  ( 5.076628168052704559, 25.17559781766745175, -8.527530157486179263 ) ) ;
#71288 = CARTESIAN_POINT ( 'NONE',  ( -0.8801773607111008646, 33.27201867748817676, 2.915334737309923430 ) ) ;
#71289 = CARTESIAN_POINT ( 'NONE',  ( -2.816281873526471635, 33.91530133659708213, -3.434112377981056508 ) ) ;
#71290 = AXIS2_PLACEMENT_3D ( 'NONE', #91708, #23227, #69209 ) ;
#71291 = CARTESIAN_POINT ( 'NONE',  ( 10.00000000000000000, 24.75893115100078745, -9.846743663894594434 ) ) ;
#71292 = CIRCLE ( 'NONE', #20171, 100.0000000000000000 ) ;
#71293 =( LENGTH_UNIT ( ) NAMED_UNIT ( * ) SI_UNIT ( .MILLI., .METRE. ) );
#71294 = CARTESIAN_POINT ( 'NONE',  ( 18.29284471827481795, 45.40189080397284016, -6.499999999999946709 ) ) ;
#71295 =( GEOMETRIC_REPRESENTATION_CONTEXT ( 3 ) GLOBAL_UNCERTAINTY_ASSIGNED_CONTEXT ( ( #40475 ) ) GLOBAL_UNIT_ASSIGNED_CONTEXT ( ( #19141, #3658, #64127 ) ) REPRESENTATION_CONTEXT ( 'NONE', 'WORKASPACE' ) );
#71296 = B_SPLINE_CURVE_WITH_KNOTS ( 'NONE', 3,
 ( #64830, #95348, #26846, #89326, #87835, #19354 ),
 .UNSPECIFIED., .F., .F.,
 ( 4, 2, 4 ),
 ( 3.409110551496216072E-05, 0.0004400426677368010999, 0.0008459942299586401069 ),
 .UNSPECIFIED. ) ;
#71297 = CARTESIAN_POINT ( 'NONE',  ( 20.88017736071110164, 20.35535201082150891, 2.915334737309930979 ) ) ;
#71298 = ORIENTED_EDGE ( 'NONE', *, *, #94836, .F. ) ;
#71299 = CARTESIAN_POINT ( 'NONE',  ( 20.88017736071110875, 55.77201867748816966, -2.915334737309920765 ) ) ;
#71301 = CARTESIAN_POINT ( 'NONE',  ( 2.035157376598822676, 27.43868534415483396, -7.964842623401177768 ) ) ;
#71300 = CARTESIAN_POINT ( 'NONE',  ( 19.84674366389459266, 43.30059781766744464, 2.638427012816836559 ) ) ;
#71302 = LINE ( 'NONE', #33273, #85437 ) ;
#71303 = CARTESIAN_POINT ( 'NONE',  ( -0.8801773607110991993, 52.85535201082151247, -2.915334737309923874 ) ) ;
#71305 = SURFACE_SIDE_STYLE ('',( #9309 ) ) ;
#71304 = CARTESIAN_POINT ( 'NONE',  ( 7.084665262690076126, 12.02201867748817321, -10.88017736071110164 ) ) ;
#71306 = LINE ( 'NONE', #2825, #16339 ) ;
#71307 = CARTESIAN_POINT ( 'NONE',  ( 19.84674366389459621, 33.50893115100078745, 7.409399052514197653E-17 ) ) ;
#71308 = CARTESIAN_POINT ( 'NONE',  ( 2.148416515056650766, 47.23726573380441351, 6.500000000000004441 ) ) ;
#71309 = PRESENTATION_LAYER_ASSIGNMENT (  '', '', ( #15448 ) ) ;
#71310 = DIRECTION ( 'NONE',  ( 0.000000000000000000, 0.000000000000000000, 1.000000000000000000 ) ) ;
#71311 = CYLINDRICAL_SURFACE ( 'NONE', #68147, 1.999999999999996669 ) ;
#71312 = CARTESIAN_POINT ( 'NONE',  ( 6.204703633549690345, 22.84541550158062861, 14.16423886937410082 ) ) ;
#71313 = DIRECTION ( 'NONE',  ( 0.9997628902338895340, -0.02177529129954166101, 0.000000000000000000 ) ) ;
#71314 = ORIENTED_EDGE ( 'NONE', *, *, #60187, .F. ) ;
#71315 = CARTESIAN_POINT ( 'NONE',  ( 6.204703633549690345, 60.76208216824730357, -14.16423886937410259 ) ) ;
#71316 = CARTESIAN_POINT ( 'NONE',  ( 19.84674366389459266, 28.30059781766745886, 2.638427012816836559 ) ) ;
#71318 = SURFACE_STYLE_FILL_AREA ( #70833 ) ;
#71317 =( NAMED_UNIT ( * ) PLANE_ANGLE_UNIT ( ) SI_UNIT ( $, .RADIAN. ) );
#71319 = CARTESIAN_POINT ( 'NONE',  ( 20.88017736071110164, 55.35535201082149825, 2.915334737309930979 ) ) ;
#71320 = CARTESIAN_POINT ( 'NONE',  ( -1.099225684535947600, 63.70696800326376774, -6.408140936763238038 ) ) ;
#71321 = PRESENTATION_LAYER_ASSIGNMENT (  '', '', ( #87220 ) ) ;
#71322 = CARTESIAN_POINT ( 'NONE',  ( 17.96484262340118221, 36.18868534415484106, -7.964842623401177768 ) ) ;
#71323 = CARTESIAN_POINT ( 'NONE',  ( 21.09922568453595559, 57.04030133659708923, -6.408140936763230044 ) ) ;
#71324 = CARTESIAN_POINT ( 'NONE',  ( 22.81628187352647785, 6.415301336597088344, 3.434112377981063169 ) ) ;
#71325 = CARTESIAN_POINT ( 'NONE',  ( 0.1532563361054082862, 11.21726448433411605, 2.638427012816831674 ) ) ;
#71326 = ORIENTED_EDGE ( 'NONE', *, *, #86042, .F. ) ;
#71327 = CARTESIAN_POINT ( 'NONE',  ( 10.00000000000000000, -0.2410688489992152128, -9.846743663894594434 ) ) ;
#71328 = CARTESIAN_POINT ( 'NONE',  ( 0.2751277870542912507, 20.30223176428831167, 6.499999999999992006 ) ) ;
#71329 = CARTESIAN_POINT ( 'NONE',  ( 17.08211943468705840, 50.13708216824730357, -12.26659068614894466 ) ) ;
#71330 = CARTESIAN_POINT ( 'NONE',  ( 10.00000000000000000, 25.55374883491396787, -14.16423886937410082 ) ) ;
#71331 = CARTESIAN_POINT ( 'NONE',  ( 19.42250999205614193, 45.14701867748817676, 5.440088680355555262 ) ) ;
#71332 = CARTESIAN_POINT ( 'NONE',  ( 0.2751277870542965243, 3.218334437839379891, 6.500000000000000888 ) ) ;
#71333 = DIRECTION ( 'NONE',  ( -0.000000000000000000, -0.000000000000000000, -1.000000000000000000 ) ) ;
#71334 = CARTESIAN_POINT ( 'NONE',  ( 7.361572987183169658, 9.967264484334119601, -9.846743663894592657 ) ) ;
#71335 = SURFACE_STYLE_FILL_AREA ( #85843 ) ;
#71336 = CARTESIAN_POINT ( 'NONE',  ( 14.92337183194729633, 17.67559781766745175, 8.527530157486181039 ) ) ;
#71337 = FILL_AREA_STYLE ('',( #78828 ) ) ;
#71338 = CYLINDRICAL_SURFACE ( 'NONE', #69132, 15.00000000000000000 ) ;
#71339 = CARTESIAN_POINT ( 'NONE',  ( 1.472469842513823179, 21.42559781766745175, 4.923371831947296329 ) ) ;
#71340 = CARTESIAN_POINT ( 'NONE',  ( 18.52753015748618282, 43.92559781766745175, -4.923371831947291888 ) ) ;
#71341 = CARTESIAN_POINT ( 'NONE',  ( 0.5774900079438607392, 28.48035201082150891, 5.440088680355550821 ) ) ;
#71342 = B_SPLINE_CURVE_WITH_KNOTS ( 'NONE', 3,
 ( #39526, #7057, #53027, #46516, #16028, #92504 ),
 .UNSPECIFIED., .F., .F.,
 ( 4, 2, 4 ),
 ( 3.409110551494637880E-05, 0.0004400426677367927516, 0.0008459942299586391311 ),
 .UNSPECIFIED. ) ;
#71343 = MECHANICAL_DESIGN_GEOMETRIC_PRESENTATION_REPRESENTATION (  '', ( #1050 ), #13810 ) ;
#71344 = UNCERTAINTY_MEASURE_WITH_UNIT (LENGTH_MEASURE( 1.000000000000000082E-05 ), #38409, 'distance_accuracy_value', 'NONE');
#71345 = CARTESIAN_POINT ( 'NONE',  ( 13.43411237798106583, 32.66530133659708213, -12.81628187352647252 ) ) ;
#71346 = CARTESIAN_POINT ( 'NONE',  ( 15.44008868035555260, 49.73035201082150536, 9.422509992056143702 ) ) ;
#71347 = CARTESIAN_POINT ( 'NONE',  ( 10.00000000000000000, 29.75893115100078745, -9.846743663894594434 ) ) ;
#71349 = CARTESIAN_POINT ( 'NONE',  ( 0.1532563361054083140, 16.00893115100078390, 1.131784320476157264E-15 ) ) ;
#71348 = CARTESIAN_POINT ( 'NONE',  ( 2.917880565312950480, 40.97041550158063217, -12.26659068614894821 ) ) ;
#71350 = DIRECTION ( 'NONE',  ( -0.000000000000000000, 1.000000000000000000, 0.000000000000000000 ) ) ;
#71351 = TOROIDAL_SURFACE ( 'NONE', #55415, 14.49999999999999822, 0.5000000000000000000 ) ;
#71352 = CARTESIAN_POINT ( 'NONE',  ( 7.361572987183169658, 49.96726448433410894, -9.846743663894592657 ) ) ;
#71354 = CARTESIAN_POINT ( 'NONE',  ( 6.204703633549690345, 5.762082168247301794, -14.16423886937410259 ) ) ;
#71353 = CARTESIAN_POINT ( 'NONE',  ( 17.20831665107776587, 49.13393115100078745, -7.208316651077762316 ) ) ;
#71355 = CARTESIAN_POINT ( 'NONE',  ( -4.164238869374099927, 37.01208216824731068, 3.795296366450308767 ) ) ;
#71356 = CARTESIAN_POINT ( 'NONE',  ( 12.63842701281683922, 24.55059781766745175, -9.846743663894590881 ) ) ;
#71357 = CARTESIAN_POINT ( 'NONE',  ( 7.084665262690076126, 47.02201867748818387, -10.88017736071110164 ) ) ;
#71358 = CARTESIAN_POINT ( 'NONE',  ( 7.084665262690076126, 22.02201867748817321, -10.88017736071110164 ) ) ;
#71359 = B_SPLINE_CURVE_WITH_KNOTS ( 'NONE', 3,
 ( #32466, #85977, #31959, #39000, #2500, #92475 ),
 .UNSPECIFIED., .F., .F.,
 ( 4, 2, 4 ),
 ( 3.409110551496104263E-05, 0.0004400426677367857585, 0.0008459942299586103998 ),
 .UNSPECIFIED. ) ;
#71360 = CARTESIAN_POINT ( 'NONE',  ( 12.91533473730992121, 49.52201867748817676, 10.88017736071110164 ) ) ;
#71361 = CARTESIAN_POINT ( 'NONE',  ( 17.96484262340118221, 31.18868534415483751, -7.964842623401177768 ) ) ;
#71362 = ORIENTED_EDGE ( 'NONE', *, *, #80532, .F. ) ;
#71363 = CARTESIAN_POINT ( 'NONE',  ( 22.81628187352647785, 31.62363466993042138, 6.195893100308588602E-16 ) ) ;
#71364 = EDGE_CURVE ( 'NONE', #11587, #98827, #79624, .T. ) ;
#71365 = CARTESIAN_POINT ( 'NONE',  ( 7.084665262690076126, 49.10535201082149825, 10.88017736071109987 ) ) ;
#71366 = EDGE_LOOP ( 'NONE', ( #23309, #73956, #73560, #67798, #84431, #11841 ) ) ;
#71367 = CARTESIAN_POINT ( 'NONE',  ( 0.000000000000000000, 0.5000000000000004441, 0.000000000000000000 ) ) ;
#71368 = CIRCLE ( 'NONE', #79345, 14.49999999999999822 ) ;
#71369 = CARTESIAN_POINT ( 'NONE',  ( 7.084665262690076126, 62.02201867748816966, -10.88017736071110164 ) ) ;
#71370 = ORIENTED_EDGE ( 'NONE', *, *, #37885, .F. ) ;
#71371 = AXIS2_PLACEMENT_3D ( 'NONE', #1138, #24127, #85608 ) ;
#71373 = EDGE_CURVE ( 'NONE', #37516, #76346, #19950, .T. ) ;
#71372 = CARTESIAN_POINT ( 'NONE',  ( -0.8801773607111008646, 68.27201867748817676, 2.915334737309923430 ) ) ;
#71374 = AXIS2_PLACEMENT_3D ( 'NONE', #41052, #26044, #71056 ) ;
#71375 = CARTESIAN_POINT ( 'NONE',  ( 18.72515096720572458, 40.05509018479936145, 6.499999999999964473 ) ) ;
#71376 = LINE ( 'NONE', #25866, #87162 ) ;
#71377 = CARTESIAN_POINT ( 'NONE',  ( 6.204703633549690345, 60.76208216824730357, -14.16423886937410259 ) ) ;
#71378 = CARTESIAN_POINT ( 'NONE',  ( 2.791683348922237240, 15.38393115100078212, -7.208316651077763204 ) ) ;
#71379 = CARTESIAN_POINT ( 'NONE',  ( 10.00000000000000178, 3.053748834913967425, 14.16423886937410082 ) ) ;
#71380 = EDGE_CURVE ( 'NONE', #18961, #88806, #59912, .T. ) ;
#71381 = CARTESIAN_POINT ( 'NONE',  ( 18.52753015748617571, 8.092264484334117824, 4.923371831947298993 ) ) ;
#71382 = CARTESIAN_POINT ( 'NONE',  ( 19.42250999205614548, 5.980352010821504471, -5.440088680355545492 ) ) ;
#71383 = CARTESIAN_POINT ( 'NONE',  ( 2.791683348922240793, 41.63393115100078745, 7.208316651077764092 ) ) ;
#71384 = ORIENTED_EDGE ( 'NONE', *, *, #74797, .T. ) ;
#71385 = CARTESIAN_POINT ( 'NONE',  ( 19.84674366389459621, 43.50893115100078745, 7.409399052514197653E-17 ) ) ;
#71386 = ORIENTED_EDGE ( 'NONE', *, *, #8376, .T. ) ;
#71387 = CARTESIAN_POINT ( 'NONE',  ( 7.084665262690076126, 52.02201867748816255, -10.88017736071110164 ) ) ;
#71388 = CARTESIAN_POINT ( 'NONE',  ( 1.472469842513823179, 56.42559781766745886, 4.923371831947296329 ) ) ;
#71389 = CARTESIAN_POINT ( 'NONE',  ( 15.44008868035555260, 64.73035201082151957, 9.422509992056143702 ) ) ;
#71390 = CARTESIAN_POINT ( 'NONE',  ( 0.5774900079438590739, 57.64701867748817676, -5.440088680355550821 ) ) ;
#71391 = CARTESIAN_POINT ( 'NONE',  ( -2.266590686148945544, 67.22041550158063217, 7.082119434687048631 ) ) ;
#71392 = CARTESIAN_POINT ( 'NONE',  ( 16.40814093676324603, 42.45696800326375353, -11.09922568453594671 ) ) ;
#71393 = FACE_OUTER_BOUND ( 'NONE', #25220, .T. ) ;
#71394 = ORIENTED_EDGE ( 'NONE', *, *, #89313, .F. ) ;
#71395 = CARTESIAN_POINT ( 'NONE',  ( 0.6178305044545838731, 34.74863466993042493, 9.382169495545420901 ) ) ;
#71396 = CARTESIAN_POINT ( 'NONE',  ( 0.5774900079438607392, 28.48035201082150891, 5.440088680355550821 ) ) ;
#71398 = ORIENTED_EDGE ( 'NONE', *, *, #16746, .T. ) ;
#71397 = EDGE_CURVE ( 'NONE', #15653, #83267, #21942, .T. ) ;
#71399 = CARTESIAN_POINT ( 'NONE',  ( -2.816281873526471635, -1.084698663402913210, -3.434112377981056508 ) ) ;
#71401 = CARTESIAN_POINT ( 'NONE',  ( 18.52753015748617571, 48.09226448433412315, 4.923371831947298993 ) ) ;
#71400 = CARTESIAN_POINT ( 'NONE',  ( 0.1532563361054083140, 11.00893115100078568, 1.131784320476157264E-15 ) ) ;
#71402 = CARTESIAN_POINT ( 'NONE',  ( -8.469568049931512022, -9.365055636449845622, 3.750000000000000000 ) ) ;
#71403 = CARTESIAN_POINT ( 'NONE',  ( 0.6178305044545818747, 63.49863466993043204, -9.382169495545419124 ) ) ;
#71404 = CARTESIAN_POINT ( 'NONE',  ( 18.52753015748617571, 43.09226448433412315, 4.923371831947298993 ) ) ;
#71405 = DIRECTION ( 'NONE',  ( -0.000000000000000000, -1.000000000000000000, -0.000000000000000000 ) ) ;
#71406 = DIRECTION ( 'NONE',  ( -0.9969173337331284079, 0.000000000000000000, 0.07845909572783861530 ) ) ;
#71408 = DIRECTION ( 'NONE',  ( 0.000000000000000000, 0.000000000000000000, -1.000000000000000000 ) ) ;
#71407 = CARTESIAN_POINT ( 'NONE',  ( 19.84674366389459266, 33.30059781766744464, 2.638427012816836559 ) ) ;
#71409 = SURFACE_STYLE_USAGE ( .BOTH. , #62397 ) ;
#71411 = ORIENTED_EDGE ( 'NONE', *, *, #47439, .T. ) ;
#71410 = CARTESIAN_POINT ( 'NONE',  ( 19.84674366389459621, 63.50893115100078745, 7.409399052514197653E-17 ) ) ;
#71412 = EDGE_CURVE ( 'NONE', #40991, #85047, #84892, .T. ) ;
#71413 = DIRECTION ( 'NONE',  ( 1.000000000000000000, 0.000000000000000000, 0.000000000000000000 ) ) ;
#71414 = CARTESIAN_POINT ( 'NONE',  ( 19.38216949554541557, 22.24863466993041428, -9.382169495545420901 ) ) ;
#71415 = CARTESIAN_POINT ( 'NONE',  ( 0.1532563361054100626, 40.80059781766745886, -2.638427012816831230 ) ) ;
#71416 = CARTESIAN_POINT ( 'NONE',  ( 0.000000000000000000, 10.49999999999999822, -6.000000000000000000 ) ) ;
#71417 = AXIS2_PLACEMENT_3D ( 'NONE', #68580, #111, #68088 ) ;
#71418 = CARTESIAN_POINT ( 'NONE',  ( 13.79529636645030344, 43.26208216824730357, 14.16423886937410614 ) ) ;
#71419 = CARTESIAN_POINT ( 'NONE',  ( 17.20831665107776587, 12.88393115100078390, 7.208316651077764980 ) ) ;
#71420 = CARTESIAN_POINT ( 'NONE',  ( 19.99999999999862510, 87.39268192868374285, 5.318367326097882319 ) ) ;
#71421 = CARTESIAN_POINT ( 'NONE',  ( 10.00000000000000000, 45.55374883491397497, -14.16423886937410082 ) ) ;
#71422 = CARTESIAN_POINT ( 'NONE',  ( 17.20831665107776587, 52.88393115100078035, 7.208316651077764980 ) ) ;
#71423 = CARTESIAN_POINT ( 'NONE',  ( 10.00000000000000000, 11.81368534415483751, -10.88017736071110342 ) ) ;
#71425 = AXIS2_PLACEMENT_3D ( 'NONE', #23080, #102, #59577 ) ;
#71424 = CARTESIAN_POINT ( 'NONE',  ( 17.08211943468705130, 28.47041550158063572, 12.26659068614894998 ) ) ;
#71426 = CARTESIAN_POINT ( 'NONE',  ( -0.3689425029237898834, 36.17874883491396787, -10.36894250292378850 ) ) ;
#71427 = FACE_OUTER_BOUND ( 'NONE', #94343, .T. ) ;
#71429 = CARTESIAN_POINT ( 'NONE',  ( 17.20831665107776587, 59.13393115100078745, -7.208316651077762316 ) ) ;
#71428 = CARTESIAN_POINT ( 'NONE',  ( 0.000000000000000000, 0.000000000000000000, 0.000000000000000000 ) ) ;
#71430 = MECHANICAL_DESIGN_GEOMETRIC_PRESENTATION_REPRESENTATION (  '', ( #2790 ), #84209 ) ;
#71431 = CARTESIAN_POINT ( 'NONE',  ( 15.44008868035555793, 41.39701867748817676, -9.422509992056140149 ) ) ;
#71432 = CARTESIAN_POINT ( 'NONE',  ( 3.897244926436219892, 4.401207273199346175E-16, -13.96644127841330807 ) ) ;
#71434 = DIRECTION ( 'NONE',  ( -0.000000000000000000, -1.000000000000000000, 0.000000000000000000 ) ) ;
#71433 = VECTOR ( 'NONE', #93398, 1000.000000000000000 ) ;
#71435 = CARTESIAN_POINT ( 'NONE',  ( -12.26659068614895354, 6.387082168247300018, -7.082119434687038861 ) ) ;
#71436 = AXIS2_PLACEMENT_3D ( 'NONE', #10845, #76508, #23529 ) ;
#71437 = CARTESIAN_POINT ( 'NONE',  ( 5.076628168052704559, 50.17559781766745886, -8.527530157486179263 ) ) ;
#71438 = CARTESIAN_POINT ( 'NONE',  ( 2.791683348922240793, 66.63393115100079456, 7.208316651077764092 ) ) ;
#71439 = EDGE_LOOP ( 'NONE', ( #10537, #31929, #16000, #313 ) ) ;
#71440 = CARTESIAN_POINT ( 'NONE',  ( 20.36894250292379738, 24.92874883491396787, -10.36894250292379027 ) ) ;
#71441 = LINE ( 'NONE', #85948, #69412 ) ;
#71443 = CARTESIAN_POINT ( 'NONE',  ( -6.091055032734201014, 15.00000000000000888, -13.29802223412764484 ) ) ;
#71442 = CARTESIAN_POINT ( 'NONE',  ( -5.068142462349377375, -24.94450071862243590, -2.750000000000000000 ) ) ;
#71444 = CARTESIAN_POINT ( 'NONE',  ( 4.559911319644449179, 7.230352010821505360, -9.422509992056141925 ) ) ;
#71445 = CARTESIAN_POINT ( 'NONE',  ( 21.09922568453594849, 31.20696800326375353, 6.408140936763242479 ) ) ;
#71446 = DIRECTION ( 'NONE',  ( -0.000000000000000000, -0.000000000000000000, 1.000000000000000000 ) ) ;
#71447 = CARTESIAN_POINT ( 'NONE',  ( 7.361572987183170547, 17.05059781766745530, 9.846743663894590881 ) ) ;
#71448 = CARTESIAN_POINT ( 'NONE',  ( -0.2418659066527782397, 10.11633188102327274, 6.114288769123032985 ) ) ;
#71449 = ADVANCED_FACE ( 'NONE', ( #39885 ), #46881, .T. ) ;
#71450 = CARTESIAN_POINT ( 'NONE',  ( 0.2751277870542914172, 43.21833443783938122, 6.499999999999992006 ) ) ;
#71451 = CARTESIAN_POINT ( 'NONE',  ( 20.88017736071110875, 15.77201867748817143, -2.915334737309920765 ) ) ;
#71452 = CARTESIAN_POINT ( 'NONE',  ( -0.1503990784575247319, 32.22266099184917465, -6.262539305110083276 ) ) ;
#71453 = CARTESIAN_POINT ( 'NONE',  ( 15.44008868035555793, 41.39701867748817676, -9.422509992056140149 ) ) ;
#71454 = CARTESIAN_POINT ( 'NONE',  ( 10.00000000000000000, 41.81368534415484106, -10.88017736071110342 ) ) ;
#71455 = CARTESIAN_POINT ( 'NONE',  ( 3.591859063236761518, 4.956968003263753531, 11.09922568453594849 ) ) ;
#71456 = DIRECTION ( 'NONE',  ( -0.2672383760782501838, 0.000000000000000000, -0.9636304532086248376 ) ) ;
#71457 = CARTESIAN_POINT ( 'NONE',  ( -42.50369195530268485, 107.9060299417078426, -4.500000000000000888 ) ) ;
#71458 = CARTESIAN_POINT ( 'NONE',  ( 14.92337183194729988, 14.34226448433411782, -8.527530157486177487 ) ) ;
#71459 = VERTEX_POINT ( 'NONE', #30396 ) ;
#71460 = PRODUCT_DEFINITION_SHAPE ( 'NONE', 'NONE',  #98993 ) ;
#71461 = EDGE_CURVE ( 'NONE', #67657, #95164, #89254, .T. ) ;
#71462 = CARTESIAN_POINT ( 'NONE',  ( 20.88017736071110519, 30.56368534415484106, 2.639326808657452039E-16 ) ) ;
#71463 = CARTESIAN_POINT ( 'NONE',  ( 21.09922568453595559, 37.04030133659708923, -6.408140936763230044 ) ) ;
#71464 = CARTESIAN_POINT ( 'NONE',  ( -0.1503990784575277295, 54.24884699246889852, -6.262539305110077947 ) ) ;
#71465 = UNCERTAINTY_MEASURE_WITH_UNIT (LENGTH_MEASURE( 1.000000000000000082E-05 ), #89494, 'distance_accuracy_value', 'NONE');
#71466 = CARTESIAN_POINT ( 'NONE',  ( 12.63842701281683034, 57.46726448433411605, 9.846743663894596210 ) ) ;
#71467 = CARTESIAN_POINT ( 'NONE',  ( -0.8801773607110991993, 67.85535201082151957, -2.915334737309923874 ) ) ;
#71468 = CARTESIAN_POINT ( 'NONE',  ( 7.361572987183170547, 7.050597817667451750, 9.846743663894590881 ) ) ;
#71469 = AXIS2_PLACEMENT_3D ( 'NONE', #23449, #69921, #54895 ) ;
#71470 = CARTESIAN_POINT ( 'NONE',  ( -2.816281873526473856, 34.33196800326376064, 3.434112377981055619 ) ) ;
#71472 = DIRECTION ( 'NONE',  ( -0.5547001962252291474, -0.8320502943378437211, -0.000000000000000000 ) ) ;
#71471 = CARTESIAN_POINT ( 'NONE',  ( 19.42250999205614548, 55.98035201082150536, -5.440088680355545492 ) ) ;
#71473 = VERTEX_POINT ( 'NONE', #92384 ) ;
#71474 = CARTESIAN_POINT ( 'NONE',  ( 64.56412365047461321, 28.99999999999999645, 10.00000000000000000 ) ) ;
#71475 = CARTESIAN_POINT ( 'NONE',  ( 0.6178305044545838731, 59.74863466993041783, 9.382169495545420901 ) ) ;
#71476 = CARTESIAN_POINT ( 'NONE',  ( 1.472469842513823179, 15.59226448433411960, -4.923371831947296329 ) ) ;
#71477 = CARTESIAN_POINT ( 'NONE',  ( 4.559911319644449179, 8.897018677488171434, 9.422509992056141925 ) ) ;
#71478 = CARTESIAN_POINT ( 'NONE',  ( 17.20831665107776587, 24.13393115100078035, -7.208316651077762316 ) ) ;
#71479 = CARTESIAN_POINT ( 'NONE',  ( -2.266590686148945544, 62.22041550158063927, 7.082119434687048631 ) ) ;
#71480 = EDGE_LOOP ( 'NONE', ( #45671, #88761, #57000, #58762, #52940, #46135 ) ) ;
#71481 = CARTESIAN_POINT ( 'NONE',  ( 17.96484262340118221, 16.18868534415483396, -7.964842623401177768 ) ) ;
#71482 = STYLED_ITEM ( 'NONE', ( #91588 ), #44265 ) ;
#71483 = CARTESIAN_POINT ( 'NONE',  ( 10.00000000000000178, 19.31368534415484106, 10.88017736071110342 ) ) ;
#71484 = CARTESIAN_POINT ( 'NONE',  ( 1.959929470562091547, 16.50257860105346097, 5.767676674365524114 ) ) ;
#71485 = VECTOR ( 'NONE', #81151, 1000.000000000000000 ) ;
#71486 = ORIENTED_EDGE ( 'NONE', *, *, #49678, .T. ) ;
#71487 = ORIENTED_EDGE ( 'NONE', *, *, #18758, .F. ) ;
#71488 = CARTESIAN_POINT ( 'NONE',  ( 20.32896413005680714, 27.60497603579417714, -5.963430220938276349 ) ) ;
#71490 = EDGE_CURVE ( 'NONE', #21109, #81310, #72662, .T. ) ;
#71489 = CARTESIAN_POINT ( 'NONE',  ( 19.42250999205614193, 25.14701867748817321, 5.440088680355555262 ) ) ;
#71491 = CARTESIAN_POINT ( 'NONE',  ( 19.84674366389459266, 58.30059781766745886, 2.638427012816836559 ) ) ;
#71492 = CARTESIAN_POINT ( 'NONE',  ( 1.274849032794280523, 68.57228050351031357, 6.499999999999960032 ) ) ;
#71493 = CARTESIAN_POINT ( 'NONE',  ( 20.36894250292379738, 24.92874883491396787, -10.36894250292379027 ) ) ;
#71494 = CARTESIAN_POINT ( 'NONE',  ( 19.42250999205614193, 35.14701867748816966, 5.440088680355555262 ) ) ;
#71495 = B_SPLINE_CURVE_WITH_KNOTS ( 'NONE', 3,
 ( #5049, #21036, #5548, #89527, #35532, #81520 ),
 .UNSPECIFIED., .F., .F.,
 ( 4, 2, 4 ),
 ( 0.0002800715030460590818, 0.0006862774322447821786, 0.001092483361443505330 ),
 .UNSPECIFIED. ) ;
#71496 = CARTESIAN_POINT ( 'NONE',  ( 15.44008868035555260, 14.73035201082150536, 9.422509992056143702 ) ) ;
#71497 = CARTESIAN_POINT ( 'NONE',  ( 0.1532563361054082862, 56.21726448433411605, 2.638427012816831674 ) ) ;
#71498 = EDGE_CURVE ( 'NONE', #36998, #22141, #98927, .T. ) ;
#71499 = CARTESIAN_POINT ( 'NONE',  ( -11.51437862373891363, -65.40122319151942065, -3.750000000000001332 ) ) ;
#71500 = CARTESIAN_POINT ( 'NONE',  ( 12.63842701281683922, 39.55059781766744464, -9.846743663894590881 ) ) ;
#71501 = CARTESIAN_POINT ( 'NONE',  ( 14.49440716394873618, 15.00000000000000000, -0.4026921475166200803 ) ) ;
#71502 = CARTESIAN_POINT ( 'NONE',  ( 2.791683348922240793, 11.63393115100078568, 7.208316651077764092 ) ) ;
#71503 = CARTESIAN_POINT ( 'NONE',  ( -9.382169495545413795, -25.25136533006957862, 9.382169495545428006 ) ) ;
#71504 = AXIS2_PLACEMENT_3D ( 'NONE', #33701, #64201, #94717 ) ;
#71505 = ORIENTED_EDGE ( 'NONE', *, *, #79727, .F. ) ;
#71506 = CARTESIAN_POINT ( 'NONE',  ( 15.44008868035555260, 19.73035201082150536, 9.422509992056143702 ) ) ;
#71507 = CARTESIAN_POINT ( 'NONE',  ( 2.791683348922237240, 15.38393115100078212, -7.208316651077763204 ) ) ;
#71508 = CARTESIAN_POINT ( 'NONE',  ( 16.40814093676323893, 0.7903013365970867898, 11.09922568453595026 ) ) ;
#71509 = CARTESIAN_POINT ( 'NONE',  ( 20.88017736071110519, 50.56368534415484106, 2.639326808657452039E-16 ) ) ;
#71511 = CARTESIAN_POINT ( 'NONE',  ( 13.43411237798106583, 42.66530133659707502, -12.81628187352647252 ) ) ;
#71510 = CARTESIAN_POINT ( 'NONE',  ( 7.084665262690076126, 17.02201867748817676, -10.88017736071110164 ) ) ;
#71512 = CARTESIAN_POINT ( 'NONE',  ( 2.917880565312950480, 30.97041550158063572, -12.26659068614894821 ) ) ;
#71513 = STYLED_ITEM ( 'NONE', ( #28001 ), #58355 ) ;
#71514 = CARTESIAN_POINT ( 'NONE',  ( 20.15039907845753575, 12.62777174578613071, -6.262539305110077059 ) ) ;
#71515 = CIRCLE ( 'NONE', #23627, 0.5000000000000000000 ) ;
#71516 = ADVANCED_FACE ( 'NONE', ( #16401 ), #68651, .T. ) ;
#71517 = EDGE_CURVE ( 'NONE', #91342, #12526, #65251, .T. ) ;
#71518 = CARTESIAN_POINT ( 'NONE',  ( 22.81628187352648496, 56.83196800326374643, -3.434112377981050290 ) ) ;
#71519 = ORIENTED_EDGE ( 'NONE', *, *, #18082, .F. ) ;
#71520 = CARTESIAN_POINT ( 'NONE',  ( 1.472469842513823179, 61.42559781766745175, 4.923371831947296329 ) ) ;
#71521 = CARTESIAN_POINT ( 'NONE',  ( 12.91533473730992121, 39.52201867748817676, 10.88017736071110164 ) ) ;
#71523 = ORIENTED_EDGE ( 'NONE', *, *, #66402, .F. ) ;
#71522 = EDGE_CURVE ( 'NONE', #42904, #40747, #40278, .T. ) ;
#71524 = CARTESIAN_POINT ( 'NONE',  ( 5.076628168052703671, 1.842264484334118047, 8.527530157486179263 ) ) ;
#71525 = CARTESIAN_POINT ( 'NONE',  ( 0.9408516040111367662, 42.46693863883976405, -6.499999999999915623 ) ) ;
#71526 = CARTESIAN_POINT ( 'NONE',  ( 19.84674366389459621, 23.50893115100078390, 7.409399052514197653E-17 ) ) ;
#71527 = CARTESIAN_POINT ( 'NONE',  ( 0.5774900079438590739, 67.64701867748817676, -5.440088680355550821 ) ) ;
#71528 = CARTESIAN_POINT ( 'NONE',  ( 5.076628168052703671, 1.842264484334118047, 8.527530157486179263 ) ) ;
#71530 = DIRECTION ( 'NONE',  ( 0.000000000000000000, 1.000000000000000000, 0.000000000000000000 ) ) ;
#71529 = CARTESIAN_POINT ( 'NONE',  ( 19.42250999205614193, 60.14701867748817676, 5.440088680355555262 ) ) ;
#71531 = CARTESIAN_POINT ( 'NONE',  ( 15.44008868035555793, 61.39701867748817676, -9.422509992056140149 ) ) ;
#71533 = ORIENTED_EDGE ( 'NONE', *, *, #79500, .T. ) ;
#71532 = CARTESIAN_POINT ( 'NONE',  ( 2.791683348922240793, 11.63393115100078568, 7.208316651077764092 ) ) ;
#71534 = FACE_OUTER_BOUND ( 'NONE', #78419, .T. ) ;
#71535 = CARTESIAN_POINT ( 'NONE',  ( 2.791683348922240793, 51.63393115100078745, 7.208316651077764092 ) ) ;
#71536 = ORIENTED_EDGE ( 'NONE', *, *, #60295, .T. ) ;
#71537 = EDGE_LOOP ( 'NONE', ( #10013, #56604, #88791 ) ) ;
#71538 = CARTESIAN_POINT ( 'NONE',  ( -4.922013193295457611, 0.000000000000000000, 2.347679864819414153 ) ) ;
#71539 = CARTESIAN_POINT ( 'NONE',  ( 17.08211943468705130, 8.470415501580635720, 12.26659068614894998 ) ) ;
#71540 = CARTESIAN_POINT ( 'NONE',  ( 22.81628187352647785, 61.62363466993041783, 6.195893100308588602E-16 ) ) ;
#71541 = CARTESIAN_POINT ( 'NONE',  ( 2.917880565312948704, 7.637082168247301794, 12.26659068614894643 ) ) ;
#71542 = CARTESIAN_POINT ( 'NONE',  ( -4.164238869374099927, 37.01208216824731068, 3.795296366450308767 ) ) ;
#71543 = CARTESIAN_POINT ( 'NONE',  ( -14.97687855664608847, 0.5000000000000004441, 0.8325315005899532883 ) ) ;
#71544 = CARTESIAN_POINT ( 'NONE',  ( 17.96484262340118221, 26.18868534415483396, -7.964842623401177768 ) ) ;
#71545 = ORIENTED_EDGE ( 'NONE', *, *, #84364, .T. ) ;
#71546 = CARTESIAN_POINT ( 'NONE',  ( 1.472469842513823179, 11.42559781766745175, 4.923371831947296329 ) ) ;
#71548 = CARTESIAN_POINT ( 'NONE',  ( 12.63842701281683922, 19.55059781766745175, -9.846743663894590881 ) ) ;
#71547 = CARTESIAN_POINT ( 'NONE',  ( 19.42250999205614548, 55.98035201082150536, -5.440088680355545492 ) ) ;
#71549 = CARTESIAN_POINT ( 'NONE',  ( 6.565887622018943937, 50.16530133659708213, 12.81628187352647430 ) ) ;
#71550 = CARTESIAN_POINT ( 'NONE',  ( 19.84674366389459621, 38.50893115100078745, 7.409399052514197653E-17 ) ) ;
#71551 = CARTESIAN_POINT ( 'NONE',  ( 18.04007052943772038, 59.00257860105349295, -5.767676674365850076 ) ) ;
#71552 = CARTESIAN_POINT ( 'NONE',  ( 2.035157376598824452, 58.68868534415482685, 7.964842623401179544 ) ) ;
#71553 = CARTESIAN_POINT ( 'NONE',  ( 10.00000000000000178, 35.37363466993042493, 12.81628187352647608 ) ) ;
#71554 = CARTESIAN_POINT ( 'NONE',  ( 3.469446951953614189E-15, -26.94625116508602858, 14.16423886937410259 ) ) ;
#71555 = CARTESIAN_POINT ( 'NONE',  ( 1.472469842513823179, 21.42559781766745175, 4.923371831947296329 ) ) ;
#71556 = CARTESIAN_POINT ( 'NONE',  ( -0.3689425029237881626, 7.428748834913967869, 10.36894250292379027 ) ) ;
#71557 = VERTEX_POINT ( 'NONE', #24793 ) ;
#71558 = CARTESIAN_POINT ( 'NONE',  ( 20.88017736071110164, 35.35535201082150536, 2.915334737309930979 ) ) ;
#71559 = CARTESIAN_POINT ( 'NONE',  ( 10.00000000000000000, 35.55374883491396787, -14.16423886937410082 ) ) ;
#71560 = CARTESIAN_POINT ( 'NONE',  ( 1.472469842513823179, 50.59226448433411605, -4.923371831947296329 ) ) ;
#71561 = CARTESIAN_POINT ( 'NONE',  ( 5.076628168052703671, 11.84226448433411960, 8.527530157486179263 ) ) ;
#71562 = CARTESIAN_POINT ( 'NONE',  ( 19.38216949554541557, 52.24863466993041072, -9.382169495545420901 ) ) ;
#71563 = CARTESIAN_POINT ( 'NONE',  ( 0.5774900079438590739, 42.64701867748816966, -5.440088680355550821 ) ) ;
#71564 = AXIS2_PLACEMENT_3D ( 'NONE', #78157, #95112, #2683 ) ;
#71565 = CARTESIAN_POINT ( 'NONE',  ( 6.565887622018943937, 18.08196800326375708, -12.81628187352647608 ) ) ;
#71566 = CARTESIAN_POINT ( 'NONE',  ( 2.791683348922240793, 41.63393115100078745, 7.208316651077764092 ) ) ;
#71567 = CARTESIAN_POINT ( 'NONE',  ( -10.88017736071110342, 8.063685344154844614, 3.903127820947815962E-15 ) ) ;
#71568 = FILL_AREA_STYLE ('',( #41073 ) ) ;
#71570 = CARTESIAN_POINT ( 'NONE',  ( -2.253458813454140675, 12.77999999999999936, -9.500000000000000000 ) ) ;
#71569 = CARTESIAN_POINT ( 'NONE',  ( 20.88017736071110519, 60.56368534415484106, 2.639326808657452039E-16 ) ) ;
#71571 = ADVANCED_FACE ( 'NONE', ( #47768 ), #46782, .T. ) ;
#71572 = PRESENTATION_LAYER_ASSIGNMENT (  '', '', ( #15696 ) ) ;
#71573 = CARTESIAN_POINT ( 'NONE',  ( -10.95094547650107053, -94.44763431416065202, 3.999999999999999112 ) ) ;
#71574 = DIRECTION ( 'NONE',  ( 0.000000000000000000, -1.000000000000000000, 0.000000000000000000 ) ) ;
#71575 = AXIS2_PLACEMENT_3D ( 'NONE', #36564, #22555, #30026 ) ;
#71576 = CARTESIAN_POINT ( 'NONE',  ( 7.084665262690076126, 57.02201867748817676, -10.88017736071110164 ) ) ;
#71577 = CARTESIAN_POINT ( 'NONE',  ( -0.8801773607110991993, 62.85535201082150536, -2.915334737309923874 ) ) ;
#71578 = CARTESIAN_POINT ( 'NONE',  ( 1.377727649040772586E-15, 15.00000000000000000, 11.25000000000000178 ) ) ;
#71579 = CARTESIAN_POINT ( 'NONE',  ( -7.750000000000000000, 80.32179676972448590, -3.750000000000000000 ) ) ;
#71580 = CARTESIAN_POINT ( 'NONE',  ( 12.63842701281683034, 22.46726448433411605, 9.846743663894596210 ) ) ;
#71581 = CARTESIAN_POINT ( 'NONE',  ( 15.44008868035555260, 19.73035201082150536, 9.422509992056143702 ) ) ;
#71582 = CARTESIAN_POINT ( 'NONE',  ( 5.076628168052704559, 65.17559781766745175, -8.527530157486179263 ) ) ;
#71584 = CARTESIAN_POINT ( 'NONE',  ( 38.04706783004212411, 29.00000000000000355, -7.000000000000000000 ) ) ;
#71583 = CARTESIAN_POINT ( 'NONE',  ( 15.44008868035555793, 26.39701867748817321, -9.422509992056140149 ) ) ;
#71585 = DIRECTION ( 'NONE',  ( 0.000000000000000000, 0.000000000000000000, 1.000000000000000000 ) ) ;
#71586 = CARTESIAN_POINT ( 'NONE',  ( 21.09922568453595559, 22.04030133659708923, -6.408140936763230044 ) ) ;
#71587 = EDGE_LOOP ( 'NONE', ( #15313, #96845, #79015, #81978 ) ) ;
#71588 = CARTESIAN_POINT ( 'NONE',  ( 4.559911319644449179, 48.89701867748817676, 9.422509992056141925 ) ) ;
#71589 = CARTESIAN_POINT ( 'NONE',  ( 19.84674366389459266, 33.30059781766744464, 2.638427012816836559 ) ) ;
#71591 = CARTESIAN_POINT ( 'NONE',  ( 17.39651004071842522, 19.08210964143329491, -6.499999999999992895 ) ) ;
#71590 = CARTESIAN_POINT ( 'NONE',  ( 10.00000000000000178, 25.37363466993041783, 12.81628187352647608 ) ) ;
#71592 = CARTESIAN_POINT ( 'NONE',  ( 15.44008868035555260, 29.73035201082150891, 9.422509992056143702 ) ) ;
#71593 = CARTESIAN_POINT ( 'NONE',  ( 7.084665262690076126, 37.02201867748817676, -10.88017736071110164 ) ) ;
#71594 = CARTESIAN_POINT ( 'NONE',  ( -0.3689425029237898834, 56.17874883491396076, -10.36894250292378850 ) ) ;
#71595 = CARTESIAN_POINT ( 'NONE',  ( 12.63842701281683922, 44.55059781766745175, -9.846743663894590881 ) ) ;
#71596 = CARTESIAN_POINT ( 'NONE',  ( 19.84674366389459621, 8.508931151000785675, 7.409399052514197653E-17 ) ) ;
#71597 = CARTESIAN_POINT ( 'NONE',  ( 12.91533473730992121, 44.52201867748816966, 10.88017736071110164 ) ) ;
#71598 = SURFACE_STYLE_USAGE ( .BOTH. , #17611 ) ;
#71599 = CARTESIAN_POINT ( 'NONE',  ( 2.917880565312950480, 15.97041550158063217, -12.26659068614894821 ) ) ;
#71600 = SURFACE_SIDE_STYLE ('',( #94575 ) ) ;
#71601 = VERTEX_POINT ( 'NONE', #47269 ) ;
#71602 = CARTESIAN_POINT ( 'NONE',  ( 10.00000000000000178, 48.05374883491396787, 14.16423886937410082 ) ) ;
#71604 = ADVANCED_FACE ( 'NONE', ( #40772 ), #6194, .F. ) ;
#71603 = CARTESIAN_POINT ( 'NONE',  ( 24.16423886937410614, 54.30374883491396787, 8.672049930838204340E-16 ) ) ;
#71605 = CARTESIAN_POINT ( 'NONE',  ( 7.361572987183170547, 22.05059781766745530, 9.846743663894590881 ) ) ;
#71606 = CARTESIAN_POINT ( 'NONE',  ( -13.77612262535527954, 90.93158326518027934, 7.883772450803742338 ) ) ;
#71607 = CARTESIAN_POINT ( 'NONE',  ( 0.2751277870542914172, 58.21833443783938833, 6.499999999999992006 ) ) ;
#71609 = CARTESIAN_POINT ( 'NONE',  ( 0.6178305044545838731, 34.74863466993042493, 9.382169495545420901 ) ) ;
#71608 = CARTESIAN_POINT ( 'NONE',  ( 2.035157376598824452, 68.68868534415484817, 7.964842623401179544 ) ) ;
#71610 = CARTESIAN_POINT ( 'NONE',  ( -4.164238869374098151, 46.59541550158063927, -3.795296366450310543 ) ) ;
#71611 = ADVANCED_FACE ( 'NONE', ( #23814 ), #31725, .T. ) ;
#71612 = CARTESIAN_POINT ( 'NONE',  ( 10.00000000000000178, 69.31368534415484817, 10.88017736071110342 ) ) ;
#71613 = CARTESIAN_POINT ( 'NONE',  ( 7.208316651077762316, 9.133931151000789228, -7.208316651077764980 ) ) ;
#71614 = ORIENTED_EDGE ( 'NONE', *, *, #29040, .F. ) ;
#71615 = CARTESIAN_POINT ( 'NONE',  ( 19.84674366389459266, 23.30059781766745530, 2.638427012816836559 ) ) ;
#71616 = DIRECTION ( 'NONE',  ( 0.000000000000000000, 0.000000000000000000, -1.000000000000000000 ) ) ;
#71617 = VERTEX_POINT ( 'NONE', #25774 ) ;
#71619 = CARTESIAN_POINT ( 'NONE',  ( 17.96484262340118221, 14.93868534415484106, 7.964842623401181321 ) ) ;
#71618 = CARTESIAN_POINT ( 'NONE',  ( 4.559911319644449179, 12.23035201082150714, -9.422509992056141925 ) ) ;
#71621 = CARTESIAN_POINT ( 'NONE',  ( 16.40814093676323893, 0.7903013365970867898, 11.09922568453595026 ) ) ;
#71620 = CARTESIAN_POINT ( 'NONE',  ( 12.63842701281683922, 44.55059781766745175, -9.846743663894590881 ) ) ;
#71622 = FILL_AREA_STYLE ('',( #73072 ) ) ;
#71623 = CARTESIAN_POINT ( 'NONE',  ( 14.97687855664614176, 14.49999999999999112, 0.8325315005901842147 ) ) ;
#71624 = COLOUR_RGB ( '', 0.40784314, 0.44705882, 0.49803922) ;
#71625 = CARTESIAN_POINT ( 'NONE',  ( 10.00000000000000000, 22.87363466993042138, -12.81628187352647608 ) ) ;
#71626 = ORIENTED_EDGE ( 'NONE', *, *, #15726, .F. ) ;
#71627 = CARTESIAN_POINT ( 'NONE',  ( 17.08211943468705840, 55.13708216824731068, -12.26659068614894466 ) ) ;
#71628 = CARTESIAN_POINT ( 'NONE',  ( 17.08211943468705130, 58.47041550158063927, 12.26659068614894998 ) ) ;
#71629 = VERTEX_POINT ( 'NONE', #84792 ) ;
#71630 = CARTESIAN_POINT ( 'NONE',  ( 15.44008868035555793, 36.39701867748816966, -9.422509992056140149 ) ) ;
#71631 = CARTESIAN_POINT ( 'NONE',  ( 19.42250999205614548, 40.98035201082150536, -5.440088680355545492 ) ) ;
#71632 = CARTESIAN_POINT ( 'NONE',  ( 4.559911319644449179, 67.23035201082150536, -9.422509992056141925 ) ) ;
#71633 = CARTESIAN_POINT ( 'NONE',  ( 7.084665262690076126, 22.02201867748817321, -10.88017736071110164 ) ) ;
#71634 = EDGE_CURVE ( 'NONE', #49831, #43714, #60498, .T. ) ;
#71635 = STYLED_ITEM ( 'NONE', ( #12811 ), #59675 ) ;
#71636 = B_SPLINE_CURVE_WITH_KNOTS ( 'NONE', 3,
 ( #57722, #73710, #87731, #80234, #34223, #28216 ),
 .UNSPECIFIED., .F., .F.,
 ( 4, 2, 4 ),
 ( 3.409110551496141533E-05, 0.0004400426677367868427, 0.0008459942299586122429 ),
 .UNSPECIFIED. ) ;
#71637 = CARTESIAN_POINT ( 'NONE',  ( 0.9940297508536876103, -0.03417435944610275333, 14.21528771620250353 ) ) ;
#71638 = CARTESIAN_POINT ( 'NONE',  ( 19.84674366389459266, 8.717264484334116048, -2.638427012816827677 ) ) ;
#71639 = DIRECTION ( 'NONE',  ( 0.000000000000000000, 1.000000000000000000, 0.000000000000000000 ) ) ;
#71640 = ORIENTED_EDGE ( 'NONE', *, *, #85395, .F. ) ;
#71641 = CARTESIAN_POINT ( 'NONE',  ( 10.83696084481538868, -98.17058944465519232, 4.000000000000000000 ) ) ;
#71642 = CARTESIAN_POINT ( 'NONE',  ( 0.1532563361054083140, 41.00893115100078745, 1.131784320476157264E-15 ) ) ;
#71643 = CARTESIAN_POINT ( 'NONE',  ( 17.39651004071841456, 9.082109641433294911, -6.500000000000003553 ) ) ;
#71644 = CARTESIAN_POINT ( 'NONE',  ( 6.565887622018943937, 48.08196800326375353, -12.81628187352647608 ) ) ;
#71645 = CARTESIAN_POINT ( 'NONE',  ( -6.841090228438033272, -58.65898919720570603, 3.750000000000000444 ) ) ;
#71646 = ORIENTED_EDGE ( 'NONE', *, *, #55011, .F. ) ;
#71647 = DIRECTION ( 'NONE',  ( -0.000000000000000000, -0.000000000000000000, -1.000000000000000000 ) ) ;
#71648 = CARTESIAN_POINT ( 'NONE',  ( -45.64141537884788846, 104.8111512546448125, 5.509330541965931971 ) ) ;
#71649 = CARTESIAN_POINT ( 'NONE',  ( 1.274849032794280523, 48.57228050351032067, 6.499999999999960032 ) ) ;
#71650 = CARTESIAN_POINT ( 'NONE',  ( -4.164238869374098151, 51.59541550158063217, -3.795296366450310543 ) ) ;
#71651 = CARTESIAN_POINT ( 'NONE',  ( 12.22474924877137070, 14.76984934309701991, 8.589397507024928657 ) ) ;
#71652 = EDGE_LOOP ( 'NONE', ( #68080, #54633, #53152, #71326 ) ) ;
#71653 = CARTESIAN_POINT ( 'NONE',  ( 14.47650479471822926, 14.63606881343832100, 3.928206833722133862 ) ) ;
#71654 = CARTESIAN_POINT ( 'NONE',  ( 12.63842701281683922, 29.55059781766745175, -9.846743663894590881 ) ) ;
#71655 = CARTESIAN_POINT ( 'NONE',  ( 3.591859063236761518, 9.956968003263753531, 11.09922568453594849 ) ) ;
#71656 = CARTESIAN_POINT ( 'NONE',  ( 7.084665262690076126, 62.02201867748816966, -10.88017736071110164 ) ) ;
#71657 = FACE_OUTER_BOUND ( 'NONE', #90684, .T. ) ;
#71658 = CARTESIAN_POINT ( 'NONE',  ( 19.84674366389459266, 58.30059781766745886, 2.638427012816836559 ) ) ;
#71659 = DIRECTION ( 'NONE',  ( -0.000000000000000000, -0.000000000000000000, -1.000000000000000000 ) ) ;
#71660 = ORIENTED_EDGE ( 'NONE', *, *, #35122, .T. ) ;
#71661 = CARTESIAN_POINT ( 'NONE',  ( 6.204703633549690345, 67.84541550158060375, 14.16423886937410082 ) ) ;
#71662 = PRESENTATION_STYLE_ASSIGNMENT (( #70686 ) ) ;
#71663 = CARTESIAN_POINT ( 'NONE',  ( 10.00000000000000000, 41.81368534415484106, -10.88017736071110342 ) ) ;
#71665 = CARTESIAN_POINT ( 'NONE',  ( 7.792922786566074400, 12.98375417942040322, -8.778698621334729779 ) ) ;
#71664 = CARTESIAN_POINT ( 'NONE',  ( 16.40814093676323893, 10.79030133659708923, 11.09922568453595026 ) ) ;
#71666 = CARTESIAN_POINT ( 'NONE',  ( -7.551349515323020789, 0.000000000000000000, -12.08468537022916323 ) ) ;
#71667 = FACE_OUTER_BOUND ( 'NONE', #50697, .T. ) ;
#71668 = DIRECTION ( 'NONE',  ( 0.000000000000000000, 0.000000000000000000, 1.000000000000000000 ) ) ;
#71669 = CARTESIAN_POINT ( 'NONE',  ( 2.791683348922237240, 50.38393115100078035, -7.208316651077763204 ) ) ;
#71670 = CARTESIAN_POINT ( 'NONE',  ( 18.52753015748618282, 3.925597817667451306, -4.923371831947291888 ) ) ;
#71671 = CARTESIAN_POINT ( 'NONE',  ( -9.422509992056145478, -32.35298132251182324, -5.440088680355541939 ) ) ;
#71672 = CARTESIAN_POINT ( 'NONE',  ( -1.099225684535947600, 4.540301336597087456, 6.408140936763237150 ) ) ;
#71673 = CARTESIAN_POINT ( 'NONE',  ( -11.26386101273796925, -65.37750071430100718, -4.000000000000000000 ) ) ;
#71675 = LINE ( 'NONE', #3185, #3293 ) ;
#71674 = CARTESIAN_POINT ( 'NONE',  ( 0.5774900079438590739, 27.64701867748817676, -5.440088680355550821 ) ) ;
#71676 = CARTESIAN_POINT ( 'NONE',  ( 13.79529636645030344, 33.26208216824730357, 14.16423886937410614 ) ) ;
#71677 = EDGE_CURVE ( 'NONE', #68087, #62473, #55726, .T. ) ;
#71678 = CARTESIAN_POINT ( 'NONE',  ( 20.36894250292379738, 24.92874883491396787, -10.36894250292379027 ) ) ;
#71679 = CARTESIAN_POINT ( 'NONE',  ( 12.91533473730993009, 11.60535201082150714, -10.88017736071109987 ) ) ;
#71680 = CARTESIAN_POINT ( 'NONE',  ( 5.076628168052703671, 46.84226448433412315, 8.527530157486179263 ) ) ;
#71681 = CARTESIAN_POINT ( 'NONE',  ( 22.81628187352648496, 36.83196800326376064, -3.434112377981050290 ) ) ;
#71682 = CARTESIAN_POINT ( 'NONE',  ( 7.084665262690076126, 9.105352010821503583, 10.88017736071109987 ) ) ;
#71683 = ORIENTED_EDGE ( 'NONE', *, *, #16385, .T. ) ;
#71684 = CARTESIAN_POINT ( 'NONE',  ( 0.1532563361054082862, 36.21726448433410894, 2.638427012816831674 ) ) ;
#71685 = CARTESIAN_POINT ( 'NONE',  ( 2.035157376598822676, 42.43868534415483396, -7.964842623401177768 ) ) ;
#71686 = CARTESIAN_POINT ( 'NONE',  ( 6.565887622018943937, 3.081968003263753531, -12.81628187352647608 ) ) ;
#71688 = FACE_OUTER_BOUND ( 'NONE', #89835, .T. ) ;
#71687 = CARTESIAN_POINT ( 'NONE',  ( 22.26659068614895176, 19.72041550158063572, -7.082119434687042414 ) ) ;
#71689 = PLANE ( 'NONE',  #75948 ) ;
#71690 = CARTESIAN_POINT ( 'NONE',  ( 1.472469842513823179, 21.42559781766745175, 4.923371831947296329 ) ) ;
#71691 = CARTESIAN_POINT ( 'NONE',  ( 16.40814093676324603, 57.45696800326375353, -11.09922568453594671 ) ) ;
#71692 = CARTESIAN_POINT ( 'NONE',  ( 18.52753015748618282, 58.92559781766745886, -4.923371831947291888 ) ) ;
#71693 = ORIENTED_EDGE ( 'NONE', *, *, #28330, .T. ) ;
#71694 = CARTESIAN_POINT ( 'NONE',  ( 0.2751277870542911952, 34.36607318730131055, -6.499999999999992006 ) ) ;
#71695 = CARTESIAN_POINT ( 'NONE',  ( 24.16423886937410614, 64.51208216824728936, -3.795296366450302550 ) ) ;
#71696 = CARTESIAN_POINT ( 'NONE',  ( 20.36894250292379382, 8.678748834913967869, 10.36894250292379205 ) ) ;
#71697 = CARTESIAN_POINT ( 'NONE',  ( 1.472469842513823179, 0.5922644843341181575, -4.923371831947296329 ) ) ;
#71698 = CARTESIAN_POINT ( 'NONE',  ( 18.52753015748617571, 48.09226448433412315, 4.923371831947298993 ) ) ;
#71699 = CARTESIAN_POINT ( 'NONE',  ( 15.44008868035555793, 26.39701867748817321, -9.422509992056140149 ) ) ;
#71700 = DIRECTION ( 'NONE',  ( -0.9762960071199346945, 0.000000000000000000, 0.2164396139380971029 ) ) ;
#71701 = CARTESIAN_POINT ( 'NONE',  ( 10.00000000000000000, 64.75893115100078035, -9.846743663894594434 ) ) ;
#71702 = COLOUR_RGB ( '', 0.40784314, 0.44705882, 0.49803922) ;
#71703 = VERTEX_POINT ( 'NONE', #81218 ) ;
#71704 = CIRCLE ( 'NONE', #98511, 10.90000000000000036 ) ;
#71705 = DIRECTION ( 'NONE',  ( -0.6087614290087242086, 0.000000000000000000, 0.7933533402912323895 ) ) ;
#71706 = ORIENTED_EDGE ( 'NONE', *, *, #25227, .F. ) ;
#71707 = ORIENTED_EDGE ( 'NONE', *, *, #12686, .T. ) ;
#71708 = CARTESIAN_POINT ( 'NONE',  ( 5.624999999999998224, 11.25513551118487676, -9.742785792574936821 ) ) ;
#71709 = CARTESIAN_POINT ( 'NONE',  ( 13.79529636645031943, 5.345415501580634832, -14.16423886937409904 ) ) ;
#71711 = EDGE_CURVE ( 'NONE', #69641, #26110, #18763, .T. ) ;
#71710 = SURFACE_SIDE_STYLE ('',( #62226 ) ) ;
#71712 = CARTESIAN_POINT ( 'NONE',  ( 5.076628168052703671, 51.84226448433412315, 8.527530157486179263 ) ) ;
#71713 = CARTESIAN_POINT ( 'NONE',  ( 1.472469842513823179, 36.42559781766745175, 4.923371831947296329 ) ) ;
#71715 = CARTESIAN_POINT ( 'NONE',  ( 2.791683348922240793, 61.63393115100079456, 7.208316651077764092 ) ) ;
#71714 = CARTESIAN_POINT ( 'NONE',  ( 20.88017736071110164, 30.35535201082151247, 2.915334737309930979 ) ) ;
#71716 = CARTESIAN_POINT ( 'NONE',  ( 13.79529636645031943, 5.345415501580634832, -14.16423886937409904 ) ) ;
#71717 = CARTESIAN_POINT ( 'NONE',  ( 13.79529636645030344, 43.26208216824730357, 14.16423886937410614 ) ) ;
#71718 = CARTESIAN_POINT ( 'NONE',  ( 4.559911319644449179, 8.897018677488173211, 9.422509992056141925 ) ) ;
#71719 = CARTESIAN_POINT ( 'NONE',  ( 14.92337183194729988, 64.34226448433412315, -8.527530157486177487 ) ) ;
#71720 = DIRECTION ( 'NONE',  ( 0.000000000000000000, 0.000000000000000000, 1.000000000000000000 ) ) ;
#71721 = CARTESIAN_POINT ( 'NONE',  ( 4.559911319644449179, 62.23035201082150536, -9.422509992056141925 ) ) ;
#71722 = EDGE_CURVE ( 'NONE', #86936, #97713, #42942, .T. ) ;
#71723 = CARTESIAN_POINT ( 'NONE',  ( 19.84674366389459266, 28.30059781766745886, 2.638427012816836559 ) ) ;
#71724 = CARTESIAN_POINT ( 'NONE',  ( -5.320324007936277688, -24.96642978969368443, 3.999999999999999112 ) ) ;
#71725 = ORIENTED_EDGE ( 'NONE', *, *, #48113, .F. ) ;
#71726 = CARTESIAN_POINT ( 'NONE',  ( 15.81765804549837107, 15.00000000000000000, 2.383084218346927408 ) ) ;
#71727 = ORIENTED_EDGE ( 'NONE', *, *, #28521, .F. ) ;
#71728 = CARTESIAN_POINT ( 'NONE',  ( 10.00000000000000000, 19.75893115100078390, -9.846743663894594434 ) ) ;
#71729 = ORIENTED_EDGE ( 'NONE', *, *, #21925, .F. ) ;
#71730 = CARTESIAN_POINT ( 'NONE',  ( -0.3689425029237881626, 27.42874883491397142, 10.36894250292379027 ) ) ;
#71731 = CARTESIAN_POINT ( 'NONE',  ( 10.00000000000000178, 27.25893115100078390, 9.846743663894594434 ) ) ;
#71732 = CARTESIAN_POINT ( 'NONE',  ( 4.559911319644449179, 57.23035201082150536, -9.422509992056141925 ) ) ;
#71733 = DIRECTION ( 'NONE',  ( -1.000000000000000000, 0.000000000000000000, 0.000000000000000000 ) ) ;
#71734 = CARTESIAN_POINT ( 'NONE',  ( 2.035157376598824452, 43.68868534415484106, 7.964842623401179544 ) ) ;
#71735 = CARTESIAN_POINT ( 'NONE',  ( 5.076628168052703671, 41.84226448433411605, 8.527530157486179263 ) ) ;
#71736 = B_SPLINE_CURVE_WITH_KNOTS ( 'NONE', 3,
 ( #44202, #97740, #74712, #98736, #92183, #30678 ),
 .UNSPECIFIED., .F., .F.,
 ( 4, 2, 4 ),
 ( 3.409110551496111717E-05, 0.0004400426677367866800, 0.0008459942299586122429 ),
 .UNSPECIFIED. ) ;
#71737 = CARTESIAN_POINT ( 'NONE',  ( 12.81628187352647608, -8.584698663402908991, 3.434112377981052511 ) ) ;
#71738 = ORIENTED_EDGE ( 'NONE', *, *, #33841, .F. ) ;
#71739 = CARTESIAN_POINT ( 'NONE',  ( 2.035157376598822676, 42.43868534415483396, -7.964842623401177768 ) ) ;
#71740 = CARTESIAN_POINT ( 'NONE',  ( -0.3689425029237898834, 6.178748834913968757, -10.36894250292378850 ) ) ;
#71741 = ORIENTED_EDGE ( 'NONE', *, *, #3531, .F. ) ;
#71742 = VERTEX_POINT ( 'NONE', #27221 ) ;
#71743 = CARTESIAN_POINT ( 'NONE',  ( -2.816281873526471635, 33.91530133659708213, -3.434112377981056508 ) ) ;
#71744 = AXIS2_PLACEMENT_3D ( 'NONE', #39617, #9596, #24120 ) ;
#71745 = LINE ( 'NONE', #94234, #41416 ) ;
#71746 = CARTESIAN_POINT ( 'NONE',  ( 5.076628168052704559, 25.17559781766745175, -8.527530157486179263 ) ) ;
#71747 = CARTESIAN_POINT ( 'NONE',  ( 12.91533473730992121, 4.522018677488169658, 10.88017736071110164 ) ) ;
#71748 = CARTESIAN_POINT ( 'NONE',  ( 10.00000000000000000, 29.75893115100078745, -9.846743663894594434 ) ) ;
#71749 = EDGE_CURVE ( 'NONE', #38758, #23770, #69239, .T. ) ;
#71750 = CARTESIAN_POINT ( 'NONE',  ( -0.8801773607111008646, 63.27201867748817676, 2.915334737309923430 ) ) ;
#71751 = CARTESIAN_POINT ( 'NONE',  ( -11.81378540890925066, -0.03417435944610275333, -7.968498874458281200 ) ) ;
#71752 = CARTESIAN_POINT ( 'NONE',  ( 9.383795276901695459, 0.2306972965111900586, 11.62679839395699943 ) ) ;
#71753 = CARTESIAN_POINT ( 'NONE',  ( -0.04068437667225256044, 17.21974360917720404, -6.396802510829700417 ) ) ;
#71754 = CARTESIAN_POINT ( 'NONE',  ( 1.472469842513823179, 6.425597817667451750, 4.923371831947296329 ) ) ;
#71755 = CARTESIAN_POINT ( 'NONE',  ( 21.09922568453594849, 16.20696800326375353, 6.408140936763242479 ) ) ;
#71756 = CARTESIAN_POINT ( 'NONE',  ( 26.00000000000000355, 35.99999999999997158, -7.000000000000000000 ) ) ;
#71757 = EDGE_CURVE ( 'NONE', #85662, #23769, #23827, .T. ) ;
#71758 = CARTESIAN_POINT ( 'NONE',  ( 1.472469842513823179, 50.59226448433411605, -4.923371831947296329 ) ) ;
#71759 = CARTESIAN_POINT ( 'NONE',  ( 19.10478245763053451, 35.10160829253886305, 5.990408912944295672 ) ) ;
#71760 = CARTESIAN_POINT ( 'NONE',  ( -2.266590686148945544, 11.38708216824730179, -7.082119434687050408 ) ) ;
#71761 = CARTESIAN_POINT ( 'NONE',  ( 0.1532563361054082862, 31.21726448433412315, 2.638427012816831674 ) ) ;
#71762 = CARTESIAN_POINT ( 'NONE',  ( -2.816281873526471635, 28.91530133659708213, -3.434112377981056508 ) ) ;
#71764 = CARTESIAN_POINT ( 'NONE',  ( -14.43100913236848371, 4.112960668137814512E-16, -1.412789942453356318 ) ) ;
#71763 =( NAMED_UNIT ( * ) PLANE_ANGLE_UNIT ( ) SI_UNIT ( $, .RADIAN. ) );
#71765 = CARTESIAN_POINT ( 'NONE',  ( 0.5774900079438607392, 53.48035201082151247, 5.440088680355550821 ) ) ;
#71766 = CARTESIAN_POINT ( 'NONE',  ( -1.099225684535947600, 8.706968003263753531, -6.408140936763238038 ) ) ;
#71767 = LINE ( 'NONE', #79759, #64679 ) ;
#71768 = CARTESIAN_POINT ( 'NONE',  ( 19.84674366389459266, 18.71726448433411960, -2.638427012816827677 ) ) ;
#71769 = CARTESIAN_POINT ( 'NONE',  ( 17.96484262340118221, 26.18868534415483396, -7.964842623401177768 ) ) ;
#71770 = CARTESIAN_POINT ( 'NONE',  ( 0.6178305044545838731, 29.74863466993042138, 9.382169495545420901 ) ) ;
#71771 = CARTESIAN_POINT ( 'NONE',  ( 14.92337183194729988, 19.34226448433411960, -8.527530157486177487 ) ) ;
#71772 =( BOUNDED_SURFACE ( )  B_SPLINE_SURFACE ( 1, 2, ( 
 ( #48532, #88009, #33520, #49511, #64509, #19035, #64016, #11036, #88505, #26048, #94528, #96022, #73002, #95013, #80018, #18540, #3067, #11520, #49031, #57513, #42044, #79032, #19521, #3551, #12508, #5018, #34503, #56538, #65500, #79536, #87028, #41558, #35501, #72022, #26522, #27503, #64995, #57018, #65996, #96524, #87520, #86548, #10545, #81007, #4041, #50017, #95521, #27014, #57999, #80521, #12019, #20008, #42519, #4533, #34997, #73491, #50509, #43009, #56055, #41055, #71554, #73991, #89496, #44971, #81491, #66992, #98510, #82981, #75476, #21499, #35994, #14997, #21007, #97515, #89004, #52476, #20511, #5517, #67489, #6991, #58493, #97023, #98011, #50996, #12994, #66497, #6486, #43490, #22001, #37495, #22491, #58994, #6005, #83475, #29964, #51494, #29465, #51996, #28500, #36500, #45467, #7495, #74483, #28978, #60470, #14003, #81988, #67983, #75967, #13500, #43979, #90959, #59481, #37989, #52964, #89982, #82485, #44480, #36993, #68481, #14501, #74982, #27996, #59971, #90466, #78425, #8943, #76948, #16458, #16949, #61449, #8458, #31438, #23964, #47434, #77431, #84465, #62425, #17453, #38964, #70445, #54438, #69457, #31925, #84947, #92928, #46938, #9942, #91464, #46455, #85442, #61940, #53456, #60955, #68970, #30950, #23485, #83963, #501, #91955, #55437, #24953, #9441, #975, #69952, #39462, #92441, #1471, #53958, #77933, #85942, #22990, #38477, #39942, #24460, #47920, #40445, #54926, #1962, #32428, #62929, #93431, #8, #30456, #15490, #45973, #76463, #7978, #15963, #48906, #88753, #89248, #33398, #79421, #3427, #94901, #20758, #50762, #56427, #35751, #89733, #10918, #43741, #26399, #41443, #5274, #58233, #66238, #20263, #51750, #63422, #18423, #58744, #33886, #25451, #32920, #40937, #2950, #94410, #55934, #71435, #63897, #28741, #97270, #81734, #71903, #43248, #81251, #64391, #82234, #25925, #2464, #93925, #59232, #10430, #96773, #86914, #12749, #74227, #73743, #78920, #13250, #28249, #51247, #5761, #21252, #36249, #66746, #13749, #70946, #86434, #17933, #48418, #61216, #97768, #83230, #15739, #255, #91719, #37747, #52239, #31199, #37258, #14754, #6249, #68727, #36753, #21758, #83727, #23240, #74736, #14250, #15250, #67243, #29232, #82731, #22741, #59731, #38237, #53712, #38721, #75228, #22248, #746, #46222, #6741, #45727, #68245, #44731, #52724, #61692, #23734, #90723, #45228, #76707, #60228, #75726, #30704, #67745, #60716, #92208, #44232, #84231, #8227, #69221, #90226, #54197, #76229, #91213, #7241, #7743, #98265, #84712, #29722, #98763, #30213, #53224, #69706, #33647, #85691, #56660, #16214, #54682, #2215, #24705, #56183, #39220, #85204, #79163, #9694, #55690, #17211, #55176, #41191, #86188, #16708, #70696, #64143, #77198, #39712, #71186, #93179, #77685, #47181, #32674, #1236, #9200, #63168, #2711 ),
 ( #63657, #94660, #48169, #33163, #8703, #78681, #92691, #40188, #47688, #78181, #24216, #70201, #48661, #1720, #32176, #86676, #94163, #93675, #25210, #62679, #62181, #17698, #10192, #40685, #25692, #31691, #18181, #10676, #71671, #26169, #3181, #46699, #96651, #11654, #87643, #19157, #36121, #26650, #49636, #28130, #96152, #34632, #97158, #89129, #50641, #72148, #80649, #88628, #81130, #65627, #66629, #58630, #20640, #35128, #28626, #73623, #58120, #27635, #5146, #57146, #51129, #50140, #12143, #12632, #35636, #81619, #80144, #65131, #43625, #13128, #42169, #20137, #42648, #95139, #95652, #5645, #87149, #27136, #57640, #74111, #73124, #72632, #66122, #18674, #11159, #4164, #49160, #88135, #79663, #41679, #19648, #4666, #43131, #3676, #34138, #64630, #98136, #83612, #46106, #76100, #38603, #68119, #37132, #75608, #7631, #21635, #67627, #90600, #83109, #38122, #37623, #44616, #22623, #76590, #29597, #30588, #14638, #60099, #91096, #45101, #53102, #7119, #69102, #51636, #6618, #45602, #22127, #13625, #21135, #29110, #90110, #82615, #44107, #59613, #52121, #15621, #84105, #68610, #52608, #30094, #98645, #60601, #636, #14131, #89623, #82115, #8108, #97646, #15127, #75112, #139, #61093, #91603, #67121, #23119, #53591, #59113, #74618, #6132, #36638, #62068, #9576, #92575, #84599, #77082, #24099, #48051, #16097, #70085, #2598, #86074, #78565, #24596, #39100, #18069, #54568, #1609, #92090, #55576, #23618, #8593, #70577, #10075, #61579, #1111, #2104, #54083, #46584, #69591, #40076, #31574, #25093, #86566, #56071, #40576, #32058, #32563, #55061, #62561, #41072, #85084, #16592, #47069, #48548, #77567, #63061, #9083, #39597, #33052, #93065, #85579, #71073, #93559, #17093, #17586, #79048, #63548, #47575, #94057, #78071, #25579, #10561, #71567, #31084, #56553, #42060, #73508, #58011, #50524, #95539, #11053, #89018, #95030, #72523, #64032, #27520, #94544, #79554, #42532, #81021, #33537, #72040, #73016, #26062, #87047, #41573, #80535, #18558, #96036, #12523, #96538, #34028, #80034, #58509, #5032, #64525, #4549, #27029, #3570, #11539, #20527, #81507, #49527, #4057, #35519, #88023, #26539, #43025, #51012, #49050, #57035, #66010, #34518, #13011, #28013, #65011, #57528, #19536, #12034, #43508, #88521, #50032, #20024, #3079, #87537, #19050, #35013, #65514, #90480, #90975, #36517, #82499, #6500, #98024, #22508, #52491, #59499, #37509, #91484, #14017, #45482, #29478, #44497, #7004, #59987, #68002, #22017, #53473, #66513, #21513, #60486, #37008, #28515, #36011, #43996, #6021, #97530, #59009, #74498, #67009, #83983, #75984, #83494, #82998, #15508, #52980, #44985, #14516, #15013, #13515, #7513, #67504, #75492, #98528, #89997, #74998, #29981, #28989, #38004, #30471, #74006, #68497, #24, #60972, #97040, #23005, #5531, #89512, #21022 ) ),
 .UNSPECIFIED., .F., .F., .T. ) 
 B_SPLINE_SURFACE_WITH_KNOTS ( ( 2, 2 ),
 ( 3, 2, 2, 2, 2, 2, 2, 2, 2, 2, 2, 2, 2, 2, 2, 2, 2, 2, 2, 2, 2, 2, 2, 2, 2, 2, 2, 2, 2, 2, 2, 2, 2, 2, 2, 2, 2, 2, 2, 2, 2, 2, 2, 2, 2, 2, 2, 2, 2, 2, 2, 2, 2, 2, 2, 2, 2, 2, 2, 2, 2, 2, 2, 2, 2, 2, 2, 2, 2, 2, 2, 2, 2, 2, 2, 2, 2, 2, 2, 2, 2, 2, 2, 2, 2, 2, 2, 2, 2, 2, 2, 2, 2, 2, 2, 2, 2, 2, 2, 2, 2, 2, 2, 2, 2, 2, 2, 2, 2, 2, 2, 2, 2, 2, 2, 2, 2, 2, 2, 2, 2, 2, 2, 2, 2, 2, 2, 2, 2, 2, 2, 2, 2, 2, 2, 2, 2, 2, 2, 2, 2, 2, 2, 2, 2, 2, 2, 2, 2, 2, 2, 2, 2, 2, 2, 2, 2, 2, 2, 2, 2, 2, 2, 2, 2, 2, 2, 2, 2, 2, 2, 2, 2, 2, 3 ),
 ( 0.000000000000000000, 1.000000000000000000 ),
 ( 0.000000000000000000, 0.005555555555555555768, 0.01111111111111111154, 0.01666666666666666644, 0.02222222222222222307, 0.02777777777777777624, 0.03333333333333333287, 0.03888888888888888951, 0.04444444444444444614, 0.05000000000000000278, 0.05555555555555555247, 0.06111111111111110911, 0.06666666666666666574, 0.07222222222222221544, 0.07777777777777777901, 0.08333333333333332871, 0.08888888888888889228, 0.09444444444444444198, 0.1000000000000000056, 0.1055555555555555552, 0.1111111111111111049, 0.1166666666666666685, 0.1222222222222222182, 0.1277777777777777679, 0.1333333333333333315, 0.1388888888888888951, 0.1444444444444444309, 0.1499999999999999944, 0.1555555555555555580, 0.1611111111111111216, 0.1666666666666666574, 0.1722222222222222210, 0.1777777777777777846, 0.1833333333333333204, 0.1888888888888888840, 0.1944444444444444475, 0.2000000000000000111, 0.2055555555555555469, 0.2111111111111111105, 0.2166666666666666741, 0.2222222222222222099, 0.2277777777777777735, 0.2333333333333333370, 0.2388888888888889006, 0.2444444444444444364, 0.2500000000000000000, 0.2555555555555555358, 0.2611111111111111271, 0.2666666666666666630, 0.2722222222222221988, 0.2777777777777777901, 0.2833333333333333259, 0.2888888888888888618, 0.2944444444444444531, 0.2999999999999999889, 0.3055555555555555802, 0.3111111111111111160, 0.3166666666666666519, 0.3222222222222222432, 0.3277777777777777790, 0.3333333333333333148, 0.3388888888888889062, 0.3444444444444444420, 0.3499999999999999778, 0.3555555555555555691, 0.3611111111111111049, 0.3666666666666666408, 0.3722222222222222321, 0.3777777777777777679, 0.3833333333333333592, 0.3888888888888888951, 0.3944444444444444309, 0.4000000000000000222, 0.4055555555555555580, 0.4111111111111110938, 0.4166666666666666852, 0.4222222222222222210, 0.4277777777777777568, 0.4333333333333333481, 0.4388888888888888840, 0.4444444444444444198, 0.4500000000000000111, 0.4555555555555555469, 0.4611111111111111382, 0.4666666666666666741, 0.4722222222222222099, 0.4777777777777778012, 0.4833333333333333370, 0.4888888888888888729, 0.4944444444444444642, 0.5000000000000000000, 0.5055555555555555358, 0.5111111111111110716, 0.5166666666666667185, 0.5222222222222222543, 0.5277777777777777901, 0.5333333333333333259, 0.5388888888888888618, 0.5444444444444443976, 0.5500000000000000444, 0.5555555555555555802, 0.5611111111111111160, 0.5666666666666666519, 0.5722222222222221877, 0.5777777777777777235, 0.5833333333333333703, 0.5888888888888889062, 0.5944444444444444420, 0.5999999999999999778, 0.6055555555555555136, 0.6111111111111111605, 0.6166666666666666963, 0.6222222222222222321, 0.6277777777777777679, 0.6333333333333333037, 0.6388888888888888395, 0.6444444444444444864, 0.6500000000000000222, 0.6555555555555555580, 0.6611111111111110938, 0.6666666666666666297, 0.6722222222222222765, 0.6777777777777778123, 0.6833333333333333481, 0.6888888888888888840, 0.6944444444444444198, 0.6999999999999999556, 0.7055555555555556024, 0.7111111111111111382, 0.7166666666666666741, 0.7222222222222222099, 0.7277777777777777457, 0.7333333333333332815, 0.7388888888888889284, 0.7444444444444444642, 0.7500000000000000000, 0.7555555555555555358, 0.7611111111111110716, 0.7666666666666667185, 0.7722222222222222543, 0.7777777777777777901, 0.7833333333333333259, 0.7888888888888888618, 0.7944444444444443976, 0.8000000000000000444, 0.8055555555555555802, 0.8111111111111111160, 0.8166666666666666519, 0.8222222222222221877, 0.8277777777777777235, 0.8333333333333333703, 0.8388888888888889062, 0.8444444444444444420, 0.8499999999999999778, 0.8555555555555555136, 0.8611111111111111605, 0.8666666666666666963, 0.8722222222222222321, 0.8777777777777777679, 0.8833333333333333037, 0.8888888888888888395, 0.8944444444444444864, 0.9000000000000000222, 0.9055555555555555580, 0.9111111111111110938, 0.9166666666666666297, 0.9222222222222222765, 0.9277777777777778123, 0.9333333333333333481, 0.9388888888888888840, 0.9444444444444444198, 0.9499999999999999556, 0.9555555555555556024, 0.9611111111111111382, 0.9666666666666666741 ),
 .UNSPECIFIED. ) 
 GEOMETRIC_REPRESENTATION_ITEM ( )  RATIONAL_B_SPLINE_SURFACE ( (
 ( 1.000000000000000000, 0.9659258262890683122, 1.000000000000000000, 0.9659258262890683122, 1.000000000000000000, 0.9659258262890683122, 1.000000000000000000, 0.9659258262890683122, 1.000000000000000000, 0.9659258262890683122, 1.000000000000000000, 0.9659258262890683122, 1.000000000000000000, 0.9659258262890683122, 1.000000000000000000, 0.9659258262890683122, 1.000000000000000000, 0.9659258262890683122, 1.000000000000000000, 0.9659258262890683122, 1.000000000000000000, 0.9659258262890683122, 1.000000000000000000, 0.9659258262890683122, 1.000000000000000000, 0.9659258262890683122, 1.000000000000000000, 0.9659258262890683122, 1.000000000000000000, 0.9659258262890683122, 1.000000000000000000, 0.9659258262890683122, 1.000000000000000000, 0.9659258262890683122, 1.000000000000000000, 0.9659258262890683122, 1.000000000000000000, 0.9659258262890683122, 1.000000000000000000, 0.9659258262890683122, 1.000000000000000000, 0.9659258262890683122, 1.000000000000000000, 0.9659258262890683122, 1.000000000000000000, 0.9659258262890683122, 1.000000000000000000, 0.9659258262890683122, 1.000000000000000000, 0.9659258262890683122, 1.000000000000000000, 0.9659258262890683122, 1.000000000000000000, 0.9659258262890683122, 1.000000000000000000, 0.9659258262890683122, 1.000000000000000000, 0.9659258262890683122, 1.000000000000000000, 0.9659258262890683122, 1.000000000000000000, 0.9659258262890683122, 1.000000000000000000, 0.9659258262890683122, 1.000000000000000000, 0.9659258262890683122, 1.000000000000000000, 0.9659258262890683122, 1.000000000000000000, 0.9659258262890683122, 1.000000000000000000, 0.9659258262890683122, 1.000000000000000000, 0.9659258262890683122, 1.000000000000000000, 0.9659258262890683122, 1.000000000000000000, 0.9659258262890683122, 1.000000000000000000, 0.9659258262890683122, 1.000000000000000000, 0.9659258262890683122, 1.000000000000000000, 0.9659258262890683122, 1.000000000000000000, 0.9659258262890683122, 1.000000000000000000, 0.9659258262890683122, 1.000000000000000000, 0.9659258262890683122, 1.000000000000000000, 0.9659258262890683122, 1.000000000000000000, 0.9659258262890683122, 1.000000000000000000, 0.9659258262890683122, 1.000000000000000000, 0.9659258262890683122, 1.000000000000000000, 0.9659258262890683122, 1.000000000000000000, 0.9659258262890683122, 1.000000000000000000, 0.9659258262890683122, 1.000000000000000000, 0.9659258262890683122, 1.000000000000000000, 0.9659258262890683122, 1.000000000000000000, 0.9659258262890683122, 1.000000000000000000, 0.9659258262890683122, 1.000000000000000000, 0.9659258262890683122, 1.000000000000000000, 0.9659258262890683122, 1.000000000000000000, 0.9659258262890683122, 1.000000000000000000, 0.9659258262890683122, 1.000000000000000000, 0.9659258262890683122, 1.000000000000000000, 0.9659258262890683122, 1.000000000000000000, 0.9659258262890683122, 1.000000000000000000, 0.9659258262890683122, 1.000000000000000000, 0.9659258262890683122, 1.000000000000000000, 0.9659258262890683122, 1.000000000000000000, 0.9659258262890683122, 1.000000000000000000, 0.9659258262890683122, 1.000000000000000000, 0.9659258262890683122, 1.000000000000000000, 0.9659258262890683122, 1.000000000000000000, 0.9659258262890683122, 1.000000000000000000, 0.9659258262890683122, 1.000000000000000000, 0.9659258262890683122, 1.000000000000000000, 0.9659258262890683122, 1.000000000000000000, 0.9659258262890683122, 1.000000000000000000, 0.9659258262890683122, 1.000000000000000000, 0.9659258262890683122, 1.000000000000000000, 0.9659258262890683122, 1.000000000000000000, 0.9659258262890683122, 1.000000000000000000, 0.9659258262890683122, 1.000000000000000000, 0.9659258262890683122, 1.000000000000000000, 0.9659258262890683122, 1.000000000000000000, 0.9659258262890683122, 1.000000000000000000, 0.9659258262890683122, 1.000000000000000000, 0.9659258262890683122, 1.000000000000000000, 0.9659258262890683122, 1.000000000000000000, 0.9659258262890683122, 1.000000000000000000, 0.9659258262890683122, 1.000000000000000000, 0.9659258262890683122, 1.000000000000000000, 0.9659258262890683122, 1.000000000000000000, 0.9659258262890683122, 1.000000000000000000, 0.9659258262890683122, 1.000000000000000000, 0.9659258262890683122, 1.000000000000000000, 0.9659258262890683122, 1.000000000000000000, 0.9659258262890683122, 1.000000000000000000, 0.9659258262890683122, 1.000000000000000000, 0.9659258262890683122, 1.000000000000000000, 0.9659258262890683122, 1.000000000000000000, 0.9659258262890683122, 1.000000000000000000, 0.9659258262890683122, 1.000000000000000000, 0.9659258262890683122, 1.000000000000000000, 0.9659258262890683122, 1.000000000000000000, 0.9659258262890683122, 1.000000000000000000, 0.9659258262890683122, 1.000000000000000000, 0.9659258262890683122, 1.000000000000000000, 0.9659258262890683122, 1.000000000000000000, 0.9659258262890683122, 1.000000000000000000, 0.9659258262890683122, 1.000000000000000000, 0.9659258262890683122, 1.000000000000000000, 0.9659258262890683122, 1.000000000000000000, 0.9659258262890683122, 1.000000000000000000, 0.9659258262890683122, 1.000000000000000000, 0.9659258262890683122, 1.000000000000000000, 0.9659258262890683122, 1.000000000000000000, 0.9659258262890683122, 1.000000000000000000, 0.9659258262890683122, 1.000000000000000000, 0.9659258262890683122, 1.000000000000000000, 0.9659258262890683122, 1.000000000000000000, 0.9659258262890683122, 1.000000000000000000, 0.9659258262890683122, 1.000000000000000000, 0.9659258262890683122, 1.000000000000000000, 0.9659258262890683122, 1.000000000000000000, 0.9659258262890683122, 1.000000000000000000, 0.9659258262890683122, 1.000000000000000000, 0.9659258262890683122, 1.000000000000000000, 0.9659258262890683122, 1.000000000000000000, 0.9659258262890683122, 1.000000000000000000, 0.9659258262890683122, 1.000000000000000000, 0.9659258262890683122, 1.000000000000000000, 0.9659258262890683122, 1.000000000000000000, 0.9659258262890683122, 1.000000000000000000, 0.9659258262890683122, 1.000000000000000000, 0.9659258262890683122, 1.000000000000000000, 0.9659258262890683122, 1.000000000000000000, 0.9659258262890683122, 1.000000000000000000, 0.9659258262890683122, 1.000000000000000000, 0.9659258262890683122, 1.000000000000000000, 0.9659258262890683122, 1.000000000000000000, 0.9659258262890683122, 1.000000000000000000, 0.9659258262890683122, 1.000000000000000000, 0.9659258262890683122, 1.000000000000000000, 0.9659258262890683122, 1.000000000000000000, 0.9659258262890683122, 1.000000000000000000, 0.9659258262890683122, 1.000000000000000000, 0.9659258262890683122, 1.000000000000000000, 0.9659258262890683122, 1.000000000000000000, 0.9659258262890683122, 1.000000000000000000, 0.9659258262890683122, 1.000000000000000000, 0.9659258262890683122, 1.000000000000000000, 0.9659258262890683122, 1.000000000000000000, 0.9659258262890683122, 1.000000000000000000, 0.9659258262890683122, 1.000000000000000000, 0.9659258262890683122, 1.000000000000000000, 0.9659258262890683122, 1.000000000000000000, 0.9659258262890683122, 1.000000000000000000, 0.9659258262890683122, 1.000000000000000000, 0.9659258262890683122, 1.000000000000000000, 0.9659258262890683122, 1.000000000000000000, 0.9659258262890683122, 1.000000000000000000, 0.9659258262890683122, 1.000000000000000000, 0.9659258262890683122, 1.000000000000000000, 0.9659258262890683122, 1.000000000000000000, 0.9659258262890683122, 1.000000000000000000, 0.9659258262890683122, 1.000000000000000000, 0.9659258262890683122, 1.000000000000000000, 0.9659258262890683122, 1.000000000000000000, 0.9659258262890683122, 1.000000000000000000, 0.9659258262890683122, 1.000000000000000000, 0.9659258262890683122, 1.000000000000000000, 0.9659258262890683122, 1.000000000000000000, 0.9659258262890683122, 1.000000000000000000, 0.9659258262890683122, 1.000000000000000000, 0.9659258262890683122, 1.000000000000000000, 0.9659258262890683122, 1.000000000000000000),
 ( 1.000000000000000000, 0.9659258262890683122, 1.000000000000000000, 0.9659258262890683122, 1.000000000000000000, 0.9659258262890683122, 1.000000000000000000, 0.9659258262890683122, 1.000000000000000000, 0.9659258262890683122, 1.000000000000000000, 0.9659258262890683122, 1.000000000000000000, 0.9659258262890683122, 1.000000000000000000, 0.9659258262890683122, 1.000000000000000000, 0.9659258262890683122, 1.000000000000000000, 0.9659258262890683122, 1.000000000000000000, 0.9659258262890683122, 1.000000000000000000, 0.9659258262890683122, 1.000000000000000000, 0.9659258262890683122, 1.000000000000000000, 0.9659258262890683122, 1.000000000000000000, 0.9659258262890683122, 1.000000000000000000, 0.9659258262890683122, 1.000000000000000000, 0.9659258262890683122, 1.000000000000000000, 0.9659258262890683122, 1.000000000000000000, 0.9659258262890683122, 1.000000000000000000, 0.9659258262890683122, 1.000000000000000000, 0.9659258262890683122, 1.000000000000000000, 0.9659258262890683122, 1.000000000000000000, 0.9659258262890683122, 1.000000000000000000, 0.9659258262890683122, 1.000000000000000000, 0.9659258262890683122, 1.000000000000000000, 0.9659258262890683122, 1.000000000000000000, 0.9659258262890683122, 1.000000000000000000, 0.9659258262890683122, 1.000000000000000000, 0.9659258262890683122, 1.000000000000000000, 0.9659258262890683122, 1.000000000000000000, 0.9659258262890683122, 1.000000000000000000, 0.9659258262890683122, 1.000000000000000000, 0.9659258262890683122, 1.000000000000000000, 0.9659258262890683122, 1.000000000000000000, 0.9659258262890683122, 1.000000000000000000, 0.9659258262890683122, 1.000000000000000000, 0.9659258262890683122, 1.000000000000000000, 0.9659258262890683122, 1.000000000000000000, 0.9659258262890683122, 1.000000000000000000, 0.9659258262890683122, 1.000000000000000000, 0.9659258262890683122, 1.000000000000000000, 0.9659258262890683122, 1.000000000000000000, 0.9659258262890683122, 1.000000000000000000, 0.9659258262890683122, 1.000000000000000000, 0.9659258262890683122, 1.000000000000000000, 0.9659258262890683122, 1.000000000000000000, 0.9659258262890683122, 1.000000000000000000, 0.9659258262890683122, 1.000000000000000000, 0.9659258262890683122, 1.000000000000000000, 0.9659258262890683122, 1.000000000000000000, 0.9659258262890683122, 1.000000000000000000, 0.9659258262890683122, 1.000000000000000000, 0.9659258262890683122, 1.000000000000000000, 0.9659258262890683122, 1.000000000000000000, 0.9659258262890683122, 1.000000000000000000, 0.9659258262890683122, 1.000000000000000000, 0.9659258262890683122, 1.000000000000000000, 0.9659258262890683122, 1.000000000000000000, 0.9659258262890683122, 1.000000000000000000, 0.9659258262890683122, 1.000000000000000000, 0.9659258262890683122, 1.000000000000000000, 0.9659258262890683122, 1.000000000000000000, 0.9659258262890683122, 1.000000000000000000, 0.9659258262890683122, 1.000000000000000000, 0.9659258262890683122, 1.000000000000000000, 0.9659258262890683122, 1.000000000000000000, 0.9659258262890683122, 1.000000000000000000, 0.9659258262890683122, 1.000000000000000000, 0.9659258262890683122, 1.000000000000000000, 0.9659258262890683122, 1.000000000000000000, 0.9659258262890683122, 1.000000000000000000, 0.9659258262890683122, 1.000000000000000000, 0.9659258262890683122, 1.000000000000000000, 0.9659258262890683122, 1.000000000000000000, 0.9659258262890683122, 1.000000000000000000, 0.9659258262890683122, 1.000000000000000000, 0.9659258262890683122, 1.000000000000000000, 0.9659258262890683122, 1.000000000000000000, 0.9659258262890683122, 1.000000000000000000, 0.9659258262890683122, 1.000000000000000000, 0.9659258262890683122, 1.000000000000000000, 0.9659258262890683122, 1.000000000000000000, 0.9659258262890683122, 1.000000000000000000, 0.9659258262890683122, 1.000000000000000000, 0.9659258262890683122, 1.000000000000000000, 0.9659258262890683122, 1.000000000000000000, 0.9659258262890683122, 1.000000000000000000, 0.9659258262890683122, 1.000000000000000000, 0.9659258262890683122, 1.000000000000000000, 0.9659258262890683122, 1.000000000000000000, 0.9659258262890683122, 1.000000000000000000, 0.9659258262890683122, 1.000000000000000000, 0.9659258262890683122, 1.000000000000000000, 0.9659258262890683122, 1.000000000000000000, 0.9659258262890683122, 1.000000000000000000, 0.9659258262890683122, 1.000000000000000000, 0.9659258262890683122, 1.000000000000000000, 0.9659258262890683122, 1.000000000000000000, 0.9659258262890683122, 1.000000000000000000, 0.9659258262890683122, 1.000000000000000000, 0.9659258262890683122, 1.000000000000000000, 0.9659258262890683122, 1.000000000000000000, 0.9659258262890683122, 1.000000000000000000, 0.9659258262890683122, 1.000000000000000000, 0.9659258262890683122, 1.000000000000000000, 0.9659258262890683122, 1.000000000000000000, 0.9659258262890683122, 1.000000000000000000, 0.9659258262890683122, 1.000000000000000000, 0.9659258262890683122, 1.000000000000000000, 0.9659258262890683122, 1.000000000000000000, 0.9659258262890683122, 1.000000000000000000, 0.9659258262890683122, 1.000000000000000000, 0.9659258262890683122, 1.000000000000000000, 0.9659258262890683122, 1.000000000000000000, 0.9659258262890683122, 1.000000000000000000, 0.9659258262890683122, 1.000000000000000000, 0.9659258262890683122, 1.000000000000000000, 0.9659258262890683122, 1.000000000000000000, 0.9659258262890683122, 1.000000000000000000, 0.9659258262890683122, 1.000000000000000000, 0.9659258262890683122, 1.000000000000000000, 0.9659258262890683122, 1.000000000000000000, 0.9659258262890683122, 1.000000000000000000, 0.9659258262890683122, 1.000000000000000000, 0.9659258262890683122, 1.000000000000000000, 0.9659258262890683122, 1.000000000000000000, 0.9659258262890683122, 1.000000000000000000, 0.9659258262890683122, 1.000000000000000000, 0.9659258262890683122, 1.000000000000000000, 0.9659258262890683122, 1.000000000000000000, 0.9659258262890683122, 1.000000000000000000, 0.9659258262890683122, 1.000000000000000000, 0.9659258262890683122, 1.000000000000000000, 0.9659258262890683122, 1.000000000000000000, 0.9659258262890683122, 1.000000000000000000, 0.9659258262890683122, 1.000000000000000000, 0.9659258262890683122, 1.000000000000000000, 0.9659258262890683122, 1.000000000000000000, 0.9659258262890683122, 1.000000000000000000, 0.9659258262890683122, 1.000000000000000000, 0.9659258262890683122, 1.000000000000000000, 0.9659258262890683122, 1.000000000000000000, 0.9659258262890683122, 1.000000000000000000, 0.9659258262890683122, 1.000000000000000000, 0.9659258262890683122, 1.000000000000000000, 0.9659258262890683122, 1.000000000000000000, 0.9659258262890683122, 1.000000000000000000, 0.9659258262890683122, 1.000000000000000000, 0.9659258262890683122, 1.000000000000000000, 0.9659258262890683122, 1.000000000000000000, 0.9659258262890683122, 1.000000000000000000, 0.9659258262890683122, 1.000000000000000000, 0.9659258262890683122, 1.000000000000000000, 0.9659258262890683122, 1.000000000000000000, 0.9659258262890683122, 1.000000000000000000, 0.9659258262890683122, 1.000000000000000000, 0.9659258262890683122, 1.000000000000000000, 0.9659258262890683122, 1.000000000000000000, 0.9659258262890683122, 1.000000000000000000, 0.9659258262890683122, 1.000000000000000000, 0.9659258262890683122, 1.000000000000000000, 0.9659258262890683122, 1.000000000000000000, 0.9659258262890683122, 1.000000000000000000, 0.9659258262890683122, 1.000000000000000000, 0.9659258262890683122, 1.000000000000000000, 0.9659258262890683122, 1.000000000000000000, 0.9659258262890683122, 1.000000000000000000, 0.9659258262890683122, 1.000000000000000000, 0.9659258262890683122, 1.000000000000000000, 0.9659258262890683122, 1.000000000000000000, 0.9659258262890683122, 1.000000000000000000, 0.9659258262890683122, 1.000000000000000000, 0.9659258262890683122, 1.000000000000000000, 0.9659258262890683122, 1.000000000000000000) ) ) 
 REPRESENTATION_ITEM ( '' )  SURFACE ( )  );
#71773 =( NAMED_UNIT ( * ) SI_UNIT ( $, .STERADIAN. ) SOLID_ANGLE_UNIT ( ) );
#71774 = CARTESIAN_POINT ( 'NONE',  ( -9.297374403301716939, 88.08016496434417775, 4.860721439949188039 ) ) ;
#71775 = CARTESIAN_POINT ( 'NONE',  ( 12.91533473730993009, 31.60535201082150891, -10.88017736071109987 ) ) ;
#71776 = VERTEX_POINT ( 'NONE', #34721 ) ;
#71777 = CARTESIAN_POINT ( 'NONE',  ( 20.88017736071110519, 60.56368534415484106, 2.639326808657452039E-16 ) ) ;
#71778 = CARTESIAN_POINT ( 'NONE',  ( 32.26500600480481040, 44.99999999999999289, 0.000000000000000000 ) ) ;
#71780 = CARTESIAN_POINT ( 'NONE',  ( 12.91533473730992121, 24.52201867748816966, 10.88017736071110164 ) ) ;
#71779 = CARTESIAN_POINT ( 'NONE',  ( 7.361572987183170547, 47.05059781766745175, 9.846743663894590881 ) ) ;
#71781 = SURFACE_SIDE_STYLE ('',( #41308 ) ) ;
#71782 = CARTESIAN_POINT ( 'NONE',  ( 0.5774900079438607392, 48.48035201082150536, 5.440088680355550821 ) ) ;
#71784 = PRESENTATION_STYLE_ASSIGNMENT (( #79285 ) ) ;
#71783 = CARTESIAN_POINT ( 'NONE',  ( -0.8801773607111009756, 13.06368534415483929, 1.068504757029289695E-15 ) ) ;
#71785 = CARTESIAN_POINT ( 'NONE',  ( 0.000000000000000000, 15.00000000000000000, 0.000000000000000000 ) ) ;
#71786 = CARTESIAN_POINT ( 'NONE',  ( 5.076628168052703671, 41.84226448433411605, 8.527530157486179263 ) ) ;
#71788 =( LENGTH_UNIT ( ) NAMED_UNIT ( * ) SI_UNIT ( .MILLI., .METRE. ) );
#71787 = CARTESIAN_POINT ( 'NONE',  ( 20.36894250292379382, 38.67874883491396076, 10.36894250292379205 ) ) ;
#71789 = CARTESIAN_POINT ( 'NONE',  ( 2.603489959281586774, 5.435752660568278216, -6.500000000000001776 ) ) ;
#71790 = AXIS2_PLACEMENT_3D ( 'NONE', #42550, #44517, #37031 ) ;
#71791 = SURFACE_SIDE_STYLE ('',( #32793 ) ) ;
#71792 = EDGE_CURVE ( 'NONE', #34469, #83674, #35717, .T. ) ;
#71793 = CARTESIAN_POINT ( 'NONE',  ( 2.917880565312948704, 22.63708216824730002, 12.26659068614894643 ) ) ;
#71794 = CARTESIAN_POINT ( 'NONE',  ( -13.82671409943298357, -0.03417435944610275333, 3.447387012295131115 ) ) ;
#71795 = ORIENTED_EDGE ( 'NONE', *, *, #32623, .T. ) ;
#71796 = CARTESIAN_POINT ( 'NONE',  ( -0.8801773607110991993, 2.855352010821504471, -2.915334737309923874 ) ) ;
#71797 = ADVANCED_FACE ( 'NONE', ( #64717 ), #36528, .T. ) ;
#71798 = CARTESIAN_POINT ( 'NONE',  ( 12.63842701281683034, 32.46726448433412315, 9.846743663894596210 ) ) ;
#71800 = DIRECTION ( 'NONE',  ( 0.000000000000000000, 0.000000000000000000, 1.000000000000000000 ) ) ;
#71799 = LINE ( 'NONE', #2835, #88256 ) ;
#71801 = CARTESIAN_POINT ( 'NONE',  ( 17.96484262340118221, 54.93868534415484106, 7.964842623401181321 ) ) ;
#71802 = CARTESIAN_POINT ( 'NONE',  ( 19.38216949554541202, 60.99863466993042493, 9.382169495545424454 ) ) ;
#71803 = CARTESIAN_POINT ( 'NONE',  ( 10.00000000000000000, 36.81368534415484106, -10.88017736071110342 ) ) ;
#71804 = CARTESIAN_POINT ( 'NONE',  ( 0.6178305044545838731, 64.74863466993043914, 9.382169495545420901 ) ) ;
#71805 = CARTESIAN_POINT ( 'NONE',  ( 22.81628187352648496, 11.83196800326375531, -3.434112377981050290 ) ) ;
#71806 = CARTESIAN_POINT ( 'NONE',  ( 10.00000000000000178, 12.25893115100078568, 9.846743663894594434 ) ) ;
#71807 = ORIENTED_EDGE ( 'NONE', *, *, #16284, .F. ) ;
#71808 = DIRECTION ( 'NONE',  ( 1.000000000000000000, 0.000000000000000000, 0.000000000000000000 ) ) ;
#71809 = CARTESIAN_POINT ( 'NONE',  ( 2.917880565312950480, 60.97041550158063927, -12.26659068614894821 ) ) ;
#71810 = CARTESIAN_POINT ( 'NONE',  ( 2.917880565312950480, 20.97041550158063217, -12.26659068614894821 ) ) ;
#71811 = CARTESIAN_POINT ( 'NONE',  ( 19.42250999205614193, 30.14701867748817321, 5.440088680355555262 ) ) ;
#71812 = CARTESIAN_POINT ( 'NONE',  ( -0.8801773607111008646, 43.27201867748817676, 2.915334737309923430 ) ) ;
#71813 = PRESENTATION_LAYER_ASSIGNMENT (  '', '', ( #76585 ) ) ;
#71814 = CARTESIAN_POINT ( 'NONE',  ( 8.862914611995314829, -7.247476534008700177, -4.000000000000000888 ) ) ;
#71815 = CARTESIAN_POINT ( 'NONE',  ( 0.1532563361054100626, 5.800597817667452638, -2.638427012816831230 ) ) ;
#71816 = CARTESIAN_POINT ( 'NONE',  ( -14.36343418943216577, 0.04922511925147166761, 3.367173657400553743 ) ) ;
#71817 = CARTESIAN_POINT ( 'NONE',  ( 17.20831665107776587, 17.88393115100078745, 7.208316651077764980 ) ) ;
#71818 = LINE ( 'NONE', #3325, #3258 ) ;
#71819 = CARTESIAN_POINT ( 'NONE',  ( 2.791683348922237240, 20.38393115100078745, -7.208316651077763204 ) ) ;
#71820 = CARTESIAN_POINT ( 'NONE',  ( 2.791683348922240793, 51.63393115100078745, 7.208316651077764092 ) ) ;
#71821 = ADVANCED_FACE ( 'NONE', ( #65214 ), #64229, .F. ) ;
#71822 = CARTESIAN_POINT ( 'NONE',  ( 20.88017736071110875, 25.77201867748816966, -2.915334737309920765 ) ) ;
#71823 = CARTESIAN_POINT ( 'NONE',  ( 0.6178305044545838731, 44.74863466993042493, 9.382169495545420901 ) ) ;
#71824 = CARTESIAN_POINT ( 'NONE',  ( 10.00000000000000000, 56.81368534415484106, -10.88017736071110342 ) ) ;
#71825 = CARTESIAN_POINT ( 'NONE',  ( 10.00000000000000178, 27.25893115100078390, 9.846743663894594434 ) ) ;
#71827 = CARTESIAN_POINT ( 'NONE',  ( 2.791683348922240793, 16.63393115100078745, 7.208316651077764092 ) ) ;
#71826 = CARTESIAN_POINT ( 'NONE',  ( 22.26659068614895176, 44.72041550158063927, -7.082119434687042414 ) ) ;
#71828 = CARTESIAN_POINT ( 'NONE',  ( 1.821158202401483850, 51.16688879859522388, 6.499999999999917399 ) ) ;
#71829 = CARTESIAN_POINT ( 'NONE',  ( 0.1532563361054100626, 60.80059781766744464, -2.638427012816831230 ) ) ;
#71830 = CARTESIAN_POINT ( 'NONE',  ( -0.3689425029237898834, 11.17874883491396787, -10.36894250292378850 ) ) ;
#71831 = CARTESIAN_POINT ( 'NONE',  ( 17.08211943468705840, 25.13708216824730357, -12.26659068614894466 ) ) ;
#71832 = CARTESIAN_POINT ( 'NONE',  ( 5.076628168052703671, 31.84226448433412315, 8.527530157486179263 ) ) ;
#71833 = DIRECTION ( 'NONE',  ( -0.7253743710122912969, 0.000000000000000000, 0.6883545756937501370 ) ) ;
#71834 = CARTESIAN_POINT ( 'NONE',  ( 17.96484262340118221, 21.18868534415483396, -7.964842623401177768 ) ) ;
#71835 = EDGE_CURVE ( 'NONE', #84403, #10365, #26114, .T. ) ;
#71836 = CARTESIAN_POINT ( 'NONE',  ( 12.91533473730992121, 39.52201867748817676, 10.88017736071110164 ) ) ;
#71837 = CARTESIAN_POINT ( 'NONE',  ( 7.084665262690076126, 37.02201867748817676, -10.88017736071110164 ) ) ;
#71838 = ORIENTED_EDGE ( 'NONE', *, *, #27831, .F. ) ;
#71839 = CARTESIAN_POINT ( 'NONE',  ( -0.8801773607110991993, 57.85535201082149825, -2.915334737309923874 ) ) ;
#71840 = ORIENTED_EDGE ( 'NONE', *, *, #48770, .T. ) ;
#71841 = CARTESIAN_POINT ( 'NONE',  ( 0.000000000000000000, 15.00000000000000000, 0.000000000000000000 ) ) ;
#71842 = CARTESIAN_POINT ( 'NONE',  ( 15.44008868035555793, 61.39701867748817676, -9.422509992056140149 ) ) ;
#71843 = VERTEX_POINT ( 'NONE', #50730 ) ;
#71844 = CARTESIAN_POINT ( 'NONE',  ( 20.88017736071110519, 60.56368534415484106, 2.639326808657452039E-16 ) ) ;
#71845 = SURFACE_STYLE_USAGE ( .BOTH. , #41857 ) ;
#71846 = DIRECTION ( 'NONE',  ( -0.000000000000000000, -1.000000000000000000, -0.000000000000000000 ) ) ;
#71847 = CARTESIAN_POINT ( 'NONE',  ( 0.000000000000000000, 15.00000000000000000, 0.000000000000000000 ) ) ;
#71848 = CARTESIAN_POINT ( 'NONE',  ( 2.917880565312948704, 67.63708216824730357, 12.26659068614894643 ) ) ;
#71849 = CARTESIAN_POINT ( 'NONE',  ( 1.472469842513823179, 6.425597817667451750, 4.923371831947296329 ) ) ;
#71850 = CARTESIAN_POINT ( 'NONE',  ( 10.00000000000000000, 5.553748834913967869, -14.16423886937410082 ) ) ;
#71851 = CARTESIAN_POINT ( 'NONE',  ( 14.92337183194729633, 7.675597817667451750, 8.527530157486181039 ) ) ;
#71852 = CARTESIAN_POINT ( 'NONE',  ( 10.00000000000000000, 11.81368534415483751, -10.88017736071110342 ) ) ;
#71853 = CARTESIAN_POINT ( 'NONE',  ( 14.92337183194729988, 44.34226448433412315, -8.527530157486177487 ) ) ;
#71854 = ORIENTED_EDGE ( 'NONE', *, *, #75076, .T. ) ;
#71855 = VECTOR ( 'NONE', #72290, 1000.000000000000000 ) ;
#71856 = CARTESIAN_POINT ( 'NONE',  ( 7.361572987183169658, 49.96726448433410894, -9.846743663894592657 ) ) ;
#71857 = ORIENTED_EDGE ( 'NONE', *, *, #62162, .T. ) ;
#71858 = CARTESIAN_POINT ( 'NONE',  ( -10.64017930668191170, 0.5000000000000004441, -10.57291749337230158 ) ) ;
#71859 = CARTESIAN_POINT ( 'NONE',  ( 20.88017736071110875, 50.77201867748817676, -2.915334737309920765 ) ) ;
#71860 = CARTESIAN_POINT ( 'NONE',  ( 0.1532563361054082862, 46.21726448433411605, 2.638427012816831674 ) ) ;
#71861 = FACE_OUTER_BOUND ( 'NONE', #29141, .T. ) ;
#71862 = CARTESIAN_POINT ( 'NONE',  ( 4.559911319644449179, 53.89701867748817676, 9.422509992056141925 ) ) ;
#71863 = CARTESIAN_POINT ( 'NONE',  ( 13.79529636645031943, 65.34541550158063217, -14.16423886937409904 ) ) ;
#71864 = AXIS2_PLACEMENT_3D ( 'NONE', #62993, #47498, #17021 ) ;
#71865 = EDGE_CURVE ( 'NONE', #29178, #28808, #74836, .T. ) ;
#71866 = CARTESIAN_POINT ( 'NONE',  ( 21.09922568453594849, 41.20696800326375353, 6.408140936763242479 ) ) ;
#71867 = DIRECTION ( 'NONE',  ( 0.000000000000000000, 0.000000000000000000, 1.000000000000000000 ) ) ;
#71868 = ORIENTED_EDGE ( 'NONE', *, *, #53039, .F. ) ;
#71869 = CARTESIAN_POINT ( 'NONE',  ( 16.40814093676323893, 25.79030133659708923, 11.09922568453595026 ) ) ;
#71870 = CARTESIAN_POINT ( 'NONE',  ( 20.88017736071110875, 35.77201867748816966, -2.915334737309920765 ) ) ;
#71871 = VERTEX_POINT ( 'NONE', #27718 ) ;
#71872 = CARTESIAN_POINT ( 'NONE',  ( -2.816281873526473856, -0.8763653300695799508, 9.499525473075851096E-16 ) ) ;
#71874 = CARTESIAN_POINT ( 'NONE',  ( 14.92337183194729633, 47.67559781766745175, 8.527530157486181039 ) ) ;
#71873 = CARTESIAN_POINT ( 'NONE',  ( 12.63842701281683034, 17.46726448433411250, 9.846743663894596210 ) ) ;
#71875 = CARTESIAN_POINT ( 'NONE',  ( -1.087200977609965147, 0.000000000000000000, 5.343763529286919223 ) ) ;
#71876 = CARTESIAN_POINT ( 'NONE',  ( 0.2751277870542910842, 52.28217586085238366, -6.499999999999992006 ) ) ;
#71877 = CARTESIAN_POINT ( 'NONE',  ( -13.14228782657336581, 14.49999999999999112, -7.230509711182429022 ) ) ;
#71879 = PRESENTATION_STYLE_ASSIGNMENT (( #48877 ) ) ;
#71878 = CARTESIAN_POINT ( 'NONE',  ( 0.1532563361054082862, 21.21726448433412315, 2.638427012816831674 ) ) ;
#71880 = CARTESIAN_POINT ( 'NONE',  ( -15.00000000000000000, 83.99999999999998579, -7.750000000000000000 ) ) ;
#71882 = ORIENTED_EDGE ( 'NONE', *, *, #86174, .T. ) ;
#71881 = CARTESIAN_POINT ( 'NONE',  ( 2.791683348922237240, 55.38393115100078745, -7.208316651077763204 ) ) ;
#71883 = CARTESIAN_POINT ( 'NONE',  ( 13.43411237798105340, 25.58196800326374998, 12.81628187352647963 ) ) ;
#71884 = CARTESIAN_POINT ( 'NONE',  ( 0.1532563361054083140, 41.00893115100078745, 1.131784320476157264E-15 ) ) ;
#71885 = CARTESIAN_POINT ( 'NONE',  ( -13.79463296483944923, 90.89544289844283753, 7.796684565667933775 ) ) ;
#71886 = CARTESIAN_POINT ( 'NONE',  ( 13.79529636645030344, 58.26208216824728936, 14.16423886937410614 ) ) ;
#71887 = CARTESIAN_POINT ( 'NONE',  ( 2.791683348922237240, 15.38393115100078212, -7.208316651077763204 ) ) ;
#71888 = CARTESIAN_POINT ( 'NONE',  ( 20.00000000000000711, 85.81090550035371223, 4.886738312952367380 ) ) ;
#71889 = CARTESIAN_POINT ( 'NONE',  ( 10.00000000000000178, 63.05374883491396076, 14.16423886937410082 ) ) ;
#71890 = CARTESIAN_POINT ( 'NONE',  ( 2.791683348922240793, 56.63393115100078035, 7.208316651077764092 ) ) ;
#71891 = CARTESIAN_POINT ( 'NONE',  ( 10.00000000000000178, 9.313685344154839285, 10.88017736071110342 ) ) ;
#71892 = CARTESIAN_POINT ( 'NONE',  ( -4.164238869374099039, 36.80374883491396787, 8.674139862899312516E-16 ) ) ;
#71894 = CARTESIAN_POINT ( 'NONE',  ( 18.52753015748618282, 33.92559781766745886, -4.923371831947291888 ) ) ;
#71893 = CARTESIAN_POINT ( 'NONE',  ( 17.08211943468705840, 35.13708216824730357, -12.26659068614894466 ) ) ;
#71895 = FACE_OUTER_BOUND ( 'NONE', #43329, .T. ) ;
#71897 = CARTESIAN_POINT ( 'NONE',  ( 12.63842701281683034, 57.46726448433411605, 9.846743663894596210 ) ) ;
#71896 = CARTESIAN_POINT ( 'NONE',  ( 6.933985542721516460, -73.15302115705439689, 2.749999999998391065 ) ) ;
#71898 = EDGE_LOOP ( 'NONE', ( #25726, #15928, #7470, #24843 ) ) ;
#71899 = CARTESIAN_POINT ( 'NONE',  ( 17.96484262340118221, 39.93868534415484106, 7.964842623401181321 ) ) ;
#71900 = CARTESIAN_POINT ( 'NONE',  ( 8.879999999999999005, -0.01540240839183078247, 3.750000000000000444 ) ) ;
#71901 = CARTESIAN_POINT ( 'NONE',  ( 5.076628168052703671, 46.84226448433412315, 8.527530157486179263 ) ) ;
#71902 = LINE ( 'NONE', #95398, #12316 ) ;
#71903 = CARTESIAN_POINT ( 'NONE',  ( -10.36894250292378317, 7.428748834913971422, 10.36894250292379560 ) ) ;
#71904 = CARTESIAN_POINT ( 'NONE',  ( 14.92337183194729633, 52.67559781766745175, 8.527530157486181039 ) ) ;
#71905 = CARTESIAN_POINT ( 'NONE',  ( -0.1503990784575407469, 12.22266099184918531, -6.262539305110056631 ) ) ;
#71906 = AXIS2_PLACEMENT_3D ( 'NONE', #79691, #10708, #94191 ) ;
#71907 = EDGE_CURVE ( 'NONE', #2489, #84641, #79758, .T. ) ;
#71908 = B_SPLINE_CURVE_WITH_KNOTS ( 'NONE', 3,
 ( #40597, #1132, #54101, #70106, #1631, #71094 ),
 .UNSPECIFIED., .F., .F.,
 ( 4, 2, 4 ),
 ( 0.0002800591277523079015, 0.0006862649357714276999, 0.001092470743790547498 ),
 .UNSPECIFIED. ) ;
#71909 = CARTESIAN_POINT ( 'NONE',  ( -0.3689425029237898834, 26.17874883491396432, -10.36894250292378850 ) ) ;
#71910 = EDGE_CURVE ( 'NONE', #93709, #52823, #27338, .T. ) ;
#71911 = EDGE_CURVE ( 'NONE', #98100, #35821, #64346, .T. ) ;
#71912 = CARTESIAN_POINT ( 'NONE',  ( -13.61464873478171533, 15.00000000000000000, 6.296136897217742501 ) ) ;
#71914 = CARTESIAN_POINT ( 'NONE',  ( 19.42250999205614548, 45.98035201082150536, -5.440088680355545492 ) ) ;
#71913 =( LENGTH_UNIT ( ) NAMED_UNIT ( * ) SI_UNIT ( .MILLI., .METRE. ) );
#71915 = CARTESIAN_POINT ( 'NONE',  ( 0.5774900079438590739, 22.64701867748817321, -5.440088680355550821 ) ) ;
#71916 = CARTESIAN_POINT ( 'NONE',  ( 6.565887622018943937, 28.08196800326375353, -12.81628187352647608 ) ) ;
#71917 = CARTESIAN_POINT ( 'NONE',  ( 10.84451454130507209, 15.00000000000000000, -9.625305416630832056 ) ) ;
#71918 = CARTESIAN_POINT ( 'NONE',  ( 12.63842701281683034, 17.46726448433411250, 9.846743663894596210 ) ) ;
#71919 = CIRCLE ( 'NONE', #24049, 0.5000000000000004441 ) ;
#71920 = CARTESIAN_POINT ( 'NONE',  ( 6.284516029235898138, -36.06297093898795936, -4.000000000000000000 ) ) ;
#71921 = VECTOR ( 'NONE', #71472, 1000.000000000000000 ) ;
#71922 = DIRECTION ( 'NONE',  ( 1.000000000000000000, 0.000000000000000000, 0.000000000000000000 ) ) ;
#71923 = CARTESIAN_POINT ( 'NONE',  ( -4.787136363774558312, -17.54594992866426395, 4.000000000000000888 ) ) ;
#71924 = CARTESIAN_POINT ( 'NONE',  ( 0.5774900079438607392, 3.480352010821504916, 5.440088680355550821 ) ) ;
#71925 = CARTESIAN_POINT ( 'NONE',  ( 0.2751277870542912507, 20.30223176428831167, 6.499999999999992006 ) ) ;
#71926 = FACE_OUTER_BOUND ( 'NONE', #84775, .T. ) ;
#71927 = CARTESIAN_POINT ( 'NONE',  ( 0.5774900079438607392, 38.48035201082150536, 5.440088680355550821 ) ) ;
#71928 = CARTESIAN_POINT ( 'NONE',  ( 17.96484262340118221, 41.18868534415484106, -7.964842623401177768 ) ) ;
#71929 = CARTESIAN_POINT ( 'NONE',  ( -2.816281873526473856, 4.331968003263754419, 3.434112377981055619 ) ) ;
#71930 = CARTESIAN_POINT ( 'NONE',  ( 8.629999999999995453, 41.24999999999999289, 6.500000000000000888 ) ) ;
#71931 = CARTESIAN_POINT ( 'NONE',  ( -0.1503990784575328643, 70.00000000000000000, -6.262539305110068177 ) ) ;
#71932 = CARTESIAN_POINT ( 'NONE',  ( 12.63842701281683922, 4.550597817667451750, -9.846743663894590881 ) ) ;
#71933 = EDGE_CURVE ( 'NONE', #44443, #94977, #87727, .T. ) ;
#71935 = EDGE_LOOP ( 'NONE', ( #36957, #95589, #90708, #22258, #55313, #80501 ) ) ;
#71934 = VECTOR ( 'NONE', #5717, 1000.000000000000000 ) ;
#71936 = CARTESIAN_POINT ( 'NONE',  ( 7.084665262690076126, 47.02201867748818387, -10.88017736071110164 ) ) ;
#71937 = CARTESIAN_POINT ( 'NONE',  ( 0.6178305044545818747, 3.498634669930420049, -9.382169495545419124 ) ) ;
#71938 = CARTESIAN_POINT ( 'NONE',  ( 10.00000000000000000, 56.81368534415484106, -10.88017736071110342 ) ) ;
#71939 = CARTESIAN_POINT ( 'NONE',  ( 7.361572987183169658, 9.967264484334119601, -9.846743663894592657 ) ) ;
#71940 = CARTESIAN_POINT ( 'NONE',  ( -1.099225684535947600, 28.70696800326375353, -6.408140936763238038 ) ) ;
#71942 = DIRECTION ( 'NONE',  ( 0.000000000000000000, 0.000000000000000000, 1.000000000000000000 ) ) ;
#71941 = CARTESIAN_POINT ( 'NONE',  ( 17.20831665107776587, 7.883931151000784787, 7.208316651077764980 ) ) ;
#71943 = VERTEX_POINT ( 'NONE', #67209 ) ;
#71944 = CARTESIAN_POINT ( 'NONE',  ( 0.000000000000000000, 15.00000000000000000, 0.000000000000000000 ) ) ;
#71945 = CARTESIAN_POINT ( 'NONE',  ( 17.96484262340118221, 4.938685344154837509, 7.964842623401181321 ) ) ;
#71946 = CYLINDRICAL_SURFACE ( 'NONE', #24960, 0.5000000000000004441 ) ;
#71947 = EDGE_CURVE ( 'NONE', #6107, #52027, #44506, .T. ) ;
#71948 = CARTESIAN_POINT ( 'NONE',  ( 17.20831665107776587, 17.88393115100078745, 7.208316651077764980 ) ) ;
#71949 = CARTESIAN_POINT ( 'NONE',  ( 19.42250999205614548, 10.98035201082150358, -5.440088680355545492 ) ) ;
#71950 = AXIS2_PLACEMENT_3D ( 'NONE', #70089, #78075, #639 ) ;
#71951 = CARTESIAN_POINT ( 'NONE',  ( 7.084665262690076126, 7.022018677488170546, -10.88017736071110164 ) ) ;
#71952 = VERTEX_POINT ( 'NONE', #13213 ) ;
#71953 = AXIS2_PLACEMENT_3D ( 'NONE', #1603, #40071, #98637 ) ;
#71954 = CARTESIAN_POINT ( 'NONE',  ( 17.96484262340118221, 14.93868534415483751, 7.964842623401181321 ) ) ;
#71955 = CARTESIAN_POINT ( 'NONE',  ( 20.88017736071110875, 20.77201867748816611, -2.915334737309920765 ) ) ;
#71956 = FACE_OUTER_BOUND ( 'NONE', #39560, .T. ) ;
#71957 = ORIENTED_EDGE ( 'NONE', *, *, #8714, .F. ) ;
#71958 = CARTESIAN_POINT ( 'NONE',  ( 13.14228782657338535, 0.3639308284105124969, 7.230509711182335764 ) ) ;
#71959 = CARTESIAN_POINT ( 'NONE',  ( 0.5774900079438590739, 27.64701867748817676, -5.440088680355550821 ) ) ;
#71960 = CARTESIAN_POINT ( 'NONE',  ( 2.791683348922240793, 56.63393115100078035, 7.208316651077764092 ) ) ;
#71961 = CARTESIAN_POINT ( 'NONE',  ( -8.470897558477686218, 15.00000000000000888, 11.92401951126073278 ) ) ;
#71962 = CARTESIAN_POINT ( 'NONE',  ( 19.38216949554541557, 47.24863466993041783, -9.382169495545420901 ) ) ;
#71963 = DIRECTION ( 'NONE',  ( -0.000000000000000000, -0.000000000000000000, 1.000000000000000000 ) ) ;
#71964 = CARTESIAN_POINT ( 'NONE',  ( 17.08211943468705130, 28.47041550158063572, 12.26659068614894998 ) ) ;
#71965 = CARTESIAN_POINT ( 'NONE',  ( 19.42250999205614548, 35.98035201082151247, -5.440088680355545492 ) ) ;
#71966 = CARTESIAN_POINT ( 'NONE',  ( 7.084665262690076126, 14.10535201082150358, 10.88017736071109987 ) ) ;
#71967 = CARTESIAN_POINT ( 'NONE',  ( 14.92337183194729988, 59.34226448433412315, -8.527530157486177487 ) ) ;
#71968 = LINE ( 'NONE', #3012, #57207 ) ;
#71969 = CARTESIAN_POINT ( 'NONE',  ( 1.472469842513823179, 30.59226448433411960, -4.923371831947296329 ) ) ;
#71970 = DIRECTION ( 'NONE',  ( 0.9426414910921736556, 0.000000000000000000, 0.3338068592337842255 ) ) ;
#71971 = CARTESIAN_POINT ( 'NONE',  ( 5.076628168052703671, 11.84226448433411960, 8.527530157486179263 ) ) ;
#71972 = CARTESIAN_POINT ( 'NONE',  ( 3.434112377981054287, -37.33469866340291077, -12.81628187352647608 ) ) ;
#71973 = VERTEX_POINT ( 'NONE', #52204 ) ;
#71974 = CARTESIAN_POINT ( 'NONE',  ( -0.8801773607111008646, 8.272018677488171434, 2.915334737309923430 ) ) ;
#71975 = CARTESIAN_POINT ( 'NONE',  ( 7.361572987183170547, 12.05059781766744997, 9.846743663894590881 ) ) ;
#71976 = CARTESIAN_POINT ( 'NONE',  ( 20.88017736071110164, 40.35535201082150536, 2.915334737309930979 ) ) ;
#71978 = CARTESIAN_POINT ( 'NONE',  ( 10.00000000000000178, 40.37363466993042493, 12.81628187352647608 ) ) ;
#71977 = CARTESIAN_POINT ( 'NONE',  ( -0.8801773607111008646, 23.27201867748817676, 2.915334737309923430 ) ) ;
#71979 = CARTESIAN_POINT ( 'NONE',  ( -0.3689425029237881626, 37.42874883491396787, 10.36894250292379027 ) ) ;
#71980 = CARTESIAN_POINT ( 'NONE',  ( -2.962741594152892510, 15.00000000000000000, -13.93860331045676837 ) ) ;
#71981 = AXIS2_PLACEMENT_3D ( 'NONE', #63647, #18663, #49151 ) ;
#71982 = CARTESIAN_POINT ( 'NONE',  ( -2.816281873526473856, 64.33196800326376774, 3.434112377981055619 ) ) ;
#71983 = ORIENTED_EDGE ( 'NONE', *, *, #25103, .F. ) ;
#71984 = CARTESIAN_POINT ( 'NONE',  ( 14.92337183194729633, 57.67559781766745886, 8.527530157486181039 ) ) ;
#71985 = CYLINDRICAL_SURFACE ( 'NONE', #40984, 0.2500000000000002220 ) ;
#71986 = CARTESIAN_POINT ( 'NONE',  ( -0.8801773607110991993, 27.85535201082150181, -2.915334737309923874 ) ) ;
#71987 = TOROIDAL_SURFACE ( 'NONE', #87971, 14.49999999999999822, 0.5000000000000000000 ) ;
#71988 = VERTEX_POINT ( 'NONE', #29683 ) ;
#71989 = CARTESIAN_POINT ( 'NONE',  ( 2.791683348922237240, 5.383931151000785675, -7.208316651077763204 ) ) ;
#71990 = CARTESIAN_POINT ( 'NONE',  ( 18.52753015748618282, 13.92559781766745175, -4.923371831947291888 ) ) ;
#71991 = CARTESIAN_POINT ( 'NONE',  ( 19.84674366389459266, 18.71726448433411960, -2.638427012816827677 ) ) ;
#71992 = CARTESIAN_POINT ( 'NONE',  ( 0.1532563361054082862, 16.21726448433411960, 2.638427012816831674 ) ) ;
#71993 = FACE_OUTER_BOUND ( 'NONE', #39486, .T. ) ;
#71994 = EDGE_CURVE ( 'NONE', #92979, #11604, #74913, .T. ) ;
#71995 = CARTESIAN_POINT ( 'NONE',  ( -0.8801773607111008646, 63.27201867748817676, 2.915334737309923430 ) ) ;
#71996 = CARTESIAN_POINT ( 'NONE',  ( 4.559911319644449179, 67.23035201082150536, -9.422509992056141925 ) ) ;
#71998 = VERTEX_POINT ( 'NONE', #6704 ) ;
#71997 = CARTESIAN_POINT ( 'NONE',  ( 14.92337183194729988, 14.34226448433411782, -8.527530157486177487 ) ) ;
#71999 = CARTESIAN_POINT ( 'NONE',  ( -3.699999999999999289, 0.2999999999999982125, 4.531193156845205215E-16 ) ) ;
#72000 = CARTESIAN_POINT ( 'NONE',  ( 5.076628168052703671, 51.84226448433412315, 8.527530157486179263 ) ) ;
#72001 = EDGE_LOOP ( 'NONE', ( #75825, #53579, #60772, #92246 ) ) ;
#72002 = CARTESIAN_POINT ( 'NONE',  ( -12.11331110855146953, 14.95077488074853456, 8.421032842869358603 ) ) ;
#72003 = CARTESIAN_POINT ( 'NONE',  ( -4.164238869374099039, 11.80374883491396965, 8.674139862899312516E-16 ) ) ;
#72004 = B_SPLINE_CURVE_WITH_KNOTS ( 'NONE', 3,
 ( #90749, #51774, #45253, #52751, #97798, #29260 ),
 .UNSPECIFIED., .F., .F.,
 ( 4, 2, 4 ),
 ( 0.0002800452451363289125, 0.0006862509172491817848, 0.001092456589362034549 ),
 .UNSPECIFIED. ) ;
#72005 = CARTESIAN_POINT ( 'NONE',  ( -45.94000000000001194, 99.99999999999998579, -9.500000000000000000 ) ) ;
#72006 = CARTESIAN_POINT ( 'NONE',  ( -2.266590686148945544, 12.22041550158063394, 7.082119434687048631 ) ) ;
#72007 = CARTESIAN_POINT ( 'NONE',  ( 24.16423886937410614, 34.51208216824731068, -3.795296366450302550 ) ) ;
#72008 = CARTESIAN_POINT ( 'NONE',  ( 20.88017736071110164, 30.35535201082151247, 2.915334737309930979 ) ) ;
#72009 = CARTESIAN_POINT ( 'NONE',  ( 8.879999999999991900, 69.99999999999998579, 6.396446609406726935 ) ) ;
#72010 = ORIENTED_EDGE ( 'NONE', *, *, #11212, .F. ) ;
#72011 = CARTESIAN_POINT ( 'NONE',  ( 12.63842701281683034, 17.46726448433411250, 9.846743663894596210 ) ) ;
#72012 = EDGE_CURVE ( 'NONE', #73005, #80852, #51249, .T. ) ;
#72014 = CARTESIAN_POINT ( 'NONE',  ( 12.63842701281683034, 17.46726448433411250, 9.846743663894596210 ) ) ;
#72013 = CARTESIAN_POINT ( 'NONE',  ( 10.00000000000000000, 51.81368534415484106, -10.88017736071110342 ) ) ;
#72015 = AXIS2_PLACEMENT_3D ( 'NONE', #62810, #63778, #94288 ) ;
#72016 = AXIS2_PLACEMENT_3D ( 'NONE', #17809, #25326, #49279 ) ;
#72017 = CARTESIAN_POINT ( 'NONE',  ( 16.40814093676323893, 45.79030133659708923, 11.09922568453595026 ) ) ;
#72018 = CARTESIAN_POINT ( 'NONE',  ( 18.52753015748617571, 33.09226448433411605, 4.923371831947298993 ) ) ;
#72019 = CARTESIAN_POINT ( 'NONE',  ( 17.39651004071841811, 4.082109641433293135, -6.499999999999999112 ) ) ;
#72020 = CARTESIAN_POINT ( 'NONE',  ( 17.96484262340118221, 61.18868534415482685, -7.964842623401177768 ) ) ;
#72021 = CARTESIAN_POINT ( 'NONE',  ( -2.816281873526473856, 29.33196800326376064, 3.434112377981055619 ) ) ;
#72022 = CARTESIAN_POINT ( 'NONE',  ( -10.36894250292378317, -32.57125116508603213, 10.36894250292379560 ) ) ;
#72023 = CARTESIAN_POINT ( 'NONE',  ( 10.00000000000000000, 19.75893115100078390, -9.846743663894594434 ) ) ;
#72024 = EDGE_CURVE ( 'NONE', #1780, #11601, #28588, .T. ) ;
#72025 = PRESENTATION_LAYER_ASSIGNMENT (  '', '', ( #46481 ) ) ;
#72026 = CARTESIAN_POINT ( 'NONE',  ( 17.08211943468705840, 10.13708216824730179, -12.26659068614894466 ) ) ;
#72027 = EDGE_LOOP ( 'NONE', ( #86540, #3409, #94445, #72823 ) ) ;
#72028 = EDGE_CURVE ( 'NONE', #13314, #47944, #81000, .T. ) ;
#72029 = CARTESIAN_POINT ( 'NONE',  ( 20.88017736071110519, 40.56368534415484106, 2.639326808657452039E-16 ) ) ;
#72030 = CARTESIAN_POINT ( 'NONE',  ( 15.44008868035555793, 51.39701867748816966, -9.422509992056140149 ) ) ;
#72031 = CARTESIAN_POINT ( 'NONE',  ( 13.79529636645030344, 43.26208216824730357, 14.16423886937410614 ) ) ;
#72032 = CARTESIAN_POINT ( 'NONE',  ( 14.92337183194729633, 52.67559781766745175, 8.527530157486181039 ) ) ;
#72033 = CARTESIAN_POINT ( 'NONE',  ( 19.84674366389459266, 8.300597817667451750, 2.638427012816836559 ) ) ;
#72035 = CARTESIAN_POINT ( 'NONE',  ( -13.34727560011345027, 90.86036091889431532, 7.765078796629374835 ) ) ;
#72034 = DIRECTION ( 'NONE',  ( 0.000000000000000000, 1.000000000000000000, 0.000000000000000000 ) ) ;
#72036 = CARTESIAN_POINT ( 'NONE',  ( 12.91533473730993009, 36.60535201082151247, -10.88017736071109987 ) ) ;
#72037 = CYLINDRICAL_SURFACE ( 'NONE', #27861, 19.43999999999999773 ) ;
#72038 = CARTESIAN_POINT ( 'NONE',  ( 21.09922568453594849, 21.20696800326375353, 6.408140936763242479 ) ) ;
#72039 = CARTESIAN_POINT ( 'NONE',  ( 7.361572987183169658, 49.96726448433410894, -9.846743663894592657 ) ) ;
#72040 = CARTESIAN_POINT ( 'NONE',  ( -2.915334737309934532, 12.02201867748817499, -10.88017736071109987 ) ) ;
#72041 =( BOUNDED_SURFACE ( )  B_SPLINE_SURFACE ( 1, 2, ( 
 ( #45366, #75870, #21897, #76365, #74878, #82373, #60860, #53358, #28873, #52374, #97910, #68873, #28396, #97406, #7391, #43876, #21397, #59375, #51891, #22886, #14394, #67884, #37889, #52867, #60364, #75368, #13895, #44865, #7879, #20905, #38372, #29370, #98901, #6883, #44380, #30353, #29861, #6378, #98406, #5899, #37396, #90860, #90359, #22391, #36893, #83373, #83865, #67381, #15389, #51394, #58890, #81881, #74372, #36394, #92835, #17831, #46839, #54337, #32813, #25350, #880, #24363, #69854, #40830, #403, #38868, #78321, #84374, #92347, #31340, #69359, #63309, #54826, #39842, #85837, #24848, #32324, #47326, #61840, #85338, #48313, #61352, #78821, #1377, #9841, #16851, #23873, #2358, #1866, #84851, #70348, #76846, #77825, #9340, #31831, #62327, #16358, #55330, #17351, #77334, #62827, #91861, #47821, #10331, #93327, #40342, #23379, #70845, #8360, #93819, #8846, #55833, #39360, #86327, #30855, #53863, #15873, #46358, #88285, #79800, #34274, #33780, #50785, #64775, #4309, #12776, #95291, #63796, #72772, #18816, #27776, #20287, #49786, #41340, #80789, #94799, #71811, #3317, #27280, #26793, #34783, #33304, #80294, #49298, #81276, #73278, #65271, #56325, #57290, #95799, #57778, #11792, #25827, #42793, #86820, #19784, #64287, #4800, #42300, #50272, #12286, #10820, #35276, #87784, #19300, #65771, #18323, #48804, #41822, #96300, #58261, #56801, #88776, #79313, #26301, #87297, #11302, #72288, #3819, #74253, #22276, #67268, #52748, #37772, #66263, #91241, #97292, #66769, #83257, #14780, #36776, #60739, #89759, #59258, #75748, #68268, #43764, #97796, #13772, #83751, #43273, #21276, #7270, #28273, #51772, #29258, #90250, #98787, #21782, #82756, #29744, #30235, #22765, #52261, #14279, #44752, #73768, #96798, #58768, #89272, #20783, #51274, #76732, #47711, #16734, #84258, #85231, #91744, #62212, #1260, #8727, #39245, #15761, #70229, #32203, #53740, #69735, #7766, #62704, #63195, #47211, #1748, #38261, #77712, #23264, #31716, #92233, #92717, #46247, #69249, #78206, #38748, #770, #85720, #93204, #23759, #24243, #31222, #55715, #54709, #9224, #15274, #9718, #68752, #40217, #61718, #2241, #284, #32699, #54222, #30731, #84737, #61237, #18209, #42191, #41704, #80170, #10219, #87666, #94688, #17722, #4688, #4190, #63683, #79686, #34660, #65156, #25716, #49184, #72174, #3703, #34163, #51156, #60123, #29132, #67141, #75132, #96675, #90621, #21155, #82135, #21657, #20161, #68142, #28644, #36655, #51656, #43647, #45122, #50664, #97666, #5667, #58144, #22145, #52141, #43157, #13644, #59636, #82637, #90127, #37645, #29617, #88653, #6637, #81640 ),
 ( #59135, #98161, #36149, #66653, #13148, #14657, #14154, #97177, #12657, #28154, #58650, #75629, #73643, #89643, #7141, #37155, #66142, #35657, #44129, #74639, #67651, #89149, #6150, #44638, #52629, #74131, #20660, #83132, #81153, #5172, #48939, #79447, #62957, #17965, #10947, #71468, #41472, #93463, #25954, #30115, #77465, #92959, #48452, #84976, #24989, #9973, #70975, #2982, #33430, #71939, #63453, #47950, #62457, #70476, #31955, #55471, #60621, #1508, #85974, #1996, #63927, #16494, #9472, #25483, #69983, #40478, #91122, #55968, #78950, #56457, #24493, #39975, #86943, #94442, #85477, #2496, #17484, #39492, #32462, #22645, #53125, #78460, #93958, #18456, #46971, #16986, #40971, #8976, #47464, #86468, #10461, #11932, #20919, #28410, #80434, #72919, #95936, #80924, #50911, #27906, #34914, #19922, #13406, #65411, #64909, #81895, #27418, #35412, #43891, #57911, #94931, #4932, #49923, #58905, #51408, #12417, #72420, #12909, #26928, #3946, #34419, #58399, #88422, #65904, #64424, #42924, #42437, #3462, #5435, #96436, #87433, #50415, #88917, #20424, #73404, #33917, #73904, #26434, #81407, #95434, #35907, #43406, #66404, #96935, #41956, #89403, #56932, #18949, #49426, #79930, #11437, #4449, #57426, #87919, #19436, #61367, #98423, #53372, #68891, #66902, #23399, #29384, #6391, #91374, #22900, #67899, #91877, #21915, #59885, #7894, #419, #74892, #29877, #44880, #15889, #74391, #13915, #83882, #59391, #67398, #36906, #44393, #38388, #60379, #14908, #60874, #98915, #7409, #22405, #97924, #90877, #53883, #36408, #84390, #75382, #15409, #52880, #90376, #76379, #75886, #52393, #45380, #51906, #83390, #37905, #6898, #37412, #82893, #30370, #45892, #14409, #68394, #97421, #30870, #5915, #28887, #89893, #21411, #82391, #23890, #39861, #24378, #9356, #54355, #1392, #78838, #16376, #84867, #86346, #63334, #54843, #8862, #85358, #77847, #70367, #93839, #24869, #31847, #46857, #46374, #16870, #71352, #1885, #47344, #78341, #32343, #40361, #93345, #25846, #38886, #62845, #17849, #92850, #55351, #39378, #2871, #17369, #85857, #897, #77351, #69872, #33320, #31359, #47838, #63815, #25365, #62344, #9862, #70862, #2377, #55851, #32832, #48334, #10349, #40849, #94325, #56344, #86838, #76863, #8378, #69375, #61859, #92363, #4821, #35796, #58281, #66283, #49804, #12792, #18343, #64307, #79819, #35295, #71829, #80312, #95819, #57800, #88799, #20308, #96818, #50295, #34802, #49315, #57308, #18835, #11812, #28295, #87318, #42320, #87800, #50807, #3338, #64793, #12306, #56820, #27299, #48822, #42813, #65788, #43292, #11321, #95312, #73787, #81296, #41840 ) ),
 .UNSPECIFIED., .F., .F., .F. ) 
 B_SPLINE_SURFACE_WITH_KNOTS ( ( 2, 2 ),
 ( 3, 2, 2, 2, 2, 2, 2, 2, 2, 2, 2, 2, 2, 2, 2, 2, 2, 2, 2, 2, 2, 2, 2, 2, 2, 2, 2, 2, 2, 2, 2, 2, 2, 2, 2, 2, 2, 2, 2, 2, 2, 2, 2, 2, 2, 2, 2, 2, 2, 2, 2, 2, 2, 2, 2, 2, 2, 2, 2, 2, 2, 2, 2, 2, 2, 2, 2, 2, 2, 2, 2, 2, 2, 2, 2, 2, 2, 2, 2, 2, 2, 2, 2, 2, 2, 2, 2, 2, 2, 2, 2, 2, 2, 2, 2, 2, 2, 2, 2, 2, 2, 2, 2, 2, 2, 2, 2, 2, 2, 2, 2, 2, 2, 2, 2, 2, 2, 2, 2, 2, 2, 2, 2, 2, 2, 2, 2, 2, 2, 2, 2, 2, 2, 2, 2, 2, 2, 2, 2, 2, 2, 2, 2, 2, 2, 2, 2, 2, 2, 2, 2, 2, 2, 2, 2, 2, 2, 2, 2, 2, 2, 2, 3 ),
 ( 0.000000000000000000, 1.000000000000000000 ),
 ( 0.000000000000000000, 0.005952380952380952051, 0.01190476190476190410, 0.01785714285714285615, 0.02380952380952380820, 0.02976190476190476025, 0.03571428571428571230, 0.04166666666666666435, 0.04761904761904761640, 0.05357142857142856845, 0.05952380952380952051, 0.06547619047619047949, 0.07142857142857142461, 0.07738095238095238360, 0.08333333333333332871, 0.08928571428571428770, 0.09523809523809523281, 0.1011904761904761918, 0.1071428571428571369, 0.1130952380952380959, 0.1190476190476190410, 0.1250000000000000000, 0.1309523809523809590, 0.1369047619047619180, 0.1428571428571428492, 0.1488095238095238082, 0.1547619047619047672, 0.1607142857142857262, 0.1666666666666666574, 0.1726190476190476164, 0.1785714285714285754, 0.1845238095238095344, 0.1904761904761904656, 0.1964285714285714246, 0.2023809523809523836, 0.2083333333333333426, 0.2142857142857142738, 0.2202380952380952328, 0.2261904761904761918, 0.2321428571428571508, 0.2380952380952380820, 0.2440476190476190410, 0.2500000000000000000, 0.2559523809523809312, 0.2619047619047619180, 0.2678571428571428492, 0.2738095238095238360, 0.2797619047619047672, 0.2857142857142856984, 0.2916666666666666852, 0.2976190476190476164, 0.3035714285714285476, 0.3095238095238095344, 0.3154761904761904656, 0.3214285714285714524, 0.3273809523809523836, 0.3333333333333333148, 0.3392857142857143016, 0.3452380952380952328, 0.3511904761904761640, 0.3571428571428571508, 0.3630952380952380820, 0.3690476190476190688, 0.3750000000000000000, 0.3809523809523809312, 0.3869047619047619180, 0.3928571428571428492, 0.3988095238095238360, 0.4047619047619047672, 0.4107142857142856984, 0.4166666666666666852, 0.4226190476190476164, 0.4285714285714285476, 0.4345238095238095344, 0.4404761904761904656, 0.4464285714285714524, 0.4523809523809523836, 0.4583333333333333148, 0.4642857142857143016, 0.4702380952380952328, 0.4761904761904761640, 0.4821428571428571508, 0.4880952380952380820, 0.4940476190476190688, 0.5000000000000000000, 0.5059523809523809312, 0.5119047619047618625, 0.5178571428571429047, 0.5238095238095238360, 0.5297619047619047672, 0.5357142857142856984, 0.5416666666666666297, 0.5476190476190476719, 0.5535714285714286031, 0.5595238095238095344, 0.5654761904761904656, 0.5714285714285713969, 0.5773809523809523281, 0.5833333333333333703, 0.5892857142857143016, 0.5952380952380952328, 0.6011904761904761640, 0.6071428571428570953, 0.6130952380952381375, 0.6190476190476190688, 0.6250000000000000000, 0.6309523809523809312, 0.6369047619047618625, 0.6428571428571429047, 0.6488095238095238360, 0.6547619047619047672, 0.6607142857142856984, 0.6666666666666666297, 0.6726190476190476719, 0.6785714285714286031, 0.6845238095238095344, 0.6904761904761904656, 0.6964285714285713969, 0.7023809523809523281, 0.7083333333333333703, 0.7142857142857143016, 0.7202380952380952328, 0.7261904761904761640, 0.7321428571428570953, 0.7380952380952381375, 0.7440476190476190688, 0.7500000000000000000, 0.7559523809523809312, 0.7619047619047618625, 0.7678571428571429047, 0.7738095238095238360, 0.7797619047619047672, 0.7857142857142856984, 0.7916666666666666297, 0.7976190476190476719, 0.8035714285714286031, 0.8095238095238095344, 0.8154761904761904656, 0.8214285714285713969, 0.8273809523809523281, 0.8333333333333333703, 0.8392857142857143016, 0.8452380952380952328, 0.8511904761904761640, 0.8571428571428570953, 0.8630952380952381375, 0.8690476190476190688, 0.8750000000000000000, 0.8809523809523809312, 0.8869047619047618625, 0.8928571428571429047, 0.8988095238095238360, 0.9047619047619047672, 0.9107142857142856984, 0.9166666666666666297, 0.9226190476190476719, 0.9285714285714286031, 0.9345238095238095344, 0.9404761904761904656, 0.9464285714285713969, 0.9523809523809523281, 0.9583333333333333703, 0.9642857142857143016 ),
 .UNSPECIFIED. ) 
 GEOMETRIC_REPRESENTATION_ITEM ( )  RATIONAL_B_SPLINE_SURFACE ( (
 ( 1.000000000000000000, 0.9659258262890683122, 1.000000000000000000, 0.9659258262890683122, 1.000000000000000000, 0.9659258262890683122, 1.000000000000000000, 0.9659258262890683122, 1.000000000000000000, 0.9659258262890683122, 1.000000000000000000, 0.9659258262890683122, 1.000000000000000000, 0.9659258262890683122, 1.000000000000000000, 0.9659258262890683122, 1.000000000000000000, 0.9659258262890683122, 1.000000000000000000, 0.9659258262890683122, 1.000000000000000000, 0.9659258262890683122, 1.000000000000000000, 0.9659258262890683122, 1.000000000000000000, 0.9659258262890683122, 1.000000000000000000, 0.9659258262890683122, 1.000000000000000000, 0.9659258262890683122, 1.000000000000000000, 0.9659258262890683122, 1.000000000000000000, 0.9659258262890683122, 1.000000000000000000, 0.9659258262890683122, 1.000000000000000000, 0.9659258262890683122, 1.000000000000000000, 0.9659258262890683122, 1.000000000000000000, 0.9659258262890683122, 1.000000000000000000, 0.9659258262890683122, 1.000000000000000000, 0.9659258262890683122, 1.000000000000000000, 0.9659258262890683122, 1.000000000000000000, 0.9659258262890683122, 1.000000000000000000, 0.9659258262890683122, 1.000000000000000000, 0.9659258262890683122, 1.000000000000000000, 0.9659258262890683122, 1.000000000000000000, 0.9659258262890683122, 1.000000000000000000, 0.9659258262890683122, 1.000000000000000000, 0.9659258262890683122, 1.000000000000000000, 0.9659258262890683122, 1.000000000000000000, 0.9659258262890683122, 1.000000000000000000, 0.9659258262890683122, 1.000000000000000000, 0.9659258262890683122, 1.000000000000000000, 0.9659258262890683122, 1.000000000000000000, 0.9659258262890683122, 1.000000000000000000, 0.9659258262890683122, 1.000000000000000000, 0.9659258262890683122, 1.000000000000000000, 0.9659258262890683122, 1.000000000000000000, 0.9659258262890683122, 1.000000000000000000, 0.9659258262890683122, 1.000000000000000000, 0.9659258262890683122, 1.000000000000000000, 0.9659258262890683122, 1.000000000000000000, 0.9659258262890683122, 1.000000000000000000, 0.9659258262890683122, 1.000000000000000000, 0.9659258262890683122, 1.000000000000000000, 0.9659258262890683122, 1.000000000000000000, 0.9659258262890683122, 1.000000000000000000, 0.9659258262890683122, 1.000000000000000000, 0.9659258262890683122, 1.000000000000000000, 0.9659258262890683122, 1.000000000000000000, 0.9659258262890683122, 1.000000000000000000, 0.9659258262890683122, 1.000000000000000000, 0.9659258262890683122, 1.000000000000000000, 0.9659258262890683122, 1.000000000000000000, 0.9659258262890683122, 1.000000000000000000, 0.9659258262890683122, 1.000000000000000000, 0.9659258262890683122, 1.000000000000000000, 0.9659258262890683122, 1.000000000000000000, 0.9659258262890683122, 1.000000000000000000, 0.9659258262890683122, 1.000000000000000000, 0.9659258262890683122, 1.000000000000000000, 0.9659258262890683122, 1.000000000000000000, 0.9659258262890683122, 1.000000000000000000, 0.9659258262890683122, 1.000000000000000000, 0.9659258262890683122, 1.000000000000000000, 0.9659258262890683122, 1.000000000000000000, 0.9659258262890683122, 1.000000000000000000, 0.9659258262890683122, 1.000000000000000000, 0.9659258262890683122, 1.000000000000000000, 0.9659258262890683122, 1.000000000000000000, 0.9659258262890683122, 1.000000000000000000, 0.9659258262890683122, 1.000000000000000000, 0.9659258262890683122, 1.000000000000000000, 0.9659258262890683122, 1.000000000000000000, 0.9659258262890683122, 1.000000000000000000, 0.9659258262890683122, 1.000000000000000000, 0.9659258262890683122, 1.000000000000000000, 0.9659258262890683122, 1.000000000000000000, 0.9659258262890683122, 1.000000000000000000, 0.9659258262890683122, 1.000000000000000000, 0.9659258262890683122, 1.000000000000000000, 0.9659258262890683122, 1.000000000000000000, 0.9659258262890683122, 1.000000000000000000, 0.9659258262890683122, 1.000000000000000000, 0.9659258262890683122, 1.000000000000000000, 0.9659258262890683122, 1.000000000000000000, 0.9659258262890683122, 1.000000000000000000, 0.9659258262890683122, 1.000000000000000000, 0.9659258262890683122, 1.000000000000000000, 0.9659258262890683122, 1.000000000000000000, 0.9659258262890683122, 1.000000000000000000, 0.9659258262890683122, 1.000000000000000000, 0.9659258262890683122, 1.000000000000000000, 0.9659258262890683122, 1.000000000000000000, 0.9659258262890683122, 1.000000000000000000, 0.9659258262890683122, 1.000000000000000000, 0.9659258262890683122, 1.000000000000000000, 0.9659258262890683122, 1.000000000000000000, 0.9659258262890683122, 1.000000000000000000, 0.9659258262890683122, 1.000000000000000000, 0.9659258262890683122, 1.000000000000000000, 0.9659258262890683122, 1.000000000000000000, 0.9659258262890683122, 1.000000000000000000, 0.9659258262890683122, 1.000000000000000000, 0.9659258262890683122, 1.000000000000000000, 0.9659258262890683122, 1.000000000000000000, 0.9659258262890683122, 1.000000000000000000, 0.9659258262890683122, 1.000000000000000000, 0.9659258262890683122, 1.000000000000000000, 0.9659258262890683122, 1.000000000000000000, 0.9659258262890683122, 1.000000000000000000, 0.9659258262890683122, 1.000000000000000000, 0.9659258262890683122, 1.000000000000000000, 0.9659258262890683122, 1.000000000000000000, 0.9659258262890683122, 1.000000000000000000, 0.9659258262890683122, 1.000000000000000000, 0.9659258262890683122, 1.000000000000000000, 0.9659258262890683122, 1.000000000000000000, 0.9659258262890683122, 1.000000000000000000, 0.9659258262890683122, 1.000000000000000000, 0.9659258262890683122, 1.000000000000000000, 0.9659258262890683122, 1.000000000000000000, 0.9659258262890683122, 1.000000000000000000, 0.9659258262890683122, 1.000000000000000000, 0.9659258262890683122, 1.000000000000000000, 0.9659258262890683122, 1.000000000000000000, 0.9659258262890683122, 1.000000000000000000, 0.9659258262890683122, 1.000000000000000000, 0.9659258262890683122, 1.000000000000000000, 0.9659258262890683122, 1.000000000000000000, 0.9659258262890683122, 1.000000000000000000, 0.9659258262890683122, 1.000000000000000000, 0.9659258262890683122, 1.000000000000000000, 0.9659258262890683122, 1.000000000000000000, 0.9659258262890683122, 1.000000000000000000, 0.9659258262890683122, 1.000000000000000000, 0.9659258262890683122, 1.000000000000000000, 0.9659258262890683122, 1.000000000000000000, 0.9659258262890683122, 1.000000000000000000, 0.9659258262890683122, 1.000000000000000000, 0.9659258262890683122, 1.000000000000000000, 0.9659258262890683122, 1.000000000000000000, 0.9659258262890683122, 1.000000000000000000, 0.9659258262890683122, 1.000000000000000000, 0.9659258262890683122, 1.000000000000000000, 0.9659258262890683122, 1.000000000000000000, 0.9659258262890683122, 1.000000000000000000, 0.9659258262890683122, 1.000000000000000000, 0.9659258262890683122, 1.000000000000000000, 0.9659258262890683122, 1.000000000000000000, 0.9659258262890683122, 1.000000000000000000, 0.9659258262890683122, 1.000000000000000000, 0.9659258262890683122, 1.000000000000000000, 0.9659258262890683122, 1.000000000000000000, 0.9659258262890683122, 1.000000000000000000, 0.9659258262890683122, 1.000000000000000000, 0.9659258262890683122, 1.000000000000000000, 0.9659258262890683122, 1.000000000000000000, 0.9659258262890683122, 1.000000000000000000, 0.9659258262890683122, 1.000000000000000000),
 ( 1.000000000000000000, 0.9659258262890683122, 1.000000000000000000, 0.9659258262890683122, 1.000000000000000000, 0.9659258262890683122, 1.000000000000000000, 0.9659258262890683122, 1.000000000000000000, 0.9659258262890683122, 1.000000000000000000, 0.9659258262890683122, 1.000000000000000000, 0.9659258262890683122, 1.000000000000000000, 0.9659258262890683122, 1.000000000000000000, 0.9659258262890683122, 1.000000000000000000, 0.9659258262890683122, 1.000000000000000000, 0.9659258262890683122, 1.000000000000000000, 0.9659258262890683122, 1.000000000000000000, 0.9659258262890683122, 1.000000000000000000, 0.9659258262890683122, 1.000000000000000000, 0.9659258262890683122, 1.000000000000000000, 0.9659258262890683122, 1.000000000000000000, 0.9659258262890683122, 1.000000000000000000, 0.9659258262890683122, 1.000000000000000000, 0.9659258262890683122, 1.000000000000000000, 0.9659258262890683122, 1.000000000000000000, 0.9659258262890683122, 1.000000000000000000, 0.9659258262890683122, 1.000000000000000000, 0.9659258262890683122, 1.000000000000000000, 0.9659258262890683122, 1.000000000000000000, 0.9659258262890683122, 1.000000000000000000, 0.9659258262890683122, 1.000000000000000000, 0.9659258262890683122, 1.000000000000000000, 0.9659258262890683122, 1.000000000000000000, 0.9659258262890683122, 1.000000000000000000, 0.9659258262890683122, 1.000000000000000000, 0.9659258262890683122, 1.000000000000000000, 0.9659258262890683122, 1.000000000000000000, 0.9659258262890683122, 1.000000000000000000, 0.9659258262890683122, 1.000000000000000000, 0.9659258262890683122, 1.000000000000000000, 0.9659258262890683122, 1.000000000000000000, 0.9659258262890683122, 1.000000000000000000, 0.9659258262890683122, 1.000000000000000000, 0.9659258262890683122, 1.000000000000000000, 0.9659258262890683122, 1.000000000000000000, 0.9659258262890683122, 1.000000000000000000, 0.9659258262890683122, 1.000000000000000000, 0.9659258262890683122, 1.000000000000000000, 0.9659258262890683122, 1.000000000000000000, 0.9659258262890683122, 1.000000000000000000, 0.9659258262890683122, 1.000000000000000000, 0.9659258262890683122, 1.000000000000000000, 0.9659258262890683122, 1.000000000000000000, 0.9659258262890683122, 1.000000000000000000, 0.9659258262890683122, 1.000000000000000000, 0.9659258262890683122, 1.000000000000000000, 0.9659258262890683122, 1.000000000000000000, 0.9659258262890683122, 1.000000000000000000, 0.9659258262890683122, 1.000000000000000000, 0.9659258262890683122, 1.000000000000000000, 0.9659258262890683122, 1.000000000000000000, 0.9659258262890683122, 1.000000000000000000, 0.9659258262890683122, 1.000000000000000000, 0.9659258262890683122, 1.000000000000000000, 0.9659258262890683122, 1.000000000000000000, 0.9659258262890683122, 1.000000000000000000, 0.9659258262890683122, 1.000000000000000000, 0.9659258262890683122, 1.000000000000000000, 0.9659258262890683122, 1.000000000000000000, 0.9659258262890683122, 1.000000000000000000, 0.9659258262890683122, 1.000000000000000000, 0.9659258262890683122, 1.000000000000000000, 0.9659258262890683122, 1.000000000000000000, 0.9659258262890683122, 1.000000000000000000, 0.9659258262890683122, 1.000000000000000000, 0.9659258262890683122, 1.000000000000000000, 0.9659258262890683122, 1.000000000000000000, 0.9659258262890683122, 1.000000000000000000, 0.9659258262890683122, 1.000000000000000000, 0.9659258262890683122, 1.000000000000000000, 0.9659258262890683122, 1.000000000000000000, 0.9659258262890683122, 1.000000000000000000, 0.9659258262890683122, 1.000000000000000000, 0.9659258262890683122, 1.000000000000000000, 0.9659258262890683122, 1.000000000000000000, 0.9659258262890683122, 1.000000000000000000, 0.9659258262890683122, 1.000000000000000000, 0.9659258262890683122, 1.000000000000000000, 0.9659258262890683122, 1.000000000000000000, 0.9659258262890683122, 1.000000000000000000, 0.9659258262890683122, 1.000000000000000000, 0.9659258262890683122, 1.000000000000000000, 0.9659258262890683122, 1.000000000000000000, 0.9659258262890683122, 1.000000000000000000, 0.9659258262890683122, 1.000000000000000000, 0.9659258262890683122, 1.000000000000000000, 0.9659258262890683122, 1.000000000000000000, 0.9659258262890683122, 1.000000000000000000, 0.9659258262890683122, 1.000000000000000000, 0.9659258262890683122, 1.000000000000000000, 0.9659258262890683122, 1.000000000000000000, 0.9659258262890683122, 1.000000000000000000, 0.9659258262890683122, 1.000000000000000000, 0.9659258262890683122, 1.000000000000000000, 0.9659258262890683122, 1.000000000000000000, 0.9659258262890683122, 1.000000000000000000, 0.9659258262890683122, 1.000000000000000000, 0.9659258262890683122, 1.000000000000000000, 0.9659258262890683122, 1.000000000000000000, 0.9659258262890683122, 1.000000000000000000, 0.9659258262890683122, 1.000000000000000000, 0.9659258262890683122, 1.000000000000000000, 0.9659258262890683122, 1.000000000000000000, 0.9659258262890683122, 1.000000000000000000, 0.9659258262890683122, 1.000000000000000000, 0.9659258262890683122, 1.000000000000000000, 0.9659258262890683122, 1.000000000000000000, 0.9659258262890683122, 1.000000000000000000, 0.9659258262890683122, 1.000000000000000000, 0.9659258262890683122, 1.000000000000000000, 0.9659258262890683122, 1.000000000000000000, 0.9659258262890683122, 1.000000000000000000, 0.9659258262890683122, 1.000000000000000000, 0.9659258262890683122, 1.000000000000000000, 0.9659258262890683122, 1.000000000000000000, 0.9659258262890683122, 1.000000000000000000, 0.9659258262890683122, 1.000000000000000000, 0.9659258262890683122, 1.000000000000000000, 0.9659258262890683122, 1.000000000000000000, 0.9659258262890683122, 1.000000000000000000, 0.9659258262890683122, 1.000000000000000000, 0.9659258262890683122, 1.000000000000000000, 0.9659258262890683122, 1.000000000000000000, 0.9659258262890683122, 1.000000000000000000, 0.9659258262890683122, 1.000000000000000000, 0.9659258262890683122, 1.000000000000000000, 0.9659258262890683122, 1.000000000000000000, 0.9659258262890683122, 1.000000000000000000, 0.9659258262890683122, 1.000000000000000000, 0.9659258262890683122, 1.000000000000000000, 0.9659258262890683122, 1.000000000000000000, 0.9659258262890683122, 1.000000000000000000, 0.9659258262890683122, 1.000000000000000000, 0.9659258262890683122, 1.000000000000000000, 0.9659258262890683122, 1.000000000000000000, 0.9659258262890683122, 1.000000000000000000, 0.9659258262890683122, 1.000000000000000000, 0.9659258262890683122, 1.000000000000000000, 0.9659258262890683122, 1.000000000000000000, 0.9659258262890683122, 1.000000000000000000, 0.9659258262890683122, 1.000000000000000000, 0.9659258262890683122, 1.000000000000000000, 0.9659258262890683122, 1.000000000000000000, 0.9659258262890683122, 1.000000000000000000, 0.9659258262890683122, 1.000000000000000000, 0.9659258262890683122, 1.000000000000000000, 0.9659258262890683122, 1.000000000000000000, 0.9659258262890683122, 1.000000000000000000, 0.9659258262890683122, 1.000000000000000000, 0.9659258262890683122, 1.000000000000000000, 0.9659258262890683122, 1.000000000000000000, 0.9659258262890683122, 1.000000000000000000, 0.9659258262890683122, 1.000000000000000000, 0.9659258262890683122, 1.000000000000000000, 0.9659258262890683122, 1.000000000000000000, 0.9659258262890683122, 1.000000000000000000, 0.9659258262890683122, 1.000000000000000000) ) ) 
 REPRESENTATION_ITEM ( '' )  SURFACE ( )  );
#72042 = CARTESIAN_POINT ( 'NONE',  ( -3.822225673302299676, 0.000000000000000000, 3.889525102760206909 ) ) ;
#72044 = CARTESIAN_POINT ( 'NONE',  ( -11.05192081855304309, -57.06859629180129900, -4.000000000000000888 ) ) ;
#72043 = CARTESIAN_POINT ( 'NONE',  ( 20.88017736071110875, 60.77201867748817676, -2.915334737309920765 ) ) ;
#72045 = CARTESIAN_POINT ( 'NONE',  ( -7.858200837834798946, -3.137962441252946544, 4.000000000000000888 ) ) ;
#72046 = CARTESIAN_POINT ( 'NONE',  ( -6.689969769698787871, 15.00000000000000000, -12.58200319823979285 ) ) ;
#72047 = CARTESIAN_POINT ( 'NONE',  ( 17.96484262340118221, 66.18868534415483396, -7.964842623401177768 ) ) ;
#72048 = VECTOR ( 'NONE', #82510, 1000.000000000000000 ) ;
#72049 = CARTESIAN_POINT ( 'NONE',  ( -0.8801773607111008646, 68.27201867748817676, 2.915334737309923430 ) ) ;
#72050 = DIRECTION ( 'NONE',  ( 0.000000000000000000, 1.000000000000000000, 0.000000000000000000 ) ) ;
#72051 = CARTESIAN_POINT ( 'NONE',  ( 7.361572987183170547, 22.05059781766745530, 9.846743663894590881 ) ) ;
#72052 = CARTESIAN_POINT ( 'NONE',  ( 0.5774900079438607392, 23.48035201082150536, 5.440088680355550821 ) ) ;
#72053 = CARTESIAN_POINT ( 'NONE',  ( 1.472469842513823179, 60.59226448433412315, -4.923371831947296329 ) ) ;
#72055 = CARTESIAN_POINT ( 'NONE',  ( 0.9413316022086168910, 13.45508385108958826, 6.499999999999973355 ) ) ;
#72054 = CARTESIAN_POINT ( 'NONE',  ( 20.88017736071110875, 35.77201867748816966, -2.915334737309920765 ) ) ;
#72056 = CARTESIAN_POINT ( 'NONE',  ( 17.39651004071841456, 64.08210964143329136, -6.500000000000001776 ) ) ;
#72057 = AXIS2_PLACEMENT_3D ( 'NONE', #29997, #60504, #67025 ) ;
#72058 = CARTESIAN_POINT ( 'NONE',  ( -2.816281873526473856, 44.12363466993042493, 9.499525473075851096E-16 ) ) ;
#72059 = VERTEX_POINT ( 'NONE', #28707 ) ;
#72060 = CARTESIAN_POINT ( 'NONE',  ( 10.00000000000000178, 49.31368534415484106, 10.88017736071110342 ) ) ;
#72062 = CARTESIAN_POINT ( 'NONE',  ( -13.69000000000001194, 92.00000000000000000, 9.500000000000000000 ) ) ;
#72061 = CARTESIAN_POINT ( 'NONE',  ( 22.81628187352647785, 26.41530133659708923, 3.434112377981063169 ) ) ;
#72063 = ADVANCED_FACE ( 'NONE', ( #22215 ), #22707, .F. ) ;
#72064 = CARTESIAN_POINT ( 'NONE',  ( 19.42250999205614548, 20.98035201082150891, -5.440088680355545492 ) ) ;
#72065 = CARTESIAN_POINT ( 'NONE',  ( 10.00000000000000000, 45.55374883491397497, -14.16423886937410082 ) ) ;
#72066 = CARTESIAN_POINT ( 'NONE',  ( 2.791683348922240793, 46.63393115100077324, 7.208316651077764092 ) ) ;
#72067 = CARTESIAN_POINT ( 'NONE',  ( 5.076628168052704559, 0.1755978176674514724, -8.527530157486179263 ) ) ;
#72068 = CARTESIAN_POINT ( 'NONE',  ( 0.5774900079438607392, 68.48035201082150536, 5.440088680355550821 ) ) ;
#72069 = CARTESIAN_POINT ( 'NONE',  ( -7.750000000000000000, 1.019547802438458550, -3.750000000000000000 ) ) ;
#72070 = CARTESIAN_POINT ( 'NONE',  ( 20.36894250292379382, 13.67874883491396965, 10.36894250292379205 ) ) ;
#72071 = PRESENTATION_LAYER_ASSIGNMENT (  '', '', ( #9849 ) ) ;
#72072 = CARTESIAN_POINT ( 'NONE',  ( 8.629999999999995453, 43.00000000000000000, 6.500000000000000888 ) ) ;
#72073 = CARTESIAN_POINT ( 'NONE',  ( 17.39651004071842166, 12.93575266056827822, 6.499999999999998224 ) ) ;
#72074 = ORIENTED_EDGE ( 'NONE', *, *, #44949, .F. ) ;
#72075 = CARTESIAN_POINT ( 'NONE',  ( 6.204703633549690345, 52.84541550158062506, 14.16423886937410082 ) ) ;
#72076 = CARTESIAN_POINT ( 'NONE',  ( 22.26659068614894466, 43.88708216824729647, 7.082119434687054849 ) ) ;
#72077 = CARTESIAN_POINT ( 'NONE',  ( 7.361572987183169658, 19.96726448433411960, -9.846743663894592657 ) ) ;
#72078 = FACE_BOUND ( 'NONE', #51699, .T. ) ;
#72079 = CARTESIAN_POINT ( 'NONE',  ( 34.56412365047464874, 28.99999999999999645, 10.00000000000000000 ) ) ;
#72081 = CARTESIAN_POINT ( 'NONE',  ( 22.81628187352647785, 26.62363466993042138, 6.195893100308588602E-16 ) ) ;
#72080 = CARTESIAN_POINT ( 'NONE',  ( 20.88017736071110875, 5.772018677488170546, -2.915334737309920765 ) ) ;
#72082 = CARTESIAN_POINT ( 'NONE',  ( -0.3689425029237881626, 37.42874883491396787, 10.36894250292379027 ) ) ;
#72083 = LINE ( 'NONE', #64566, #12531 ) ;
#72084 = CARTESIAN_POINT ( 'NONE',  ( -2.638427012816840111, 4.967264484334121377, -9.846743663894590881 ) ) ;
#72085 = ORIENTED_EDGE ( 'NONE', *, *, #73858, .T. ) ;
#72086 =( LENGTH_UNIT ( ) NAMED_UNIT ( * ) SI_UNIT ( .MILLI., .METRE. ) );
#72087 = CARTESIAN_POINT ( 'NONE',  ( 12.63842701281683922, 24.55059781766745175, -9.846743663894590881 ) ) ;
#72088 =( LENGTH_UNIT ( ) NAMED_UNIT ( * ) SI_UNIT ( .MILLI., .METRE. ) );
#72089 = ORIENTED_EDGE ( 'NONE', *, *, #6776, .T. ) ;
#72091 = CARTESIAN_POINT ( 'NONE',  ( 10.00000000000000000, 6.813685344154838397, -10.88017736071110342 ) ) ;
#72090 = CARTESIAN_POINT ( 'NONE',  ( -0.8801773607111008646, 8.272018677488171434, 2.915334737309923430 ) ) ;
#72093 = CARTESIAN_POINT ( 'NONE',  ( 19.38216949554541202, 5.998634669930420493, 9.382169495545424454 ) ) ;
#72092 = CARTESIAN_POINT ( 'NONE',  ( 14.92337183194729633, 52.67559781766745175, 8.527530157486181039 ) ) ;
#72094 = DIRECTION ( 'NONE',  ( -0.000000000000000000, -1.000000000000000000, 0.000000000000000000 ) ) ;
#72095 = VECTOR ( 'NONE', #31202, 1000.000000000000000 ) ;
#72096 = LINE ( 'NONE', #63606, #43022 ) ;
#72097 = CARTESIAN_POINT ( 'NONE',  ( 13.43411237798106583, 12.66530133659708746, -12.81628187352647252 ) ) ;
#72098 = EDGE_LOOP ( 'NONE', ( #25793, #56036, #65987, #20697 ) ) ;
#72099 = CARTESIAN_POINT ( 'NONE',  ( 22.26659068614895176, 54.72041550158063217, -7.082119434687042414 ) ) ;
#72100 = ORIENTED_EDGE ( 'NONE', *, *, #63870, .T. ) ;
#72101 = CARTESIAN_POINT ( 'NONE',  ( 22.26659068614894466, 53.88708216824731068, 7.082119434687054849 ) ) ;
#72102 = ORIENTED_EDGE ( 'NONE', *, *, #55358, .F. ) ;
#72103 = CARTESIAN_POINT ( 'NONE',  ( 4.559911319644449179, 38.89701867748817676, 9.422509992056141925 ) ) ;
#72104 = CARTESIAN_POINT ( 'NONE',  ( 12.91533473730993009, 46.60535201082150536, -10.88017736071109987 ) ) ;
#72105 = CARTESIAN_POINT ( 'NONE',  ( 7.084665262690076126, 32.02201867748816966, -10.88017736071110164 ) ) ;
#72106 = CARTESIAN_POINT ( 'NONE',  ( 20.88017736071110875, 45.77201867748816966, -2.915334737309920765 ) ) ;
#72107 = EDGE_CURVE ( 'NONE', #68599, #32737, #41399, .T. ) ;
#72108 = EDGE_CURVE ( 'NONE', #156, #90281, #3455, .T. ) ;
#72111 = VERTEX_POINT ( 'NONE', #13712 ) ;
#72110 = AXIS2_PLACEMENT_3D ( 'NONE', #8598, #68126, #84110 ) ;
#72109 = SURFACE_SIDE_STYLE ('',( #20097 ) ) ;
#72112 = CARTESIAN_POINT ( 'NONE',  ( 0.1532563361054082862, 11.21726448433411605, 2.638427012816831674 ) ) ;
#72113 = ORIENTED_EDGE ( 'NONE', *, *, #96068, .T. ) ;
#72114 = DIRECTION ( 'NONE',  ( 0.009903002720634835818, -0.9999509640662961329, 0.000000000000000000 ) ) ;
#72115 = CARTESIAN_POINT ( 'NONE',  ( 12.63842701281683922, 44.55059781766745175, -9.846743663894590881 ) ) ;
#72116 = CARTESIAN_POINT ( 'NONE',  ( -6.000000000000000000, 78.07179676972447169, -4.250000000000000000 ) ) ;
#72117 = CARTESIAN_POINT ( 'NONE',  ( 22.81628187352648496, 56.83196800326374643, -3.434112377981050290 ) ) ;
#72118 = LINE ( 'NONE', #3646, #31518 ) ;
#72119 = DIRECTION ( 'NONE',  ( 0.000000000000000000, 0.000000000000000000, -1.000000000000000000 ) ) ;
#72120 = CARTESIAN_POINT ( 'NONE',  ( -43.50402400080862009, 106.3600696521562412, 5.072649039476010202 ) ) ;
#72121 = FACE_OUTER_BOUND ( 'NONE', #48308, .T. ) ;
#72122 = CARTESIAN_POINT ( 'NONE',  ( 2.917880565312950480, 60.97041550158063927, -12.26659068614894821 ) ) ;
#72123 = CARTESIAN_POINT ( 'NONE',  ( 6.382347221874381304, 14.49999999999999112, 13.57444820018236520 ) ) ;
#72124 = VERTEX_POINT ( 'NONE', #83692 ) ;
#72126 = AXIS2_PLACEMENT_3D ( 'NONE', #83082, #98618, #60576 ) ;
#72125 = CARTESIAN_POINT ( 'NONE',  ( 2.313926553644108641E-17, 1.840000000000001412, 0.000000000000000000 ) ) ;
#72127 = CARTESIAN_POINT ( 'NONE',  ( 2.791683348922237240, 30.38393115100078390, -7.208316651077763204 ) ) ;
#72128 = CARTESIAN_POINT ( 'NONE',  ( -1.099225684535947600, 63.70696800326376774, -6.408140936763238038 ) ) ;
#72129 = CARTESIAN_POINT ( 'NONE',  ( -2.816281873526473856, 4.331968003263754419, 3.434112377981055619 ) ) ;
#72130 = CARTESIAN_POINT ( 'NONE',  ( 0.1532563361054100626, 0.8005978176674514168, -2.638427012816831230 ) ) ;
#72131 = DIRECTION ( 'NONE',  ( 0.000000000000000000, 1.000000000000000000, 0.000000000000000000 ) ) ;
#72132 = CARTESIAN_POINT ( 'NONE',  ( 0.1532563361054083140, 11.00893115100078568, 1.131784320476157264E-15 ) ) ;
#72133 = CARTESIAN_POINT ( 'NONE',  ( 7.361572987183170547, 52.05059781766745175, 9.846743663894590881 ) ) ;
#72134 = CARTESIAN_POINT ( 'NONE',  ( 4.873787042390789637, -0.03417435944610275333, -13.39061984619918988 ) ) ;
#72135 = ADVANCED_FACE ( 'NONE', ( #44195, #74705 ), #29196, .T. ) ;
#72136 = ORIENTED_EDGE ( 'NONE', *, *, #19227, .T. ) ;
#72137 = EDGE_CURVE ( 'NONE', #11101, #94992, #87675, .T. ) ;
#72138 = CARTESIAN_POINT ( 'NONE',  ( -0.3689425029237881626, 57.42874883491397497, 10.36894250292379027 ) ) ;
#72139 = CARTESIAN_POINT ( 'NONE',  ( 0.000000000000000000, 14.49999999999999822, 0.000000000000000000 ) ) ;
#72140 = CARTESIAN_POINT ( 'NONE',  ( 19.42250999205614548, 35.98035201082151247, -5.440088680355545492 ) ) ;
#72142 = FACE_OUTER_BOUND ( 'NONE', #65800, .T. ) ;
#72141 = CARTESIAN_POINT ( 'NONE',  ( 13.43411237798106583, 22.66530133659708923, -12.81628187352647252 ) ) ;
#72143 = CARTESIAN_POINT ( 'NONE',  ( 4.559911319644449179, 2.230352010821504471, -9.422509992056141925 ) ) ;
#72144 = CARTESIAN_POINT ( 'NONE',  ( 13.34948392230371361, 14.95077488074853456, 6.279918722515068552 ) ) ;
#72145 = CARTESIAN_POINT ( 'NONE',  ( 1.274849032794280523, 68.57228050351031357, 6.499999999999960032 ) ) ;
#72146 = CARTESIAN_POINT ( 'NONE',  ( 17.20831665107776587, 52.88393115100078035, 7.208316651077764980 ) ) ;
#72147 = CARTESIAN_POINT ( 'NONE',  ( 2.791683348922237240, 20.38393115100078745, -7.208316651077763204 ) ) ;
#72148 = CARTESIAN_POINT ( 'NONE',  ( 7.964842623401177768, -28.81131465584515539, -7.964842623401181321 ) ) ;
#72149 = CARTESIAN_POINT ( 'NONE',  ( 22.81628187352648496, 16.83196800326374998, -3.434112377981050290 ) ) ;
#72150 = CARTESIAN_POINT ( 'NONE',  ( -45.94000000000001194, 99.99999999999998579, -5.000000000000000000 ) ) ;
#72152 = CARTESIAN_POINT ( 'NONE',  ( -7.750000000000000000, 80.07179676972448590, -6.500000000000000888 ) ) ;
#72151 = CARTESIAN_POINT ( 'NONE',  ( 20.88017736071110164, 30.35535201082151247, 2.915334737309930979 ) ) ;
#72153 = DIRECTION ( 'NONE',  ( 0.000000000000000000, 0.000000000000000000, 1.000000000000000000 ) ) ;
#72154 = CARTESIAN_POINT ( 'NONE',  ( 2.917880565312950480, 35.97041550158063217, -12.26659068614894821 ) ) ;
#72155 = CARTESIAN_POINT ( 'NONE',  ( 13.79529636645030344, 28.26208216824729647, 14.16423886937410614 ) ) ;
#72156 = CARTESIAN_POINT ( 'NONE',  ( 20.88017736071110164, 10.35535201082150714, 2.915334737309930979 ) ) ;
#72157 = CARTESIAN_POINT ( 'NONE',  ( 19.84674366389459621, 48.50893115100078745, 7.409399052514197653E-17 ) ) ;
#72158 = CARTESIAN_POINT ( 'NONE',  ( 0.6178305044545818747, 43.49863466993042493, -9.382169495545419124 ) ) ;
#72159 = CARTESIAN_POINT ( 'NONE',  ( 2.035157376598822676, 22.43868534415483396, -7.964842623401177768 ) ) ;
#72160 = AXIS2_PLACEMENT_3D ( 'NONE', #24753, #94211, #56233 ) ;
#72161 = CARTESIAN_POINT ( 'NONE',  ( 19.84674366389459266, 48.71726448433413026, -2.638427012816827677 ) ) ;
#72162 = CARTESIAN_POINT ( 'NONE',  ( 17.96484262340118221, 39.93868534415484106, 7.964842623401181321 ) ) ;
#72163 = CARTESIAN_POINT ( 'NONE',  ( -2.816281873526473856, 4.331968003263754419, 3.434112377981055619 ) ) ;
#72165 = ADVANCED_FACE ( 'NONE', ( #32643 ), #85167, .F. ) ;
#72164 = CARTESIAN_POINT ( 'NONE',  ( 2.917880565312950480, 25.97041550158063572, -12.26659068614894821 ) ) ;
#72166 = CARTESIAN_POINT ( 'NONE',  ( 14.82629065241282262, 14.76984952913051430, 1.844815641835429121 ) ) ;
#72167 = UNCERTAINTY_MEASURE_WITH_UNIT (LENGTH_MEASURE( 1.000000000000000082E-05 ), #72086, 'distance_accuracy_value', 'NONE');
#72168 = CARTESIAN_POINT ( 'NONE',  ( 18.52753015748617571, 28.09226448433411960, 4.923371831947298993 ) ) ;
#72169 = CARTESIAN_POINT ( 'NONE',  ( 10.00000000000000000, 47.87363466993042493, -12.81628187352647608 ) ) ;
#72170 = CARTESIAN_POINT ( 'NONE',  ( 7.361572987183170547, 67.05059781766746596, 9.846743663894590881 ) ) ;
#72171 = ORIENTED_EDGE ( 'NONE', *, *, #11124, .T. ) ;
#72172 = CARTESIAN_POINT ( 'NONE',  ( 20.03743638938528804, 11.75197528031017136, 6.399506433553904472 ) ) ;
#72173 = CARTESIAN_POINT ( 'NONE',  ( 7.084665262690076126, 2.022018677488171434, -10.88017736071110164 ) ) ;
#72174 = CARTESIAN_POINT ( 'NONE',  ( 7.084665262690076126, 62.02201867748816966, -10.88017736071110164 ) ) ;
#72175 = CARTESIAN_POINT ( 'NONE',  ( 13.79529636645031943, 15.34541550158063750, -14.16423886937409904 ) ) ;
#72176 = CARTESIAN_POINT ( 'NONE',  ( 12.91533473730992121, 64.52201867748817676, 10.88017736071110164 ) ) ;
#72177 = CARTESIAN_POINT ( 'NONE',  ( 14.92337183194729633, 47.67559781766745175, 8.527530157486181039 ) ) ;
#72178 = CARTESIAN_POINT ( 'NONE',  ( 12.91533473730993009, 36.60535201082151247, -10.88017736071109987 ) ) ;
#72179 = CYLINDRICAL_SURFACE ( 'NONE', #4837, 15.00000000000000000 ) ;
#72180 = CARTESIAN_POINT ( 'NONE',  ( 14.92337183194729633, 62.67559781766745886, 8.527530157486181039 ) ) ;
#72181 = EDGE_LOOP ( 'NONE', ( #28675, #9645, #57574, #92217 ) ) ;
#72182 = CIRCLE ( 'NONE', #65826, 0.5000000000000004441 ) ;
#72183 = DIRECTION ( 'NONE',  ( 0.000000000000000000, 0.000000000000000000, -1.000000000000000000 ) ) ;
#72184 = ORIENTED_EDGE ( 'NONE', *, *, #88912, .F. ) ;
#72185 = ORIENTED_EDGE ( 'NONE', *, *, #90571, .F. ) ;
#72186 = CARTESIAN_POINT ( 'NONE',  ( 6.382347221874334231, 0.5000000000000004441, 13.57444820018231724 ) ) ;
#72187 = CARTESIAN_POINT ( 'NONE',  ( -2.266590686148945544, 2.220415501580634388, 7.082119434687048631 ) ) ;
#72188 = CARTESIAN_POINT ( 'NONE',  ( 24.16423886937409904, 4.095415501580634832, 3.795296366450317205 ) ) ;
#72189 = CARTESIAN_POINT ( 'NONE',  ( 24.16423886937409904, 49.09541550158063217, 3.795296366450317205 ) ) ;
#72190 = CARTESIAN_POINT ( 'NONE',  ( 18.52753015748617571, 53.09226448433412315, 4.923371831947298993 ) ) ;
#72191 = CARTESIAN_POINT ( 'NONE',  ( 10.00000000000000178, 32.25893115100078745, 9.846743663894594434 ) ) ;
#72192 = CARTESIAN_POINT ( 'NONE',  ( 3.591859063236761518, 64.95696800326376774, 11.09922568453594849 ) ) ;
#72194 = CARTESIAN_POINT ( 'NONE',  ( 7.361572987183169658, 59.96726448433410894, -9.846743663894592657 ) ) ;
#72193 = CARTESIAN_POINT ( 'NONE',  ( 7.084665262690076126, 32.02201867748816966, -10.88017736071110164 ) ) ;
#72195 = CARTESIAN_POINT ( 'NONE',  ( 6.204703633549690345, 5.762082168247301794, -14.16423886937410259 ) ) ;
#72196 = CARTESIAN_POINT ( 'NONE',  ( -4.164238869374099039, 56.80374883491397497, 8.674139862899312516E-16 ) ) ;
#72197 = CARTESIAN_POINT ( 'NONE',  ( 15.44008868035555260, 4.730352010821505360, 9.422509992056143702 ) ) ;
#72198 = CARTESIAN_POINT ( 'NONE',  ( 0.1532563361054082862, 66.21726448433413736, 2.638427012816831674 ) ) ;
#72199 = VECTOR ( 'NONE', #63526, 1000.000000000000000 ) ;
#72200 = CARTESIAN_POINT ( 'NONE',  ( -38.69000000000001194, 93.50000000000000000, 9.500000000000000000 ) ) ;
#72201 = CARTESIAN_POINT ( 'NONE',  ( 20.88017736071110519, 60.56368534415484106, 2.639326808657452039E-16 ) ) ;
#72202 = CARTESIAN_POINT ( 'NONE',  ( 2.791683348922237240, 25.38393115100078390, -7.208316651077763204 ) ) ;
#72203 = CARTESIAN_POINT ( 'NONE',  ( 8.527530157486179263, -31.90773551566587685, 4.923371831947292776 ) ) ;
#72204 = ORIENTED_EDGE ( 'NONE', *, *, #505, .F. ) ;
#72205 = CARTESIAN_POINT ( 'NONE',  ( 3.999999999999999112, 1.639999999999999014, 4.898587196589411843E-16 ) ) ;
#72206 = STYLED_ITEM ( 'NONE', ( #4423 ), #75723 ) ;
#72207 = ORIENTED_EDGE ( 'NONE', *, *, #96222, .F. ) ;
#72208 = CARTESIAN_POINT ( 'NONE',  ( 7.361572987183170547, 17.05059781766745530, 9.846743663894590881 ) ) ;
#72209 = ORIENTED_EDGE ( 'NONE', *, *, #17841, .F. ) ;
#72210 = CARTESIAN_POINT ( 'NONE',  ( 20.36894250292379382, 28.67874883491396787, 10.36894250292379205 ) ) ;
#72211 = CARTESIAN_POINT ( 'NONE',  ( 10.00000000000000000, 34.75893115100078745, -9.846743663894594434 ) ) ;
#72212 = CARTESIAN_POINT ( 'NONE',  ( 17.96484262340118221, 51.18868534415483396, -7.964842623401177768 ) ) ;
#72213 = CARTESIAN_POINT ( 'NONE',  ( 18.00000000000000355, 73.00000000000001421, -6.250000000000000000 ) ) ;
#72214 = CARTESIAN_POINT ( 'NONE',  ( 7.084665262690076126, 49.10535201082149825, 10.88017736071109987 ) ) ;
#72215 = CARTESIAN_POINT ( 'NONE',  ( 0.1532563361054083140, 46.00893115100079456, 1.131784320476157264E-15 ) ) ;
#72216 = CARTESIAN_POINT ( 'NONE',  ( -12.81628187352647608, 14.12363466993042671, 3.903127820947815962E-15 ) ) ;
#72217 = ORIENTED_EDGE ( 'NONE', *, *, #57021, .F. ) ;
#72218 = CARTESIAN_POINT ( 'NONE',  ( -0.8801773607111008646, 48.27201867748816966, 2.915334737309923430 ) ) ;
#72219 = CARTESIAN_POINT ( 'NONE',  ( 22.26659068614895176, 24.72041550158063572, -7.082119434687042414 ) ) ;
#72220 = ORIENTED_EDGE ( 'NONE', *, *, #18920, .T. ) ;
#72221 = VERTEX_POINT ( 'NONE', #23202 ) ;
#72222 = CARTESIAN_POINT ( 'NONE',  ( 22.81628187352647785, 36.41530133659707502, 3.434112377981063169 ) ) ;
#72223 = CARTESIAN_POINT ( 'NONE',  ( 1.472469842513823179, 20.59226448433411960, -4.923371831947296329 ) ) ;
#72224 = CARTESIAN_POINT ( 'NONE',  ( 2.035157376598824452, 3.688685344154837953, 7.964842623401179544 ) ) ;
#72225 = CARTESIAN_POINT ( 'NONE',  ( 10.00000000000000000, 52.87363466993041783, -12.81628187352647608 ) ) ;
#72226 = CYLINDRICAL_SURFACE ( 'NONE', #55959, 0.5000000000000004441 ) ;
#72227 = CARTESIAN_POINT ( 'NONE',  ( 14.92337183194729633, 32.67559781766745175, 8.527530157486181039 ) ) ;
#72228 = EDGE_CURVE ( 'NONE', #13314, #14763, #85656, .T. ) ;
#72230 = ORIENTED_EDGE ( 'NONE', *, *, #5652, .F. ) ;
#72229 = CARTESIAN_POINT ( 'NONE',  ( 2.035157376598824452, 58.68868534415482685, 7.964842623401179544 ) ) ;
#72231 = AXIS2_PLACEMENT_3D ( 'NONE', #95981, #42969, #36455 ) ;
#72232 = CARTESIAN_POINT ( 'NONE',  ( -3.115783986955657614, 15.00000000000000000, 14.16128137375395468 ) ) ;
#72233 = DIRECTION ( 'NONE',  ( -8.704148513061227277E-14, 0.000000000000000000, 1.000000000000000000 ) ) ;
#72234 = CARTESIAN_POINT ( 'NONE',  ( 17.20831665107776587, 2.883931151000785231, 7.208316651077764980 ) ) ;
#72235 = CARTESIAN_POINT ( 'NONE',  ( 6.565887622018943937, 18.08196800326375708, -12.81628187352647608 ) ) ;
#72236 = FACE_OUTER_BOUND ( 'NONE', #5769, .T. ) ;
#72237 = CARTESIAN_POINT ( 'NONE',  ( 0.1532563361054100626, 40.80059781766745886, -2.638427012816831230 ) ) ;
#72238 = CARTESIAN_POINT ( 'NONE',  ( -8.900000000000002132, 80.99999999999994316, 0.000000000000000000 ) ) ;
#72239 = CARTESIAN_POINT ( 'NONE',  ( 22.26659068614895176, 4.720415501580633943, -7.082119434687042414 ) ) ;
#72240 = CARTESIAN_POINT ( 'NONE',  ( 17.20831665107776587, 32.88393115100078745, 7.208316651077764980 ) ) ;
#72241 = CARTESIAN_POINT ( 'NONE',  ( 21.09922568453594849, 31.20696800326375353, 6.408140936763242479 ) ) ;
#72243 = CARTESIAN_POINT ( 'NONE',  ( 7.640917710488917436, 0.04922511925146979411, 12.61992379908760853 ) ) ;
#72242 = PLANE ( 'NONE',  #42107 ) ;
#72244 = CARTESIAN_POINT ( 'NONE',  ( 10.00000000000000000, 61.81368534415484106, -10.88017736071110342 ) ) ;
#72245 = CARTESIAN_POINT ( 'NONE',  ( 3.591859063236761518, 4.956968003263753531, 11.09922568453594849 ) ) ;
#72246 = FACE_OUTER_BOUND ( 'NONE', #78449, .T. ) ;
#72247 = CARTESIAN_POINT ( 'NONE',  ( 2.791683348922237240, 40.38393115100078035, -7.208316651077763204 ) ) ;
#72248 = CARTESIAN_POINT ( 'NONE',  ( 7.084665262690076126, 22.02201867748817321, -10.88017736071110164 ) ) ;
#72249 = CARTESIAN_POINT ( 'NONE',  ( 10.00000000000000178, 30.37363466993042138, 12.81628187352647608 ) ) ;
#72250 = MECHANICAL_DESIGN_GEOMETRIC_PRESENTATION_REPRESENTATION (  '', ( #81812 ), #64246 ) ;
#72251 = CARTESIAN_POINT ( 'NONE',  ( 5.076628168052703671, 16.84226448433411960, 8.527530157486179263 ) ) ;
#72252 = SURFACE_STYLE_FILL_AREA ( #10781 ) ;
#72253 = CARTESIAN_POINT ( 'NONE',  ( 3.035766082959412415E-15, 78.91966277462714174, -5.000000000000000000 ) ) ;
#72254 = ADVANCED_FACE ( 'NONE', ( #9163 ), #17175, .F. ) ;
#72255 = CARTESIAN_POINT ( 'NONE',  ( -0.8801773607110991993, 27.85535201082150181, -2.915334737309923874 ) ) ;
#72256 = ORIENTED_EDGE ( 'NONE', *, *, #24195, .T. ) ;
#72257 = CIRCLE ( 'NONE', #6825, 0.2500000000000002220 ) ;
#72258 = CARTESIAN_POINT ( 'NONE',  ( 17.96484262340118221, 64.93868534415483396, 7.964842623401181321 ) ) ;
#72259 = CARTESIAN_POINT ( 'NONE',  ( 10.00000000000000000, 1.813685344154837731, -10.88017736071110342 ) ) ;
#72261 = CARTESIAN_POINT ( 'NONE',  ( 17.96484262340118221, 26.18868534415483396, -7.964842623401177768 ) ) ;
#72260 = CARTESIAN_POINT ( 'NONE',  ( 14.92337183194729633, 37.67559781766745175, 8.527530157486181039 ) ) ;
#72262 = DIRECTION ( 'NONE',  ( -0.5547001962252290364, -0.8320502943378437211, 0.000000000000000000 ) ) ;
#72263 = CIRCLE ( 'NONE', #61061, 14.49999999999999822 ) ;
#72264 = CARTESIAN_POINT ( 'NONE',  ( 4.559911319644449179, 48.89701867748817676, 9.422509992056141925 ) ) ;
#72266 = DIRECTION ( 'NONE',  ( -0.000000000000000000, 0.000000000000000000, 1.000000000000000000 ) ) ;
#72265 = CARTESIAN_POINT ( 'NONE',  ( 17.96484262340118221, 9.938685344154839285, 7.964842623401181321 ) ) ;
#72267 = CARTESIAN_POINT ( 'NONE',  ( 12.63842701281683922, 4.550597817667451750, -9.846743663894590881 ) ) ;
#72268 = CARTESIAN_POINT ( 'NONE',  ( 17.20831665107776587, 57.88393115100078745, 7.208316651077764980 ) ) ;
#72269 = CARTESIAN_POINT ( 'NONE',  ( 10.00000000000000178, 48.05374883491396787, 14.16423886937410082 ) ) ;
#72270 = DIRECTION ( 'NONE',  ( 0.000000000000000000, 0.000000000000000000, -1.000000000000000000 ) ) ;
#72272 = TOROIDAL_SURFACE ( 'NONE', #24193, 3.250000000000001332, 0.2500000000000000000 ) ;
#72271 = CARTESIAN_POINT ( 'NONE',  ( 10.00000000000000000, 35.55374883491396787, -14.16423886937410082 ) ) ;
#72273 = FACE_OUTER_BOUND ( 'NONE', #74009, .T. ) ;
#72274 = CARTESIAN_POINT ( 'NONE',  ( 12.91533473730992121, 4.522018677488170546, 10.88017736071110164 ) ) ;
#72275 = CARTESIAN_POINT ( 'NONE',  ( 7.361572987183169658, 34.96726448433411605, -9.846743663894592657 ) ) ;
#72277 = PLANE ( 'NONE',  #86989 ) ;
#72276 = DIRECTION ( 'NONE',  ( 0.000000000000000000, 1.000000000000000000, 0.000000000000000000 ) ) ;
#72278 = CARTESIAN_POINT ( 'NONE',  ( -0.8801773607110991993, 62.85535201082150536, -2.915334737309923874 ) ) ;
#72279 = CARTESIAN_POINT ( 'NONE',  ( -8.470897558477446410, 2.337810934421868936E-16, -11.92401951126092641 ) ) ;
#72280 = CARTESIAN_POINT ( 'NONE',  ( -0.8801773607111008646, 33.27201867748817676, 2.915334737309923430 ) ) ;
#72281 = CARTESIAN_POINT ( 'NONE',  ( 13.43411237798105340, 55.58196800326374643, 12.81628187352647963 ) ) ;
#72282 = CARTESIAN_POINT ( 'NONE',  ( 22.81628187352648496, 16.83196800326374998, -3.434112377981050290 ) ) ;
#72283 = CARTESIAN_POINT ( 'NONE',  ( 19.84674366389459621, 8.508931151000785675, 7.409399052514197653E-17 ) ) ;
#72284 = ORIENTED_EDGE ( 'NONE', *, *, #4631, .F. ) ;
#72285 = CARTESIAN_POINT ( 'NONE',  ( -4.164238869374099927, 62.01208216824728936, 3.795296366450308767 ) ) ;
#72286 = AXIS2_PLACEMENT_3D ( 'NONE', #75680, #90180, #90677 ) ;
#72287 = CARTESIAN_POINT ( 'NONE',  ( 10.00000000000000178, 23.05374883491397142, 14.16423886937410082 ) ) ;
#72288 = CARTESIAN_POINT ( 'NONE',  ( 2.035157376598824452, 38.68868534415483396, 7.964842623401179544 ) ) ;
#72289 = CARTESIAN_POINT ( 'NONE',  ( 20.88017736071110519, 45.56368534415484106, 2.639326808657452039E-16 ) ) ;
#72290 = DIRECTION ( 'NONE',  ( 0.1736481776669272503, -0.9848077530122086864, 0.000000000000000000 ) ) ;
#72291 = EDGE_CURVE ( 'NONE', #12076, #74689, #71704, .T. ) ;
#72292 = CARTESIAN_POINT ( 'NONE',  ( 11.04400142266738882, -89.88311504653209738, -3.999999999999999112 ) ) ;
#72293 = CARTESIAN_POINT ( 'NONE',  ( 1.472469842513823179, 11.42559781766745175, 4.923371831947296329 ) ) ;
#72294 = CARTESIAN_POINT ( 'NONE',  ( 20.03743638938523830, 21.75197528031017669, 6.399506433553980855 ) ) ;
#72295 = CARTESIAN_POINT ( 'NONE',  ( -46.50477113700967635, 102.7537820721726831, 6.796471197945592735 ) ) ;
#72296 = CARTESIAN_POINT ( 'NONE',  ( 0.1532563361054100626, 20.80059781766744464, -2.638427012816831230 ) ) ;
#72297 = CARTESIAN_POINT ( 'NONE',  ( 0.1532563361054083140, 56.00893115100078745, 1.131784320476157264E-15 ) ) ;
#72298 = ADVANCED_FACE ( 'NONE', ( #31164 ), #41785, .T. ) ;
#72299 = CARTESIAN_POINT ( 'NONE',  ( 10.00000000000000000, 26.81368534415484106, -10.88017736071110342 ) ) ;
#72300 = UNCERTAINTY_MEASURE_WITH_UNIT (LENGTH_MEASURE( 1.000000000000000082E-05 ), #46609, 'distance_accuracy_value', 'NONE');
#72301 = CARTESIAN_POINT ( 'NONE',  ( 0.6178305044545838731, 39.74863466993041072, 9.382169495545420901 ) ) ;
#72302 = CARTESIAN_POINT ( 'NONE',  ( 0.5774900079438607392, 63.48035201082149825, 5.440088680355550821 ) ) ;
#72303 = CARTESIAN_POINT ( 'NONE',  ( 2.791683348922237240, 25.38393115100078390, -7.208316651077763204 ) ) ;
#72305 = CARTESIAN_POINT ( 'NONE',  ( 10.00000000000000178, 27.25893115100078390, 9.846743663894594434 ) ) ;
#72304 = CARTESIAN_POINT ( 'NONE',  ( 2.917880565312950480, 60.97041550158063927, -12.26659068614894821 ) ) ;
#72306 = CARTESIAN_POINT ( 'NONE',  ( 12.83294900548068007, 14.49999999999999112, -7.766300266068417280 ) ) ;
#72307 = CARTESIAN_POINT ( 'NONE',  ( 22.26659068614895176, 14.72041550158063572, -7.082119434687042414 ) ) ;
#72308 = CARTESIAN_POINT ( 'NONE',  ( -0.3689425029237881626, 37.42874883491396787, 10.36894250292379027 ) ) ;
#72309 = CARTESIAN_POINT ( 'NONE',  ( 0.1532563361054083140, 26.00893115100078745, 1.131784320476157264E-15 ) ) ;
#72310 = CARTESIAN_POINT ( 'NONE',  ( -0.3077640640441539621, 70.00000000000000000, 5.999999999999999112 ) ) ;
#72311 = CARTESIAN_POINT ( 'NONE',  ( 19.42250999205614193, 30.14701867748817321, 5.440088680355555262 ) ) ;
#72312 = CARTESIAN_POINT ( 'NONE',  ( -0.8801773607110991993, 52.85535201082151247, -2.915334737309923874 ) ) ;
#72313 = CARTESIAN_POINT ( 'NONE',  ( 1.472469842513823179, 56.42559781766745886, 4.923371831947296329 ) ) ;
#72314 = ORIENTED_EDGE ( 'NONE', *, *, #23539, .T. ) ;
#72315 = CARTESIAN_POINT ( 'NONE',  ( -2.816281873526471635, 48.91530133659708213, -3.434112377981056508 ) ) ;
#72316 = CARTESIAN_POINT ( 'NONE',  ( 20.88017736071110875, 50.77201867748817676, -2.915334737309920765 ) ) ;
#72317 = ORIENTED_EDGE ( 'NONE', *, *, #16399, .T. ) ;
#72318 = CARTESIAN_POINT ( 'NONE',  ( 7.084665262690076126, 59.10535201082150536, 10.88017736071109987 ) ) ;
#72319 = COLOUR_RGB ( '', 0.72549020, 0.75294118, 0.79215686) ;
#72320 = ORIENTED_EDGE ( 'NONE', *, *, #30401, .T. ) ;
#72321 = CARTESIAN_POINT ( 'NONE',  ( 17.96484262340118221, 64.93868534415483396, 7.964842623401181321 ) ) ;
#72322 = CARTESIAN_POINT ( 'NONE',  ( 20.88017736071110875, 60.77201867748817676, -2.915334737309920321 ) ) ;
#72323 = CARTESIAN_POINT ( 'NONE',  ( 19.72487221294570858, 0.000000000000000000, -6.500000000000000888 ) ) ;
#72324 = CARTESIAN_POINT ( 'NONE',  ( 12.91533473730992121, 9.522018677488171434, 10.88017736071110164 ) ) ;
#72325 = CARTESIAN_POINT ( 'NONE',  ( 17.20831665107776587, 14.13393115100078568, -7.208316651077762316 ) ) ;
#72326 = CARTESIAN_POINT ( 'NONE',  ( 17.08211943468705840, 20.13708216824730357, -12.26659068614894466 ) ) ;
#72327 = CARTESIAN_POINT ( 'NONE',  ( 18.52753015748617571, 3.092264484334118269, 4.923371831947298993 ) ) ;
#72328 = CARTESIAN_POINT ( 'NONE',  ( 19.42250999205614193, 30.14701867748817321, 5.440088680355555262 ) ) ;
#72329 = CARTESIAN_POINT ( 'NONE',  ( 5.076628168052703671, 56.84226448433412315, 8.527530157486179263 ) ) ;
#72330 = VECTOR ( 'NONE', #16099, 1000.000000000000000 ) ;
#72331 = CARTESIAN_POINT ( 'NONE',  ( 7.361572987183170547, 52.05059781766745175, 9.846743663894590881 ) ) ;
#72332 = ORIENTED_EDGE ( 'NONE', *, *, #93915, .F. ) ;
#72333 = CYLINDRICAL_SURFACE ( 'NONE', #82855, 0.5000000000000004441 ) ;
#72334 = PRESENTATION_LAYER_ASSIGNMENT (  '', '', ( #16482 ) ) ;
#72335 = CARTESIAN_POINT ( 'NONE',  ( 17.96484262340118221, 51.18868534415483396, -7.964842623401177768 ) ) ;
#72336 = CARTESIAN_POINT ( 'NONE',  ( 10.00000000000000000, 49.75893115100078745, -9.846743663894594434 ) ) ;
#72338 = CARTESIAN_POINT ( 'NONE',  ( 9.779999999999994031, 1.885066177228129719E-15, 2.900000000000000355 ) ) ;
#72337 = CARTESIAN_POINT ( 'NONE',  ( 0.5774900079438607392, 13.48035201082150358, 5.440088680355550821 ) ) ;
#72339 = CARTESIAN_POINT ( 'NONE',  ( 2.035157376598824452, 63.68868534415484106, 7.964842623401179544 ) ) ;
#72340 = CARTESIAN_POINT ( 'NONE',  ( 20.88017736071110875, 10.77201867748817143, -2.915334737309920765 ) ) ;
#72341 = EDGE_CURVE ( 'NONE', #16571, #10746, #21832, .T. ) ;
#72342 = CARTESIAN_POINT ( 'NONE',  ( -2.816281873526473856, 44.33196800326375353, 3.434112377981055619 ) ) ;
#72343 = CARTESIAN_POINT ( 'NONE',  ( 17.96484262340118221, 31.18868534415483751, -7.964842623401177768 ) ) ;
#72344 = DIRECTION ( 'NONE',  ( 0.000000000000000000, -1.000000000000000000, 0.000000000000000000 ) ) ;
#72345 = EDGE_CURVE ( 'NONE', #64921, #20501, #75654, .T. ) ;
#72346 = ORIENTED_EDGE ( 'NONE', *, *, #3302, .F. ) ;
#72347 = CARTESIAN_POINT ( 'NONE',  ( 3.591859063236763294, 38.29030133659708923, -11.09922568453595026 ) ) ;
#72348 = CARTESIAN_POINT ( 'NONE',  ( 4.559911319644449179, 32.23035201082150536, -9.422509992056141925 ) ) ;
#72349 = ORIENTED_EDGE ( 'NONE', *, *, #19545, .F. ) ;
#72350 = CARTESIAN_POINT ( 'NONE',  ( 0.1532563361054100626, 60.80059781766744464, -2.638427012816831230 ) ) ;
#72351 = EDGE_CURVE ( 'NONE', #1450, #76280, #84442, .T. ) ;
#72353 = CARTESIAN_POINT ( 'NONE',  ( 7.361572987183169658, 49.96726448433410894, -9.846743663894592657 ) ) ;
#72352 = CARTESIAN_POINT ( 'NONE',  ( 5.076628168052703671, 11.84226448433411960, 8.527530157486179263 ) ) ;
#72354 = CARTESIAN_POINT ( 'NONE',  ( 0.5774900079438590739, 17.64701867748817321, -5.440088680355550821 ) ) ;
#72355 = CARTESIAN_POINT ( 'NONE',  ( 0.1532563361054100626, 35.80059781766745175, -2.638427012816831230 ) ) ;
#72356 = CARTESIAN_POINT ( 'NONE',  ( 13.48255862861927312, 3.989652714533045580E-16, -5.335786055104159153 ) ) ;
#72357 = LINE ( 'NONE', #86884, #13284 ) ;
#72358 = AXIS2_PLACEMENT_3D ( 'NONE', #17703, #40689, #1239 ) ;
#72360 = CARTESIAN_POINT ( 'NONE',  ( 0.1532563361054082862, 11.21726448433411605, 2.638427012816831674 ) ) ;
#72359 = CARTESIAN_POINT ( 'NONE',  ( 19.84674366389459266, 28.71726448433411960, -2.638427012816827677 ) ) ;
#72361 = CARTESIAN_POINT ( 'NONE',  ( 0.6081133539230624274, 8.337033823263999111, 6.500000000000005329 ) ) ;
#72363 = ORIENTED_EDGE ( 'NONE', *, *, #32933, .F. ) ;
#72362 = CARTESIAN_POINT ( 'NONE',  ( 2.791683348922237240, 65.38393115100078035, -7.208316651077763204 ) ) ;
#72364 = VECTOR ( 'NONE', #97979, 1000.000000000000000 ) ;
#72365 = CARTESIAN_POINT ( 'NONE',  ( 19.88565890683628368, 7.716910754863025801, -6.480892540919851008 ) ) ;
#72366 = CARTESIAN_POINT ( 'NONE',  ( 3.591859063236763294, 38.29030133659708923, -11.09922568453595026 ) ) ;
#72367 = EDGE_CURVE ( 'NONE', #84883, #3732, #67462, .T. ) ;
#72368 = CARTESIAN_POINT ( 'NONE',  ( 7.361572987183169658, 44.96726448433412315, -9.846743663894592657 ) ) ;
#72369 = CARTESIAN_POINT ( 'NONE',  ( 0.1089645850228881108, 8.162345557925705819, 6.479102184480789894 ) ) ;
#72370 = CARTESIAN_POINT ( 'NONE',  ( 6.204703633549690345, 60.76208216824730357, -14.16423886937410259 ) ) ;
#72371 = CARTESIAN_POINT ( 'NONE',  ( 14.92337183194729988, 24.34226448433411960, -8.527530157486177487 ) ) ;
#72372 = VERTEX_POINT ( 'NONE', #475 ) ;
#72373 = CARTESIAN_POINT ( 'NONE',  ( 19.50000000000000711, 79.40087001978916703, 4.999999999999999112 ) ) ;
#72374 = EDGE_CURVE ( 'NONE', #90157, #9521, #90934, .T. ) ;
#72375 = CARTESIAN_POINT ( 'NONE',  ( 6.204703633549690345, 50.76208216824730357, -14.16423886937410259 ) ) ;
#72377 = B_SPLINE_CURVE_WITH_KNOTS ( 'NONE', 3,
 ( #67472, #6971, #90446, #21985, #52460, #37478, #60938, #29946, #60452, #22471, #52947, #83457, #14978, #45449, #75951, #7478, #91449, #22972, #15474, #24444 ),
 .UNSPECIFIED., .F., .F.,
 ( 4, 2, 2, 2, 2, 2, 2, 2, 2, 4 ),
 ( 0.000000000000000000, 0.001321439349356821023, 0.002642878698713642047, 0.003964318048070463070, 0.005285757397427284093, 0.006607196746784105117, 0.007928636096140926140, 0.009250075445497746296, 0.009910795120176157241, 0.01057151479485456819 ),
 .UNSPECIFIED. ) ;
#72376 = CARTESIAN_POINT ( 'NONE',  ( 10.00000000000000178, 57.25893115100078745, 9.846743663894594434 ) ) ;
#72378 = CARTESIAN_POINT ( 'NONE',  ( 12.91533473730992121, 4.522018677488170546, 10.88017736071110164 ) ) ;
#72379 = CARTESIAN_POINT ( 'NONE',  ( 17.08211943468705130, 38.47041550158063217, 12.26659068614894998 ) ) ;
#72380 = CARTESIAN_POINT ( 'NONE',  ( 20.36894250292379382, 33.67874883491396076, 10.36894250292379205 ) ) ;
#72381 = CARTESIAN_POINT ( 'NONE',  ( 14.02068044289381987, 14.49999999999999112, 5.331089937175756077 ) ) ;
#72383 = CARTESIAN_POINT ( 'NONE',  ( 14.92337183194729633, 57.67559781766745886, 8.527530157486181039 ) ) ;
#72382 = CARTESIAN_POINT ( 'NONE',  ( 6.933985542757959308, -73.15302115705439689, 2.499999999997586375 ) ) ;
#72384 = ORIENTED_EDGE ( 'NONE', *, *, #56910, .T. ) ;
#72385 = CARTESIAN_POINT ( 'NONE',  ( 20.88017736071110875, 55.77201867748816966, -2.915334737309920765 ) ) ;
#72386 = CARTESIAN_POINT ( 'NONE',  ( 19.67388484268946058, 90.60256703073459050, -5.439657303569386926 ) ) ;
#72387 = CARTESIAN_POINT ( 'NONE',  ( 1.472469842513823179, 51.42559781766745886, 4.923371831947296329 ) ) ;
#72388 = CARTESIAN_POINT ( 'NONE',  ( 13.43411237798106583, 62.66530133659708923, -12.81628187352647252 ) ) ;
#72389 = CARTESIAN_POINT ( 'NONE',  ( 1.472469842513823179, 56.42559781766745886, 4.923371831947296329 ) ) ;
#72390 = FACE_OUTER_BOUND ( 'NONE', #96481, .T. ) ;
#72391 =( GEOMETRIC_REPRESENTATION_CONTEXT ( 3 ) GLOBAL_UNCERTAINTY_ASSIGNED_CONTEXT ( ( #66475 ) ) GLOBAL_UNIT_ASSIGNED_CONTEXT ( ( #67377, #37392, #14892 ) ) REPRESENTATION_CONTEXT ( 'NONE', 'WORKASPACE' ) );
#72392 = CARTESIAN_POINT ( 'NONE',  ( 24.16423886937410614, 29.30374883491396787, 8.672049930838204340E-16 ) ) ;
#72394 = DIRECTION ( 'NONE',  ( 0.000000000000000000, 0.000000000000000000, -1.000000000000000000 ) ) ;
#72393 = CARTESIAN_POINT ( 'NONE',  ( -3.500000000000000444, 0.09224605989684696306, -2.750000000000000000 ) ) ;
#72396 = AXIS2_PLACEMENT_3D ( 'NONE', #56152, #86155, #3151 ) ;
#72395 = CARTESIAN_POINT ( 'NONE',  ( 4.559911319644449179, 23.89701867748817321, 9.422509992056141925 ) ) ;
#72397 = CARTESIAN_POINT ( 'NONE',  ( 6.565887622018943937, 23.08196800326375708, -12.81628187352647608 ) ) ;
#72398 = DIRECTION ( 'NONE',  ( 0.9969173337331289630, 0.000000000000000000, -0.07845909572783234254 ) ) ;
#72399 = CARTESIAN_POINT ( 'NONE',  ( 2.791683348922240793, 11.63393115100078568, 7.208316651077764092 ) ) ;
#72400 = ORIENTED_EDGE ( 'NONE', *, *, #61197, .T. ) ;
#72401 = AXIS2_PLACEMENT_3D ( 'NONE', #22482, #52956, #53447 ) ;
#72402 = CARTESIAN_POINT ( 'NONE',  ( 6.934035614042552531, -73.16521313705239038, -3.999999999998390177 ) ) ;
#72403 = B_SPLINE_CURVE_WITH_KNOTS ( 'NONE', 3,
 ( #98394, #36381, #89868, #21383, #82362, #53851 ),
 .UNSPECIFIED., .F., .F.,
 ( 4, 2, 4 ),
 ( 0.000000000000000000, 0.0002605067024380873812, 0.0005210134048761747624 ),
 .UNSPECIFIED. ) ;
#72404 = CARTESIAN_POINT ( 'NONE',  ( 2.917880565312948704, 27.63708216824730357, 12.26659068614894643 ) ) ;
#72405 = DIRECTION ( 'NONE',  ( 0.000000000000000000, 0.000000000000000000, -1.000000000000000000 ) ) ;
#72406 = CARTESIAN_POINT ( 'NONE',  ( 4.559911319644449179, 3.897018677488171434, 9.422509992056141925 ) ) ;
#72407 = CARTESIAN_POINT ( 'NONE',  ( -1.354709868695754826, 14.49999999999999112, 14.93870011653156915 ) ) ;
#72408 = CARTESIAN_POINT ( 'NONE',  ( -0.8801773607111009756, 43.06368534415484106, 1.068504757029289695E-15 ) ) ;
#72410 = VECTOR ( 'NONE', #80739, 1000.000000000000000 ) ;
#72409 = CARTESIAN_POINT ( 'NONE',  ( 17.96484262340118221, 31.18868534415483751, -7.964842623401177768 ) ) ;
#72411 = CARTESIAN_POINT ( 'NONE',  ( 13.43411237798105340, 10.58196800326375353, 12.81628187352647963 ) ) ;
#72412 = CARTESIAN_POINT ( 'NONE',  ( 0.6261916924966959286, 0.5000000000000002220, 6.500000000000003553 ) ) ;
#72413 = CARTESIAN_POINT ( 'NONE',  ( 14.92337183194729633, 12.67559781766745353, 8.527530157486181039 ) ) ;
#72414 = CYLINDRICAL_SURFACE ( 'NONE', #81186, 0.2500000000000002220 ) ;
#72415 = CARTESIAN_POINT ( 'NONE',  ( 17.96484262340118221, 39.93868534415484106, 7.964842623401181321 ) ) ;
#72416 = EDGE_CURVE ( 'NONE', #23594, #6107, #6961, .T. ) ;
#72417 = UNCERTAINTY_MEASURE_WITH_UNIT (LENGTH_MEASURE( 1.000000000000000082E-05 ), #64780, 'distance_accuracy_value', 'NONE');
#72418 = CARTESIAN_POINT ( 'NONE',  ( 16.40814093676324603, 2.456968003263753531, -11.09922568453594671 ) ) ;
#72419 = CARTESIAN_POINT ( 'NONE',  ( 17.96484262340118221, 64.93868534415483396, 7.964842623401181321 ) ) ;
#72420 = CARTESIAN_POINT ( 'NONE',  ( 18.52753015748618282, 23.92559781766745530, -4.923371831947291888 ) ) ;
#72421 = CARTESIAN_POINT ( 'NONE',  ( 16.40814093676323893, 40.79030133659708923, 11.09922568453595026 ) ) ;
#72423 = CARTESIAN_POINT ( 'NONE',  ( -6.000000000000009770, 40.99999999999999289, -4.250000000000000000 ) ) ;
#72422 = CARTESIAN_POINT ( 'NONE',  ( 7.084665262690076126, 69.10535201082151957, 10.88017736071109987 ) ) ;
#72424 = ORIENTED_EDGE ( 'NONE', *, *, #50446, .T. ) ;
#72425 = PRESENTATION_STYLE_ASSIGNMENT (( #41477 ) ) ;
#72426 = CYLINDRICAL_SURFACE ( 'NONE', #33448, 0.1000000000000001166 ) ;
#72427 = CARTESIAN_POINT ( 'NONE',  ( 10.00000000000000000, 1.813685344154837731, -10.88017736071110342 ) ) ;
#72429 = CARTESIAN_POINT ( 'NONE',  ( 2.917880565312948704, 22.63708216824730002, 12.26659068614894643 ) ) ;
#72428 = FACE_OUTER_BOUND ( 'NONE', #79892, .T. ) ;
#72430 = CARTESIAN_POINT ( 'NONE',  ( 12.63842701281683922, 24.55059781766745175, -9.846743663894590881 ) ) ;
#72431 = CARTESIAN_POINT ( 'NONE',  ( 17.96484262340118221, 24.93868534415484461, 7.964842623401181321 ) ) ;
#72432 = CARTESIAN_POINT ( 'NONE',  ( -2.266590686148945544, 66.38708216824730357, -7.082119434687050408 ) ) ;
#72433 = ORIENTED_EDGE ( 'NONE', *, *, #78891, .F. ) ;
#72434 = CARTESIAN_POINT ( 'NONE',  ( 2.035157376598824452, 13.68868534415483751, 7.964842623401179544 ) ) ;
#72435 = CARTESIAN_POINT ( 'NONE',  ( 15.44008868035555793, 26.39701867748817321, -9.422509992056140149 ) ) ;
#72436 = CARTESIAN_POINT ( 'NONE',  ( 14.03351048042395632, -0.03417435944610275333, 2.474486531753810059 ) ) ;
#72437 = ORIENTED_EDGE ( 'NONE', *, *, #59750, .T. ) ;
#72438 = CARTESIAN_POINT ( 'NONE',  ( 21.92686044187657046, 27.39664270246083788, -3.195792623639524432 ) ) ;
#72439 = CARTESIAN_POINT ( 'NONE',  ( 17.96484262340118221, 26.18868534415483396, -7.964842623401177768 ) ) ;
#72440 = CARTESIAN_POINT ( 'NONE',  ( 17.20831665107776587, 62.88393115100078745, 7.208316651077764980 ) ) ;
#72441 = DIRECTION ( 'NONE',  ( -0.000000000000000000, -0.000000000000000000, 1.000000000000000000 ) ) ;
#72442 = CARTESIAN_POINT ( 'NONE',  ( 13.43411237798106583, 57.66530133659708923, -12.81628187352647252 ) ) ;
#72443 = CARTESIAN_POINT ( 'NONE',  ( -0.1503990784575328643, 5.127771745786130708, 6.262539305110068177 ) ) ;
#72444 = CARTESIAN_POINT ( 'NONE',  ( 13.79529636645031943, 30.34541550158063927, -14.16423886937409904 ) ) ;
#72445 = CARTESIAN_POINT ( 'NONE',  ( 19.42250999205614548, 40.98035201082150536, -5.440088680355545492 ) ) ;
#72446 = CARTESIAN_POINT ( 'NONE',  ( 12.91533473730993009, 11.60535201082150714, -10.88017736071109987 ) ) ;
#72447 = CARTESIAN_POINT ( 'NONE',  ( 12.63842701281683922, 54.55059781766745175, -9.846743663894590881 ) ) ;
#72448 = DIRECTION ( 'NONE',  ( 0.000000000000000000, 1.000000000000000000, 0.000000000000000000 ) ) ;
#72450 = EDGE_CURVE ( 'NONE', #40259, #33221, #97983, .T. ) ;
#72449 = CARTESIAN_POINT ( 'NONE',  ( 18.52753015748618282, 43.92559781766745175, -4.923371831947291888 ) ) ;
#72451 = LINE ( 'NONE', #11469, #38333 ) ;
#72452 = CARTESIAN_POINT ( 'NONE',  ( 18.52753015748618282, 13.92559781766745175, -4.923371831947291888 ) ) ;
#72453 = CARTESIAN_POINT ( 'NONE',  ( -11.09922568453594316, -30.45969866340291077, 6.408140936763246920 ) ) ;
#72454 = EDGE_LOOP ( 'NONE', ( #85261, #1129, #19332, #51824, #93526, #43540 ) ) ;
#72455 = CARTESIAN_POINT ( 'NONE',  ( 4.559911319644449179, 7.230352010821504471, -9.422509992056141925 ) ) ;
#72456 = CARTESIAN_POINT ( 'NONE',  ( 1.472469842513823179, 5.592264484334118713, -4.923371831947296329 ) ) ;
#72457 = CARTESIAN_POINT ( 'NONE',  ( 17.20831665107776587, 64.13393115100079456, -7.208316651077762316 ) ) ;
#72458 = CARTESIAN_POINT ( 'NONE',  ( 15.44008868035555793, 61.39701867748817676, -9.422509992056140149 ) ) ;
#72460 = CARTESIAN_POINT ( 'NONE',  ( 6.565887622018943937, 48.08196800326375353, -12.81628187352647608 ) ) ;
#72459 = CARTESIAN_POINT ( 'NONE',  ( 4.559911319644449179, 22.23035201082150536, -9.422509992056141925 ) ) ;
#72461 = CARTESIAN_POINT ( 'NONE',  ( 24.16423886937409904, 29.09541550158063572, 3.795296366450317205 ) ) ;
#72462 = FACE_OUTER_BOUND ( 'NONE', #12801, .T. ) ;
#72463 = EDGE_CURVE ( 'NONE', #92371, #42155, #39222, .T. ) ;
#72464 = B_SPLINE_CURVE_WITH_KNOTS ( 'NONE', 3,
 ( #74695, #30167, #60671, #91169, #76177, #7698 ),
 .UNSPECIFIED., .F., .F.,
 ( 4, 2, 4 ),
 ( 3.409110551496077158E-05, 0.0004400426677367853790, 0.0008459942299586099661 ),
 .UNSPECIFIED. ) ;
#72465 = EDGE_CURVE ( 'NONE', #19716, #538, #87257, .T. ) ;
#72466 = CARTESIAN_POINT ( 'NONE',  ( -2.816281873526471635, 53.91530133659709634, -3.434112377981056508 ) ) ;
#72467 = EDGE_CURVE ( 'NONE', #60570, #11086, #82955, .T. ) ;
#72468 = EDGE_LOOP ( 'NONE', ( #29999, #57100, #14007, #22676 ) ) ;
#72469 = CARTESIAN_POINT ( 'NONE',  ( 6.565887622018943937, 3.081968003263753531, -12.81628187352647608 ) ) ;
#72470 = FILL_AREA_STYLE_COLOUR ( '', #36185 ) ;
#72471 = CARTESIAN_POINT ( 'NONE',  ( 17.96484262340118221, 29.93868534415484106, 7.964842623401181321 ) ) ;
#72472 = CARTESIAN_POINT ( 'NONE',  ( -10.44999999999999751, 99.99999999999998579, -8.525133428036873795 ) ) ;
#72473 = TOROIDAL_SURFACE ( 'NONE', #35802, 14.49999999999999822, 0.5000000000000000000 ) ;
#72474 = ORIENTED_EDGE ( 'NONE', *, *, #31618, .T. ) ;
#72475 = CARTESIAN_POINT ( 'NONE',  ( 19.84674366389459266, 8.717264484334116048, -2.638427012816827677 ) ) ;
#72476 = CARTESIAN_POINT ( 'NONE',  ( 17.20831665107776587, 9.133931151000787452, -7.208316651077762316 ) ) ;
#72477 = CARTESIAN_POINT ( 'NONE',  ( 18.52753015748617571, 23.09226448433411960, 4.923371831947298993 ) ) ;
#72478 = CARTESIAN_POINT ( 'NONE',  ( 19.84674366389459621, 13.50893115100078568, 7.409399052514197653E-17 ) ) ;
#72479 = CARTESIAN_POINT ( 'NONE',  ( 0.1532563361054082862, 1.217264484334117824, 2.638427012816831674 ) ) ;
#72481 = CARTESIAN_POINT ( 'NONE',  ( 14.48718990079892599, 4.585916678612670543E-16, -0.6093675230840440715 ) ) ;
#72480 = CARTESIAN_POINT ( 'NONE',  ( 7.084665262690076126, 54.10535201082151247, 10.88017736071109987 ) ) ;
#72482 = CARTESIAN_POINT ( 'NONE',  ( 10.00000000000000000, 56.81368534415484106, -10.88017736071110342 ) ) ;
#72484 = ORIENTED_EDGE ( 'NONE', *, *, #89151, .F. ) ;
#72483 = CARTESIAN_POINT ( 'NONE',  ( 5.076628168052704559, 25.17559781766745175, -8.527530157486179263 ) ) ;
#72485 = CARTESIAN_POINT ( 'NONE',  ( 5.806616290881322584, 15.00000000000000533, 13.42355087257366364 ) ) ;
#72486 = CARTESIAN_POINT ( 'NONE',  ( 1.472469842513823179, 60.59226448433412315, -4.923371831947296329 ) ) ;
#72487 = EDGE_LOOP ( 'NONE', ( #10466, #18369, #52079, #91176 ) ) ;
#72488 = ORIENTED_EDGE ( 'NONE', *, *, #17104, .T. ) ;
#72489 = CARTESIAN_POINT ( 'NONE',  ( 17.96484262340118221, 4.938685344154837509, 7.964842623401181321 ) ) ;
#72490 = CARTESIAN_POINT ( 'NONE',  ( 24.16423886937410614, 24.51208216824730002, -3.795296366450302550 ) ) ;
#72491 = UNCERTAINTY_MEASURE_WITH_UNIT (LENGTH_MEASURE( 1.000000000000000082E-05 ), #98428, 'distance_accuracy_value', 'NONE');
#72492 = CYLINDRICAL_SURFACE ( 'NONE', #67908, 0.5000000000000004441 ) ;
#72493 = EDGE_CURVE ( 'NONE', #13062, #16387, #61700, .T. ) ;
#72494 = CARTESIAN_POINT ( 'NONE',  ( -4.164238869374098151, 11.59541550158063217, -3.795296366450310543 ) ) ;
#72495 = CARTESIAN_POINT ( 'NONE',  ( 20.36894250292379382, 33.67874883491396076, 10.36894250292379205 ) ) ;
#72496 = LINE ( 'NONE', #65488, #27454 ) ;
#72497 = CARTESIAN_POINT ( 'NONE',  ( 15.44008868035555260, 39.73035201082150536, 9.422509992056143702 ) ) ;
#72498 =( NAMED_UNIT ( * ) PLANE_ANGLE_UNIT ( ) SI_UNIT ( $, .RADIAN. ) );
#72499 = ORIENTED_EDGE ( 'NONE', *, *, #37042, .T. ) ;
#72500 = CARTESIAN_POINT ( 'NONE',  ( 10.00000000000000000, 14.75893115100078568, -9.846743663894594434 ) ) ;
#72502 = CARTESIAN_POINT ( 'NONE',  ( 7.361572987183169658, 19.96726448433411960, -9.846743663894592657 ) ) ;
#72501 = CARTESIAN_POINT ( 'NONE',  ( 7.084665262690076126, 57.02201867748817676, -10.88017736071110164 ) ) ;
#72503 = CARTESIAN_POINT ( 'NONE',  ( 10.00000000000000000, 6.813685344154838397, -10.88017736071110342 ) ) ;
#72504 = CARTESIAN_POINT ( 'NONE',  ( 16.40814093676323893, 50.79030133659708923, 11.09922568453595026 ) ) ;
#72505 = CARTESIAN_POINT ( 'NONE',  ( 7.361572987183170547, 42.05059781766745886, 9.846743663894590881 ) ) ;
#72506 = CARTESIAN_POINT ( 'NONE',  ( -3.250000000000000444, 1.019547802438453887, 2.750000000000000444 ) ) ;
#72507 = CARTESIAN_POINT ( 'NONE',  ( 21.09922568453595559, 27.04030133659708568, -6.408140936763230044 ) ) ;
#72508 = FACE_OUTER_BOUND ( 'NONE', #58753, .T. ) ;
#72509 = CARTESIAN_POINT ( 'NONE',  ( 0.1532563361054100626, 25.80059781766744820, -2.638427012816831230 ) ) ;
#72510 = CARTESIAN_POINT ( 'NONE',  ( 24.16423886937410614, 9.512082168247301794, -3.795296366450302550 ) ) ;
#72511 = VERTEX_POINT ( 'NONE', #8433 ) ;
#72512 = EDGE_LOOP ( 'NONE', ( #74453, #1292, #19262 ) ) ;
#72513 = CARTESIAN_POINT ( 'NONE',  ( -0.8801773607110991993, 52.85535201082151247, -2.915334737309923874 ) ) ;
#72514 = CARTESIAN_POINT ( 'NONE',  ( 7.084665262690076126, 52.02201867748816255, -10.88017736071110164 ) ) ;
#72515 = CARTESIAN_POINT ( 'NONE',  ( 6.204703633549690345, 47.84541550158064638, 14.16423886937410082 ) ) ;
#72516 = CARTESIAN_POINT ( 'NONE',  ( 12.63842701281683922, 59.55059781766744464, -9.846743663894590881 ) ) ;
#72517 = CARTESIAN_POINT ( 'NONE',  ( 0.1532563361054082862, 16.21726448433411960, 2.638427012816831674 ) ) ;
#72518 = DIRECTION ( 'NONE',  ( 0.000000000000000000, 0.000000000000000000, -1.000000000000000000 ) ) ;
#72519 = CARTESIAN_POINT ( 'NONE',  ( 20.88017736071110164, 45.35535201082149115, 2.915334737309930979 ) ) ;
#72520 = DIRECTION ( 'NONE',  ( 0.000000000000000000, 0.000000000000000000, 1.000000000000000000 ) ) ;
#72521 = CARTESIAN_POINT ( 'NONE',  ( -1.099225684535947600, 23.70696800326375708, -6.408140936763238038 ) ) ;
#72522 = CARTESIAN_POINT ( 'NONE',  ( 2.791683348922240793, 56.63393115100078035, 7.208316651077764092 ) ) ;
#72523 = CARTESIAN_POINT ( 'NONE',  ( 10.88017736071110164, 10.35535201082150181, 2.915334737309921209 ) ) ;
#72524 = CARTESIAN_POINT ( 'NONE',  ( 20.88017736071110519, 65.56368534415483396, 2.639326808657452039E-16 ) ) ;
#72525 = CARTESIAN_POINT ( 'NONE',  ( 7.084665262690076126, 7.022018677488169658, -10.88017736071110164 ) ) ;
#72526 = CARTESIAN_POINT ( 'NONE',  ( 5.076628168052703671, 1.842264484334118047, 8.527530157486179263 ) ) ;
#72527 = CARTESIAN_POINT ( 'NONE',  ( 17.96484262340118221, 64.93868534415483396, 7.964842623401181321 ) ) ;
#72528 = DIRECTION ( 'NONE',  ( 0.000000000000000000, 0.000000000000000000, 1.000000000000000000 ) ) ;
#72529 = VECTOR ( 'NONE', #7471, 999.9999999999998863 ) ;
#72530 = CARTESIAN_POINT ( 'NONE',  ( 7.361572987183170547, 37.05059781766744464, 9.846743663894590881 ) ) ;
#72531 = CARTESIAN_POINT ( 'NONE',  ( 20.88017736071110875, 20.77201867748816611, -2.915334737309920765 ) ) ;
#72532 = CARTESIAN_POINT ( 'NONE',  ( 0.1532563361054083140, 61.00893115100078745, 1.131784320476157264E-15 ) ) ;
#72534 = DIRECTION ( 'NONE',  ( -3.907985046680551022E-14, 0.000000000000000000, 1.000000000000000000 ) ) ;
#72533 = CARTESIAN_POINT ( 'NONE',  ( 0.5774900079438607392, 33.48035201082150536, 5.440088680355550821 ) ) ;
#72535 = CARTESIAN_POINT ( 'NONE',  ( 0.000000000000000000, 0.5000000000000004441, 0.000000000000000000 ) ) ;
#72536 = CARTESIAN_POINT ( 'NONE',  ( 19.38216949554541557, 37.24863466993041783, -9.382169495545420901 ) ) ;
#72537 = ORIENTED_EDGE ( 'NONE', *, *, #83383, .T. ) ;
#72538 = CARTESIAN_POINT ( 'NONE',  ( 12.91533473730992121, 54.52201867748816255, 10.88017736071110164 ) ) ;
#72539 = CIRCLE ( 'NONE', #16679, 14.49999999999999822 ) ;
#72541 = FACE_OUTER_BOUND ( 'NONE', #38592, .T. ) ;
#72540 = CARTESIAN_POINT ( 'NONE',  ( 21.09922568453595559, 17.04030133659708923, -6.408140936763230044 ) ) ;
#72542 = CARTESIAN_POINT ( 'NONE',  ( 0.1532563361054082862, 1.217264484334117824, 2.638427012816831674 ) ) ;
#72543 = CARTESIAN_POINT ( 'NONE',  ( 10.00000000000000178, 24.31368534415484106, 10.88017736071110342 ) ) ;
#72544 = CARTESIAN_POINT ( 'NONE',  ( 10.00000000000000178, 58.05374883491397497, 14.16423886937410082 ) ) ;
#72545 = CARTESIAN_POINT ( 'NONE',  ( 7.361572987183170547, 47.05059781766745175, 9.846743663894590881 ) ) ;
#72546 = CARTESIAN_POINT ( 'NONE',  ( 14.92337183194729633, 7.675597817667451750, 8.527530157486181039 ) ) ;
#72547 = CARTESIAN_POINT ( 'NONE',  ( 19.42250999205614193, 60.14701867748817676, 5.440088680355555262 ) ) ;
#72548 = DIRECTION ( 'NONE',  ( -0.000000000000000000, -1.000000000000000000, -0.000000000000000000 ) ) ;
#72549 = CARTESIAN_POINT ( 'NONE',  ( 22.26659068614894466, 23.88708216824730357, 7.082119434687054849 ) ) ;
#72550 = ADVANCED_FACE ( 'NONE', ( #83939 ), #45948, .F. ) ;
#72551 = B_SPLINE_CURVE_WITH_KNOTS ( 'NONE', 3,
 ( #71917, #80900, #94419, #18436, #34893, #4427 ),
 .UNSPECIFIED., .F., .F.,
 ( 4, 2, 4 ),
 ( 0.0002800138956475372188, 0.0006862192609879400919, 0.001092424626328342965 ),
 .UNSPECIFIED. ) ;
#72552 = PLANE ( 'NONE',  #81622 ) ;
#72553 = CARTESIAN_POINT ( 'NONE',  ( -3.586264863366058542, -2.711807932106038876, -3.750000000000000000 ) ) ;
#72554 = VERTEX_POINT ( 'NONE', #16433 ) ;
#72555 = ORIENTED_EDGE ( 'NONE', *, *, #18341, .T. ) ;
#72556 = CARTESIAN_POINT ( 'NONE',  ( -0.3689425029237881626, 42.42874883491396787, 10.36894250292379027 ) ) ;
#72557 = CARTESIAN_POINT ( 'NONE',  ( -0.3689425029237881626, 47.42874883491396787, 10.36894250292379027 ) ) ;
#72558 = CARTESIAN_POINT ( 'NONE',  ( 12.63842701281683922, 14.55059781766744997, -9.846743663894590881 ) ) ;
#72559 = CARTESIAN_POINT ( 'NONE',  ( -2.816281873526473856, 14.33196800326375531, 3.434112377981055619 ) ) ;
#72560 = DIRECTION ( 'NONE',  ( 0.000000000000000000, 0.8042198116157012189, -0.5943319733993840392 ) ) ;
#72562 = CARTESIAN_POINT ( 'NONE',  ( -1.099225684535947600, 49.54030133659708923, 6.408140936763237150 ) ) ;
#72561 = CARTESIAN_POINT ( 'NONE',  ( 17.96484262340118221, 6.188685344154836621, -7.964842623401177768 ) ) ;
#72563 = CARTESIAN_POINT ( 'NONE',  ( 6.204703633549690345, 37.84541550158063927, 14.16423886937410082 ) ) ;
#72564 = CARTESIAN_POINT ( 'NONE',  ( 12.63842701281683922, 4.550597817667451750, -9.846743663894590881 ) ) ;
#72565 = CARTESIAN_POINT ( 'NONE',  ( -9.846743663894590881, 1.217264484334116492, 2.638427012816840111 ) ) ;
#72566 = VERTEX_POINT ( 'NONE', #46429 ) ;
#72567 = SURFACE_SIDE_STYLE ('',( #63597 ) ) ;
#72568 = CARTESIAN_POINT ( 'NONE',  ( 18.52753015748617571, 13.09226448433411960, 4.923371831947298993 ) ) ;
#72570 = EDGE_CURVE ( 'NONE', #38899, #75564, #46911, .T. ) ;
#72569 =( LENGTH_UNIT ( ) NAMED_UNIT ( * ) SI_UNIT ( .MILLI., .METRE. ) );
#72571 = VERTEX_POINT ( 'NONE', #38940 ) ;
#72572 = CARTESIAN_POINT ( 'NONE',  ( 2.917880565312950480, 10.97041550158063572, -12.26659068614894821 ) ) ;
#72574 = CARTESIAN_POINT ( 'NONE',  ( -0.8801773607111008646, 28.27201867748817321, 2.915334737309923430 ) ) ;
#72573 = CARTESIAN_POINT ( 'NONE',  ( 4.559911319644449179, 2.230352010821504916, -9.422509992056141925 ) ) ;
#72576 = CARTESIAN_POINT ( 'NONE',  ( 3.591859063236761518, -0.04303199673624671928, 11.09922568453594849 ) ) ;
#72575 = CARTESIAN_POINT ( 'NONE',  ( 5.076628168052704559, 55.17559781766745175, -8.527530157486179263 ) ) ;
#72577 = CARTESIAN_POINT ( 'NONE',  ( 0.000000000000000000, 0.000000000000000000, 0.000000000000000000 ) ) ;
#72578 = AXIS2_PLACEMENT_3D ( 'NONE', #86230, #1283, #17741 ) ;
#72579 = ADVANCED_FACE ( 'NONE', ( #39918 ), #17053, .T. ) ;
#72580 = B_SPLINE_CURVE_WITH_KNOTS ( 'NONE', 3,
 ( #23542, #77009, #8521, #52049, #16523, #40001 ),
 .UNSPECIFIED., .F., .F.,
 ( 4, 2, 4 ),
 ( 3.409110551494299067E-05, 0.0004400426677367894448, 0.0008459942299586358785 ),
 .UNSPECIFIED. ) ;
#72581 = CARTESIAN_POINT ( 'NONE',  ( 21.09922568453595559, 12.04030133659708746, -6.408140936763230044 ) ) ;
#72582 = ADVANCED_FACE ( 'NONE', ( #48878 ), #36161, .T. ) ;
#72583 = VERTEX_POINT ( 'NONE', #78894 ) ;
#72584 = CARTESIAN_POINT ( 'NONE',  ( 2.917880565312950480, 55.97041550158063217, -12.26659068614894821 ) ) ;
#72585 = EDGE_LOOP ( 'NONE', ( #73217, #1098, #79639, #89416 ) ) ;
#72586 = CARTESIAN_POINT ( 'NONE',  ( 10.00000000000000178, 58.05374883491397497, 14.16423886937410082 ) ) ;
#72587 = ORIENTED_EDGE ( 'NONE', *, *, #50275, .T. ) ;
#72588 = CARTESIAN_POINT ( 'NONE',  ( 0.5774900079438590739, 32.64701867748816966, -5.440088680355550821 ) ) ;
#72589 = CARTESIAN_POINT ( 'NONE',  ( 7.084665262690076126, 39.10535201082150536, 10.88017736071109987 ) ) ;
#72590 = CARTESIAN_POINT ( 'NONE',  ( 4.559911319644449179, 48.89701867748817676, 9.422509992056141925 ) ) ;
#72591 = DIRECTION ( 'NONE',  ( 0.000000000000000000, 0.000000000000000000, 1.000000000000000000 ) ) ;
#72592 = CARTESIAN_POINT ( 'NONE',  ( 20.88017736071110519, 45.56368534415484106, 2.639326808657452039E-16 ) ) ;
#72594 = VERTEX_POINT ( 'NONE', #40910 ) ;
#72593 = DIRECTION ( 'NONE',  ( -0.000000000000000000, -0.000000000000000000, -1.000000000000000000 ) ) ;
#72595 = PRESENTATION_LAYER_ASSIGNMENT (  '', '', ( #67848 ) ) ;
#72596 = CARTESIAN_POINT ( 'NONE',  ( 17.20831665107776587, 17.88393115100078745, 7.208316651077764980 ) ) ;
#72597 = EDGE_LOOP ( 'NONE', ( #80681, #91048, #46942, #48829 ) ) ;
#72598 = CARTESIAN_POINT ( 'NONE',  ( 11.19532980483368867, -77.48602862273223479, 4.000000000000000000 ) ) ;
#72599 = CARTESIAN_POINT ( 'NONE',  ( 14.92337183194729633, 52.67559781766745175, 8.527530157486181039 ) ) ;
#72600 = MECHANICAL_DESIGN_GEOMETRIC_PRESENTATION_REPRESENTATION (  '', ( #78979 ), #67852 ) ;
#72601 = CARTESIAN_POINT ( 'NONE',  ( 21.09922568453594849, 61.20696800326376064, 6.408140936763242479 ) ) ;
#72602 = EDGE_CURVE ( 'NONE', #4006, #45903, #71292, .T. ) ;
#72603 = LINE ( 'NONE', #27107, #52355 ) ;
#72604 = LINE ( 'NONE', #87614, #38029 ) ;
#72605 = DIRECTION ( 'NONE',  ( 1.000000000000000000, 0.000000000000000000, 0.000000000000000000 ) ) ;
#72606 = CARTESIAN_POINT ( 'NONE',  ( 17.75000000000000355, 78.80384757729336798, 3.750000000000000000 ) ) ;
#72607 = CARTESIAN_POINT ( 'NONE',  ( 2.917880565312948704, 62.63708216824730357, 12.26659068614894643 ) ) ;
#72608 = LINE ( 'NONE', #40664, #75414 ) ;
#72609 = ORIENTED_EDGE ( 'NONE', *, *, #6234, .F. ) ;
#72610 = CARTESIAN_POINT ( 'NONE',  ( 0.000000000000000000, 70.00000000000000000, -6.000000000000000000 ) ) ;
#72611 = CARTESIAN_POINT ( 'NONE',  ( 19.84674366389459266, 38.30059781766745175, 2.638427012816836559 ) ) ;
#72612 = CARTESIAN_POINT ( 'NONE',  ( -2.816281873526473856, 59.12363466993042493, 9.499525473075851096E-16 ) ) ;
#72613 = CARTESIAN_POINT ( 'NONE',  ( 3.591859063236761518, -0.04303199673624671928, 11.09922568453594849 ) ) ;
#72614 = CARTESIAN_POINT ( 'NONE',  ( 20.88017736071110875, 65.77201867748817676, -2.915334737309920765 ) ) ;
#72615 = DIRECTION ( 'NONE',  ( 0.000000000000000000, 0.000000000000000000, 1.000000000000000000 ) ) ;
#72616 = CARTESIAN_POINT ( 'NONE',  ( 7.361572987183170547, 12.05059781766744997, 9.846743663894590881 ) ) ;
#72617 = CARTESIAN_POINT ( 'NONE',  ( 10.00000000000000000, 59.75893115100078745, -9.846743663894594434 ) ) ;
#72618 = DIRECTION ( 'NONE',  ( -0.000000000000000000, -0.000000000000000000, -1.000000000000000000 ) ) ;
#72619 = TOROIDAL_SURFACE ( 'NONE', #5573, 14.49999999999999822, 0.5000000000000000000 ) ;
#72620 = ORIENTED_EDGE ( 'NONE', *, *, #17361, .T. ) ;
#72621 = CARTESIAN_POINT ( 'NONE',  ( 15.44008868035555793, 16.39701867748817321, -9.422509992056140149 ) ) ;
#72622 = CARTESIAN_POINT ( 'NONE',  ( 22.26659068614895176, 4.720415501580633943, -7.082119434687042414 ) ) ;
#72623 = CARTESIAN_POINT ( 'NONE',  ( 7.361572987183169658, 9.967264484334119601, -9.846743663894592657 ) ) ;
#72624 = CARTESIAN_POINT ( 'NONE',  ( 17.96484262340118221, 41.18868534415484106, -7.964842623401177768 ) ) ;
#72626 = CARTESIAN_POINT ( 'NONE',  ( 15.44008868035555793, 66.39701867748817676, -9.422509992056140149 ) ) ;
#72625 = CARTESIAN_POINT ( 'NONE',  ( 6.565887622018943937, 23.08196800326375708, -12.81628187352647608 ) ) ;
#72627 = CARTESIAN_POINT ( 'NONE',  ( 4.469999999999999751, 36.75000000000000000, 3.750000000000000000 ) ) ;
#72628 = CARTESIAN_POINT ( 'NONE',  ( -24.42076923076924189, 85.65384615384614619, -9.500000000000000000 ) ) ;
#72629 = LINE ( 'NONE', #37127, #26453 ) ;
#72630 = CARTESIAN_POINT ( 'NONE',  ( 5.076628168052703671, 56.84226448433412315, 8.527530157486179263 ) ) ;
#72631 = CARTESIAN_POINT ( 'NONE',  ( 2.791683348922237240, 15.38393115100078212, -7.208316651077763204 ) ) ;
#72632 = CARTESIAN_POINT ( 'NONE',  ( -7.964842623401172439, -21.31131465584516249, 7.964842623401183097 ) ) ;
#72633 = CARTESIAN_POINT ( 'NONE',  ( 19.38216949554541557, 17.24863466993041783, -9.382169495545420901 ) ) ;
#72634 = CARTESIAN_POINT ( 'NONE',  ( -10.77730536144846774, -98.63085534186637915, -3.999999999999996447 ) ) ;
#72635 = CARTESIAN_POINT ( 'NONE',  ( 0.5774900079438607392, 23.48035201082150536, 5.440088680355550821 ) ) ;
#72636 = CARTESIAN_POINT ( 'NONE',  ( -1.915564264621539392, 15.00000000000000000, 14.37291249357986445 ) ) ;
#72637 = AXIS2_PLACEMENT_3D ( 'NONE', #8553, #39052, #31035 ) ;
#72638 = CARTESIAN_POINT ( 'NONE',  ( 22.26659068614895176, 49.72041550158063927, -7.082119434687042414 ) ) ;
#72639 = CARTESIAN_POINT ( 'NONE',  ( 6.910406350442640289, -84.29253233655508382, -3.750000000000000444 ) ) ;
#72640 = CARTESIAN_POINT ( 'NONE',  ( 17.20831665107776587, 44.13393115100078745, -7.208316651077762316 ) ) ;
#72641 = CARTESIAN_POINT ( 'NONE',  ( 22.81628187352647785, 36.62363466993041783, 6.195893100308588602E-16 ) ) ;
#72642 = CARTESIAN_POINT ( 'NONE',  ( 20.88017736071110875, 30.77201867748816966, -2.915334737309920765 ) ) ;
#72643 = CARTESIAN_POINT ( 'NONE',  ( 12.63842701281683922, 49.55059781766744464, -9.846743663894590881 ) ) ;
#72644 = CARTESIAN_POINT ( 'NONE',  ( 17.96484262340118221, 46.18868534415484106, -7.964842623401177768 ) ) ;
#72645 = CARTESIAN_POINT ( 'NONE',  ( 21.09922568453594849, 11.20696800326375531, 6.408140936763242479 ) ) ;
#72646 = CARTESIAN_POINT ( 'NONE',  ( 24.16423886937409904, 39.09541550158062506, 3.795296366450317205 ) ) ;
#72647 = CARTESIAN_POINT ( 'NONE',  ( 5.500000000000000000, 11.00000000000000000, -5.000000000000000000 ) ) ;
#72648 = CARTESIAN_POINT ( 'NONE',  ( 17.20831665107776587, 22.88393115100078745, 7.208316651077764980 ) ) ;
#72649 = CARTESIAN_POINT ( 'NONE',  ( -2.816281873526471635, 63.91530133659708923, -3.434112377981056508 ) ) ;
#72650 = CARTESIAN_POINT ( 'NONE',  ( 17.20831665107776587, 64.13393115100079456, -7.208316651077762316 ) ) ;
#72651 = ORIENTED_EDGE ( 'NONE', *, *, #30401, .F. ) ;
#72652 = LINE ( 'NONE', #64652, #3035 ) ;
#72653 = CARTESIAN_POINT ( 'NONE',  ( 6.533420211785746723, -50.31490269211863620, 2.750000000000000000 ) ) ;
#72654 = CARTESIAN_POINT ( 'NONE',  ( 20.88017736071110519, 20.56368534415484106, 2.639326808657452039E-16 ) ) ;
#72655 = CARTESIAN_POINT ( 'NONE',  ( 6.204703633549690345, 30.76208216824730357, -14.16423886937410259 ) ) ;
#72656 = ADVANCED_FACE ( 'NONE', ( #55907, #9416 ), #94876, .T. ) ;
#72657 = CARTESIAN_POINT ( 'NONE',  ( 20.88017736071110519, 65.56368534415483396, 2.639326808657452039E-16 ) ) ;
#72658 = CARTESIAN_POINT ( 'NONE',  ( 19.84674366389459266, 53.30059781766744464, 2.638427012816836559 ) ) ;
#72659 = CARTESIAN_POINT ( 'NONE',  ( 0.5774900079438590739, 37.64701867748817676, -5.440088680355550821 ) ) ;
#72660 = LINE ( 'NONE', #49665, #28797 ) ;
#72661 = CARTESIAN_POINT ( 'NONE',  ( -27.43587634952537968, 0.5000000000000038858, 9.500000000000000000 ) ) ;
#72662 = B_SPLINE_CURVE_WITH_KNOTS ( 'NONE', 3,
 ( #76888, #47372, #23910, #61389, #91898, #84410 ),
 .UNSPECIFIED., .F., .F.,
 ( 4, 2, 4 ),
 ( 0.0002800026249563253040, 0.0006862078800502578041, 0.001092413135144190304 ),
 .UNSPECIFIED. ) ;
#72663 = EDGE_CURVE ( 'NONE', #25669, #95488, #10403, .T. ) ;
#72664 = ORIENTED_EDGE ( 'NONE', *, *, #49558, .F. ) ;
#72665 = CARTESIAN_POINT ( 'NONE',  ( -4.841283923550251167, 0.2306972965111909746, -14.13506365971153222 ) ) ;
#72666 = ORIENTED_EDGE ( 'NONE', *, *, #18651, .T. ) ;
#72667 = ORIENTED_EDGE ( 'NONE', *, *, #51090, .T. ) ;
#72668 = LINE ( 'NONE', #80682, #37380 ) ;
#72669 = CARTESIAN_POINT ( 'NONE',  ( 13.79529636645030344, 13.26208216824729824, 14.16423886937410614 ) ) ;
#72670 = CARTESIAN_POINT ( 'NONE',  ( 24.16423886937410614, 4.512082168247300906, -3.795296366450302550 ) ) ;
#72671 = AXIS2_PLACEMENT_3D ( 'NONE', #65731, #97255, #50749 ) ;
#72672 = CARTESIAN_POINT ( 'NONE',  ( 17.08211943468705840, 55.13708216824731068, -12.26659068614894466 ) ) ;
#72673 = CARTESIAN_POINT ( 'NONE',  ( 17.20831665107776587, 57.88393115100078745, 7.208316651077764980 ) ) ;
#72674 = CARTESIAN_POINT ( 'NONE',  ( 1.472469842513823179, 30.59226448433411960, -4.923371831947296329 ) ) ;
#72675 = CARTESIAN_POINT ( 'NONE',  ( 10.00000000000000178, 65.37363466993042493, 12.81628187352647608 ) ) ;
#72677 = CARTESIAN_POINT ( 'NONE',  ( -1.099225684535947600, -1.293031996736246469, -6.408140936763238038 ) ) ;
#72676 = CARTESIAN_POINT ( 'NONE',  ( 19.42250999205614548, 35.98035201082151247, -5.440088680355545492 ) ) ;
#72678 = CARTESIAN_POINT ( 'NONE',  ( -2.266590686148945544, 51.38708216824730357, -7.082119434687050408 ) ) ;
#72679 = VECTOR ( 'NONE', #80369, 1000.000000000000114 ) ;
#72680 = CARTESIAN_POINT ( 'NONE',  ( 20.88017736071110164, 5.355352010821503583, 2.915334737309930979 ) ) ;
#72681 = CARTESIAN_POINT ( 'NONE',  ( 19.05914839598884924, 4.966938638839758724, 6.499999999999964473 ) ) ;
#72682 = FACE_OUTER_BOUND ( 'NONE', #62292, .T. ) ;
#72683 = CARTESIAN_POINT ( 'NONE',  ( -2.638427012816840111, -35.03273551566588395, -9.846743663894590881 ) ) ;
#72684 = ORIENTED_EDGE ( 'NONE', *, *, #27998, .F. ) ;
#72685 = DIRECTION ( 'NONE',  ( -0.000000000000000000, -0.000000000000000000, -1.000000000000000000 ) ) ;
#72686 = ORIENTED_EDGE ( 'NONE', *, *, #58130, .F. ) ;
#72687 = CARTESIAN_POINT ( 'NONE',  ( 0.1532563361054100626, 20.80059781766744464, -2.638427012816831230 ) ) ;
#72688 = ORIENTED_EDGE ( 'NONE', *, *, #83458, .F. ) ;
#72689 = CARTESIAN_POINT ( 'NONE',  ( 6.204703633549690345, 35.76208216824729647, -14.16423886937410259 ) ) ;
#72690 = CARTESIAN_POINT ( 'NONE',  ( 7.361572987183169658, 34.96726448433411605, -9.846743663894592657 ) ) ;
#72691 = CARTESIAN_POINT ( 'NONE',  ( 0.5774900079438607392, 53.48035201082151247, 5.440088680355550821 ) ) ;
#72692 = CARTESIAN_POINT ( 'NONE',  ( 20.03743638938529159, 36.75197528031017669, 6.399506433553890261 ) ) ;
#72693 = CARTESIAN_POINT ( 'NONE',  ( 17.96484262340118221, 49.93868534415484106, 7.964842623401181321 ) ) ;
#72694 = ADVANCED_FACE ( 'NONE', ( #39434 ), #93684, .T. ) ;
#72695 = AXIS2_PLACEMENT_3D ( 'NONE', #91733, #15263, #53730 ) ;
#72696 = CARTESIAN_POINT ( 'NONE',  ( 16.40814093676323893, 55.79030133659708923, 11.09922568453595026 ) ) ;
#72697 = CARTESIAN_POINT ( 'NONE',  ( 6.408140936763236262, 7.456968003263758860, -11.09922568453595026 ) ) ;
#72698 = ADVANCED_FACE ( 'NONE', ( #2926 ), #68152, .T. ) ;
#72699 = ORIENTED_EDGE ( 'NONE', *, *, #28024, .F. ) ;
#72700 = CARTESIAN_POINT ( 'NONE',  ( -4.164238869374098151, 16.59541550158063927, -3.795296366450310543 ) ) ;
#72701 = ORIENTED_EDGE ( 'NONE', *, *, #20806, .F. ) ;
#72702 = CARTESIAN_POINT ( 'NONE',  ( 0.6178305044545818747, 48.49863466993042493, -9.382169495545419124 ) ) ;
#72703 = CARTESIAN_POINT ( 'NONE',  ( 0.5774900079438590739, 17.64701867748817321, -5.440088680355550821 ) ) ;
#72704 = CARTESIAN_POINT ( 'NONE',  ( 12.63842701281683922, 19.55059781766745175, -9.846743663894590881 ) ) ;
#72705 = CARTESIAN_POINT ( 'NONE',  ( -0.8801773607111008646, 18.27201867748817321, 2.915334737309923430 ) ) ;
#72706 = CARTESIAN_POINT ( 'NONE',  ( 0.6178305044545838731, 59.74863466993041783, 9.382169495545420901 ) ) ;
#72707 = FACE_OUTER_BOUND ( 'NONE', #84444, .T. ) ;
#72708 = CARTESIAN_POINT ( 'NONE',  ( 2.791683348922237240, 30.38393115100078390, -7.208316651077763204 ) ) ;
#72709 = VECTOR ( 'NONE', #80875, 1000.000000000000114 ) ;
#72710 = CARTESIAN_POINT ( 'NONE',  ( 21.92686044187657046, 22.39664270246083788, -3.195792623639524432 ) ) ;
#72711 = AXIS2_PLACEMENT_3D ( 'NONE', #30720, #8242, #52738 ) ;
#72713 = EDGE_CURVE ( 'NONE', #42602, #66663, #28165, .T. ) ;
#72712 = FACE_OUTER_BOUND ( 'NONE', #74798, .T. ) ;
#72714 = CARTESIAN_POINT ( 'NONE',  ( 0.000000000000000000, 0.000000000000000000, 0.000000000000000000 ) ) ;
#72715 = ADVANCED_FACE ( 'NONE', ( #17908 ), #10625, .T. ) ;
#72716 = CARTESIAN_POINT ( 'NONE',  ( 13.75543905097463337, 0.04962897369418881044, 5.333404663735670681 ) ) ;
#72717 = CARTESIAN_POINT ( 'NONE',  ( 10.00000000000000000, 4.758931151000784787, -9.846743663894594434 ) ) ;
#72718 = CARTESIAN_POINT ( 'NONE',  ( 13.43411237798106583, 17.66530133659708923, -12.81628187352647252 ) ) ;
#72719 = LINE ( 'NONE', #50219, #54630 ) ;
#72720 = ADVANCED_FACE ( 'NONE', ( #47895, #32398 ), #54901, .T. ) ;
#72721 = CARTESIAN_POINT ( 'NONE',  ( 5.076628168052704559, 45.17559781766745175, -8.527530157486179263 ) ) ;
#72722 = CARTESIAN_POINT ( 'NONE',  ( -10.53011945866294852, -98.59345040283277228, -3.750000000000000000 ) ) ;
#72723 = CARTESIAN_POINT ( 'NONE',  ( 2.917880565312948704, 17.63708216824730357, 12.26659068614894643 ) ) ;
#72724 = CARTESIAN_POINT ( 'NONE',  ( 1.472469842513823179, 30.59226448433411960, -4.923371831947296329 ) ) ;
#72725 = CARTESIAN_POINT ( 'NONE',  ( 3.591859063236763294, 38.29030133659708923, -11.09922568453595026 ) ) ;
#72727 = DIRECTION ( 'NONE',  ( -0.6626200482157305061, 0.000000000000000000, -0.7489557207890082946 ) ) ;
#72726 = CARTESIAN_POINT ( 'NONE',  ( -10.19513985507820486, 14.49999999999999112, -11.00268709613237306 ) ) ;
#72728 = CARTESIAN_POINT ( 'NONE',  ( -0.8801773607111009756, 63.06368534415484106, 1.068504757029289695E-15 ) ) ;
#72729 = CARTESIAN_POINT ( 'NONE',  ( 21.09922568453594849, 1.206968003263753531, 6.408140936763242479 ) ) ;
#72730 = DIRECTION ( 'NONE',  ( -0.000000000000000000, 1.000000000000000000, -0.000000000000000000 ) ) ;
#72731 = CARTESIAN_POINT ( 'NONE',  ( 0.1532563361054083140, 31.00893115100078390, 1.131784320476157264E-15 ) ) ;
#72732 = CARTESIAN_POINT ( 'NONE',  ( 12.91533473730992121, 24.52201867748816966, 10.88017736071110164 ) ) ;
#72733 = CARTESIAN_POINT ( 'NONE',  ( 19.38216949554541202, 30.99863466993042138, 9.382169495545424454 ) ) ;
#72734 = DIRECTION ( 'NONE',  ( -0.8610351672809762880, 0.4339697742547274362, -0.2651201156810292225 ) ) ;
#72735 = CARTESIAN_POINT ( 'NONE',  ( 11.22915323889574601, 15.00000000000000000, 8.773176023390684364 ) ) ;
#72736 = AXIS2_PLACEMENT_3D ( 'NONE', #30438, #90941, #74462 ) ;
#72737 = CARTESIAN_POINT ( 'NONE',  ( 10.00000000000000000, 31.81368534415483751, -10.88017736071110342 ) ) ;
#72738 = PRESENTATION_LAYER_ASSIGNMENT (  '', '', ( #16894 ) ) ;
#72739 = EDGE_LOOP ( 'NONE', ( #90275, #32969, #73590, #24683, #90393, #90418 ) ) ;
#72740 = CARTESIAN_POINT ( 'NONE',  ( -11.25000000000000178, 2.713468844518205803, -3.014428414850123250 ) ) ;
#72741 = CARTESIAN_POINT ( 'NONE',  ( 17.96484262340118221, 4.938685344154837509, 7.964842623401181321 ) ) ;
#72743 = CARTESIAN_POINT ( 'NONE',  ( 15.44008868035555260, 34.73035201082151247, 9.422509992056143702 ) ) ;
#72742 = CARTESIAN_POINT ( 'NONE',  ( 2.791683348922240793, 61.63393115100079456, 7.208316651077764092 ) ) ;
#72744 = CARTESIAN_POINT ( 'NONE',  ( 12.50534872682727539, 3.894361491432412218E-16, 7.339363270777609749 ) ) ;
#72745 = CARTESIAN_POINT ( 'NONE',  ( 0.5774900079438607392, 58.48035201082151247, 5.440088680355550821 ) ) ;
#72747 = DIRECTION ( 'NONE',  ( -0.8241261886220129229, 0.000000000000000000, -0.5664062369248369366 ) ) ;
#72746 = CARTESIAN_POINT ( 'NONE',  ( 10.00000000000000000, 26.81368534415484106, -10.88017736071110342 ) ) ;
#72748 = CARTESIAN_POINT ( 'NONE',  ( 1.472469842513823179, 0.5922644843341181575, -4.923371831947296329 ) ) ;
#72749 = SURFACE_STYLE_USAGE ( .BOTH. , #59231 ) ;
#72750 = CARTESIAN_POINT ( 'NONE',  ( 12.63842701281683034, 52.46726448433413026, 9.846743663894596210 ) ) ;
#72752 = SURFACE_SIDE_STYLE ('',( #64754 ) ) ;
#72751 = CARTESIAN_POINT ( 'NONE',  ( -2.266590686148945544, 52.22041550158064638, 7.082119434687048631 ) ) ;
#72753 = SURFACE_STYLE_USAGE ( .BOTH. , #20267 ) ;
#72754 = CARTESIAN_POINT ( 'NONE',  ( 6.204703633549690345, 12.84541550158063572, 14.16423886937410082 ) ) ;
#72755 = CARTESIAN_POINT ( 'NONE',  ( 10.00000000000000178, 38.05374883491396787, 14.16423886937410082 ) ) ;
#72756 = CARTESIAN_POINT ( 'NONE',  ( 13.43411237798105340, 10.58196800326375353, 12.81628187352647963 ) ) ;
#72757 = DIRECTION ( 'NONE',  ( 0.7808688094430307203, -0.6246950475544238435, 0.000000000000000000 ) ) ;
#72758 = EDGE_LOOP ( 'NONE', ( #77655, #48863, #89424, #34175 ) ) ;
#72759 = CARTESIAN_POINT ( 'NONE',  ( 15.44008868035555260, 4.730352010821505360, 9.422509992056143702 ) ) ;
#72760 = CARTESIAN_POINT ( 'NONE',  ( 19.84674366389459621, 38.50893115100078745, 7.409399052514197653E-17 ) ) ;
#72762 = DIRECTION ( 'NONE',  ( -0.000000000000000000, 1.000000000000000000, 0.000000000000000000 ) ) ;
#72761 = DIRECTION ( 'NONE',  ( 0.7971177707001108059, 0.6038238647437559337, -1.106223127961422775E-14 ) ) ;
#72763 = CARTESIAN_POINT ( 'NONE',  ( 15.44008868035555793, 56.39701867748817676, -9.422509992056140149 ) ) ;
#72764 = CARTESIAN_POINT ( 'NONE',  ( 7.551349515323185990, 0.000000000000000000, -12.08468537022906020 ) ) ;
#72765 = DIRECTION ( 'NONE',  ( -0.9636304532086211738, 0.000000000000000000, -0.2672383760782636175 ) ) ;
#72766 = CARTESIAN_POINT ( 'NONE',  ( 3.591859063236761518, 29.95696800326375708, 11.09922568453594849 ) ) ;
#72767 = CARTESIAN_POINT ( 'NONE',  ( 0.1532563361054083140, 31.00893115100078390, 1.131784320476157264E-15 ) ) ;
#72768 = ORIENTED_EDGE ( 'NONE', *, *, #7540, .T. ) ;
#72769 = CARTESIAN_POINT ( 'NONE',  ( 18.61655166652078464, 4.877183271974287138, 6.499999999999961808 ) ) ;
#72770 = CARTESIAN_POINT ( 'NONE',  ( 6.204703633549690345, 67.84541550158060375, 14.16423886937410082 ) ) ;
#72771 = CARTESIAN_POINT ( 'NONE',  ( 22.26659068614894466, 43.88708216824729647, 7.082119434687054849 ) ) ;
#72772 = CARTESIAN_POINT ( 'NONE',  ( 0.5774900079438607392, 28.48035201082150891, 5.440088680355550821 ) ) ;
#72773 = CARTESIAN_POINT ( 'NONE',  ( 15.44008868035555260, 44.73035201082151247, 9.422509992056143702 ) ) ;
#72774 = CARTESIAN_POINT ( 'NONE',  ( 67.06412365047464164, 14.00000000000000888, 10.00000000000000000 ) ) ;
#72775 = CARTESIAN_POINT ( 'NONE',  ( 10.69986656896780275, -97.11187948767582157, -3.999999999999999112 ) ) ;
#72776 = CARTESIAN_POINT ( 'NONE',  ( 0.1532563361054083140, 16.00893115100078390, 1.131784320476157264E-15 ) ) ;
#72778 = SURFACE_SIDE_STYLE ('',( #42306 ) ) ;
#72777 = ADVANCED_BREP_SHAPE_REPRESENTATION ( '', ( #8224, #27931 ), #10314 ) ;
#72779 = DIRECTION ( 'NONE',  ( 0.000000000000000000, 0.000000000000000000, -1.000000000000000000 ) ) ;
#72780 = CARTESIAN_POINT ( 'NONE',  ( 19.84674366389459621, 43.50893115100078745, 7.409399052514197653E-17 ) ) ;
#72781 = CARTESIAN_POINT ( 'NONE',  ( 19.84674366389459266, 48.30059781766745175, 2.638427012816836559 ) ) ;
#72782 = MECHANICAL_DESIGN_GEOMETRIC_PRESENTATION_REPRESENTATION (  '', ( #24859 ), #39279 ) ;
#72783 = EDGE_CURVE ( 'NONE', #9285, #26361, #88364, .T. ) ;
#72784 = CARTESIAN_POINT ( 'NONE',  ( 10.00000000000000000, 21.81368534415484106, -10.88017736071110342 ) ) ;
#72785 = VERTEX_POINT ( 'NONE', #50353 ) ;
#72786 = CARTESIAN_POINT ( 'NONE',  ( 22.81628187352647785, 51.62363466993042493, 6.195893100308588602E-16 ) ) ;
#72787 = DIRECTION ( 'NONE',  ( 0.000000000000000000, 1.000000000000000000, 0.000000000000000000 ) ) ;
#72788 = CARTESIAN_POINT ( 'NONE',  ( 17.96484262340118221, 64.93868534415483396, 7.964842623401181321 ) ) ;
#72789 = CARTESIAN_POINT ( 'NONE',  ( 12.63842701281683034, 22.46726448433411605, 9.846743663894596210 ) ) ;
#72791 = CARTESIAN_POINT ( 'NONE',  ( 19.84674366389459266, 18.30059781766745175, 2.638427012816836559 ) ) ;
#72790 = CARTESIAN_POINT ( 'NONE',  ( 6.204703633549690345, 62.84541550158063927, 14.16423886937410082 ) ) ;
#72792 = DIRECTION ( 'NONE',  ( 0.000000000000000000, 0.000000000000000000, -1.000000000000000000 ) ) ;
#72793 = FACE_OUTER_BOUND ( 'NONE', #60492, .T. ) ;
#72794 = CARTESIAN_POINT ( 'NONE',  ( 17.08211943468705130, 23.47041550158063572, 12.26659068614894998 ) ) ;
#72795 = CARTESIAN_POINT ( 'NONE',  ( 13.79529636645030344, 38.26208216824729647, 14.16423886937410614 ) ) ;
#72796 = CARTESIAN_POINT ( 'NONE',  ( 7.361572987183170547, 42.05059781766745886, 9.846743663894590881 ) ) ;
#72797 = CARTESIAN_POINT ( 'NONE',  ( -4.250000000000000000, 10.25000000000000000, 4.000000000000000000 ) ) ;
#72798 = CARTESIAN_POINT ( 'NONE',  ( 7.084665262690076126, 27.02201867748817676, -10.88017736071110164 ) ) ;
#72799 = CARTESIAN_POINT ( 'NONE',  ( 4.559911319644449179, 58.89701867748817676, 9.422509992056141925 ) ) ;
#72800 = CARTESIAN_POINT ( 'NONE',  ( 1.959929470562282283, 56.50257860105349295, 5.767676674365853629 ) ) ;
#72801 = ORIENTED_EDGE ( 'NONE', *, *, #52388, .F. ) ;
#72802 = CARTESIAN_POINT ( 'NONE',  ( 10.00000000000000178, 45.37363466993041783, 12.81628187352647608 ) ) ;
#72803 = CARTESIAN_POINT ( 'NONE',  ( 12.91533473730992121, 59.52201867748816966, 10.88017736071110164 ) ) ;
#72804 = ORIENTED_EDGE ( 'NONE', *, *, #14357, .F. ) ;
#72805 = CARTESIAN_POINT ( 'NONE',  ( -9.281709892946317098, 15.00000000000000711, -11.30302492080718579 ) ) ;
#72806 = PRESENTATION_STYLE_ASSIGNMENT (( #79830 ) ) ;
#72807 = CARTESIAN_POINT ( 'NONE',  ( -0.8801773607111008646, 68.27201867748817676, 2.915334737309923430 ) ) ;
#72808 = VECTOR ( 'NONE', #89841, 1000.000000000000000 ) ;
#72809 = ORIENTED_EDGE ( 'NONE', *, *, #21121, .T. ) ;
#72810 = AXIS2_PLACEMENT_3D ( 'NONE', #65311, #79352, #17388 ) ;
#72811 = CARTESIAN_POINT ( 'NONE',  ( -0.8801773607111008646, 58.27201867748816966, 2.915334737309923430 ) ) ;
#72812 = CARTESIAN_POINT ( 'NONE',  ( 2.035157376598824452, 8.688685344154839285, 7.964842623401179544 ) ) ;
#72813 = EDGE_CURVE ( 'NONE', #63992, #23413, #73844, .T. ) ;
#72814 = LINE ( 'NONE', #4354, #48378 ) ;
#72815 = CARTESIAN_POINT ( 'NONE',  ( 17.39651004071841101, 37.93575266056827644, 6.500000000000005329 ) ) ;
#72816 = CARTESIAN_POINT ( 'NONE',  ( 20.88017736071110519, 5.563685344154838397, 2.639326808657452039E-16 ) ) ;
#72817 = CARTESIAN_POINT ( 'NONE',  ( 5.076628168052703671, 11.84226448433411960, 8.527530157486179263 ) ) ;
#72818 = CARTESIAN_POINT ( 'NONE',  ( 24.16423886937410614, 14.30374883491396787, 8.672049930838204340E-16 ) ) ;
#72819 = VECTOR ( 'NONE', #29787, 1000.000000000000000 ) ;
#72820 = EDGE_CURVE ( 'NONE', #4466, #67947, #31918, .T. ) ;
#72821 = CARTESIAN_POINT ( 'NONE',  ( -0.8801773607111008646, 28.27201867748817321, 2.915334737309923430 ) ) ;
#72822 = CARTESIAN_POINT ( 'NONE',  ( 17.20831665107776587, 54.13393115100079456, -7.208316651077762316 ) ) ;
#72823 = ORIENTED_EDGE ( 'NONE', *, *, #30963, .F. ) ;
#72824 = CARTESIAN_POINT ( 'NONE',  ( 1.472469842513823179, 56.42559781766745886, 4.923371831947296329 ) ) ;
#72825 = ORIENTED_EDGE ( 'NONE', *, *, #63090, .F. ) ;
#72826 = DIRECTION ( 'NONE',  ( -0.000000000000000000, -1.000000000000000000, -0.000000000000000000 ) ) ;
#72827 = CARTESIAN_POINT ( 'NONE',  ( 2.035157376598822676, 47.43868534415484817, -7.964842623401177768 ) ) ;
#72828 = DIRECTION ( 'NONE',  ( 0.8703556959399044723, 0.000000000000000000, -0.4924235601034586685 ) ) ;
#72829 = CARTESIAN_POINT ( 'NONE',  ( 0.6178305044545818747, 38.49863466993042493, -9.382169495545419124 ) ) ;
#72831 = CARTESIAN_POINT ( 'NONE',  ( -5.888281321711915872, 1.823139558123406223, -10.37198838585826266 ) ) ;
#72830 = CARTESIAN_POINT ( 'NONE',  ( 7.084665262690076126, 14.10535201082150358, 10.88017736071109987 ) ) ;
#72832 = CARTESIAN_POINT ( 'NONE',  ( 20.88017736071110875, 65.77201867748817676, -2.915334737309920765 ) ) ;
#72833 = CARTESIAN_POINT ( 'NONE',  ( 2.035157376598822676, 2.438685344154838397, -7.964842623401177768 ) ) ;
#72834 = CARTESIAN_POINT ( 'NONE',  ( 22.81628187352647785, 46.41530133659708213, 3.434112377981063169 ) ) ;
#72835 = CARTESIAN_POINT ( 'NONE',  ( 7.084665262690076126, 24.10535201082150181, 10.88017736071109987 ) ) ;
#72836 = CARTESIAN_POINT ( 'NONE',  ( 14.71525861348293596, 14.49999999999999112, 2.908807992686717192 ) ) ;
#72837 = ORIENTED_EDGE ( 'NONE', *, *, #83556, .T. ) ;
#72838 = CARTESIAN_POINT ( 'NONE',  ( 13.43411237798105340, 45.58196800326374643, 12.81628187352647963 ) ) ;
#72839 = CARTESIAN_POINT ( 'NONE',  ( 7.084665262690076126, 29.10535201082150181, 10.88017736071109987 ) ) ;
#72840 = CARTESIAN_POINT ( 'NONE',  ( 2.791683348922237240, 60.38393115100078745, -7.208316651077763204 ) ) ;
#72841 = ORIENTED_EDGE ( 'NONE', *, *, #57907, .T. ) ;
#72842 = DIRECTION ( 'NONE',  ( 1.000000000000000000, 0.000000000000000000, 0.000000000000000000 ) ) ;
#72843 = ADVANCED_FACE ( 'NONE', ( #5853 ), #20363, .F. ) ;
#72844 = CARTESIAN_POINT ( 'NONE',  ( 1.472469842513823179, 66.42559781766745175, 4.923371831947296329 ) ) ;
#72846 = CARTESIAN_POINT ( 'NONE',  ( 5.076628168052704559, 55.17559781766745175, -8.527530157486179263 ) ) ;
#72845 = CARTESIAN_POINT ( 'NONE',  ( 10.39692778084932812, 0.04962893796709086369, 10.46714871971205696 ) ) ;
#72847 = CARTESIAN_POINT ( 'NONE',  ( 7.084665262690076126, 22.02201867748817321, -10.88017736071110164 ) ) ;
#72848 = CARTESIAN_POINT ( 'NONE',  ( 5.076628168052703671, 11.84226448433411960, 8.527530157486179263 ) ) ;
#72849 = DIRECTION ( 'NONE',  ( -0.000000000000000000, 0.000000000000000000, 1.000000000000000000 ) ) ;
#72850 = AXIS2_PLACEMENT_3D ( 'NONE', #62571, #62077, #40585 ) ;
#72851 = CARTESIAN_POINT ( 'NONE',  ( 19.72487221294571214, 57.80223176428831522, -6.499999999999988454 ) ) ;
#72852 = EDGE_CURVE ( 'NONE', #87105, #65300, #24568, .T. ) ;
#72854 = CARTESIAN_POINT ( 'NONE',  ( 10.00000000000000178, 12.25893115100078568, 9.846743663894594434 ) ) ;
#72853 = CARTESIAN_POINT ( 'NONE',  ( 5.076628168052703671, 46.84226448433412315, 8.527530157486179263 ) ) ;
#72855 = CARTESIAN_POINT ( 'NONE',  ( 19.84674366389459266, 28.71726448433411960, -2.638427012816827677 ) ) ;
#72857 = VERTEX_POINT ( 'NONE', #41899 ) ;
#72856 = CARTESIAN_POINT ( 'NONE',  ( 18.52753015748617571, 58.09226448433411605, 4.923371831947298993 ) ) ;
#72858 = DIRECTION ( 'NONE',  ( -0.000000000000000000, -0.000000000000000000, 1.000000000000000000 ) ) ;
#72859 = CARTESIAN_POINT ( 'NONE',  ( -2.816281873526471635, 33.91530133659708213, -3.434112377981056508 ) ) ;
#72860 = CARTESIAN_POINT ( 'NONE',  ( 14.92337183194729633, 42.67559781766745886, 8.527530157486181039 ) ) ;
#72861 = CARTESIAN_POINT ( 'NONE',  ( 8.235571585149866536, 8.243033628982649574, -8.235571585149871865 ) ) ;
#72862 = CARTESIAN_POINT ( 'NONE',  ( 13.79529636645031943, 55.34541550158062506, -14.16423886937409904 ) ) ;
#72863 = CARTESIAN_POINT ( 'NONE',  ( 17.20831665107776587, 37.88393115100078745, 7.208316651077764980 ) ) ;
#72864 = MECHANICAL_DESIGN_GEOMETRIC_PRESENTATION_REPRESENTATION (  '', ( #87220 ), #42543 ) ;
#72865 = ORIENTED_EDGE ( 'NONE', *, *, #86681, .T. ) ;
#72866 = CARTESIAN_POINT ( 'NONE',  ( 9.240973841163532043, 4.236086333263440692E-16, 11.17382667070378943 ) ) ;
#72867 = CARTESIAN_POINT ( 'NONE',  ( 22.26659068614894466, 58.88708216824729647, 7.082119434687054849 ) ) ;
#72868 = CARTESIAN_POINT ( 'NONE',  ( -7.750355510519348456, 84.07179676972448590, -4.000000000000000000 ) ) ;
#72869 = CARTESIAN_POINT ( 'NONE',  ( 19.42250999205614193, 10.14701867748816966, 5.440088680355555262 ) ) ;
#72870 = CARTESIAN_POINT ( 'NONE',  ( 2.917880565312948704, 37.63708216824731068, 12.26659068614894643 ) ) ;
#72872 = PLANE ( 'NONE',  #3154 ) ;
#72871 = CARTESIAN_POINT ( 'NONE',  ( 10.00000000000000178, 58.05374883491397497, 14.16423886937410082 ) ) ;
#72873 = CARTESIAN_POINT ( 'NONE',  ( 19.10478245763051319, 5.101608292538858613, 5.990408912944327646 ) ) ;
#72874 = CARTESIAN_POINT ( 'NONE',  ( 1.472469842513823179, 5.592264484334118713, -4.923371831947296329 ) ) ;
#72876 = CARTESIAN_POINT ( 'NONE',  ( 0.6178305044545818747, 3.498634669930420049, -9.382169495545419124 ) ) ;
#72875 = CARTESIAN_POINT ( 'NONE',  ( 0.000000000000000000, 1.823139558123437975, 0.000000000000000000 ) ) ;
#72877 = VECTOR ( 'NONE', #25696, 1000.000000000000000 ) ;
#72878 = CARTESIAN_POINT ( 'NONE',  ( 17.96484262340118221, 56.18868534415484817, -7.964842623401177768 ) ) ;
#72879 = CARTESIAN_POINT ( 'NONE',  ( -0.8801773607110990882, 17.85535201082150536, -2.915334737309924318 ) ) ;
#72880 = FACE_OUTER_BOUND ( 'NONE', #63978, .T. ) ;
#72881 = AXIS2_PLACEMENT_3D ( 'NONE', #83229, #7240, #30212 ) ;
#72882 = CARTESIAN_POINT ( 'NONE',  ( 1.472469842513823179, 51.42559781766745886, 4.923371831947296329 ) ) ;
#72883 = CARTESIAN_POINT ( 'NONE',  ( 14.62129639376011170, 15.00000000000000711, -0.3552502084985190156 ) ) ;
#72884 = AXIS2_PLACEMENT_3D ( 'NONE', #91279, #24280, #22800 ) ;
#72885 = VERTEX_POINT ( 'NONE', #81351 ) ;
#72886 = CARTESIAN_POINT ( 'NONE',  ( -0.3689425029237881626, 27.42874883491397142, 10.36894250292379027 ) ) ;
#72887 = VECTOR ( 'NONE', #65585, 1000.000000000000000 ) ;
#72888 = CARTESIAN_POINT ( 'NONE',  ( 0.000000000000000000, 15.00000000000000000, 0.000000000000000000 ) ) ;
#72890 = DIRECTION ( 'NONE',  ( -0.5547001962252290364, -0.8320502943378437211, 0.000000000000000000 ) ) ;
#72889 = CARTESIAN_POINT ( 'NONE',  ( -5.809210876199116136, -36.07757871006175776, -2.749999999999193978 ) ) ;
#72891 = CARTESIAN_POINT ( 'NONE',  ( 20.88017736071110519, 25.56368534415483751, 2.639326808657452039E-16 ) ) ;
#72892 = CARTESIAN_POINT ( 'NONE',  ( -2.816281873526473856, 24.33196800326375353, 3.434112377981055619 ) ) ;
#72893 = LINE ( 'NONE', #10927, #94364 ) ;
#72894 = CARTESIAN_POINT ( 'NONE',  ( 7.361572987183169658, 4.967264484334119601, -9.846743663894592657 ) ) ;
#72895 = CARTESIAN_POINT ( 'NONE',  ( 21.09922568453594849, 61.20696800326376064, 6.408140936763242479 ) ) ;
#72896 = ORIENTED_EDGE ( 'NONE', *, *, #74405, .T. ) ;
#72897 = CARTESIAN_POINT ( 'NONE',  ( 8.629999999999995453, 40.74999999999999289, 4.000000000000000000 ) ) ;
#72898 = CARTESIAN_POINT ( 'NONE',  ( 24.16423886937409904, 29.09541550158063572, 3.795296366450317205 ) ) ;
#72899 = FILL_AREA_STYLE_COLOUR ( '', #41056 ) ;
#72900 = CARTESIAN_POINT ( 'NONE',  ( 20.10384461210892582, 61.74302437010793909, 6.337995344473753789 ) ) ;
#72901 = CARTESIAN_POINT ( 'NONE',  ( 7.084665262690076126, 9.105352010821503583, 10.88017736071109987 ) ) ;
#72902 = DIRECTION ( 'NONE',  ( 0.000000000000000000, 1.000000000000000000, 0.000000000000000000 ) ) ;
#72903 = CARTESIAN_POINT ( 'NONE',  ( 34.56412365047464874, 11.49999999999999645, -9.500000000000000000 ) ) ;
#72904 =( BOUNDED_CURVE ( )  B_SPLINE_CURVE ( 2, ( #93489, #24026, #54494, #85009, #39518 ),
 .UNSPECIFIED., .F., .T. ) 
 B_SPLINE_CURVE_WITH_KNOTS ( ( 3, 2, 3 ),
 ( 0.6666666666666666297, 0.6722222222222222765, 0.6777069814160940897 ),
 .UNSPECIFIED. ) 
 CURVE ( )  GEOMETRIC_REPRESENTATION_ITEM ( )  RATIONAL_B_SPLINE_CURVE ( ( 1.000000000000000000, 0.9659258262890683122, 1.000000000000000000, 0.9663600452437686172, 0.9991426288945792766 ) ) 
 REPRESENTATION_ITEM ( '' )  );
#72905 = CARTESIAN_POINT ( 'NONE',  ( 17.96484262340118221, 41.18868534415484106, -7.964842623401177768 ) ) ;
#72906 = CARTESIAN_POINT ( 'NONE',  ( 4.559911319644449179, 52.23035201082151247, -9.422509992056141925 ) ) ;
#72907 = CARTESIAN_POINT ( 'NONE',  ( 0.6178305044545838731, 14.74863466993041783, 9.382169495545420901 ) ) ;
#72908 = CARTESIAN_POINT ( 'NONE',  ( 7.361572987183170547, 62.05059781766745886, 9.846743663894590881 ) ) ;
#72909 = CARTESIAN_POINT ( 'NONE',  ( 0.5774900079438590739, 2.647018677488171434, -5.440088680355550821 ) ) ;
#72910 = CARTESIAN_POINT ( 'NONE',  ( 5.076628168052703671, 6.842264484334118713, 8.527530157486179263 ) ) ;
#72911 = COLOUR_RGB ( '', 0.31764706, 0.68627451, 0.89019608) ;
#72912 = DIRECTION ( 'NONE',  ( 1.000000000000000000, 0.000000000000000000, 0.000000000000000000 ) ) ;
#72913 = CARTESIAN_POINT ( 'NONE',  ( 4.559911319644449179, 38.89701867748817676, 9.422509992056141925 ) ) ;
#72914 = EDGE_CURVE ( 'NONE', #88979, #9752, #3893, .T. ) ;
#72915 = AXIS2_PLACEMENT_3D ( 'NONE', #91201, #52713, #6728 ) ;
#72916 = VECTOR ( 'NONE', #22964, 1000.000000000000000 ) ;
#72917 = CARTESIAN_POINT ( 'NONE',  ( 0.6178305044545818747, 8.498634669930421381, -9.382169495545419124 ) ) ;
#72918 = CARTESIAN_POINT ( 'NONE',  ( 20.88017736071110164, 60.35535201082151957, 2.915334737309930979 ) ) ;
#72919 = CARTESIAN_POINT ( 'NONE',  ( 12.63842701281683922, 19.55059781766745175, -9.846743663894590881 ) ) ;
#72920 = CARTESIAN_POINT ( 'NONE',  ( -2.816281873526473856, 49.12363466993042493, 9.499525473075851096E-16 ) ) ;
#72921 = CARTESIAN_POINT ( 'NONE',  ( 1.472469842513823179, 1.425597817667451528, 4.923371831947296329 ) ) ;
#72922 = VERTEX_POINT ( 'NONE', #57366 ) ;
#72923 = CARTESIAN_POINT ( 'NONE',  ( 2.603489959281588995, 55.43575266056826933, -6.500000000000003553 ) ) ;
#72924 = LINE ( 'NONE', #4454, #78145 ) ;
#72925 = CARTESIAN_POINT ( 'NONE',  ( 19.42250999205614548, 15.98035201082150714, -5.440088680355545492 ) ) ;
#72927 = CARTESIAN_POINT ( 'NONE',  ( 24.16423886937410614, 24.51208216824730002, -3.795296366450302550 ) ) ;
#72926 = CARTESIAN_POINT ( 'NONE',  ( 0.6178305044545838731, 64.74863466993043914, 9.382169495545420901 ) ) ;
#72928 = CARTESIAN_POINT ( 'NONE',  ( 7.361572987183169658, 24.96726448433412315, -9.846743663894592657 ) ) ;
#72929 = CARTESIAN_POINT ( 'NONE',  ( 2.035157376598824452, 13.68868534415483751, 7.964842623401179544 ) ) ;
#72930 = CARTESIAN_POINT ( 'NONE',  ( 7.084665262690076126, 2.022018677488171434, -10.88017736071110164 ) ) ;
#72931 = ORIENTED_EDGE ( 'NONE', *, *, #73087, .T. ) ;
#72932 = CARTESIAN_POINT ( 'NONE',  ( 7.084665262690076126, 14.10535201082150358, 10.88017736071109987 ) ) ;
#72933 = CARTESIAN_POINT ( 'NONE',  ( 4.559911319644449179, 33.89701867748817676, 9.422509992056141925 ) ) ;
#72935 = CARTESIAN_POINT ( 'NONE',  ( 15.44008868035555260, 29.73035201082150891, 9.422509992056143702 ) ) ;
#72934 = CARTESIAN_POINT ( 'NONE',  ( -8.000000000000000000, 1.019547802438458550, -3.750000000000000000 ) ) ;
#72936 = ORIENTED_EDGE ( 'NONE', *, *, #67334, .F. ) ;
#72937 = CARTESIAN_POINT ( 'NONE',  ( 12.91533473730992121, 24.52201867748816966, 10.88017736071110164 ) ) ;
#72938 = CARTESIAN_POINT ( 'NONE',  ( 12.63842701281683922, 64.55059781766745175, -9.846743663894590881 ) ) ;
#72939 = LINE ( 'NONE', #26454, #61657 ) ;
#72940 = ADVANCED_FACE ( 'NONE', ( #65847 ), #55198, .T. ) ;
#72941 = CARTESIAN_POINT ( 'NONE',  ( -2.816281873526471635, 58.91530133659707502, -3.434112377981056508 ) ) ;
#72942 = CARTESIAN_POINT ( 'NONE',  ( 0.000000000000000000, 0.000000000000000000, 0.000000000000000000 ) ) ;
#72943 = CARTESIAN_POINT ( 'NONE',  ( -0.3689425029237898834, 36.17874883491396787, -10.36894250292378850 ) ) ;
#72944 = CARTESIAN_POINT ( 'NONE',  ( 17.96484262340118221, 36.18868534415484106, -7.964842623401177768 ) ) ;
#72945 = CARTESIAN_POINT ( 'NONE',  ( 12.91533473730993009, 21.60535201082150536, -10.88017736071109987 ) ) ;
#72946 = FACE_OUTER_BOUND ( 'NONE', #31265, .T. ) ;
#72947 = AXIS2_PLACEMENT_3D ( 'NONE', #76183, #52523, #59531 ) ;
#72948 = CARTESIAN_POINT ( 'NONE',  ( 19.84674366389459266, 53.30059781766744464, 2.638427012816836559 ) ) ;
#72949 = EDGE_CURVE ( 'NONE', #92829, #85493, #26274, .T. ) ;
#72950 = CARTESIAN_POINT ( 'NONE',  ( 12.63842701281683922, 24.55059781766745175, -9.846743663894590881 ) ) ;
#72951 = CARTESIAN_POINT ( 'NONE',  ( -12.81628187352647963, -36.08469866340291787, -3.434112377981046293 ) ) ;
#72952 = CARTESIAN_POINT ( 'NONE',  ( 0.5774900079438590739, 7.647018677488171434, -5.440088680355550821 ) ) ;
#72953 = CARTESIAN_POINT ( 'NONE',  ( 10.00000000000000178, 12.25893115100078568, 9.846743663894594434 ) ) ;
#72954 = CARTESIAN_POINT ( 'NONE',  ( 19.38216949554541557, 12.24863466993041961, -9.382169495545420901 ) ) ;
#72955 = CARTESIAN_POINT ( 'NONE',  ( -0.8801773607111008646, 63.27201867748817676, 2.915334737309923430 ) ) ;
#72957 = CARTESIAN_POINT ( 'NONE',  ( 22.81628187352647785, 61.62363466993041783, 6.195893100308588602E-16 ) ) ;
#72956 = CARTESIAN_POINT ( 'NONE',  ( 10.00000000000000000, 21.81368534415484106, -10.88017736071110342 ) ) ;
#72958 = CARTESIAN_POINT ( 'NONE',  ( 20.36894250292379382, 28.67874883491396787, 10.36894250292379205 ) ) ;
#72959 = CARTESIAN_POINT ( 'NONE',  ( 0.000000000000000000, 15.00000000000000000, 0.000000000000000000 ) ) ;
#72961 = CARTESIAN_POINT ( 'NONE',  ( 0.6178305044545838731, 64.74863466993043914, 9.382169495545420901 ) ) ;
#72960 = VECTOR ( 'NONE', #96621, 1000.000000000000000 ) ;
#72962 = ORIENTED_EDGE ( 'NONE', *, *, #71757, .T. ) ;
#72963 = CARTESIAN_POINT ( 'NONE',  ( 10.00000000000000000, 7.873634669930421381, -12.81628187352647608 ) ) ;
#72964 = DIRECTION ( 'NONE',  ( 0.3173046564050898688, 0.000000000000000000, 0.9483236552061999891 ) ) ;
#72965 = CARTESIAN_POINT ( 'NONE',  ( 2.035157376598824452, 38.68868534415483396, 7.964842623401179544 ) ) ;
#72966 = FACE_OUTER_BOUND ( 'NONE', #56472, .T. ) ;
#72967 = VERTEX_POINT ( 'NONE', #38472 ) ;
#72968 = CARTESIAN_POINT ( 'NONE',  ( 12.63842701281683922, 19.55059781766745175, -9.846743663894590881 ) ) ;
#72969 = CARTESIAN_POINT ( 'NONE',  ( 14.92337183194729988, 14.34226448433411782, -8.527530157486177487 ) ) ;
#72970 = APPLICATION_CONTEXT ( 'automotive_design' ) ;
#72971 = CARTESIAN_POINT ( 'NONE',  ( 5.076628168052704559, 20.17559781766745175, -8.527530157486179263 ) ) ;
#72972 = CARTESIAN_POINT ( 'NONE',  ( 12.63842701281683922, 9.550597817667449974, -9.846743663894590881 ) ) ;
#72973 = AXIS2_PLACEMENT_3D ( 'NONE', #20445, #50934, #73928 ) ;
#72974 = EDGE_CURVE ( 'NONE', #51686, #651, #30450, .T. ) ;
#72977 = FACE_OUTER_BOUND ( 'NONE', #91165, .T. ) ;
#72976 = AXIS2_PLACEMENT_3D ( 'NONE', #76065, #6584, #44579 ) ;
#72975 = CARTESIAN_POINT ( 'NONE',  ( 14.92337183194729633, 2.675597817667451750, 8.527530157486181039 ) ) ;
#72978 = CARTESIAN_POINT ( 'NONE',  ( 19.84674366389459621, 8.508931151000785675, 7.409399052514197653E-17 ) ) ;
#72980 = VERTEX_POINT ( 'NONE', #61443 ) ;
#72979 = CARTESIAN_POINT ( 'NONE',  ( 18.52753015748617571, 13.09226448433411960, 4.923371831947298993 ) ) ;
#72981 = STYLED_ITEM ( 'NONE', ( #2626 ), #67807 ) ;
#72982 = DIRECTION ( 'NONE',  ( 0.5547001962252290364, 0.8320502943378437211, 0.000000000000000000 ) ) ;
#72983 = CARTESIAN_POINT ( 'NONE',  ( -2.816281873526473856, 4.123634669930420493, 9.499525473075851096E-16 ) ) ;
#72984 = ORIENTED_EDGE ( 'NONE', *, *, #91919, .T. ) ;
#72985 = FILL_AREA_STYLE ('',( #79998 ) ) ;
#72986 = CARTESIAN_POINT ( 'NONE',  ( 17.08211943468705840, 25.13708216824730357, -12.26659068614894466 ) ) ;
#72987 = PLANE ( 'NONE',  #42349 ) ;
#72988 = CARTESIAN_POINT ( 'NONE',  ( 13.79529636645030344, 13.26208216824729824, 14.16423886937410614 ) ) ;
#72989 = CARTESIAN_POINT ( 'NONE',  ( -2.266590686148945544, 37.22041550158063217, 7.082119434687048631 ) ) ;
#72990 = SURFACE_SIDE_STYLE ('',( #19507 ) ) ;
#72991 = CARTESIAN_POINT ( 'NONE',  ( -2.266590686148945544, 2.220415501580634388, 7.082119434687048631 ) ) ;
#72992 = CARTESIAN_POINT ( 'NONE',  ( 12.91533473730992121, 34.52201867748817676, 10.88017736071110164 ) ) ;
#72993 = CARTESIAN_POINT ( 'NONE',  ( -5.240416992896902215, 0.04922511925148113227, 13.79072622793298208 ) ) ;
#72994 = CARTESIAN_POINT ( 'NONE',  ( 17.20831665107776587, 12.88393115100078390, 7.208316651077764980 ) ) ;
#72996 = CARTESIAN_POINT ( 'NONE',  ( 0.1532563361054083140, 21.00893115100078745, 1.131784320476157264E-15 ) ) ;
#72995 = CARTESIAN_POINT ( 'NONE',  ( 20.88017736071110875, 50.77201867748817676, -2.915334737309920765 ) ) ;
#72997 = CARTESIAN_POINT ( 'NONE',  ( 10.00000000000000178, 9.313685344154839285, 10.88017736071110342 ) ) ;
#72998 = CARTESIAN_POINT ( 'NONE',  ( 13.43411237798106583, 42.66530133659707502, -12.81628187352647252 ) ) ;
#72999 = CARTESIAN_POINT ( 'NONE',  ( 18.52753015748618282, 48.92559781766745886, -4.923371831947291888 ) ) ;
#73000 = CARTESIAN_POINT ( 'NONE',  ( 2.120353041430647512, 4.078855811979330250E-16, -14.34413130794945523 ) ) ;
#73001 = CARTESIAN_POINT ( 'NONE',  ( 10.00000000000000178, 30.37363466993042138, 12.81628187352647608 ) ) ;
#73002 = CARTESIAN_POINT ( 'NONE',  ( 3.469446951953614189E-15, -36.94625116508602503, 14.16423886937410259 ) ) ;
#73003 = CARTESIAN_POINT ( 'NONE',  ( 17.20831665107776587, 42.88393115100077324, 7.208316651077764980 ) ) ;
#73004 = CARTESIAN_POINT ( 'NONE',  ( 24.16423886937410614, 19.30374883491397142, 8.672049930838204340E-16 ) ) ;
#73005 = VERTEX_POINT ( 'NONE', #54433 ) ;
#73006 = CARTESIAN_POINT ( 'NONE',  ( -3.836325488036278930, 0.5000000000000004441, 14.50112432709419785 ) ) ;
#73007 = CIRCLE ( 'NONE', #85802, 18.53834841531100608 ) ;
#73008 = CARTESIAN_POINT ( 'NONE',  ( 2.035157376598824452, 53.68868534415484817, 7.964842623401179544 ) ) ;
#73009 = CARTESIAN_POINT ( 'NONE',  ( 15.44008868035555260, 49.73035201082150536, 9.422509992056143702 ) ) ;
#73010 = CARTESIAN_POINT ( 'NONE',  ( 6.204703633549690345, 42.84541550158063217, 14.16423886937410082 ) ) ;
#73011 = CARTESIAN_POINT ( 'NONE',  ( 18.52753015748618282, 48.92559781766745886, -4.923371831947291888 ) ) ;
#73012 = CARTESIAN_POINT ( 'NONE',  ( -14.88232117145534517, 14.49999999999999112, -1.875237731503371030 ) ) ;
#73013 = CARTESIAN_POINT ( 'NONE',  ( -0.8801773607111008646, 38.27201867748816255, 2.915334737309923430 ) ) ;
#73014 = CARTESIAN_POINT ( 'NONE',  ( 0.1916775849787346053, 27.25868815902070352, -6.500000000000015099 ) ) ;
#73015 = CARTESIAN_POINT ( 'NONE',  ( 5.076628168052704559, 55.17559781766745175, -8.527530157486179263 ) ) ;
#73016 = CARTESIAN_POINT ( 'NONE',  ( -5.440088680355558814, 12.23035201082151069, -9.422509992056136596 ) ) ;
#73017 = CARTESIAN_POINT ( 'NONE',  ( 20.88017736071110875, 5.772018677488170546, -2.915334737309920765 ) ) ;
#73018 = CARTESIAN_POINT ( 'NONE',  ( -0.03932841506543007654, 13.12161441960500952, 6.397827110478970347 ) ) ;
#73019 = CARTESIAN_POINT ( 'NONE',  ( 7.084665262690076126, 4.105352010821503583, 10.88017736071109987 ) ) ;
#73020 = ADVANCED_FACE ( 'NONE', ( #15958 ), #18792, .T. ) ;
#73021 = DIRECTION ( 'NONE',  ( 1.000000000000000000, 0.000000000000000000, 0.000000000000000000 ) ) ;
#73022 = CARTESIAN_POINT ( 'NONE',  ( 1.472469842513823179, 1.425597817667451528, 4.923371831947296329 ) ) ;
#73023 = CARTESIAN_POINT ( 'NONE',  ( 12.91533473730992121, 64.52201867748817676, 10.88017736071110164 ) ) ;
#73024 = DIRECTION ( 'NONE',  ( 0.000000000000000000, 0.000000000000000000, 1.000000000000000000 ) ) ;
#73025 = CARTESIAN_POINT ( 'NONE',  ( 2.791683348922240793, 31.63393115100078745, 7.208316651077764092 ) ) ;
#73026 = EDGE_CURVE ( 'NONE', #81557, #24768, #17986, .T. ) ;
#73027 = EDGE_CURVE ( 'NONE', #18735, #19349, #91459, .T. ) ;
#73028 = CARTESIAN_POINT ( 'NONE',  ( -0.8801773607110991993, 27.85535201082150181, -2.915334737309923874 ) ) ;
#73029 = CARTESIAN_POINT ( 'NONE',  ( 22.81628187352647785, 11.62363466993042138, 6.195893100308588602E-16 ) ) ;
#73031 = CARTESIAN_POINT ( 'NONE',  ( -8.099999999999999645, 80.99999999999994316, 0.000000000000000000 ) ) ;
#73030 = CARTESIAN_POINT ( 'NONE',  ( 4.559911319644449179, 28.89701867748817321, 9.422509992056141925 ) ) ;
#73032 = CARTESIAN_POINT ( 'NONE',  ( 21.09922568453595559, 37.04030133659708923, -6.408140936763230044 ) ) ;
#73033 = ORIENTED_EDGE ( 'NONE', *, *, #28948, .T. ) ;
#73034 = CYLINDRICAL_SURFACE ( 'NONE', #38268, 11.92686044187656513 ) ;
#73036 = CARTESIAN_POINT ( 'NONE',  ( -11.61621867929619611, -0.03417435944610275333, 10.99731149103378058 ) ) ;
#73035 = CARTESIAN_POINT ( 'NONE',  ( 6.565887622018943937, 15.16530133659708568, 12.81628187352647430 ) ) ;
#73037 = CARTESIAN_POINT ( 'NONE',  ( 20.88017736071110875, 25.77201867748816966, -2.915334737309920765 ) ) ;
#73038 = CARTESIAN_POINT ( 'NONE',  ( 6.204703633549690345, 60.76208216824730357, -14.16423886937410259 ) ) ;
#73039 = VECTOR ( 'NONE', #77521, 1000.000000000000227 ) ;
#73040 = CARTESIAN_POINT ( 'NONE',  ( 1.472469842513823179, 50.59226448433411605, -4.923371831947296329 ) ) ;
#73041 = CARTESIAN_POINT ( 'NONE',  ( 1.472469842513823179, 0.5922644843341181575, -4.923371831947296329 ) ) ;
#73042 = CARTESIAN_POINT ( 'NONE',  ( 15.44008868035555793, 61.39701867748817676, -9.422509992056140149 ) ) ;
#73043 = CARTESIAN_POINT ( 'NONE',  ( 1.350000000000004086, 98.49999999999998579, 8.000000000000000000 ) ) ;
#73044 = CARTESIAN_POINT ( 'NONE',  ( -2.266590686148945544, 31.38708216824730002, -7.082119434687050408 ) ) ;
#73045 = EDGE_CURVE ( 'NONE', #16383, #80582, #23959, .T. ) ;
#73046 = CIRCLE ( 'NONE', #95474, 15.00000000000000000 ) ;
#73047 = AXIS2_PLACEMENT_3D ( 'NONE', #70440, #25447, #48903 ) ;
#73048 = B_SPLINE_CURVE_WITH_KNOTS ( 'NONE', 3,
 ( #95390, #80882, #94403, #13743, #18414, #44226 ),
 .UNSPECIFIED., .F., .F.,
 ( 4, 2, 4 ),
 ( 0.0002800912045164367708, 0.0006862973266905153438, 0.001092503448864594025 ),
 .UNSPECIFIED. ) ;
#73049 = AXIS2_PLACEMENT_3D ( 'NONE', #51792, #67790, #97313 ) ;
#73050 = ORIENTED_EDGE ( 'NONE', *, *, #64578, .T. ) ;
#73051 = EDGE_LOOP ( 'NONE', ( #59647, #38169, #73884, #5037 ) ) ;
#73052 = CARTESIAN_POINT ( 'NONE',  ( 2.917880565312948704, 42.63708216824729647, 12.26659068614894643 ) ) ;
#73053 = CARTESIAN_POINT ( 'NONE',  ( 13.79529636645030344, 48.26208216824728936, 14.16423886937410614 ) ) ;
#73054 = CARTESIAN_POINT ( 'NONE',  ( 17.20831665107776587, 22.88393115100078745, 7.208316651077764980 ) ) ;
#73055 = CARTESIAN_POINT ( 'NONE',  ( 22.81628187352648496, 31.83196800326375353, -3.434112377981050290 ) ) ;
#73056 = CARTESIAN_POINT ( 'NONE',  ( -13.48255862861931043, 4.084149796850864849E-16, 5.335786055104065007 ) ) ;
#73057 = PLANE ( 'NONE',  #67434 ) ;
#73058 = CARTESIAN_POINT ( 'NONE',  ( 17.08211943468705840, 45.13708216824730357, -12.26659068614894466 ) ) ;
#73059 = CARTESIAN_POINT ( 'NONE',  ( -10.70613742633244669, 15.00000000000000000, -9.778988772285387654 ) ) ;
#73060 = CARTESIAN_POINT ( 'NONE',  ( 19.84674366389459266, 8.300597817667451750, 2.638427012816836559 ) ) ;
#73061 = EDGE_CURVE ( 'NONE', #95449, #61040, #43516, .T. ) ;
#73062 = CARTESIAN_POINT ( 'NONE',  ( 3.591859063236763294, 53.29030133659708923, -11.09922568453595026 ) ) ;
#73063 = CARTESIAN_POINT ( 'NONE',  ( 2.638427012816835227, 2.467264484334120045, 9.846743663894590881 ) ) ;
#73064 = ORIENTED_EDGE ( 'NONE', *, *, #67558, .T. ) ;
#73065 = ORIENTED_EDGE ( 'NONE', *, *, #14870, .T. ) ;
#73066 = VERTEX_POINT ( 'NONE', #53952 ) ;
#73067 = CARTESIAN_POINT ( 'NONE',  ( -0.3689425029237881626, 12.42874883491396609, 10.36894250292379027 ) ) ;
#73069 = CARTESIAN_POINT ( 'NONE',  ( 19.42250999205614548, 25.98035201082150891, -5.440088680355545492 ) ) ;
#73068 = CARTESIAN_POINT ( 'NONE',  ( 12.91533473730992121, 19.52201867748816611, 10.88017736071110164 ) ) ;
#73071 = CARTESIAN_POINT ( 'NONE',  ( 22.81628187352648496, 16.83196800326374998, -3.434112377981050290 ) ) ;
#73070 = CARTESIAN_POINT ( 'NONE',  ( 1.472469842513823179, 51.42559781766745886, 4.923371831947296329 ) ) ;
#73072 = FILL_AREA_STYLE_COLOUR ( '', #2460 ) ;
#73073 = CARTESIAN_POINT ( 'NONE',  ( 17.39651004071838614, 42.93575266056826933, 6.500000000000032863 ) ) ;
#73074 = CARTESIAN_POINT ( 'NONE',  ( 0.6178305044545838731, 24.74863466993042493, 9.382169495545420901 ) ) ;
#73075 = ORIENTED_EDGE ( 'NONE', *, *, #75639, .F. ) ;
#73076 = CARTESIAN_POINT ( 'NONE',  ( 17.20831665107776587, 32.88393115100078745, 7.208316651077764980 ) ) ;
#73077 = CARTESIAN_POINT ( 'NONE',  ( 13.79529636645031943, 60.34541550158063927, -14.16423886937409904 ) ) ;
#73078 = ORIENTED_EDGE ( 'NONE', *, *, #26882, .T. ) ;
#73079 = CARTESIAN_POINT ( 'NONE',  ( 17.96484262340118221, 4.938685344154837509, 7.964842623401181321 ) ) ;
#73080 = VERTEX_POINT ( 'NONE', #56776 ) ;
#73081 = CARTESIAN_POINT ( 'NONE',  ( 15.44008868035555260, 44.73035201082151247, 9.422509992056143702 ) ) ;
#73082 = CARTESIAN_POINT ( 'NONE',  ( 10.00000000000000000, 51.81368534415484106, -10.88017736071110342 ) ) ;
#73083 = CARTESIAN_POINT ( 'NONE',  ( -0.8801773607110991993, 52.85535201082151247, -2.915334737309923874 ) ) ;
#73084 = SURFACE_STYLE_FILL_AREA ( #18627 ) ;
#73085 = CARTESIAN_POINT ( 'NONE',  ( 12.91533473730992121, 39.52201867748817676, 10.88017736071110164 ) ) ;
#73086 = FACE_OUTER_BOUND ( 'NONE', #52199, .T. ) ;
#73087 = EDGE_CURVE ( 'NONE', #38851, #36587, #7973, .T. ) ;
#73088 = VECTOR ( 'NONE', #53632, 1000.000000000000227 ) ;
#73089 = CARTESIAN_POINT ( 'NONE',  ( 10.00000000000000178, 22.25893115100078745, 9.846743663894594434 ) ) ;
#73090 = ORIENTED_EDGE ( 'NONE', *, *, #26789, .T. ) ;
#73091 = CARTESIAN_POINT ( 'NONE',  ( 19.84674366389459621, 53.50893115100078745, 7.409399052514197653E-17 ) ) ;
#73092 = FACE_OUTER_BOUND ( 'NONE', #65960, .T. ) ;
#73093 = DIRECTION ( 'NONE',  ( -1.000000000000000000, 0.000000000000000000, 0.000000000000000000 ) ) ;
#73094 = AXIS2_PLACEMENT_3D ( 'NONE', #4718, #73674, #5205 ) ;
#73095 = ORIENTED_EDGE ( 'NONE', *, *, #74328, .T. ) ;
#73096 = CARTESIAN_POINT ( 'NONE',  ( 0.000000000000000000, 0.000000000000000000, 0.000000000000000000 ) ) ;
#73097 = CARTESIAN_POINT ( 'NONE',  ( 14.54804176595378706, -0.03417435944610275333, 6.650705016170673112 ) ) ;
#73098 = CARTESIAN_POINT ( 'NONE',  ( 19.84674366389459266, 63.30059781766745886, 2.638427012816836559 ) ) ;
#73099 = CARTESIAN_POINT ( 'NONE',  ( -2.266590686148945544, 67.22041550158063217, 7.082119434687048631 ) ) ;
#73100 = DIRECTION ( 'NONE',  ( -0.000000000000000000, 0.000000000000000000, 1.000000000000000000 ) ) ;
#73101 = ORIENTED_EDGE ( 'NONE', *, *, #7589, .T. ) ;
#73102 = CARTESIAN_POINT ( 'NONE',  ( 12.63842701281683034, 37.46726448433411605, 9.846743663894596210 ) ) ;
#73103 = CARTESIAN_POINT ( 'NONE',  ( -1.099225684535947600, 59.54030133659708923, 6.408140936763237150 ) ) ;
#73104 = CARTESIAN_POINT ( 'NONE',  ( 13.43411237798105340, 5.581968003263753531, 12.81628187352647963 ) ) ;
#73105 = CARTESIAN_POINT ( 'NONE',  ( 12.63842701281683034, 12.46726448433411782, 9.846743663894596210 ) ) ;
#73106 = DIRECTION ( 'NONE',  ( 0.000000000000000000, 1.000000000000000000, 0.000000000000000000 ) ) ;
#73107 = CARTESIAN_POINT ( 'NONE',  ( 12.63842701281683922, 4.550597817667451750, -9.846743663894590881 ) ) ;
#73108 = CARTESIAN_POINT ( 'NONE',  ( 10.00000000000000000, 64.75893115100078035, -9.846743663894594434 ) ) ;
#73109 = AXIS2_PLACEMENT_3D ( 'NONE', #73177, #43183, #73670 ) ;
#73110 = CARTESIAN_POINT ( 'NONE',  ( -13.69999999999999751, 99.99999999999998579, -8.525133428036873795 ) ) ;
#73111 = VERTEX_POINT ( 'NONE', #41313 ) ;
#73112 = CARTESIAN_POINT ( 'NONE',  ( -0.8801773607110991993, 7.855352010821506248, -2.915334737309923874 ) ) ;
#73113 = CARTESIAN_POINT ( 'NONE',  ( 17.08211943468705840, 5.137082168247300906, -12.26659068614894466 ) ) ;
#73114 = CARTESIAN_POINT ( 'NONE',  ( 14.92337183194729633, 17.67559781766745175, 8.527530157486181039 ) ) ;
#73115 = B_SPLINE_CURVE_WITH_KNOTS ( 'NONE', 3,
 ( #28703, #59195, #75190, #75687 ),
 .UNSPECIFIED., .F., .F.,
 ( 4, 4 ),
 ( 0.000000000000000000, 0.002657014572711316816 ),
 .UNSPECIFIED. ) ;
#73116 = CARTESIAN_POINT ( 'NONE',  ( 4.559911319644449179, 62.23035201082150536, -9.422509992056141925 ) ) ;
#73118 = CARTESIAN_POINT ( 'NONE',  ( 7.084665262690076126, 64.10535201082150536, 10.88017736071109987 ) ) ;
#73117 = CARTESIAN_POINT ( 'NONE',  ( 19.38216949554541557, 22.24863466993041428, -9.382169495545420901 ) ) ;
#73119 = FACE_OUTER_BOUND ( 'NONE', #11983, .T. ) ;
#73120 = CARTESIAN_POINT ( 'NONE',  ( 3.699999999999999289, 0.2999999999999981570, 0.000000000000000000 ) ) ;
#73121 = CARTESIAN_POINT ( 'NONE',  ( 22.81628187352647785, 1.623634669930420271, 6.195893100308588602E-16 ) ) ;
#73122 = CARTESIAN_POINT ( 'NONE',  ( 0.6178305044545838731, -0.2513653300695798953, 9.382169495545420901 ) ) ;
#73123 = CARTESIAN_POINT ( 'NONE',  ( 19.84674366389459266, 8.300597817667451750, 2.638427012816836559 ) ) ;
#73124 = CARTESIAN_POINT ( 'NONE',  ( -9.422509992056136596, -21.51964798917849109, 5.440088680355559703 ) ) ;
#73125 = CARTESIAN_POINT ( 'NONE',  ( 0.6178305044545838731, 24.74863466993042493, 9.382169495545420901 ) ) ;
#73126 = CARTESIAN_POINT ( 'NONE',  ( -11.58434547253664171, -69.53046085282439037, -3.750000000000000000 ) ) ;
#73127 = EDGE_CURVE ( 'NONE', #70759, #46734, #22985, .T. ) ;
#73128 = CARTESIAN_POINT ( 'NONE',  ( -0.8801773607111008646, 33.27201867748817676, 2.915334737309923430 ) ) ;
#73129 = DIRECTION ( 'NONE',  ( 0.000000000000000000, 0.000000000000000000, 1.000000000000000000 ) ) ;
#73130 = CARTESIAN_POINT ( 'NONE',  ( -0.3689425029237881626, 47.42874883491396787, 10.36894250292379027 ) ) ;
#73131 = CARTESIAN_POINT ( 'NONE',  ( 1.915564264621337776, 15.00000000000000000, 14.37291249357991774 ) ) ;
#73132 = EDGE_CURVE ( 'NONE', #75285, #87937, #78862, .T. ) ;
#73133 = CARTESIAN_POINT ( 'NONE',  ( 22.81628187352648496, 31.83196800326375353, -3.434112377981050290 ) ) ;
#73134 = CARTESIAN_POINT ( 'NONE',  ( 10.00000000000000000, 26.81368534415484106, -10.88017736071110342 ) ) ;
#73135 = ADVANCED_FACE ( 'NONE', ( #11274 ), #68476, .F. ) ;
#73136 = CARTESIAN_POINT ( 'NONE',  ( 10.00000000000000000, 54.75893115100078745, -9.846743663894594434 ) ) ;
#73137 = CARTESIAN_POINT ( 'NONE',  ( 10.00000000000000000, 56.81368534415484106, -10.88017736071110342 ) ) ;
#73138 = CARTESIAN_POINT ( 'NONE',  ( 22.26659068614894466, 38.88708216824731068, 7.082119434687054849 ) ) ;
#73140 = EDGE_CURVE ( 'NONE', #75803, #53272, #46450, .T. ) ;
#73139 = FACE_OUTER_BOUND ( 'NONE', #53905, .T. ) ;
#73141 = EDGE_CURVE ( 'NONE', #57214, #44552, #32303, .T. ) ;
#73142 = UNCERTAINTY_MEASURE_WITH_UNIT (LENGTH_MEASURE( 1.000000000000000082E-05 ), #19975, 'distance_accuracy_value', 'NONE');
#73143 = CARTESIAN_POINT ( 'NONE',  ( 0.1532563361054100626, 35.80059781766745175, -2.638427012816831230 ) ) ;
#73144 = FILL_AREA_STYLE ('',( #95162 ) ) ;
#73145 = CARTESIAN_POINT ( 'NONE',  ( 12.63842701281683034, 62.46726448433410894, 9.846743663894596210 ) ) ;
#73146 = ORIENTED_EDGE ( 'NONE', *, *, #4170, .F. ) ;
#73147 = CARTESIAN_POINT ( 'NONE',  ( 19.72487221294570858, 11.86607318730075633, 6.500000000000000888 ) ) ;
#73148 = CARTESIAN_POINT ( 'NONE',  ( 2.035157376598824452, 13.68868534415483751, 7.964842623401179544 ) ) ;
#73149 = CARTESIAN_POINT ( 'NONE',  ( 2.917880565312948704, 22.63708216824730002, 12.26659068614894643 ) ) ;
#73150 = CARTESIAN_POINT ( 'NONE',  ( 19.84674366389459621, 8.508931151000785675, 7.409399052514197653E-17 ) ) ;
#73151 = STYLED_ITEM ( 'NONE', ( #41820 ), #2776 ) ;
#73152 = CARTESIAN_POINT ( 'NONE',  ( -9.990730578767625047, 46.91630561652143427, 2.900000000000000355 ) ) ;
#73153 = CARTESIAN_POINT ( 'NONE',  ( 4.559911319644449179, 33.89701867748817676, 9.422509992056141925 ) ) ;
#73154 = DIRECTION ( 'NONE',  ( -0.5948227867513371514, 0.000000000000000000, -0.8038568606172203923 ) ) ;
#73155 = CARTESIAN_POINT ( 'NONE',  ( 8.209432707284861408, 0.5000000000000004441, -12.55409154915486170 ) ) ;
#73156 = EDGE_CURVE ( 'NONE', #22113, #295, #71306, .T. ) ;
#73157 = ORIENTED_EDGE ( 'NONE', *, *, #13212, .T. ) ;
#73158 = UNCERTAINTY_MEASURE_WITH_UNIT (LENGTH_MEASURE( 1.000000000000000082E-05 ), #3395, 'distance_accuracy_value', 'NONE');
#73159 =( NAMED_UNIT ( * ) PLANE_ANGLE_UNIT ( ) SI_UNIT ( $, .RADIAN. ) );
#73160 = CARTESIAN_POINT ( 'NONE',  ( 1.472469842513823179, 41.42559781766745886, 4.923371831947296329 ) ) ;
#73161 = ORIENTED_EDGE ( 'NONE', *, *, #89986, .T. ) ;
#73162 = ORIENTED_EDGE ( 'NONE', *, *, #70206, .T. ) ;
#73163 = CARTESIAN_POINT ( 'NONE',  ( 9.742785792574936821, 10.83846884451820891, -5.625000000000004441 ) ) ;
#73164 = CARTESIAN_POINT ( 'NONE',  ( 20.36894250292379738, 9.928748834913966093, -10.36894250292379027 ) ) ;
#73165 = CARTESIAN_POINT ( 'NONE',  ( -4.164238869374098151, 6.595415501580634832, -3.795296366450310543 ) ) ;
#73166 = CARTESIAN_POINT ( 'NONE',  ( 20.88017736071110164, 50.35535201082151247, 2.915334737309930979 ) ) ;
#73167 = CARTESIAN_POINT ( 'NONE',  ( 17.08211943468705130, 53.47041550158063217, 12.26659068614894998 ) ) ;
#73168 = CARTESIAN_POINT ( 'NONE',  ( 16.40814093676323893, 5.790301336597087456, 11.09922568453595026 ) ) ;
#73169 = CARTESIAN_POINT ( 'NONE',  ( 0.1532563361054083140, 31.00893115100078390, 1.131784320476157264E-15 ) ) ;
#73170 = CARTESIAN_POINT ( 'NONE',  ( -10.77730536144846596, -98.63085534186639336, 3.750000000000000000 ) ) ;
#73172 = CARTESIAN_POINT ( 'NONE',  ( 19.38216949554541557, 12.24863466993041961, -9.382169495545420901 ) ) ;
#73171 = CARTESIAN_POINT ( 'NONE',  ( -0.8801773607111008646, 28.27201867748817321, 2.915334737309923430 ) ) ;
#73173 = CARTESIAN_POINT ( 'NONE',  ( 20.36894250292379382, 3.678748834913967869, 10.36894250292379205 ) ) ;
#73174 = CARTESIAN_POINT ( 'NONE',  ( -0.3689425029237881626, 52.42874883491396076, 10.36894250292379027 ) ) ;
#73175 = CARTESIAN_POINT ( 'NONE',  ( 2.917880565312948704, 67.63708216824730357, 12.26659068614894643 ) ) ;
#73176 = CYLINDRICAL_SURFACE ( 'NONE', #21079, 15.00000000000000000 ) ;
#73177 = CARTESIAN_POINT ( 'NONE',  ( 3.969999999999999751, 10.25000000000000000, 2.750000000000000000 ) ) ;
#73178 = EDGE_CURVE ( 'NONE', #88806, #83600, #25800, .T. ) ;
#73179 =( GEOMETRIC_REPRESENTATION_CONTEXT ( 3 ) GLOBAL_UNCERTAINTY_ASSIGNED_CONTEXT ( ( #72167 ) ) GLOBAL_UNIT_ASSIGNED_CONTEXT ( ( #72086, #80083, #48597 ) ) REPRESENTATION_CONTEXT ( 'NONE', 'WORKASPACE' ) );
#73180 = LINE ( 'NONE', #95195, #15818 ) ;
#73181 = ORIENTED_EDGE ( 'NONE', *, *, #40008, .T. ) ;
#73182 = DIRECTION ( 'NONE',  ( 0.000000000000000000, 0.000000000000000000, 1.000000000000000000 ) ) ;
#73183 = VERTEX_POINT ( 'NONE', #18296 ) ;
#73184 = ORIENTED_EDGE ( 'NONE', *, *, #58950, .T. ) ;
#73185 = CARTESIAN_POINT ( 'NONE',  ( -2.266590686148945544, 42.22041550158063217, 7.082119434687048631 ) ) ;
#73186 = CARTESIAN_POINT ( 'NONE',  ( 1.472469842513823179, 51.42559781766745886, 4.923371831947296329 ) ) ;
#73187 = CARTESIAN_POINT ( 'NONE',  ( 10.00000000000000000, 51.81368534415484106, -10.88017736071110342 ) ) ;
#73188 =( GEOMETRIC_REPRESENTATION_CONTEXT ( 3 ) GLOBAL_UNCERTAINTY_ASSIGNED_CONTEXT ( ( #59269 ) ) GLOBAL_UNIT_ASSIGNED_CONTEXT ( ( #28776, #96812, #11805 ) ) REPRESENTATION_CONTEXT ( 'NONE', 'WORKASPACE' ) );
#73189 = DIRECTION ( 'NONE',  ( 0.8870108331782150524, 0.000000000000000000, 0.4617486132350466788 ) ) ;
#73190 = EDGE_CURVE ( 'NONE', #11556, #6265, #98743, .T. ) ;
#73191 = TOROIDAL_SURFACE ( 'NONE', #65194, 2.250000000000001332, 0.2500000000000000000 ) ;
#73192 = B_SPLINE_CURVE_WITH_KNOTS ( 'NONE', 3,
 ( #58922, #49945, #12926, #19937, #20935, #43421 ),
 .UNSPECIFIED., .F., .F.,
 ( 4, 2, 4 ),
 ( 3.409110551495123060E-05, 0.0004400426677367748622, 0.0008459942299585984735 ),
 .UNSPECIFIED. ) ;
#73193 = CARTESIAN_POINT ( 'NONE',  ( 20.88017736071110164, 55.35535201082149825, 2.915334737309930979 ) ) ;
#73194 = CARTESIAN_POINT ( 'NONE',  ( -2.816281873526473856, 54.33196800326376064, 3.434112377981055619 ) ) ;
#73195 = CARTESIAN_POINT ( 'NONE',  ( 12.81628187352647252, 1.831968003263755085, -3.434112377981059172 ) ) ;
#73196 = ORIENTED_EDGE ( 'NONE', *, *, #74509, .T. ) ;
#73197 = CARTESIAN_POINT ( 'NONE',  ( 4.559911319644449179, 48.89701867748817676, 9.422509992056141925 ) ) ;
#73198 = CARTESIAN_POINT ( 'NONE',  ( -0.3689425029237898834, 16.17874883491396076, -10.36894250292378850 ) ) ;
#73199 = CARTESIAN_POINT ( 'NONE',  ( 3.591859063236761518, 29.95696800326375708, 11.09922568453594849 ) ) ;
#73200 = ORIENTED_EDGE ( 'NONE', *, *, #81181, .T. ) ;
#73201 = CARTESIAN_POINT ( 'NONE',  ( -1.099225684535947600, 48.70696800326375353, -6.408140936763238038 ) ) ;
#73202 = CARTESIAN_POINT ( 'NONE',  ( 7.084665262690076126, 19.10535201082150181, 10.88017736071109987 ) ) ;
#73203 = CARTESIAN_POINT ( 'NONE',  ( 19.84674366389459621, 33.50893115100078745, 7.409399052514197653E-17 ) ) ;
#73204 = CARTESIAN_POINT ( 'NONE',  ( 15.44008868035555260, 19.73035201082150536, 9.422509992056143702 ) ) ;
#73205 = CYLINDRICAL_SURFACE ( 'NONE', #76709, 15.00000000000000000 ) ;
#73206 = CARTESIAN_POINT ( 'NONE',  ( 12.63842701281683922, 39.55059781766744464, -9.846743663894590881 ) ) ;
#73208 = VERTEX_POINT ( 'NONE', #48779 ) ;
#73207 = CARTESIAN_POINT ( 'NONE',  ( -0.8801773607111008646, 68.27201867748817676, 2.915334737309923430 ) ) ;
#73209 = FACE_OUTER_BOUND ( 'NONE', #32212, .T. ) ;
#73210 = CARTESIAN_POINT ( 'NONE',  ( 0.5774900079438607392, 68.48035201082150536, 5.440088680355550821 ) ) ;
#73211 = CARTESIAN_POINT ( 'NONE',  ( 18.95386800104995828, 8.238109087357269544, -6.499999999999999112 ) ) ;
#73212 = DIRECTION ( 'NONE',  ( 0.000000000000000000, 1.000000000000000000, 0.000000000000000000 ) ) ;
#73213 = CARTESIAN_POINT ( 'NONE',  ( 18.52753015748617571, 23.09226448433411960, 4.923371831947298993 ) ) ;
#73214 = CARTESIAN_POINT ( 'NONE',  ( 3.591859063236761518, 19.95696800326375353, 11.09922568453594849 ) ) ;
#73215 = CARTESIAN_POINT ( 'NONE',  ( 0.000000000000000000, 14.49999999999999822, 0.000000000000000000 ) ) ;
#73216 = EDGE_CURVE ( 'NONE', #65756, #55747, #64750, .T. ) ;
#73217 = ORIENTED_EDGE ( 'NONE', *, *, #52104, .F. ) ;
#73218 = AXIS2_PLACEMENT_3D ( 'NONE', #26672, #12654, #88157 ) ;
#73219 = CARTESIAN_POINT ( 'NONE',  ( 12.63842701281683034, 42.46726448433412315, 9.846743663894596210 ) ) ;
#73220 = CARTESIAN_POINT ( 'NONE',  ( 7.313705784284555200, 14.49999999999999112, 13.09617149020753146 ) ) ;
#73221 = CARTESIAN_POINT ( 'NONE',  ( 24.16423886937410614, 24.51208216824730002, -3.795296366450302550 ) ) ;
#73222 = CARTESIAN_POINT ( 'NONE',  ( 19.84674366389459266, 38.71726448433412315, -2.638427012816827677 ) ) ;
#73223 = CARTESIAN_POINT ( 'NONE',  ( 22.81628187352647785, 51.41530133659708923, 3.434112377981063169 ) ) ;
#73225 = DIRECTION ( 'NONE',  ( 1.000000000000000000, 0.000000000000000000, 0.000000000000000000 ) ) ;
#73224 = DIRECTION ( 'NONE',  ( 0.000000000000000000, 1.000000000000000000, 0.000000000000000000 ) ) ;
#73226 = CARTESIAN_POINT ( 'NONE',  ( 20.88017736071110164, 60.35535201082151957, 2.915334737309930979 ) ) ;
#73227 = CARTESIAN_POINT ( 'NONE',  ( 3.591859063236763294, 13.29030133659708746, -11.09922568453595026 ) ) ;
#73228 = CARTESIAN_POINT ( 'NONE',  ( -0.04068437667222076642, 67.21974360917720048, -6.396802510829771471 ) ) ;
#73229 = EDGE_CURVE ( 'NONE', #13064, #56877, #20260, .T. ) ;
#73230 = CARTESIAN_POINT ( 'NONE',  ( 14.92337183194729988, 39.34226448433412315, -8.527530157486177487 ) ) ;
#73231 = CARTESIAN_POINT ( 'NONE',  ( -0.8801773607111008646, 43.27201867748817676, 2.915334737309923430 ) ) ;
#73232 = CARTESIAN_POINT ( 'NONE',  ( 22.81628187352647785, 31.62363466993042138, 6.195893100308588602E-16 ) ) ;
#73233 = CARTESIAN_POINT ( 'NONE',  ( 18.52753015748618282, 28.92559781766745175, -4.923371831947291888 ) ) ;
#73234 = DIRECTION ( 'NONE',  ( 1.000000000000000000, 0.000000000000000000, 0.000000000000000000 ) ) ;
#73235 = CARTESIAN_POINT ( 'NONE',  ( -2.189666204609396427, -2.219226321806264916E-16, 14.46180170876166748 ) ) ;
#73236 = CARTESIAN_POINT ( 'NONE',  ( 12.91533473730992121, 29.52201867748817321, 10.88017736071110164 ) ) ;
#73237 = ORIENTED_EDGE ( 'NONE', *, *, #27324, .T. ) ;
#73238 = DIRECTION ( 'NONE',  ( -0.000000000000000000, -0.000000000000000000, -1.000000000000000000 ) ) ;
#73239 = CARTESIAN_POINT ( 'NONE',  ( 6.829574850505126804, -88.00372650098204019, 2.750000000000002665 ) ) ;
#73241 = CARTESIAN_POINT ( 'NONE',  ( 19.42250999205614193, 30.14701867748817321, 5.440088680355555262 ) ) ;
#73240 = CARTESIAN_POINT ( 'NONE',  ( 0.1532563361054083140, 61.00893115100078745, 1.131784320476157264E-15 ) ) ;
#73242 = DIRECTION ( 'NONE',  ( 1.000000000000000000, 0.000000000000000000, 0.000000000000000000 ) ) ;
#73243 = CARTESIAN_POINT ( 'NONE',  ( 20.88017736071110164, 60.35535201082151957, 2.915334737309930979 ) ) ;
#73244 = CIRCLE ( 'NONE', #57259, 2.000000000000000888 ) ;
#73246 = PLANE ( 'NONE',  #30329 ) ;
#73245 = CARTESIAN_POINT ( 'NONE',  ( 15.44008868035555260, 24.73035201082150891, 9.422509992056143702 ) ) ;
#73247 = CARTESIAN_POINT ( 'NONE',  ( -4.020549461440724670, 0.000000000000000000, -3.684154808197088293 ) ) ;
#73248 = CARTESIAN_POINT ( 'NONE',  ( 1.472469842513823179, 30.59226448433411960, -4.923371831947296329 ) ) ;
#73249 = CARTESIAN_POINT ( 'NONE',  ( 18.52753015748618282, 48.92559781766745886, -4.923371831947291888 ) ) ;
#73250 = CYLINDRICAL_SURFACE ( 'NONE', #78117, 15.00000000000000000 ) ;
#73252 = SURFACE_STYLE_USAGE ( .BOTH. , #72752 ) ;
#73251 = CARTESIAN_POINT ( 'NONE',  ( 13.79529636645030344, 53.26208216824730357, 14.16423886937410614 ) ) ;
#73253 = DIRECTION ( 'NONE',  ( -0.000000000000000000, -1.000000000000000000, -0.000000000000000000 ) ) ;
#73255 = CARTESIAN_POINT ( 'NONE',  ( 6.204703633549690345, 15.76208216824730179, -14.16423886937410259 ) ) ;
#73254 = VECTOR ( 'NONE', #10131, 1000.000000000000000 ) ;
#73256 = CIRCLE ( 'NONE', #1429, 1.500000000000001332 ) ;
#73257 = CARTESIAN_POINT ( 'NONE',  ( 17.08211943468705840, 40.13708216824731068, -12.26659068614894466 ) ) ;
#73258 = CARTESIAN_POINT ( 'NONE',  ( 16.40814093676323893, 10.79030133659708923, 11.09922568453595026 ) ) ;
#73259 = ADVANCED_FACE ( 'NONE', ( #3794 ), #86472, .T. ) ;
#73260 = CARTESIAN_POINT ( 'NONE',  ( -3.585700530862828028, -2.697939587593689570, 2.750000000000001332 ) ) ;
#73261 = EDGE_LOOP ( 'NONE', ( #63623, #28413, #57824, #9836 ) ) ;
#73262 = CARTESIAN_POINT ( 'NONE',  ( 10.00000000000000178, 19.31368534415484106, 10.88017736071110342 ) ) ;
#73263 = CARTESIAN_POINT ( 'NONE',  ( 5.076628168052704559, 30.17559781766745175, -8.527530157486179263 ) ) ;
#73265 = CARTESIAN_POINT ( 'NONE',  ( -11.13303098458958296, 89.96146600687833939, -6.578309274437964760 ) ) ;
#73264 = PLANE ( 'NONE',  #40395 ) ;
#73266 = CARTESIAN_POINT ( 'NONE',  ( 4.559911319644449179, 58.89701867748817676, 9.422509992056141925 ) ) ;
#73267 = CARTESIAN_POINT ( 'NONE',  ( 0.4400000000000020006, 1.019547802438468986, 2.750000000000000000 ) ) ;
#73268 = ADVANCED_FACE ( 'NONE', ( #95283 ), #86319, .T. ) ;
#73269 = CARTESIAN_POINT ( 'NONE',  ( 3.591859063236761518, 64.95696800326376774, 11.09922568453594849 ) ) ;
#73270 = CARTESIAN_POINT ( 'NONE',  ( 19.38216949554541557, 27.24863466993041783, -9.382169495545420901 ) ) ;
#73271 = CARTESIAN_POINT ( 'NONE',  ( 2.791683348922240793, 21.63393115100078745, 7.208316651077764092 ) ) ;
#73272 = ORIENTED_EDGE ( 'NONE', *, *, #30715, .F. ) ;
#73273 = DIRECTION ( 'NONE',  ( -1.000000000000000000, 0.000000000000000000, 0.000000000000000000 ) ) ;
#73274 = DIRECTION ( 'NONE',  ( -0.000000000000000000, -1.000000000000000000, -0.000000000000000000 ) ) ;
#73275 = CARTESIAN_POINT ( 'NONE',  ( 7.084665262690076126, 4.105352010821503583, 10.88017736071109987 ) ) ;
#73276 = CARTESIAN_POINT ( 'NONE',  ( 15.44008868035555260, 9.730352010821505360, 9.422509992056143702 ) ) ;
#73277 = CARTESIAN_POINT ( 'NONE',  ( 24.16423886937409904, 39.09541550158062506, 3.795296366450317205 ) ) ;
#73278 = CARTESIAN_POINT ( 'NONE',  ( 7.084665262690076126, 32.02201867748816966, -10.88017736071110164 ) ) ;
#73279 = CARTESIAN_POINT ( 'NONE',  ( 19.42250999205614193, 60.14701867748817676, 5.440088680355555262 ) ) ;
#73280 = CARTESIAN_POINT ( 'NONE',  ( 0.000000000000000000, 14.49999999999999822, 0.000000000000000000 ) ) ;
#73281 = CARTESIAN_POINT ( 'NONE',  ( -9.159723438033276821, 15.00000000000000000, 10.91613331444536250 ) ) ;
#73282 = CARTESIAN_POINT ( 'NONE',  ( 14.92337183194729633, 7.675597817667451750, 8.527530157486181039 ) ) ;
#73283 = FILL_AREA_STYLE ('',( #57295 ) ) ;
#73284 = CARTESIAN_POINT ( 'NONE',  ( 2.791683348922237240, 10.38393115100078390, -7.208316651077763204 ) ) ;
#73285 = CARTESIAN_POINT ( 'NONE',  ( 2.791683348922240793, 41.63393115100078745, 7.208316651077764092 ) ) ;
#73286 = CARTESIAN_POINT ( 'NONE',  ( 2.791683348922237240, 65.38393115100078035, -7.208316651077763204 ) ) ;
#73287 =( GEOMETRIC_REPRESENTATION_CONTEXT ( 3 ) GLOBAL_UNCERTAINTY_ASSIGNED_CONTEXT ( ( #49177 ) ) GLOBAL_UNIT_ASSIGNED_CONTEXT ( ( #49709, #10752, #93749 ) ) REPRESENTATION_CONTEXT ( 'NONE', 'WORKASPACE' ) );
#73288 = CARTESIAN_POINT ( 'NONE',  ( -0.8801773607111008646, 23.27201867748817676, 2.915334737309923430 ) ) ;
#73289 = ORIENTED_EDGE ( 'NONE', *, *, #84582, .T. ) ;
#73290 = CARTESIAN_POINT ( 'NONE',  ( 6.565887622018943937, 45.16530133659708923, 12.81628187352647430 ) ) ;
#73291 = CARTESIAN_POINT ( 'NONE',  ( 6.898461952320343649, 4.875757609050324087E-16, 12.75387089053313971 ) ) ;
#73292 = CARTESIAN_POINT ( 'NONE',  ( 0.5774900079438590739, 67.64701867748817676, -5.440088680355550821 ) ) ;
#73293 = CARTESIAN_POINT ( 'NONE',  ( -1.099225684535947600, 49.54030133659708923, 6.408140936763237150 ) ) ;
#73295 = CARTESIAN_POINT ( 'NONE',  ( 12.63842701281683922, 34.55059781766745886, -9.846743663894590881 ) ) ;
#73294 = CARTESIAN_POINT ( 'NONE',  ( 13.79529636645030344, 53.26208216824730357, 14.16423886937410614 ) ) ;
#73296 = CARTESIAN_POINT ( 'NONE',  ( -0.1503990784575247319, 47.22266099184918886, -6.262539305110083276 ) ) ;
#73297 = FACE_OUTER_BOUND ( 'NONE', #9114, .T. ) ;
#73298 = CARTESIAN_POINT ( 'NONE',  ( 2.917880565312950480, 15.97041550158063217, -12.26659068614894821 ) ) ;
#73299 = CARTESIAN_POINT ( 'NONE',  ( -2.266590686148945544, 27.22041550158063572, 7.082119434687048631 ) ) ;
#73300 = CARTESIAN_POINT ( 'NONE',  ( 18.52753015748618282, 48.92559781766745886, -4.923371831947291888 ) ) ;
#73301 = CARTESIAN_POINT ( 'NONE',  ( 3.753761956877445627, 0.000000000000000000, 3.955639745193266776 ) ) ;
#73302 = CARTESIAN_POINT ( 'NONE',  ( 17.96484262340118221, 41.18868534415484106, -7.964842623401177768 ) ) ;
#73303 = ADVANCED_FACE ( 'NONE', ( #49779 ), #48305, .F. ) ;
#73304 = CARTESIAN_POINT ( 'NONE',  ( 12.91533473730992121, 54.52201867748816255, 10.88017736071110164 ) ) ;
#73305 = MECHANICAL_DESIGN_GEOMETRIC_PRESENTATION_REPRESENTATION (  '', ( #90863 ), #39845 ) ;
#73306 = EDGE_LOOP ( 'NONE', ( #21534, #27538, #54396, #63567 ) ) ;
#73307 = CARTESIAN_POINT ( 'NONE',  ( 3.591859063236763294, 43.29030133659708923, -11.09922568453595026 ) ) ;
#73308 = CARTESIAN_POINT ( 'NONE',  ( 20.88017736071110164, 55.35535201082149825, 2.915334737309930979 ) ) ;
#73309 = EDGE_LOOP ( 'NONE', ( #13680, #17765, #95359, #42667 ) ) ;
#73310 =( NAMED_UNIT ( * ) PLANE_ANGLE_UNIT ( ) SI_UNIT ( $, .RADIAN. ) );
#73311 = CARTESIAN_POINT ( 'NONE',  ( 13.55101055326455928, 14.76984994142753038, -6.292244619294638852 ) ) ;
#73312 = CARTESIAN_POINT ( 'NONE',  ( 4.873787042390699931, -0.03417435944610275333, 13.39061984619922718 ) ) ;
#73313 = ORIENTED_EDGE ( 'NONE', *, *, #52279, .T. ) ;
#73314 = CARTESIAN_POINT ( 'NONE',  ( -0.1503990784575359729, 13.10158574516642105, 6.262539305110062848 ) ) ;
#73315 = CARTESIAN_POINT ( 'NONE',  ( 7.084665262690076126, 9.105352010821503583, 10.88017736071109987 ) ) ;
#73316 = CARTESIAN_POINT ( 'NONE',  ( -5.056330833731841778, 15.00000000000000000, 13.58983143750696421 ) ) ;
#73317 = CARTESIAN_POINT ( 'NONE',  ( 7.084665262690076126, 2.022018677488171434, -10.88017736071110164 ) ) ;
#73318 = CARTESIAN_POINT ( 'NONE',  ( -0.3689425029237881626, 17.42874883491397142, 10.36894250292379027 ) ) ;
#73319 = CARTESIAN_POINT ( 'NONE',  ( 2.035157376598822676, 17.43868534415483751, -7.964842623401177768 ) ) ;
#73320 = CARTESIAN_POINT ( 'NONE',  ( 7.361572987183170547, 57.05059781766744464, 9.846743663894590881 ) ) ;
#73321 = ORIENTED_EDGE ( 'NONE', *, *, #20672, .F. ) ;
#73322 = CARTESIAN_POINT ( 'NONE',  ( 0.6178305044545818747, -1.501365330069579951, -9.382169495545419124 ) ) ;
#73323 = EDGE_LOOP ( 'NONE', ( #25812, #70032, #73866, #20708, #15269, #93664 ) ) ;
#73324 = CARTESIAN_POINT ( 'NONE',  ( 12.91533473730992121, 49.52201867748817676, 10.88017736071110164 ) ) ;
#73325 = DIRECTION ( 'NONE',  ( -0.4924235601034586685, 0.000000000000000000, -0.8703556959399044723 ) ) ;
#73326 = CARTESIAN_POINT ( 'NONE',  ( -2.816281873526471635, 33.91530133659708213, -3.434112377981056508 ) ) ;
#73328 = CARTESIAN_POINT ( 'NONE',  ( 7.347880794884118750E-16, 17.03999999999999915, 0.000000000000000000 ) ) ;
#73327 = CARTESIAN_POINT ( 'NONE',  ( 7.084665262690076126, 9.105352010821503583, 10.88017736071109987 ) ) ;
#73329 = CARTESIAN_POINT ( 'NONE',  ( 7.084665262690076126, 67.02201867748817676, -10.88017736071110164 ) ) ;
#73330 = CARTESIAN_POINT ( 'NONE',  ( 0.5774900079438590739, 22.64701867748817321, -5.440088680355550821 ) ) ;
#73331 = COLOUR_RGB ( '', 0.09019608, 0.27058824, 0.51372549) ;
#73332 = CARTESIAN_POINT ( 'NONE',  ( 3.591859063236763294, 58.29030133659708923, -11.09922568453595026 ) ) ;
#73333 = CARTESIAN_POINT ( 'NONE',  ( 12.91533473730993009, 26.60535201082150536, -10.88017736071109987 ) ) ;
#73334 = DIRECTION ( 'NONE',  ( -0.9170600743851266001, 0.000000000000000000, 0.3987490689252404241 ) ) ;
#73335 = CARTESIAN_POINT ( 'NONE',  ( 16.40814093676323893, 35.79030133659708923, 11.09922568453595026 ) ) ;
#73336 = CARTESIAN_POINT ( 'NONE',  ( -0.8801773607111009756, 53.06368534415484106, 1.068504757029289695E-15 ) ) ;
#73337 = CARTESIAN_POINT ( 'NONE',  ( 7.361572987183170547, 62.05059781766745886, 9.846743663894590881 ) ) ;
#73338 = EDGE_LOOP ( 'NONE', ( #59667, #46767, #65735, #51811 ) ) ;
#73339 = VECTOR ( 'NONE', #16653, 1000.000000000000000 ) ;
#73340 = CARTESIAN_POINT ( 'NONE',  ( 14.92337183194729633, 7.675597817667451750, 8.527530157486181039 ) ) ;
#73341 = CARTESIAN_POINT ( 'NONE',  ( 2.791683348922237240, 60.38393115100078745, -7.208316651077763204 ) ) ;
#73343 = CARTESIAN_POINT ( 'NONE',  ( 17.20831665107776587, 54.13393115100079456, -7.208316651077762316 ) ) ;
#73342 = DIRECTION ( 'NONE',  ( 0.000000000000000000, 1.000000000000000000, 0.000000000000000000 ) ) ;
#73344 = CARTESIAN_POINT ( 'NONE',  ( 12.91533473730993009, 16.60535201082150891, -10.88017736071109987 ) ) ;
#73345 = CARTESIAN_POINT ( 'NONE',  ( 7.361572987183170547, 42.05059781766745886, 9.846743663894590881 ) ) ;
#73346 = DIRECTION ( 'NONE',  ( 0.000000000000000000, 0.000000000000000000, -1.000000000000000000 ) ) ;
#73347 =( NAMED_UNIT ( * ) SI_UNIT ( $, .STERADIAN. ) SOLID_ANGLE_UNIT ( ) );
#73348 = EDGE_CURVE ( 'NONE', #80329, #94129, #40322, .T. ) ;
#73349 = VECTOR ( 'NONE', #24501, 1000.000000000000000 ) ;
#73351 = CARTESIAN_POINT ( 'NONE',  ( 17.20831665107776587, 7.883931151000784787, 7.208316651077764980 ) ) ;
#73350 = CARTESIAN_POINT ( 'NONE',  ( 12.63842701281683034, 47.46726448433412315, 9.846743663894596210 ) ) ;
#73352 = SURFACE_STYLE_USAGE ( .BOTH. , #96377 ) ;
#73354 = ORIENTED_EDGE ( 'NONE', *, *, #92279, .F. ) ;
#73353 = CARTESIAN_POINT ( 'NONE',  ( 2.791683348922237240, 60.38393115100078745, -7.208316651077763204 ) ) ;
#73355 = CARTESIAN_POINT ( 'NONE',  ( 10.00000000000000178, 35.37363466993042493, 12.81628187352647608 ) ) ;
#73356 = CARTESIAN_POINT ( 'NONE',  ( 0.1532563361054083140, 46.00893115100079456, 1.131784320476157264E-15 ) ) ;
#73357 = CARTESIAN_POINT ( 'NONE',  ( 12.07856007377819907, 15.00000000000000000, 8.022367888854917695 ) ) ;
#73358 = CARTESIAN_POINT ( 'NONE',  ( 22.26659068614894466, 58.88708216824729647, 7.082119434687054849 ) ) ;
#73359 = CARTESIAN_POINT ( 'NONE',  ( 1.472469842513823179, 36.42559781766745175, 4.923371831947296329 ) ) ;
#73360 = CARTESIAN_POINT ( 'NONE',  ( 19.59274024544212978, 82.56817434445966342, 5.128398454507835602 ) ) ;
#73361 = CARTESIAN_POINT ( 'NONE',  ( 24.16423886937410614, 54.30374883491396787, 8.672049930838204340E-16 ) ) ;
#73362 = CARTESIAN_POINT ( 'NONE',  ( -10.19302435262559037, 44.02336987076795083, 0.000000000000000000 ) ) ;
#73363 = CARTESIAN_POINT ( 'NONE',  ( -0.8801773607111008646, 23.27201867748817676, 2.915334737309923430 ) ) ;
#73364 = CARTESIAN_POINT ( 'NONE',  ( -4.164238869374099039, 41.80374883491397497, 8.674139862899312516E-16 ) ) ;
#73366 = CARTESIAN_POINT ( 'NONE',  ( -12.15129255554601428, 15.00000000000000000, -10.40305174771256524 ) ) ;
#73365 = CARTESIAN_POINT ( 'NONE',  ( -4.164238869374099927, 52.01208216824729647, 3.795296366450308767 ) ) ;
#73367 = CARTESIAN_POINT ( 'NONE',  ( 20.88017736071110164, 5.355352010821504471, 2.915334737309930979 ) ) ;
#73368 = CARTESIAN_POINT ( 'NONE',  ( 14.92337183194729633, 17.67559781766745175, 8.527530157486181039 ) ) ;
#73369 = CARTESIAN_POINT ( 'NONE',  ( 0.6178305044545838731, -0.2513653300695798953, 9.382169495545420901 ) ) ;
#73370 = CARTESIAN_POINT ( 'NONE',  ( -0.8801773607111008646, 48.27201867748816966, 2.915334737309923430 ) ) ;
#73371 = CARTESIAN_POINT ( 'NONE',  ( 1.042145700049421198, 39.74216108172002748, -6.499999999999917399 ) ) ;
#73372 = CARTESIAN_POINT ( 'NONE',  ( 7.361572987183170547, 47.05059781766745175, 9.846743663894590881 ) ) ;
#73373 = CARTESIAN_POINT ( 'NONE',  ( 10.93781366033340063, 0.5000000000000004441, 10.26470809774072634 ) ) ;
#73374 = DIRECTION ( 'NONE',  ( 1.000000000000000000, -0.000000000000000000, -0.000000000000000000 ) ) ;
#73375 = CARTESIAN_POINT ( 'NONE',  ( 14.91886229468048519, 14.76984964723650151, 0.8060919667645776165 ) ) ;
#73376 = EDGE_CURVE ( 'NONE', #76972, #40989, #34775, .T. ) ;
#73377 = ORIENTED_EDGE ( 'NONE', *, *, #74320, .F. ) ;
#73378 = CARTESIAN_POINT ( 'NONE',  ( 6.204703633549690345, 27.84541550158063217, 14.16423886937410082 ) ) ;
#73379 = CARTESIAN_POINT ( 'NONE',  ( 0.000000000000000000, 15.00000000000000000, 0.000000000000000000 ) ) ;
#73381 = CARTESIAN_POINT ( 'NONE',  ( -5.204170427930421283E-15, 6.671802177851543725, -11.25000000000000178 ) ) ;
#73380 = CARTESIAN_POINT ( 'NONE',  ( -6.874974626955391521, -78.82095024088569346, -2.500000000000000000 ) ) ;
#73382 = CARTESIAN_POINT ( 'NONE',  ( 10.00000000000000000, 16.81368534415483751, -10.88017736071110342 ) ) ;
#73383 = CARTESIAN_POINT ( 'NONE',  ( 13.43411237798105340, 35.58196800326375353, 12.81628187352647963 ) ) ;
#73384 = EDGE_CURVE ( 'NONE', #73524, #51377, #28264, .T. ) ;
#73385 = CARTESIAN_POINT ( 'NONE',  ( -5.204170427930422072E-15, 8.438309369127518167, -11.92686044187656513 ) ) ;
#73386 = CARTESIAN_POINT ( 'NONE',  ( -13.82671409943291785, 0.000000000000000000, -3.447387012295409114 ) ) ;
#73387 = VERTEX_POINT ( 'NONE', #12767 ) ;
#73388 = CARTESIAN_POINT ( 'NONE',  ( 10.58223187591007886, 0.2306972965111904750, -10.54772123337530587 ) ) ;
#73389 = CARTESIAN_POINT ( 'NONE',  ( -4.164238869374099927, 27.01208216824730357, 3.795296366450308767 ) ) ;
#73390 = CARTESIAN_POINT ( 'NONE',  ( 6.204703633549690345, 5.762082168247301794, -14.16423886937410259 ) ) ;
#73391 = CARTESIAN_POINT ( 'NONE',  ( 15.44008868035555260, 19.73035201082150536, 9.422509992056143702 ) ) ;
#73392 = DIRECTION ( 'NONE',  ( 0.000000000000000000, -0.000000000000000000, 1.000000000000000000 ) ) ;
#73393 = CARTESIAN_POINT ( 'NONE',  ( 0.000000000000000000, 15.00000000000000000, 0.000000000000000000 ) ) ;
#73394 = CARTESIAN_POINT ( 'NONE',  ( 7.084665262690076126, 34.10535201082151247, 10.88017736071109987 ) ) ;
#73395 = CARTESIAN_POINT ( 'NONE',  ( 4.559911319644449179, 57.23035201082150536, -9.422509992056141925 ) ) ;
#73396 = CARTESIAN_POINT ( 'NONE',  ( -2.816281873526473856, 9.331968003263753531, 3.434112377981055619 ) ) ;
#73397 = DIRECTION ( 'NONE',  ( -1.000000000000000000, 0.000000000000000000, 0.000000000000000000 ) ) ;
#73398 = FACE_OUTER_BOUND ( 'NONE', #16499, .T. ) ;
#73399 = CARTESIAN_POINT ( 'NONE',  ( 19.84674366389459266, 18.30059781766745175, 2.638427012816836559 ) ) ;
#73400 =( NAMED_UNIT ( * ) PLANE_ANGLE_UNIT ( ) SI_UNIT ( $, .RADIAN. ) );
#73401 = CARTESIAN_POINT ( 'NONE',  ( 0.5774900079438607392, 38.48035201082150536, 5.440088680355550821 ) ) ;
#73402 = CARTESIAN_POINT ( 'NONE',  ( -2.816281873526473856, 4.123634669930420493, 9.499525473075851096E-16 ) ) ;
#73403 = CARTESIAN_POINT ( 'NONE',  ( 7.084665262690076126, 59.10535201082150536, 10.88017736071109987 ) ) ;
#73404 = CARTESIAN_POINT ( 'NONE',  ( 14.92337183194729633, 27.67559781766745530, 8.527530157486181039 ) ) ;
#73405 = CARTESIAN_POINT ( 'NONE',  ( 10.00000000000000178, 45.37363466993041783, 12.81628187352647608 ) ) ;
#73406 = CARTESIAN_POINT ( 'NONE',  ( 19.84674366389459621, 8.508931151000785675, 7.409399052514197653E-17 ) ) ;
#73407 = ORIENTED_EDGE ( 'NONE', *, *, #59118, .F. ) ;
#73408 = LINE ( 'NONE', #4936, #30933 ) ;
#73409 = FACE_OUTER_BOUND ( 'NONE', #19568, .T. ) ;
#73410 = CARTESIAN_POINT ( 'NONE',  ( 15.44008868035555793, 16.39701867748817321, -9.422509992056140149 ) ) ;
#73412 = CARTESIAN_POINT ( 'NONE',  ( -2.266590686148945544, 22.22041550158063572, 7.082119434687048631 ) ) ;
#73411 = CARTESIAN_POINT ( 'NONE',  ( -2.816281873526473856, 54.12363466993041783, 9.499525473075851096E-16 ) ) ;
#73413 = CARTESIAN_POINT ( 'NONE',  ( 12.63842701281683922, 29.55059781766745175, -9.846743663894590881 ) ) ;
#73414 = AXIS2_PLACEMENT_3D ( 'NONE', #25639, #48116, #86623 ) ;
#73415 = CARTESIAN_POINT ( 'NONE',  ( 7.084665262690076126, 19.10535201082150181, 10.88017736071109987 ) ) ;
#73416 = CARTESIAN_POINT ( 'NONE',  ( 22.26659068614895176, 64.72041550158064638, -7.082119434687042414 ) ) ;
#73417 = ORIENTED_EDGE ( 'NONE', *, *, #1883, .F. ) ;
#73418 = AXIS2_PLACEMENT_3D ( 'NONE', #94853, #26354, #75302 ) ;
#73419 = CARTESIAN_POINT ( 'NONE',  ( 0.5774900079438607392, 8.480352010821505360, 5.440088680355550821 ) ) ;
#73420 = EDGE_CURVE ( 'NONE', #38633, #20656, #35766, .T. ) ;
#73421 = AXIS2_PLACEMENT_3D ( 'NONE', #59889, #1761, #22906 ) ;
#73422 = CARTESIAN_POINT ( 'NONE',  ( 15.44008868035555793, 31.39701867748817676, -9.422509992056140149 ) ) ;
#73424 = CARTESIAN_POINT ( 'NONE',  ( -0.8801773607111009756, 43.06368534415484106, 1.068504757029289695E-15 ) ) ;
#73423 = CARTESIAN_POINT ( 'NONE',  ( -5.056330833731550456, 15.00000000000000000, -13.58983143750704592 ) ) ;
#73425 = ORIENTED_EDGE ( 'NONE', *, *, #97574, .T. ) ;
#73426 = CARTESIAN_POINT ( 'NONE',  ( 12.63842701281683034, 62.46726448433410894, 9.846743663894596210 ) ) ;
#73427 = CARTESIAN_POINT ( 'NONE',  ( 2.035157376598824452, 18.68868534415484106, 7.964842623401179544 ) ) ;
#73428 = CARTESIAN_POINT ( 'NONE',  ( 22.81628187352648496, 61.83196800326376774, -3.434112377981050290 ) ) ;
#73429 = CARTESIAN_POINT ( 'NONE',  ( 6.879999999999995453, 43.00000000000000000, -4.250000000000000000 ) ) ;
#73430 = CARTESIAN_POINT ( 'NONE',  ( 24.16423886937410614, 39.30374883491396787, 8.672049930838204340E-16 ) ) ;
#73431 = CARTESIAN_POINT ( 'NONE',  ( 0.5774900079438590739, 52.64701867748817676, -5.440088680355550821 ) ) ;
#73432 = CARTESIAN_POINT ( 'NONE',  ( 10.00000000000000000, 36.81368534415484106, -10.88017736071110342 ) ) ;
#73433 = DIRECTION ( 'NONE',  ( 0.000000000000000000, 1.000000000000000000, 0.000000000000000000 ) ) ;
#73434 = DIRECTION ( 'NONE',  ( 0.000000000000000000, 0.000000000000000000, -1.000000000000000000 ) ) ;
#73435 = CARTESIAN_POINT ( 'NONE',  ( 12.63842701281683034, 52.46726448433413026, 9.846743663894596210 ) ) ;
#73436 = B_SPLINE_CURVE_WITH_KNOTS ( 'NONE', 3,
 ( #88242, #50235, #80750, #12246, #73235, #35234 ),
 .UNSPECIFIED., .F., .F.,
 ( 4, 2, 4 ),
 ( 3.409110551495419861E-05, 0.0004400426677367805001, 0.0008459942299586068219 ),
 .UNSPECIFIED. ) ;
#73437 = ORIENTED_EDGE ( 'NONE', *, *, #81638, .T. ) ;
#73438 = CARTESIAN_POINT ( 'NONE',  ( 0.2751277870542909731, 22.28217586085237656, -6.499999999999992006 ) ) ;
#73439 = CARTESIAN_POINT ( 'NONE',  ( 10.00000000000000178, 17.25893115100078745, 9.846743663894594434 ) ) ;
#73440 = CARTESIAN_POINT ( 'NONE',  ( -5.204170427930421283E-15, -32.12636533006957507, -12.81628187352647608 ) ) ;
#73441 = TOROIDAL_SURFACE ( 'NONE', #38350, 4.250000000000001776, 0.2500000000000000000 ) ;
#73442 = CARTESIAN_POINT ( 'NONE',  ( 12.91533473730993009, 6.605352010821504471, -10.88017736071109987 ) ) ;
#73443 = CARTESIAN_POINT ( 'NONE',  ( 5.076628168052704559, 30.17559781766745175, -8.527530157486179263 ) ) ;
#73444 = CARTESIAN_POINT ( 'NONE',  ( 10.00000000000000000, 7.873634669930421381, -12.81628187352647608 ) ) ;
#73445 = CARTESIAN_POINT ( 'NONE',  ( 0.5774900079438607392, 58.48035201082151247, 5.440088680355550821 ) ) ;
#73447 = CARTESIAN_POINT ( 'NONE',  ( 10.00000000000000000, 52.87363466993041783, -12.81628187352647608 ) ) ;
#73446 = CARTESIAN_POINT ( 'NONE',  ( 4.559911319644449179, 13.89701867748817143, 9.422509992056141925 ) ) ;
#73448 = CARTESIAN_POINT ( 'NONE',  ( 10.00000000000000000, 40.55374883491397497, -14.16423886937410082 ) ) ;
#73449 = DIRECTION ( 'NONE',  ( 1.000000000000000000, 0.000000000000000000, -0.000000000000000000 ) ) ;
#73450 = EDGE_LOOP ( 'NONE', ( #88069, #30029, #85568, #52921 ) ) ;
#73451 = CARTESIAN_POINT ( 'NONE',  ( 3.591859063236761518, -0.04303199673624671928, 11.09922568453594849 ) ) ;
#73452 = DIRECTION ( 'NONE',  ( 1.000000000000000000, -0.000000000000000000, 0.000000000000000000 ) ) ;
#73453 = CARTESIAN_POINT ( 'NONE',  ( 2.035157376598824452, 28.68868534415484106, 7.964842623401179544 ) ) ;
#73454 = CARTESIAN_POINT ( 'NONE',  ( 19.84674366389459266, 58.30059781766745886, 2.638427012816836559 ) ) ;
#73455 = ORIENTED_EDGE ( 'NONE', *, *, #10286, .F. ) ;
#73456 = CARTESIAN_POINT ( 'NONE',  ( 5.076628168052704559, 20.17559781766745175, -8.527530157486179263 ) ) ;
#73457 = CARTESIAN_POINT ( 'NONE',  ( 0.1532563361054100626, 10.80059781766745175, -2.638427012816831230 ) ) ;
#73458 = CARTESIAN_POINT ( 'NONE',  ( 18.52753015748617571, 28.09226448433411960, 4.923371831947298993 ) ) ;
#73459 = CARTESIAN_POINT ( 'NONE',  ( 14.92337183194729633, 17.67559781766745175, 8.527530157486181039 ) ) ;
#73460 = CARTESIAN_POINT ( 'NONE',  ( 10.00000000000000000, 4.758931151000784787, -9.846743663894594434 ) ) ;
#73461 = CARTESIAN_POINT ( 'NONE',  ( -7.121341127193570486, -73.24353698637885657, 2.750000000000000000 ) ) ;
#73462 = EDGE_CURVE ( 'NONE', #90286, #9752, #9277, .T. ) ;
#73464 = DIRECTION ( 'NONE',  ( 0.000000000000000000, 0.000000000000000000, 1.000000000000000000 ) ) ;
#73463 = CARTESIAN_POINT ( 'NONE',  ( 19.84674366389459621, 3.508931151000785231, 7.409399052514197653E-17 ) ) ;
#73465 = CARTESIAN_POINT ( 'NONE',  ( 12.63842701281683034, 7.467264484334118713, 9.846743663894596210 ) ) ;
#73467 = ORIENTED_EDGE ( 'NONE', *, *, #14425, .F. ) ;
#73466 = CARTESIAN_POINT ( 'NONE',  ( 14.92337183194729633, 22.67559781766745175, 8.527530157486181039 ) ) ;
#73468 = PRESENTATION_LAYER_ASSIGNMENT (  '', '', ( #76691 ) ) ;
#73469 = CARTESIAN_POINT ( 'NONE',  ( 4.823525747195464675, -6.402798798525323853, 4.000000000000000888 ) ) ;
#73470 = CARTESIAN_POINT ( 'NONE',  ( 13.43411237798105340, 5.581968003263753531, 12.81628187352647963 ) ) ;
#73471 = CARTESIAN_POINT ( 'NONE',  ( -4.164238869374099927, 22.01208216824730357, 3.795296366450308767 ) ) ;
#73472 = UNCERTAINTY_MEASURE_WITH_UNIT (LENGTH_MEASURE( 1.000000000000000082E-05 ), #71293, 'distance_accuracy_value', 'NONE');
#73473 = CARTESIAN_POINT ( 'NONE',  ( -2.962741594152892510, 0.000000000000000000, -13.93860331045676837 ) ) ;
#73474 = CARTESIAN_POINT ( 'NONE',  ( -4.164238869374098151, 21.59541550158063217, -3.795296366450310543 ) ) ;
#73475 = CARTESIAN_POINT ( 'NONE',  ( 13.79529636645030344, 43.26208216824730357, 14.16423886937410614 ) ) ;
#73476 = CARTESIAN_POINT ( 'NONE',  ( -13.82671409943291785, 15.00000000000000000, -3.447387012295409114 ) ) ;
#73477 = CARTESIAN_POINT ( 'NONE',  ( -0.3689425029237898834, 16.17874883491396076, -10.36894250292378850 ) ) ;
#73478 = CARTESIAN_POINT ( 'NONE',  ( 20.88017736071110875, 35.77201867748816966, -2.915334737309920765 ) ) ;
#73479 = CARTESIAN_POINT ( 'NONE',  ( -5.148594389986405062, -3.608360355303317472E-16, 13.69051944078645100 ) ) ;
#73480 = EDGE_LOOP ( 'NONE', ( #46551, #58692, #96792, #47130 ) ) ;
#73481 =( BOUNDED_CURVE ( )  B_SPLINE_CURVE ( 2, ( #73073, #96095, #80092, #81564, #27577, #51072, #13071, #32447, #1981 ),
 .UNSPECIFIED., .F., .T. ) 
 B_SPLINE_CURVE_WITH_KNOTS ( ( 3, 2, 2, 2, 3 ),
 ( 0.6167998787605536437, 0.6190476190476190688, 0.6250000000000000000, 0.6309523809523809312, 0.6332001212394463563 ),
 .UNSPECIFIED. ) 
 CURVE ( )  GEOMETRIC_REPRESENTATION_ITEM ( )  RATIONAL_B_SPLINE_CURVE ( ( 0.9839835555609424134, 0.9871328979762474809, 1.000000000000000000, 0.9659258262890683122, 1.000000000000000000, 0.9659258262890683122, 1.000000000000000000, 0.9871328979762474809, 0.9839835555609424134 ) ) 
 REPRESENTATION_ITEM ( '' )  );
#73482 = CARTESIAN_POINT ( 'NONE',  ( 14.92337183194729633, 17.67559781766745175, 8.527530157486181039 ) ) ;
#73485 = AXIS2_PLACEMENT_3D ( 'NONE', #57713, #80721, #73697 ) ;
#73484 = CARTESIAN_POINT ( 'NONE',  ( 10.00000000000000000, 24.75893115100078745, -9.846743663894594434 ) ) ;
#73483 = CARTESIAN_POINT ( 'NONE',  ( 4.559911319644449179, 62.23035201082150536, -9.422509992056141925 ) ) ;
#73486 = CARTESIAN_POINT ( 'NONE',  ( 0.5774900079438590739, 12.64701867748817321, -5.440088680355550821 ) ) ;
#73487 = CARTESIAN_POINT ( 'NONE',  ( 21.09922568453595559, 47.04030133659708923, -6.408140936763230044 ) ) ;
#73488 = CARTESIAN_POINT ( 'NONE',  ( 2.791683348922240793, 46.63393115100077324, 7.208316651077764092 ) ) ;
#73489 = CARTESIAN_POINT ( 'NONE',  ( 18.00000000000000000, 78.20644476077552554, 3.828778331633460486 ) ) ;
#73490 = CARTESIAN_POINT ( 'NONE',  ( 22.81628187352647785, 41.62363466993042493, 6.195893100308588602E-16 ) ) ;
#73491 = CARTESIAN_POINT ( 'NONE',  ( -14.16423886937409726, -27.98791783175269643, 3.795296366450320757 ) ) ;
#73492 = CARTESIAN_POINT ( 'NONE',  ( 17.20831665107776587, 34.13393115100078745, -7.208316651077762316 ) ) ;
#73493 = CARTESIAN_POINT ( 'NONE',  ( 2.917880565312948704, 22.63708216824730002, 12.26659068614894643 ) ) ;
#73494 = EDGE_CURVE ( 'NONE', #82286, #9027, #3576, .T. ) ;
#73495 = VERTEX_POINT ( 'NONE', #50775 ) ;
#73496 = CARTESIAN_POINT ( 'NONE',  ( 0.2751277870542910842, 63.21833443783937412, 6.499999999999992006 ) ) ;
#73497 = CARTESIAN_POINT ( 'NONE',  ( 20.88017736071110519, 55.56368534415484817, 2.639326808657452039E-16 ) ) ;
#73498 = CARTESIAN_POINT ( 'NONE',  ( 12.91533473730993009, 51.60535201082149825, -10.88017736071109987 ) ) ;
#73499 = CARTESIAN_POINT ( 'NONE',  ( -0.3689425029237881626, 47.42874883491396787, 10.36894250292379027 ) ) ;
#73500 = CARTESIAN_POINT ( 'NONE',  ( 1.472469842513823179, 61.42559781766745175, 4.923371831947296329 ) ) ;
#73501 = CARTESIAN_POINT ( 'NONE',  ( -14.40939250470707478, 15.00000000000000000, -1.618458416369986219 ) ) ;
#73502 = CARTESIAN_POINT ( 'NONE',  ( 19.42250999205614548, 40.98035201082150536, -5.440088680355545492 ) ) ;
#73503 = ADVANCED_FACE ( 'NONE', ( #90738 ), #18139, .T. ) ;
#73504 = DIRECTION ( 'NONE',  ( -0.000000000000000000, -1.000000000000000000, -0.000000000000000000 ) ) ;
#73505 = VECTOR ( 'NONE', #22130, 1000.000000000000000 ) ;
#73506 = CARTESIAN_POINT ( 'NONE',  ( 19.38216949554541557, 27.24863466993041783, -9.382169495545420901 ) ) ;
#73507 = CARTESIAN_POINT ( 'NONE',  ( 17.20831665107776587, 52.88393115100078035, 7.208316651077764980 ) ) ;
#73508 = CARTESIAN_POINT ( 'NONE',  ( -5.440088680355547268, 8.897018677488176763, 9.422509992056143702 ) ) ;
#73509 = DIRECTION ( 'NONE',  ( 1.000000000000000000, 0.000000000000000000, 0.000000000000000000 ) ) ;
#73510 = CARTESIAN_POINT ( 'NONE',  ( 10.00000000000000178, 64.31368534415483396, 10.88017736071110342 ) ) ;
#73511 = ORIENTED_EDGE ( 'NONE', *, *, #60493, .F. ) ;
#73512 = DIRECTION ( 'NONE',  ( 0.000000000000000000, 1.000000000000000000, 0.000000000000000000 ) ) ;
#73513 = CARTESIAN_POINT ( 'NONE',  ( 7.084665262690076126, 69.10535201082151957, 10.88017736071109987 ) ) ;
#73514 = CARTESIAN_POINT ( 'NONE',  ( 0.1532563361054100626, 5.800597817667452638, -2.638427012816831230 ) ) ;
#73515 = CARTESIAN_POINT ( 'NONE',  ( 18.00000000000000000, 77.07179676972447169, -4.250000000000000000 ) ) ;
#73516 = VECTOR ( 'NONE', #61190, 1000.000000000000000 ) ;
#73517 = CARTESIAN_POINT ( 'NONE',  ( 1.472469842513823179, 30.59226448433411960, -4.923371831947296329 ) ) ;
#73518 = CARTESIAN_POINT ( 'NONE',  ( -0.8801773607111009756, 23.06368534415484106, 1.068504757029289695E-15 ) ) ;
#73519 = CARTESIAN_POINT ( 'NONE',  ( -2.816281873526471635, 8.915301336597083903, -3.434112377981056508 ) ) ;
#73521 = LINE ( 'NONE', #59020, #30440 ) ;
#73520 = CARTESIAN_POINT ( 'NONE',  ( 10.00000000000000000, 36.81368534415484106, -10.88017736071110342 ) ) ;
#73522 =( LENGTH_UNIT ( ) NAMED_UNIT ( * ) SI_UNIT ( .MILLI., .METRE. ) );
#73523 = CARTESIAN_POINT ( 'NONE',  ( 19.38216949554541557, 32.24863466993041783, -9.382169495545420901 ) ) ;
#73524 = VERTEX_POINT ( 'NONE', #78216 ) ;
#73525 = CARTESIAN_POINT ( 'NONE',  ( -0.8801773607111009756, 63.06368534415484106, 1.068504757029289695E-15 ) ) ;
#73527 = FACE_OUTER_BOUND ( 'NONE', #27191, .T. ) ;
#73526 = CARTESIAN_POINT ( 'NONE',  ( -2.816281873526473856, 24.33196800326375353, 3.434112377981055619 ) ) ;
#73528 = CARTESIAN_POINT ( 'NONE',  ( 2.897438467171757030E-16, 23.03999999999999915, 0.000000000000000000 ) ) ;
#73529 = CARTESIAN_POINT ( 'NONE',  ( 20.88017736071110519, 45.56368534415484106, 2.639326808657452039E-16 ) ) ;
#73530 = PLANE ( 'NONE',  #56376 ) ;
#73531 = CARTESIAN_POINT ( 'NONE',  ( 10.00000000000000000, 65.55374883491396076, -14.16423886937410082 ) ) ;
#73532 = CARTESIAN_POINT ( 'NONE',  ( 17.20831665107776587, 52.88393115100078035, 7.208316651077764980 ) ) ;
#73533 = CARTESIAN_POINT ( 'NONE',  ( 0.5774900079438590739, 67.64701867748817676, -5.440088680355550821 ) ) ;
#73534 = EDGE_CURVE ( 'NONE', #24048, #98205, #90878, .T. ) ;
#73535 = CARTESIAN_POINT ( 'NONE',  ( 15.44008868035555260, 59.73035201082151247, 9.422509992056143702 ) ) ;
#73536 = CARTESIAN_POINT ( 'NONE',  ( 13.34948392230377578, 0.04922511925147182721, -6.279918722514977958 ) ) ;
#73537 = CARTESIAN_POINT ( 'NONE',  ( -4.164238869374099039, 26.80374883491397142, 8.674139862899312516E-16 ) ) ;
#73538 = EDGE_CURVE ( 'NONE', #65046, #89050, #42745, .T. ) ;
#73539 = FILL_AREA_STYLE ('',( #51045 ) ) ;
#73540 = CIRCLE ( 'NONE', #81536, 15.00000000000000000 ) ;
#73541 = VERTEX_POINT ( 'NONE', #22901 ) ;
#73542 = VERTEX_POINT ( 'NONE', #21916 ) ;
#73543 = CARTESIAN_POINT ( 'NONE',  ( 24.16423886937409904, 64.09541550158064638, 3.795296366450317205 ) ) ;
#73544 = CARTESIAN_POINT ( 'NONE',  ( 6.204703633549690345, 50.76208216824730357, -14.16423886937410259 ) ) ;
#73545 = CARTESIAN_POINT ( 'NONE',  ( 0.1532563361054082862, 26.21726448433411605, 2.638427012816831674 ) ) ;
#73546 = CARTESIAN_POINT ( 'NONE',  ( -4.873787042390880231, 15.00000000000000000, 13.39061984619915791 ) ) ;
#73547 = DIRECTION ( 'NONE',  ( 0.000000000000000000, 1.000000000000000000, 0.000000000000000000 ) ) ;
#73548 = CARTESIAN_POINT ( 'NONE',  ( -0.8801773607111008646, 3.272018677488171434, 2.915334737309923430 ) ) ;
#73549 = CARTESIAN_POINT ( 'NONE',  ( -4.164238869374098151, 56.59541550158063927, -3.795296366450310543 ) ) ;
#73550 = CARTESIAN_POINT ( 'NONE',  ( 11.96291822454879750, 15.00000000000000000, -8.193813980849057543 ) ) ;
#73551 = CARTESIAN_POINT ( 'NONE',  ( 14.92337183194729633, 7.675597817667451750, 8.527530157486181039 ) ) ;
#73552 = AXIS2_PLACEMENT_3D ( 'NONE', #73393, #94918, #87420 ) ;
#73553 = EDGE_CURVE ( 'NONE', #83062, #10816, #85002, .T. ) ;
#73554 = AXIS2_PLACEMENT_3D ( 'NONE', #88037, #71088, #2613 ) ;
#73555 = LINE ( 'NONE', #4595, #83386 ) ;
#73556 = CARTESIAN_POINT ( 'NONE',  ( 3.469446951953614189E-15, 7.258931151000791004, 9.846743663894594434 ) ) ;
#73557 = ORIENTED_EDGE ( 'NONE', *, *, #53994, .T. ) ;
#73558 = ORIENTED_EDGE ( 'NONE', *, *, #34321, .T. ) ;
#73559 = CIRCLE ( 'NONE', #12687, 6.999999999999995559 ) ;
#73560 = ORIENTED_EDGE ( 'NONE', *, *, #16669, .T. ) ;
#73562 = CARTESIAN_POINT ( 'NONE',  ( 7.084665262690076126, 22.02201867748817321, -10.88017736071110164 ) ) ;
#73561 = CARTESIAN_POINT ( 'NONE',  ( 20.88017736071110164, 15.35535201082150358, 2.915334737309930979 ) ) ;
#73564 = CARTESIAN_POINT ( 'NONE',  ( -2.816281873526471635, 13.91530133659708746, -3.434112377981056508 ) ) ;
#73563 = CARTESIAN_POINT ( 'NONE',  ( 12.63842701281683922, 54.55059781766745175, -9.846743663894590881 ) ) ;
#73565 = CARTESIAN_POINT ( 'NONE',  ( -0.3093388210927633941, 0.5000000000000004441, -14.99680997725065978 ) ) ;
#73566 = CARTESIAN_POINT ( 'NONE',  ( 22.81628187352647785, 31.62363466993042138, 6.195893100308588602E-16 ) ) ;
#73568 = ORIENTED_EDGE ( 'NONE', *, *, #88988, .T. ) ;
#73567 = CARTESIAN_POINT ( 'NONE',  ( 2.791683348922237240, 0.3839311510007847872, -7.208316651077763204 ) ) ;
#73569 = CARTESIAN_POINT ( 'NONE',  ( 18.52753015748617571, 38.09226448433412315, 4.923371831947298993 ) ) ;
#73570 = CARTESIAN_POINT ( 'NONE',  ( -4.164238869374099927, 62.01208216824728936, 3.795296366450308767 ) ) ;
#73571 = CARTESIAN_POINT ( 'NONE',  ( -0.8801773607111008646, 3.272018677488171434, 2.915334737309923430 ) ) ;
#73572 = EDGE_LOOP ( 'NONE', ( #29925, #31129, #42704, #18697 ) ) ;
#73573 = CARTESIAN_POINT ( 'NONE',  ( 0.5774900079438590739, 42.64701867748816966, -5.440088680355550821 ) ) ;
#73574 = CARTESIAN_POINT ( 'NONE',  ( 17.96484262340118221, 39.93868534415484106, 7.964842623401181321 ) ) ;
#73575 = CARTESIAN_POINT ( 'NONE',  ( 20.88017736071110875, 50.77201867748817676, -2.915334737309920765 ) ) ;
#73576 = CARTESIAN_POINT ( 'NONE',  ( -18.00000000000000355, 75.73428692542562146, 3.000000000000000000 ) ) ;
#73577 = CARTESIAN_POINT ( 'NONE',  ( 15.44008868035555260, 39.73035201082150536, 9.422509992056143702 ) ) ;
#73578 = AXIS2_PLACEMENT_3D ( 'NONE', #3563, #41568, #64519 ) ;
#73579 = CARTESIAN_POINT ( 'NONE',  ( 20.24186590665277663, 64.73410085661204505, 6.114288769123050749 ) ) ;
#73580 = ADVANCED_FACE ( 'NONE', ( #2744 ), #19190, .T. ) ;
#73582 = ORIENTED_EDGE ( 'NONE', *, *, #2694, .T. ) ;
#73581 = DIRECTION ( 'NONE',  ( 0.000000000000000000, 0.000000000000000000, 1.000000000000000000 ) ) ;
#73583 = AXIS2_PLACEMENT_3D ( 'NONE', #79546, #11046, #72518 ) ;
#73584 = CARTESIAN_POINT ( 'NONE',  ( 7.361572987183169658, 29.96726448433411960, -9.846743663894592657 ) ) ;
#73585 = ORIENTED_EDGE ( 'NONE', *, *, #18762, .T. ) ;
#73586 = CARTESIAN_POINT ( 'NONE',  ( 0.1532563361054083140, 61.00893115100078745, 1.131784320476157264E-15 ) ) ;
#73587 = EDGE_CURVE ( 'NONE', #60629, #50168, #59435, .T. ) ;
#73588 = CARTESIAN_POINT ( 'NONE',  ( 8.606322355891263598, 15.00000000000000000, 11.66967075398811282 ) ) ;
#73589 =( BOUNDED_SURFACE ( )  B_SPLINE_SURFACE ( 1, 2, ( 
 ( #23199, #15700, #1196, #84190, #39180, #84670, #85164, #30667, #47145, #46185, #31161, #31656, #16673, #68687, #54159, #83690, #218, #77646, #62143, #17172, #61176, #9160, #76670, #8188, #98725, #93144, #39678, #92172, #47654, #76184, #70169, #78147, #1685, #24669, #38684, #69185, #32138, #23699, #85653, #91178, #22705, #53186, #15207, #71638, #26612, #33611, #56147, #49124, #19117, #33128, #10155, #57108, #11614, #94623, #63137, #72112, #18149, #27100, #19609, #79626, #40650, #95104, #3147, #71149, #11127, #49598, #64107, #26135, #50105, #57600, #34103, #2676, #87606, #64594, #55653, #56628, #3638, #87116, #93639, #2181, #18634, #10639, #80107, #41645, #63621, #42130, #80613, #72596, #48623, #4132, #34595, #25174, #32640, #94127, #25655, #86641, #48134, #65089, #95613, #78649, #88100, #12108, #41153, #70660, #86152, #17662, #79127, #67591, #73089, #65589, #98099, #81095, #74580, #28091, #12597, #44577, #36599, #88591, #27599, #51596, #97614, #29560, #60065, #90565, #5108, #75077, #51093, #14093, #4627, #35090, #20605, #89587, #21096, #22094, #44072, #29074, #36087, #50603, #52572, #35597, #81582, #96115, #97119, #83076, #42610, #73584, #37092, #58087, #59080, #82080, #52087, #20099, #6095, #67086, #59579, #43097, #82580, #90072, #66085, #96614, #58589, #6582, #89091, #13590, #13091, #21598, #43587, #74076, #5609, #66592, #28590, #92533, #15094, #62524, #93028, #85045, #37587, #53060, #24063, #23085, #32020, #39558, #91568, #84070, #54531, #70048, #46069, #47033, #45567, #68081, #16559, #8561, #53553, #55024, #603, #54049, #31537, #76063, #15585, #76554, #38570, #62033, #92055, #106, #30057, #7592, #38086, #69065, #77528, #30553, #8072, #39064, #68574, #31046, #1571, #14600, #9047, #24563, #45066, #61545, #23580, #16061, #84559, #46549, #77047, #69557, #61055, #1076, #75574, #7087, #98609, #60569, #91060, #22588, #83575, #85542, #25056, #79014, #17055, #78528, #10039, #3527, #63995, #19014, #40541, #2562, #87008, #71040, #94505, #71535, #72000, #17549, #33984, #33019, #18031, #3043, #41533, #55540, #41035, #70542, #86037, #79513, #49009, #4020, #48017, #64486, #63516, #94020, #95501, #49490, #26024, #86531, #34482, #63026, #33496, #64976, #11015, #11501, #25543, #56033, #56518, #48511, #10523, #93525, #18518, #47536, #87500, #94995, #26500, #56998, #79996, #42022, #72486, #26993, #78035, #9537, #40041, #2066, #32528, #58973, #4997, #13984, #6463, #35970, #27484, #81962, #58468, #57976, #97001, #5985, #20488, #50976, #36971, #44458, #20987, #88482, #13476, #51472, #42498, #81470, #89472, #43956, #66471, #67468, #28956 ),
 ( #97988, #59459, #80499, #96000, #36477, #65974, #74960, #82461, #35478, #27973, #97490, #57491, #88982, #89959, #19985, #11996, #21476, #74457, #96500, #87985, #43469, #28476, #66970, #50483, #12974, #73969, #5498, #51974, #19497, #42988, #72983, #49992, #4511, #34976, #65476, #80986, #12485, #73470, #98487, #23463, #8923, #15471, #75947, #15943, #60935, #82960, #90439, #29942, #60447, #52942, #6966, #61919, #30926, #37474, #54417, #38944, #98982, #480, #30434, #91443, #53435, #84927, #59950, #52456, #16440, #67963, #61426, #14974, #90938, #31415, #53939, #75453, #14475, #38454, #84446, #46915, #77408, #39439, #22466, #92422, #37971, #954, #21982, #44948, #7473, #76442, #7957, #69933, #91935, #46434, #22968, #83453, #29445, #45444, #68459, #83944, #45954, #68948, #76928, #8438, #23947, #69433, #17912, #78898, #10900, #62404, #33378, #94386, #56405, #11384, #41422, #63874, #47407, #56879, #87381, #3402, #62906, #71414, #33864, #2931, #40914, #2440, #25903, #86890, #18400, #79393, #18900, #41905, #9922, #55911, #48883, #48396, #40426, #71883, #86411, #24932, #64372, #63396, #70922, #1944, #54905, #49377, #32899, #1452, #31904, #39923, #93902, #92911, #93408, #55413, #94880, #10408, #26380, #85920, #17430, #79878, #47899, #24440, #85419, #16930, #32406, #77910, #78403, #25428, #9420, #70425, #11877, #27852, #57370, #42382, #66342, #35853, #89839, #72859, #28356, #88369, #34863, #82334, #36351, #81355, #73355, #21355, #49865, #20369, #51846, #96880, #97366, #50357, #19863, #50863, #80868, #35360, #80378, #27365, #72366, #74332, #4882, #58846, #65853, #57858, #12853, #20862, #65356, #4394, #89352, #13352, #96381, #64856, #73849, #12366, #28834, #13855, #43352, #95885, #51354, #58340, #42872, #5379, #81838, #88859, #43837, #3897, #59336, #5858, #66845, #34365, #95376, #87865, #26877, #19382, #9179, #24196, #25190, #17191, #44335, #9675, #74840, #23217, #16690, #54663, #62659, #84210, #8206, #38701, #1216, #47671, #61671, #84687, #70184, #46202, #62161, #2198, #6340, #85671, #31671, #16198, #77664, #92668, #15717, #39696, #55669, #85179, #92190, #32157, #77177, #97869, #36852, #76686, #69200, #725, #53690, #78165, #47160, #31179, #70677, #55157, #46679, #1700, #8684, #39197, #69685, #32659, #67343, #29329, #63152, #23715, #93161, #54176, #24686, #40173, #93655, #91699, #59827, #86168, #72612, #4642, #73103, #65604, #79144, #19625, #26151, #88116, #48152, #10171, #94641, #64612, #95120, #35106, #19137, #4147, #11141, #25672, #96132, #10656, #56645, #78665, #72128, #27613, #17678, #48641, #12123, #40669, #34120, #26628, #27118 ) ),
 .UNSPECIFIED., .F., .F., .F. ) 
 B_SPLINE_SURFACE_WITH_KNOTS ( ( 2, 2 ),
 ( 3, 2, 2, 2, 2, 2, 2, 2, 2, 2, 2, 2, 2, 2, 2, 2, 2, 2, 2, 2, 2, 2, 2, 2, 2, 2, 2, 2, 2, 2, 2, 2, 2, 2, 2, 2, 2, 2, 2, 2, 2, 2, 2, 2, 2, 2, 2, 2, 2, 2, 2, 2, 2, 2, 2, 2, 2, 2, 2, 2, 2, 2, 2, 2, 2, 2, 2, 2, 2, 2, 2, 2, 2, 2, 2, 2, 2, 2, 2, 2, 2, 2, 2, 2, 2, 2, 2, 2, 2, 2, 2, 2, 2, 2, 2, 2, 2, 2, 2, 2, 2, 2, 2, 2, 2, 2, 2, 2, 2, 2, 2, 2, 2, 2, 2, 2, 2, 2, 2, 2, 2, 2, 2, 2, 2, 2, 2, 2, 2, 2, 2, 2, 2, 2, 2, 2, 2, 2, 2, 2, 2, 2, 2, 2, 2, 2, 2, 2, 2, 2, 2, 2, 2, 2, 2, 2, 2, 2, 2, 2, 2, 2, 3 ),
 ( 0.000000000000000000, 1.000000000000000000 ),
 ( 0.000000000000000000, 0.005952380952380952051, 0.01190476190476190410, 0.01785714285714285615, 0.02380952380952380820, 0.02976190476190476025, 0.03571428571428571230, 0.04166666666666666435, 0.04761904761904761640, 0.05357142857142856845, 0.05952380952380952051, 0.06547619047619047949, 0.07142857142857142461, 0.07738095238095238360, 0.08333333333333332871, 0.08928571428571428770, 0.09523809523809523281, 0.1011904761904761918, 0.1071428571428571369, 0.1130952380952380959, 0.1190476190476190410, 0.1250000000000000000, 0.1309523809523809590, 0.1369047619047619180, 0.1428571428571428492, 0.1488095238095238082, 0.1547619047619047672, 0.1607142857142857262, 0.1666666666666666574, 0.1726190476190476164, 0.1785714285714285754, 0.1845238095238095344, 0.1904761904761904656, 0.1964285714285714246, 0.2023809523809523836, 0.2083333333333333426, 0.2142857142857142738, 0.2202380952380952328, 0.2261904761904761918, 0.2321428571428571508, 0.2380952380952380820, 0.2440476190476190410, 0.2500000000000000000, 0.2559523809523809312, 0.2619047619047619180, 0.2678571428571428492, 0.2738095238095238360, 0.2797619047619047672, 0.2857142857142856984, 0.2916666666666666852, 0.2976190476190476164, 0.3035714285714285476, 0.3095238095238095344, 0.3154761904761904656, 0.3214285714285714524, 0.3273809523809523836, 0.3333333333333333148, 0.3392857142857143016, 0.3452380952380952328, 0.3511904761904761640, 0.3571428571428571508, 0.3630952380952380820, 0.3690476190476190688, 0.3750000000000000000, 0.3809523809523809312, 0.3869047619047619180, 0.3928571428571428492, 0.3988095238095238360, 0.4047619047619047672, 0.4107142857142856984, 0.4166666666666666852, 0.4226190476190476164, 0.4285714285714285476, 0.4345238095238095344, 0.4404761904761904656, 0.4464285714285714524, 0.4523809523809523836, 0.4583333333333333148, 0.4642857142857143016, 0.4702380952380952328, 0.4761904761904761640, 0.4821428571428571508, 0.4880952380952380820, 0.4940476190476190688, 0.5000000000000000000, 0.5059523809523809312, 0.5119047619047618625, 0.5178571428571429047, 0.5238095238095238360, 0.5297619047619047672, 0.5357142857142856984, 0.5416666666666666297, 0.5476190476190476719, 0.5535714285714286031, 0.5595238095238095344, 0.5654761904761904656, 0.5714285714285713969, 0.5773809523809523281, 0.5833333333333333703, 0.5892857142857143016, 0.5952380952380952328, 0.6011904761904761640, 0.6071428571428570953, 0.6130952380952381375, 0.6190476190476190688, 0.6250000000000000000, 0.6309523809523809312, 0.6369047619047618625, 0.6428571428571429047, 0.6488095238095238360, 0.6547619047619047672, 0.6607142857142856984, 0.6666666666666666297, 0.6726190476190476719, 0.6785714285714286031, 0.6845238095238095344, 0.6904761904761904656, 0.6964285714285713969, 0.7023809523809523281, 0.7083333333333333703, 0.7142857142857143016, 0.7202380952380952328, 0.7261904761904761640, 0.7321428571428570953, 0.7380952380952381375, 0.7440476190476190688, 0.7500000000000000000, 0.7559523809523809312, 0.7619047619047618625, 0.7678571428571429047, 0.7738095238095238360, 0.7797619047619047672, 0.7857142857142856984, 0.7916666666666666297, 0.7976190476190476719, 0.8035714285714286031, 0.8095238095238095344, 0.8154761904761904656, 0.8214285714285713969, 0.8273809523809523281, 0.8333333333333333703, 0.8392857142857143016, 0.8452380952380952328, 0.8511904761904761640, 0.8571428571428570953, 0.8630952380952381375, 0.8690476190476190688, 0.8750000000000000000, 0.8809523809523809312, 0.8869047619047618625, 0.8928571428571429047, 0.8988095238095238360, 0.9047619047619047672, 0.9107142857142856984, 0.9166666666666666297, 0.9226190476190476719, 0.9285714285714286031, 0.9345238095238095344, 0.9404761904761904656, 0.9464285714285713969, 0.9523809523809523281, 0.9583333333333333703, 0.9642857142857143016 ),
 .UNSPECIFIED. ) 
 GEOMETRIC_REPRESENTATION_ITEM ( )  RATIONAL_B_SPLINE_SURFACE ( (
 ( 1.000000000000000000, 0.9659258262890683122, 1.000000000000000000, 0.9659258262890683122, 1.000000000000000000, 0.9659258262890683122, 1.000000000000000000, 0.9659258262890683122, 1.000000000000000000, 0.9659258262890683122, 1.000000000000000000, 0.9659258262890683122, 1.000000000000000000, 0.9659258262890683122, 1.000000000000000000, 0.9659258262890683122, 1.000000000000000000, 0.9659258262890683122, 1.000000000000000000, 0.9659258262890683122, 1.000000000000000000, 0.9659258262890683122, 1.000000000000000000, 0.9659258262890683122, 1.000000000000000000, 0.9659258262890683122, 1.000000000000000000, 0.9659258262890683122, 1.000000000000000000, 0.9659258262890683122, 1.000000000000000000, 0.9659258262890683122, 1.000000000000000000, 0.9659258262890683122, 1.000000000000000000, 0.9659258262890683122, 1.000000000000000000, 0.9659258262890683122, 1.000000000000000000, 0.9659258262890683122, 1.000000000000000000, 0.9659258262890683122, 1.000000000000000000, 0.9659258262890683122, 1.000000000000000000, 0.9659258262890683122, 1.000000000000000000, 0.9659258262890683122, 1.000000000000000000, 0.9659258262890683122, 1.000000000000000000, 0.9659258262890683122, 1.000000000000000000, 0.9659258262890683122, 1.000000000000000000, 0.9659258262890683122, 1.000000000000000000, 0.9659258262890683122, 1.000000000000000000, 0.9659258262890683122, 1.000000000000000000, 0.9659258262890683122, 1.000000000000000000, 0.9659258262890683122, 1.000000000000000000, 0.9659258262890683122, 1.000000000000000000, 0.9659258262890683122, 1.000000000000000000, 0.9659258262890683122, 1.000000000000000000, 0.9659258262890683122, 1.000000000000000000, 0.9659258262890683122, 1.000000000000000000, 0.9659258262890683122, 1.000000000000000000, 0.9659258262890683122, 1.000000000000000000, 0.9659258262890683122, 1.000000000000000000, 0.9659258262890683122, 1.000000000000000000, 0.9659258262890683122, 1.000000000000000000, 0.9659258262890683122, 1.000000000000000000, 0.9659258262890683122, 1.000000000000000000, 0.9659258262890683122, 1.000000000000000000, 0.9659258262890683122, 1.000000000000000000, 0.9659258262890683122, 1.000000000000000000, 0.9659258262890683122, 1.000000000000000000, 0.9659258262890683122, 1.000000000000000000, 0.9659258262890683122, 1.000000000000000000, 0.9659258262890683122, 1.000000000000000000, 0.9659258262890683122, 1.000000000000000000, 0.9659258262890683122, 1.000000000000000000, 0.9659258262890683122, 1.000000000000000000, 0.9659258262890683122, 1.000000000000000000, 0.9659258262890683122, 1.000000000000000000, 0.9659258262890683122, 1.000000000000000000, 0.9659258262890683122, 1.000000000000000000, 0.9659258262890683122, 1.000000000000000000, 0.9659258262890683122, 1.000000000000000000, 0.9659258262890683122, 1.000000000000000000, 0.9659258262890683122, 1.000000000000000000, 0.9659258262890683122, 1.000000000000000000, 0.9659258262890683122, 1.000000000000000000, 0.9659258262890683122, 1.000000000000000000, 0.9659258262890683122, 1.000000000000000000, 0.9659258262890683122, 1.000000000000000000, 0.9659258262890683122, 1.000000000000000000, 0.9659258262890683122, 1.000000000000000000, 0.9659258262890683122, 1.000000000000000000, 0.9659258262890683122, 1.000000000000000000, 0.9659258262890683122, 1.000000000000000000, 0.9659258262890683122, 1.000000000000000000, 0.9659258262890683122, 1.000000000000000000, 0.9659258262890683122, 1.000000000000000000, 0.9659258262890683122, 1.000000000000000000, 0.9659258262890683122, 1.000000000000000000, 0.9659258262890683122, 1.000000000000000000, 0.9659258262890683122, 1.000000000000000000, 0.9659258262890683122, 1.000000000000000000, 0.9659258262890683122, 1.000000000000000000, 0.9659258262890683122, 1.000000000000000000, 0.9659258262890683122, 1.000000000000000000, 0.9659258262890683122, 1.000000000000000000, 0.9659258262890683122, 1.000000000000000000, 0.9659258262890683122, 1.000000000000000000, 0.9659258262890683122, 1.000000000000000000, 0.9659258262890683122, 1.000000000000000000, 0.9659258262890683122, 1.000000000000000000, 0.9659258262890683122, 1.000000000000000000, 0.9659258262890683122, 1.000000000000000000, 0.9659258262890683122, 1.000000000000000000, 0.9659258262890683122, 1.000000000000000000, 0.9659258262890683122, 1.000000000000000000, 0.9659258262890683122, 1.000000000000000000, 0.9659258262890683122, 1.000000000000000000, 0.9659258262890683122, 1.000000000000000000, 0.9659258262890683122, 1.000000000000000000, 0.9659258262890683122, 1.000000000000000000, 0.9659258262890683122, 1.000000000000000000, 0.9659258262890683122, 1.000000000000000000, 0.9659258262890683122, 1.000000000000000000, 0.9659258262890683122, 1.000000000000000000, 0.9659258262890683122, 1.000000000000000000, 0.9659258262890683122, 1.000000000000000000, 0.9659258262890683122, 1.000000000000000000, 0.9659258262890683122, 1.000000000000000000, 0.9659258262890683122, 1.000000000000000000, 0.9659258262890683122, 1.000000000000000000, 0.9659258262890683122, 1.000000000000000000, 0.9659258262890683122, 1.000000000000000000, 0.9659258262890683122, 1.000000000000000000, 0.9659258262890683122, 1.000000000000000000, 0.9659258262890683122, 1.000000000000000000, 0.9659258262890683122, 1.000000000000000000, 0.9659258262890683122, 1.000000000000000000, 0.9659258262890683122, 1.000000000000000000, 0.9659258262890683122, 1.000000000000000000, 0.9659258262890683122, 1.000000000000000000, 0.9659258262890683122, 1.000000000000000000, 0.9659258262890683122, 1.000000000000000000, 0.9659258262890683122, 1.000000000000000000, 0.9659258262890683122, 1.000000000000000000, 0.9659258262890683122, 1.000000000000000000, 0.9659258262890683122, 1.000000000000000000, 0.9659258262890683122, 1.000000000000000000, 0.9659258262890683122, 1.000000000000000000, 0.9659258262890683122, 1.000000000000000000, 0.9659258262890683122, 1.000000000000000000, 0.9659258262890683122, 1.000000000000000000, 0.9659258262890683122, 1.000000000000000000, 0.9659258262890683122, 1.000000000000000000, 0.9659258262890683122, 1.000000000000000000, 0.9659258262890683122, 1.000000000000000000, 0.9659258262890683122, 1.000000000000000000, 0.9659258262890683122, 1.000000000000000000, 0.9659258262890683122, 1.000000000000000000, 0.9659258262890683122, 1.000000000000000000, 0.9659258262890683122, 1.000000000000000000, 0.9659258262890683122, 1.000000000000000000, 0.9659258262890683122, 1.000000000000000000, 0.9659258262890683122, 1.000000000000000000, 0.9659258262890683122, 1.000000000000000000, 0.9659258262890683122, 1.000000000000000000, 0.9659258262890683122, 1.000000000000000000, 0.9659258262890683122, 1.000000000000000000, 0.9659258262890683122, 1.000000000000000000, 0.9659258262890683122, 1.000000000000000000, 0.9659258262890683122, 1.000000000000000000, 0.9659258262890683122, 1.000000000000000000, 0.9659258262890683122, 1.000000000000000000, 0.9659258262890683122, 1.000000000000000000, 0.9659258262890683122, 1.000000000000000000, 0.9659258262890683122, 1.000000000000000000, 0.9659258262890683122, 1.000000000000000000, 0.9659258262890683122, 1.000000000000000000, 0.9659258262890683122, 1.000000000000000000, 0.9659258262890683122, 1.000000000000000000, 0.9659258262890683122, 1.000000000000000000, 0.9659258262890683122, 1.000000000000000000, 0.9659258262890683122, 1.000000000000000000, 0.9659258262890683122, 1.000000000000000000),
 ( 1.000000000000000000, 0.9659258262890683122, 1.000000000000000000, 0.9659258262890683122, 1.000000000000000000, 0.9659258262890683122, 1.000000000000000000, 0.9659258262890683122, 1.000000000000000000, 0.9659258262890683122, 1.000000000000000000, 0.9659258262890683122, 1.000000000000000000, 0.9659258262890683122, 1.000000000000000000, 0.9659258262890683122, 1.000000000000000000, 0.9659258262890683122, 1.000000000000000000, 0.9659258262890683122, 1.000000000000000000, 0.9659258262890683122, 1.000000000000000000, 0.9659258262890683122, 1.000000000000000000, 0.9659258262890683122, 1.000000000000000000, 0.9659258262890683122, 1.000000000000000000, 0.9659258262890683122, 1.000000000000000000, 0.9659258262890683122, 1.000000000000000000, 0.9659258262890683122, 1.000000000000000000, 0.9659258262890683122, 1.000000000000000000, 0.9659258262890683122, 1.000000000000000000, 0.9659258262890683122, 1.000000000000000000, 0.9659258262890683122, 1.000000000000000000, 0.9659258262890683122, 1.000000000000000000, 0.9659258262890683122, 1.000000000000000000, 0.9659258262890683122, 1.000000000000000000, 0.9659258262890683122, 1.000000000000000000, 0.9659258262890683122, 1.000000000000000000, 0.9659258262890683122, 1.000000000000000000, 0.9659258262890683122, 1.000000000000000000, 0.9659258262890683122, 1.000000000000000000, 0.9659258262890683122, 1.000000000000000000, 0.9659258262890683122, 1.000000000000000000, 0.9659258262890683122, 1.000000000000000000, 0.9659258262890683122, 1.000000000000000000, 0.9659258262890683122, 1.000000000000000000, 0.9659258262890683122, 1.000000000000000000, 0.9659258262890683122, 1.000000000000000000, 0.9659258262890683122, 1.000000000000000000, 0.9659258262890683122, 1.000000000000000000, 0.9659258262890683122, 1.000000000000000000, 0.9659258262890683122, 1.000000000000000000, 0.9659258262890683122, 1.000000000000000000, 0.9659258262890683122, 1.000000000000000000, 0.9659258262890683122, 1.000000000000000000, 0.9659258262890683122, 1.000000000000000000, 0.9659258262890683122, 1.000000000000000000, 0.9659258262890683122, 1.000000000000000000, 0.9659258262890683122, 1.000000000000000000, 0.9659258262890683122, 1.000000000000000000, 0.9659258262890683122, 1.000000000000000000, 0.9659258262890683122, 1.000000000000000000, 0.9659258262890683122, 1.000000000000000000, 0.9659258262890683122, 1.000000000000000000, 0.9659258262890683122, 1.000000000000000000, 0.9659258262890683122, 1.000000000000000000, 0.9659258262890683122, 1.000000000000000000, 0.9659258262890683122, 1.000000000000000000, 0.9659258262890683122, 1.000000000000000000, 0.9659258262890683122, 1.000000000000000000, 0.9659258262890683122, 1.000000000000000000, 0.9659258262890683122, 1.000000000000000000, 0.9659258262890683122, 1.000000000000000000, 0.9659258262890683122, 1.000000000000000000, 0.9659258262890683122, 1.000000000000000000, 0.9659258262890683122, 1.000000000000000000, 0.9659258262890683122, 1.000000000000000000, 0.9659258262890683122, 1.000000000000000000, 0.9659258262890683122, 1.000000000000000000, 0.9659258262890683122, 1.000000000000000000, 0.9659258262890683122, 1.000000000000000000, 0.9659258262890683122, 1.000000000000000000, 0.9659258262890683122, 1.000000000000000000, 0.9659258262890683122, 1.000000000000000000, 0.9659258262890683122, 1.000000000000000000, 0.9659258262890683122, 1.000000000000000000, 0.9659258262890683122, 1.000000000000000000, 0.9659258262890683122, 1.000000000000000000, 0.9659258262890683122, 1.000000000000000000, 0.9659258262890683122, 1.000000000000000000, 0.9659258262890683122, 1.000000000000000000, 0.9659258262890683122, 1.000000000000000000, 0.9659258262890683122, 1.000000000000000000, 0.9659258262890683122, 1.000000000000000000, 0.9659258262890683122, 1.000000000000000000, 0.9659258262890683122, 1.000000000000000000, 0.9659258262890683122, 1.000000000000000000, 0.9659258262890683122, 1.000000000000000000, 0.9659258262890683122, 1.000000000000000000, 0.9659258262890683122, 1.000000000000000000, 0.9659258262890683122, 1.000000000000000000, 0.9659258262890683122, 1.000000000000000000, 0.9659258262890683122, 1.000000000000000000, 0.9659258262890683122, 1.000000000000000000, 0.9659258262890683122, 1.000000000000000000, 0.9659258262890683122, 1.000000000000000000, 0.9659258262890683122, 1.000000000000000000, 0.9659258262890683122, 1.000000000000000000, 0.9659258262890683122, 1.000000000000000000, 0.9659258262890683122, 1.000000000000000000, 0.9659258262890683122, 1.000000000000000000, 0.9659258262890683122, 1.000000000000000000, 0.9659258262890683122, 1.000000000000000000, 0.9659258262890683122, 1.000000000000000000, 0.9659258262890683122, 1.000000000000000000, 0.9659258262890683122, 1.000000000000000000, 0.9659258262890683122, 1.000000000000000000, 0.9659258262890683122, 1.000000000000000000, 0.9659258262890683122, 1.000000000000000000, 0.9659258262890683122, 1.000000000000000000, 0.9659258262890683122, 1.000000000000000000, 0.9659258262890683122, 1.000000000000000000, 0.9659258262890683122, 1.000000000000000000, 0.9659258262890683122, 1.000000000000000000, 0.9659258262890683122, 1.000000000000000000, 0.9659258262890683122, 1.000000000000000000, 0.9659258262890683122, 1.000000000000000000, 0.9659258262890683122, 1.000000000000000000, 0.9659258262890683122, 1.000000000000000000, 0.9659258262890683122, 1.000000000000000000, 0.9659258262890683122, 1.000000000000000000, 0.9659258262890683122, 1.000000000000000000, 0.9659258262890683122, 1.000000000000000000, 0.9659258262890683122, 1.000000000000000000, 0.9659258262890683122, 1.000000000000000000, 0.9659258262890683122, 1.000000000000000000, 0.9659258262890683122, 1.000000000000000000, 0.9659258262890683122, 1.000000000000000000, 0.9659258262890683122, 1.000000000000000000, 0.9659258262890683122, 1.000000000000000000, 0.9659258262890683122, 1.000000000000000000, 0.9659258262890683122, 1.000000000000000000, 0.9659258262890683122, 1.000000000000000000, 0.9659258262890683122, 1.000000000000000000, 0.9659258262890683122, 1.000000000000000000, 0.9659258262890683122, 1.000000000000000000, 0.9659258262890683122, 1.000000000000000000, 0.9659258262890683122, 1.000000000000000000, 0.9659258262890683122, 1.000000000000000000, 0.9659258262890683122, 1.000000000000000000, 0.9659258262890683122, 1.000000000000000000, 0.9659258262890683122, 1.000000000000000000, 0.9659258262890683122, 1.000000000000000000, 0.9659258262890683122, 1.000000000000000000, 0.9659258262890683122, 1.000000000000000000, 0.9659258262890683122, 1.000000000000000000, 0.9659258262890683122, 1.000000000000000000, 0.9659258262890683122, 1.000000000000000000, 0.9659258262890683122, 1.000000000000000000, 0.9659258262890683122, 1.000000000000000000, 0.9659258262890683122, 1.000000000000000000, 0.9659258262890683122, 1.000000000000000000, 0.9659258262890683122, 1.000000000000000000, 0.9659258262890683122, 1.000000000000000000, 0.9659258262890683122, 1.000000000000000000, 0.9659258262890683122, 1.000000000000000000, 0.9659258262890683122, 1.000000000000000000, 0.9659258262890683122, 1.000000000000000000, 0.9659258262890683122, 1.000000000000000000, 0.9659258262890683122, 1.000000000000000000, 0.9659258262890683122, 1.000000000000000000, 0.9659258262890683122, 1.000000000000000000, 0.9659258262890683122, 1.000000000000000000, 0.9659258262890683122, 1.000000000000000000) ) ) 
 REPRESENTATION_ITEM ( '' )  SURFACE ( )  );
#73590 = ORIENTED_EDGE ( 'NONE', *, *, #49771, .F. ) ;
#73591 = LINE ( 'NONE', #20612, #49273 ) ;
#73592 = CARTESIAN_POINT ( 'NONE',  ( 18.95785429995052240, 47.24216108172004880, 6.499999999999941380 ) ) ;
#73593 = CARTESIAN_POINT ( 'NONE',  ( 14.92337183194729988, 39.34226448433412315, -8.527530157486177487 ) ) ;
#73594 = CARTESIAN_POINT ( 'NONE',  ( 24.16423886937410614, 64.30374883491396076, 8.672049930838204340E-16 ) ) ;
#73595 = CARTESIAN_POINT ( 'NONE',  ( 17.62281668512001076, 63.28593319516823357, 6.500000000000063061 ) ) ;
#73596 = ORIENTED_EDGE ( 'NONE', *, *, #1051, .T. ) ;
#73597 = DIRECTION ( 'NONE',  ( 1.257568779154408793E-17, 1.000000000000000000, -0.000000000000000000 ) ) ;
#73598 = CARTESIAN_POINT ( 'NONE',  ( 7.361572987183170547, 37.05059781766744464, 9.846743663894590881 ) ) ;
#73599 = ADVANCED_FACE ( 'NONE', ( #87187 ), #3712, .F. ) ;
#73600 = PRESENTATION_LAYER_ASSIGNMENT (  '', '', ( #8184 ) ) ;
#73601 = DIRECTION ( 'NONE',  ( 0.000000000000000000, -1.000000000000000000, 0.000000000000000000 ) ) ;
#73602 = CARTESIAN_POINT ( 'NONE',  ( 10.00000000000000000, 2.873634669930420049, -12.81628187352647608 ) ) ;
#73603 = CARTESIAN_POINT ( 'NONE',  ( 5.076628168052703671, 16.84226448433411960, 8.527530157486179263 ) ) ;
#73604 = CARTESIAN_POINT ( 'NONE',  ( 8.879999999999995453, 40.74999999999999289, -3.750000000000000000 ) ) ;
#73605 = CARTESIAN_POINT ( 'NONE',  ( 2.791683348922237240, 10.38393115100078390, -7.208316651077763204 ) ) ;
#73606 = CARTESIAN_POINT ( 'NONE',  ( -2.816281873526473856, 4.331968003263754419, 3.434112377981055619 ) ) ;
#73607 = DIRECTION ( 'NONE',  ( -0.5905099943842175847, -0.8070303256584298035, 0.000000000000000000 ) ) ;
#73608 = EDGE_CURVE ( 'NONE', #25822, #70902, #88662, .T. ) ;
#73609 = ORIENTED_EDGE ( 'NONE', *, *, #35042, .T. ) ;
#73610 = CARTESIAN_POINT ( 'NONE',  ( 20.88017736071110519, 5.563685344154838397, 2.639326808657452039E-16 ) ) ;
#73611 = CARTESIAN_POINT ( 'NONE',  ( -4.164238869374098151, 1.595415501580634388, -3.795296366450310543 ) ) ;
#73612 = CARTESIAN_POINT ( 'NONE',  ( 2.791683348922237240, 30.38393115100078390, -7.208316651077763204 ) ) ;
#73613 = CARTESIAN_POINT ( 'NONE',  ( -0.8801773607110991993, 52.85535201082151247, -2.915334737309923874 ) ) ;
#73614 = VECTOR ( 'NONE', #93576, 1000.000000000000114 ) ;
#73616 = DIRECTION ( 'NONE',  ( 0.000000000000000000, 1.000000000000000000, 0.000000000000000000 ) ) ;
#73615 = CARTESIAN_POINT ( 'NONE',  ( 19.38216949554541557, 27.24863466993041783, -9.382169495545420901 ) ) ;
#73617 = EDGE_CURVE ( 'NONE', #92561, #65076, #96183, .T. ) ;
#73618 = B_SPLINE_CURVE_WITH_KNOTS ( 'NONE', 3,
 ( #64889, #78934, #25467, #64409 ),
 .UNSPECIFIED., .F., .F.,
 ( 4, 4 ),
 ( 0.000000000000000000, 0.0003153927346769886298 ),
 .UNSPECIFIED. ) ;
#73619 = CARTESIAN_POINT ( 'NONE',  ( 64.56412365047461321, 11.49999999999999467, 9.500000000000000000 ) ) ;
#73620 = CARTESIAN_POINT ( 'NONE',  ( 9.065164099344539039, 0.3640475087720985714, -11.95084933600768018 ) ) ;
#73621 = CARTESIAN_POINT ( 'NONE',  ( 13.43411237798105340, 0.5819680032637533085, 12.81628187352647963 ) ) ;
#73622 = CARTESIAN_POINT ( 'NONE',  ( 7.361572987183170547, 12.05059781766744997, 9.846743663894590881 ) ) ;
#73623 = CARTESIAN_POINT ( 'NONE',  ( -10.88017736071109987, -26.72798132251183034, 2.915334737309934532 ) ) ;
#73624 = CARTESIAN_POINT ( 'NONE',  ( 0.6178305044545818747, 18.49863466993041428, -9.382169495545419124 ) ) ;
#73625 = CARTESIAN_POINT ( 'NONE',  ( -11.23890517432719882, -88.22482801183184620, -4.000000000000000000 ) ) ;
#73627 = CARTESIAN_POINT ( 'NONE',  ( 9.159723438033129383, 0.000000000000000000, 10.91613331444548507 ) ) ;
#73626 = CARTESIAN_POINT ( 'NONE',  ( 20.88017736071110875, 20.77201867748816611, -2.915334737309920765 ) ) ;
#73628 = CARTESIAN_POINT ( 'NONE',  ( -10.04755927614737843, 15.00000000000000533, -10.62803196998870803 ) ) ;
#73629 = CARTESIAN_POINT ( 'NONE',  ( 2.917880565312950480, 45.97041550158063927, -12.26659068614894821 ) ) ;
#73630 = FILL_AREA_STYLE ('',( #57646 ) ) ;
#73631 = CARTESIAN_POINT ( 'NONE',  ( -0.8801773607111008646, 23.27201867748817676, 2.915334737309923430 ) ) ;
#73632 = CARTESIAN_POINT ( 'NONE',  ( 0.1532563361054083140, 51.00893115100078745, 1.131784320476157264E-15 ) ) ;
#73633 = CARTESIAN_POINT ( 'NONE',  ( 7.084665262690076126, 54.10535201082151247, 10.88017736071109987 ) ) ;
#73634 = CARTESIAN_POINT ( 'NONE',  ( 6.204703633549690345, 35.76208216824729647, -14.16423886937410259 ) ) ;
#73635 = CARTESIAN_POINT ( 'NONE',  ( 5.076628168052704559, 40.17559781766745175, -8.527530157486179263 ) ) ;
#73636 = CARTESIAN_POINT ( 'NONE',  ( 6.565887622018943937, 63.08196800326376064, -12.81628187352647608 ) ) ;
#73637 = CARTESIAN_POINT ( 'NONE',  ( 19.84674366389459266, 63.71726448433412315, -2.638427012816827677 ) ) ;
#73638 = ORIENTED_EDGE ( 'NONE', *, *, #92714, .F. ) ;
#73639 = CARTESIAN_POINT ( 'NONE',  ( -0.8801773607111009756, 18.06368534415484106, 1.068504757029289695E-15 ) ) ;
#73640 = CARTESIAN_POINT ( 'NONE',  ( 17.88864439015886276, 91.03707094060693805, -8.000000000000000000 ) ) ;
#73641 = CARTESIAN_POINT ( 'NONE',  ( 6.732888861736110009, -58.30752899003807954, 3.750000000000001776 ) ) ;
#73642 = CARTESIAN_POINT ( 'NONE',  ( 0.5774900079438607392, 8.480352010821505360, 5.440088680355550821 ) ) ;
#73643 = CARTESIAN_POINT ( 'NONE',  ( 10.00000000000000178, 2.258931151000784787, 9.846743663894594434 ) ) ;
#73644 = CARTESIAN_POINT ( 'NONE',  ( 13.79529636645030344, 23.26208216824730002, 14.16423886937410614 ) ) ;
#73645 = CARTESIAN_POINT ( 'NONE',  ( 12.63842701281683034, 7.467264484334118713, 9.846743663894596210 ) ) ;
#73646 = CARTESIAN_POINT ( 'NONE',  ( 19.84674366389459266, 58.30059781766745886, 2.638427012816836559 ) ) ;
#73647 = CARTESIAN_POINT ( 'NONE',  ( 20.88017736071110875, 35.77201867748816966, -2.915334737309920765 ) ) ;
#73648 = DIRECTION ( 'NONE',  ( 0.9999619230641714207, 0.000000000000000000, -0.008726535498360278933 ) ) ;
#73649 = CARTESIAN_POINT ( 'NONE',  ( 19.72487221294570858, 0.5000000000000000000, 6.500000000000000888 ) ) ;
#73650 = TOROIDAL_SURFACE ( 'NONE', #70469, 0.5000000000000000000, 0.2500000000000000000 ) ;
#73651 = EDGE_CURVE ( 'NONE', #40543, #74503, #42199, .T. ) ;
#73652 = ORIENTED_EDGE ( 'NONE', *, *, #85438, .F. ) ;
#73653 = CARTESIAN_POINT ( 'NONE',  ( 4.323020469704055735, -6.401304200527818011, 2.499999999999999556 ) ) ;
#73654 = CARTESIAN_POINT ( 'NONE',  ( 0.1532563361054082862, 46.21726448433411605, 2.638427012816831674 ) ) ;
#73655 = ORIENTED_EDGE ( 'NONE', *, *, #17045, .F. ) ;
#73656 = ORIENTED_EDGE ( 'NONE', *, *, #79762, .F. ) ;
#73657 = PRESENTATION_LAYER_ASSIGNMENT (  '', '', ( #22587 ) ) ;
#73658 = CARTESIAN_POINT ( 'NONE',  ( 0.5774900079438590739, 62.64701867748817676, -5.440088680355550821 ) ) ;
#73659 = CARTESIAN_POINT ( 'NONE',  ( 10.00000000000000000, 15.55374883491396787, -14.16423886937410082 ) ) ;
#73660 = CARTESIAN_POINT ( 'NONE',  ( 13.79529636645031943, 10.34541550158063394, -14.16423886937409904 ) ) ;
#73661 = CARTESIAN_POINT ( 'NONE',  ( 7.084665262690076126, 57.02201867748817676, -10.88017736071110164 ) ) ;
#73662 = CARTESIAN_POINT ( 'NONE',  ( 10.00000000000000178, 53.05374883491396787, 14.16423886937410082 ) ) ;
#73663 = CARTESIAN_POINT ( 'NONE',  ( 0.1532563361054082862, 36.21726448433410894, 2.638427012816831674 ) ) ;
#73664 = DIRECTION ( 'NONE',  ( 1.000000000000000000, -0.000000000000000000, -0.000000000000000000 ) ) ;
#73666 = CARTESIAN_POINT ( 'NONE',  ( 22.81628187352647785, 6.623634669930420493, 6.195893100308588602E-16 ) ) ;
#73665 = CARTESIAN_POINT ( 'NONE',  ( 0.5774900079438590739, 32.64701867748816966, -5.440088680355550821 ) ) ;
#73667 = CARTESIAN_POINT ( 'NONE',  ( 24.16423886937410614, 4.303748834913967869, 8.672049930838204340E-16 ) ) ;
#73668 = CARTESIAN_POINT ( 'NONE',  ( 20.36894250292379382, 53.67874883491397497, 10.36894250292379205 ) ) ;
#73669 = CARTESIAN_POINT ( 'NONE',  ( 0.5774900079438607392, 18.48035201082150536, 5.440088680355550821 ) ) ;
#73670 = DIRECTION ( 'NONE',  ( 1.000000000000000000, 0.000000000000000000, 0.000000000000000000 ) ) ;
#73671 = CARTESIAN_POINT ( 'NONE',  ( 17.96484262340118221, 49.93868534415484106, 7.964842623401181321 ) ) ;
#73672 = CARTESIAN_POINT ( 'NONE',  ( 8.879999999999991900, 69.99999999999998579, -6.396446609406726935 ) ) ;
#73673 = EDGE_LOOP ( 'NONE', ( #82554, #76758, #68186, #79117 ) ) ;
#73674 = DIRECTION ( 'NONE',  ( 0.000000000000000000, -0.000000000000000000, -1.000000000000000000 ) ) ;
#73675 = ORIENTED_EDGE ( 'NONE', *, *, #902, .F. ) ;
#73676 = VERTEX_POINT ( 'NONE', #11690 ) ;
#73677 = CARTESIAN_POINT ( 'NONE',  ( 20.36894250292379738, 44.92874883491396787, -10.36894250292379027 ) ) ;
#73678 = CARTESIAN_POINT ( 'NONE',  ( 19.84674366389459266, 53.30059781766744464, 2.638427012816836559 ) ) ;
#73679 = CARTESIAN_POINT ( 'NONE',  ( 2.035157376598822676, 62.43868534415483396, -7.964842623401177768 ) ) ;
#73680 = CARTESIAN_POINT ( 'NONE',  ( -2.602060718268879747, 0.000000000000000000, 4.792399674598840420 ) ) ;
#73681 = CARTESIAN_POINT ( 'NONE',  ( 4.559911319644449179, 53.89701867748817676, 9.422509992056141925 ) ) ;
#73682 = CARTESIAN_POINT ( 'NONE',  ( 6.565887622018943937, 60.16530133659707502, 12.81628187352647430 ) ) ;
#73683 = CARTESIAN_POINT ( 'NONE',  ( -12.81628187352647608, 4.123634669930424934, 3.903127820947815962E-15 ) ) ;
#73684 = EDGE_LOOP ( 'NONE', ( #36666, #19925, #8889, #14319, #46661, #8876, #49829, #15158 ) ) ;
#73685 = CARTESIAN_POINT ( 'NONE',  ( 17.96484262340118221, 49.93868534415484106, 7.964842623401181321 ) ) ;
#73686 = CIRCLE ( 'NONE', #88039, 2.999999999999999112 ) ;
#73687 = CARTESIAN_POINT ( 'NONE',  ( -0.3689425029237881626, 22.42874883491397142, 10.36894250292379027 ) ) ;
#73688 = ORIENTED_EDGE ( 'NONE', *, *, #46181, .T. ) ;
#73689 = CARTESIAN_POINT ( 'NONE',  ( -2.816281873526473856, 24.12363466993042138, 9.499525473075851096E-16 ) ) ;
#73690 = ORIENTED_EDGE ( 'NONE', *, *, #41252, .T. ) ;
#73691 = CARTESIAN_POINT ( 'NONE',  ( -2.816281873526473856, 44.12363466993042493, 9.499525473075851096E-16 ) ) ;
#73692 = CARTESIAN_POINT ( 'NONE',  ( 7.084665262690076126, 14.10535201082150358, 10.88017736071109987 ) ) ;
#73693 = CARTESIAN_POINT ( 'NONE',  ( 19.84674366389459266, 38.30059781766745175, 2.638427012816836559 ) ) ;
#73694 = CARTESIAN_POINT ( 'NONE',  ( 19.42250999205614548, 10.98035201082150358, -5.440088680355545492 ) ) ;
#73695 = MECHANICAL_DESIGN_GEOMETRIC_PRESENTATION_REPRESENTATION (  '', ( #92895 ), #46587 ) ;
#73696 = CARTESIAN_POINT ( 'NONE',  ( 10.00000000000000000, 57.87363466993042493, -12.81628187352647608 ) ) ;
#73697 = DIRECTION ( 'NONE',  ( 0.000000000000000000, 0.000000000000000000, -1.000000000000000000 ) ) ;
#73699 = EDGE_CURVE ( 'NONE', #71199, #24915, #2217, .T. ) ;
#73698 = CARTESIAN_POINT ( 'NONE',  ( 19.84674366389459621, 38.50893115100078745, 7.409399052514197653E-17 ) ) ;
#73701 = ORIENTED_EDGE ( 'NONE', *, *, #27363, .T. ) ;
#73700 = CARTESIAN_POINT ( 'NONE',  ( 9.722841580490404922, -0.03417435944610275333, 12.70211588817942960 ) ) ;
#73702 = CARTESIAN_POINT ( 'NONE',  ( -3.420591144908684988, 14.49999999999999112, 14.60477854057959313 ) ) ;
#73703 = DIRECTION ( 'NONE',  ( -0.000000000000000000, -1.000000000000000000, -0.000000000000000000 ) ) ;
#73704 = CARTESIAN_POINT ( 'NONE',  ( -9.402796353260967521, 0.5000000000000004441, -11.68706210897770248 ) ) ;
#73705 = ADVANCED_FACE ( 'NONE', ( #48204 ), #26683, .T. ) ;
#73706 = DIRECTION ( 'NONE',  ( -0.000000000000000000, 1.000000000000000000, -0.000000000000000000 ) ) ;
#73707 = CARTESIAN_POINT ( 'NONE',  ( 14.92337183194729988, 24.34226448433411960, -8.527530157486177487 ) ) ;
#73708 = EDGE_CURVE ( 'NONE', #63731, #15285, #65406, .T. ) ;
#73709 = CARTESIAN_POINT ( 'NONE',  ( 16.40814093676323893, 25.79030133659708923, 11.09922568453595026 ) ) ;
#73710 = CARTESIAN_POINT ( 'NONE',  ( 3.420591144908548653, 0.3640475087720985714, -14.60477854057957003 ) ) ;
#73711 = EDGE_LOOP ( 'NONE', ( #21150, #8545, #90554, #95866 ) ) ;
#73712 = CARTESIAN_POINT ( 'NONE',  ( 2.791683348922240793, 56.63393115100078035, 7.208316651077764092 ) ) ;
#73713 = DIRECTION ( 'NONE',  ( -1.000000000000000000, 0.000000000000000000, 0.000000000000000000 ) ) ;
#73714 = CARTESIAN_POINT ( 'NONE',  ( 22.26659068614895176, 24.72041550158063572, -7.082119434687042414 ) ) ;
#73715 = CARTESIAN_POINT ( 'NONE',  ( 0.1532563361054083140, 41.00893115100078745, 1.131784320476157264E-15 ) ) ;
#73716 = B_SPLINE_CURVE_WITH_KNOTS ( 'NONE', 3,
 ( #65830, #81335, #59317, #89816, #36831, #72836 ),
 .UNSPECIFIED., .F., .F.,
 ( 4, 2, 4 ),
 ( 0.0002800421826021987559, 0.0006862478247342195751, 0.001092453466866240286 ),
 .UNSPECIFIED. ) ;
#73717 = CARTESIAN_POINT ( 'NONE',  ( 10.00000000000000178, 40.37363466993042493, 12.81628187352647608 ) ) ;
#73719 = FILL_AREA_STYLE_COLOUR ( '', #17753 ) ;
#73718 = CARTESIAN_POINT ( 'NONE',  ( 2.930023131210739873, 0.000000000000000000, 4.599215049682178424 ) ) ;
#73720 = CARTESIAN_POINT ( 'NONE',  ( 10.00000000000000178, 64.31368534415483396, 10.88017736071110342 ) ) ;
#73721 = B_SPLINE_CURVE_WITH_KNOTS ( 'NONE', 3,
 ( #44645, #77597, #23649, #45633, #53131, #61122 ),
 .UNSPECIFIED., .F., .F.,
 ( 4, 2, 4 ),
 ( 0.000000000000000000, 0.0003798359240359669084, 0.0007596718480719338168 ),
 .UNSPECIFIED. ) ;
#73722 = FACE_OUTER_BOUND ( 'NONE', #32385, .T. ) ;
#73723 = CARTESIAN_POINT ( 'NONE',  ( 19.84674366389459266, 28.71726448433411960, -2.638427012816827677 ) ) ;
#73724 = CARTESIAN_POINT ( 'NONE',  ( 0.5774900079438607392, 38.48035201082150536, 5.440088680355550821 ) ) ;
#73725 = CARTESIAN_POINT ( 'NONE',  ( 3.591859063236761518, 44.95696800326376064, 11.09922568453594849 ) ) ;
#73726 = CARTESIAN_POINT ( 'NONE',  ( 0.1532563361054082862, 36.21726448433410894, 2.638427012816831674 ) ) ;
#73727 = CARTESIAN_POINT ( 'NONE',  ( -13.42719148503447357, 90.83520141668820713, 7.724461209138537399 ) ) ;
#73728 = VECTOR ( 'NONE', #97089, 1000.000000000000000 ) ;
#73729 = EDGE_CURVE ( 'NONE', #52968, #8141, #92858, .T. ) ;
#73730 = CARTESIAN_POINT ( 'NONE',  ( -0.8801773607110991993, 37.85535201082151247, -2.915334737309923874 ) ) ;
#73731 = ORIENTED_EDGE ( 'NONE', *, *, #87477, .T. ) ;
#73732 = CARTESIAN_POINT ( 'NONE',  ( -3.014428414850123250, 6.159700295649318313, 11.25000000000000178 ) ) ;
#73733 = CARTESIAN_POINT ( 'NONE',  ( 17.96484262340118221, 19.93868534415484106, 7.964842623401181321 ) ) ;
#73735 = CARTESIAN_POINT ( 'NONE',  ( 20.88017736071110164, 40.35535201082150536, 2.915334737309930979 ) ) ;
#73734 = CARTESIAN_POINT ( 'NONE',  ( 1.472469842513823179, 60.59226448433412315, -4.923371831947296329 ) ) ;
#73736 = CARTESIAN_POINT ( 'NONE',  ( 2.831191079880678085, 79.91181047996344944, -5.000000000000000000 ) ) ;
#73737 = EDGE_CURVE ( 'NONE', #11511, #17245, #60627, .T. ) ;
#73738 = CARTESIAN_POINT ( 'NONE',  ( 4.559911319644449179, 58.89701867748817676, 9.422509992056141925 ) ) ;
#73740 = CARTESIAN_POINT ( 'NONE',  ( 19.72487221294571569, 40.71833443783938122, -6.499999999999989342 ) ) ;
#73739 = CARTESIAN_POINT ( 'NONE',  ( 17.96484262340118221, 29.93868534415484106, 7.964842623401181321 ) ) ;
#73741 = CARTESIAN_POINT ( 'NONE',  ( 7.361572987183170547, 2.050597817667451750, 9.846743663894590881 ) ) ;
#73742 = CARTESIAN_POINT ( 'NONE',  ( 2.791683348922240793, 26.63393115100078745, 7.208316651077764092 ) ) ;
#73743 = CARTESIAN_POINT ( 'NONE',  ( 3.795296366450306547, 10.34541550158063394, -14.16423886937410259 ) ) ;
#73744 = CARTESIAN_POINT ( 'NONE',  ( 14.92337183194729988, 54.34226448433412315, -8.527530157486177487 ) ) ;
#73746 = CARTESIAN_POINT ( 'NONE',  ( 21.92686044187657401, 20.37045670184114243, -3.195792623639525765 ) ) ;
#73745 = CARTESIAN_POINT ( 'NONE',  ( -2.266590686148945544, 47.22041550158063927, 7.082119434687048631 ) ) ;
#73747 = DIRECTION ( 'NONE',  ( -5.818595309480553908E-17, -1.000000000000000000, 0.000000000000000000 ) ) ;
#73748 = CARTESIAN_POINT ( 'NONE',  ( 13.79529636645031943, 10.34541550158063394, -14.16423886937409904 ) ) ;
#73749 = CARTESIAN_POINT ( 'NONE',  ( 17.08211943468705840, 35.13708216824730357, -12.26659068614894466 ) ) ;
#73750 = CIRCLE ( 'NONE', #13088, 14.49999999999999822 ) ;
#73751 = CARTESIAN_POINT ( 'NONE',  ( 10.00000000000000000, 2.873634669930420049, -12.81628187352647608 ) ) ;
#73752 = ORIENTED_EDGE ( 'NONE', *, *, #44824, .T. ) ;
#73753 = CARTESIAN_POINT ( 'NONE',  ( 19.42250999205614548, 10.98035201082150536, -5.440088680355545492 ) ) ;
#73754 = CARTESIAN_POINT ( 'NONE',  ( 0.1532563361054082862, 41.21726448433411605, 2.638427012816831674 ) ) ;
#73756 = DIRECTION ( 'NONE',  ( -1.000000000000000000, 0.000000000000000000, 0.000000000000000000 ) ) ;
#73755 = DIRECTION ( 'NONE',  ( 0.000000000000000000, -1.000000000000000000, 0.000000000000000000 ) ) ;
#73757 = DIRECTION ( 'NONE',  ( 1.000000000000000000, 2.569960705150826877E-16, -0.000000000000000000 ) ) ;
#73758 = PRESENTATION_LAYER_ASSIGNMENT (  '', '', ( #37028 ) ) ;
#73759 = CARTESIAN_POINT ( 'NONE',  ( 6.565887622018943937, 20.16530133659708213, 12.81628187352647430 ) ) ;
#73760 = CARTESIAN_POINT ( 'NONE',  ( 18.52753015748618282, 28.92559781766745175, -4.923371831947291888 ) ) ;
#73761 = ORIENTED_EDGE ( 'NONE', *, *, #63902, .F. ) ;
#73762 = CARTESIAN_POINT ( 'NONE',  ( 10.00000000000000178, 12.25893115100078568, 9.846743663894594434 ) ) ;
#73763 = CIRCLE ( 'NONE', #75418, 2.999999999999997780 ) ;
#73764 = DIRECTION ( 'NONE',  ( -1.000000000000000000, 5.782411586589362323E-17, 0.000000000000000000 ) ) ;
#73765 = CARTESIAN_POINT ( 'NONE',  ( -4.164238869374099927, 67.01208216824728936, 3.795296366450308767 ) ) ;
#73766 = CARTESIAN_POINT ( 'NONE',  ( 17.96484262340118221, 9.938685344154837509, 7.964842623401181321 ) ) ;
#73767 = CARTESIAN_POINT ( 'NONE',  ( 24.16423886937410614, 39.51208216824731068, -3.795296366450302550 ) ) ;
#73768 = CARTESIAN_POINT ( 'NONE',  ( 10.00000000000000000, 46.81368534415484106, -10.88017736071110342 ) ) ;
#73769 = CARTESIAN_POINT ( 'NONE',  ( 17.96484262340118221, 59.93868534415484106, 7.964842623401181321 ) ) ;
#73770 = CARTESIAN_POINT ( 'NONE',  ( 8.880000000000020322, 80.07179676972448590, -6.500000000000000888 ) ) ;
#73771 = CARTESIAN_POINT ( 'NONE',  ( 0.000000000000000000, -97.00000000000000000, -2.750000000000000000 ) ) ;
#73772 = CARTESIAN_POINT ( 'NONE',  ( 7.361572987183170547, 17.05059781766745530, 9.846743663894590881 ) ) ;
#73773 = DIRECTION ( 'NONE',  ( 0.000000000000000000, 0.000000000000000000, 1.000000000000000000 ) ) ;
#73774 = CARTESIAN_POINT ( 'NONE',  ( 0.1532563361054083140, 11.00893115100078568, 1.131784320476157264E-15 ) ) ;
#73775 = DIRECTION ( 'NONE',  ( 1.000000000000000000, 0.000000000000000000, 0.000000000000000000 ) ) ;
#73776 = CARTESIAN_POINT ( 'NONE',  ( 17.20831665107776587, 39.13393115100079456, -7.208316651077762316 ) ) ;
#73777 = CARTESIAN_POINT ( 'NONE',  ( 19.84674366389459621, 58.50893115100078745, 7.409399052514197653E-17 ) ) ;
#73778 = CARTESIAN_POINT ( 'NONE',  ( 20.88017736071110875, 30.77201867748816966, -2.915334737309920765 ) ) ;
#73779 = ORIENTED_EDGE ( 'NONE', *, *, #86306, .F. ) ;
#73780 = CARTESIAN_POINT ( 'NONE',  ( 19.38216949554541202, 45.99863466993041072, 9.382169495545424454 ) ) ;
#73781 = PLANE ( 'NONE',  #84350 ) ;
#73782 = CARTESIAN_POINT ( 'NONE',  ( -0.8801773607111009756, 68.06368534415484817, 1.068504757029289695E-15 ) ) ;
#73783 = CARTESIAN_POINT ( 'NONE',  ( 13.43411237798106583, 37.66530133659708923, -12.81628187352647252 ) ) ;
#73785 = CARTESIAN_POINT ( 'NONE',  ( 14.92337183194729988, 39.34226448433412315, -8.527530157486177487 ) ) ;
#73784 = CARTESIAN_POINT ( 'NONE',  ( -4.164238869374099927, 57.01208216824731068, 3.795296366450308767 ) ) ;
#73786 = CARTESIAN_POINT ( 'NONE',  ( 6.715867195167361636, 4.143177415744058416E-16, 12.85095824508331930 ) ) ;
#73787 = CARTESIAN_POINT ( 'NONE',  ( 5.076628168052703671, 66.84226448433412315, 8.527530157486179263 ) ) ;
#73788 = CARTESIAN_POINT ( 'NONE',  ( 24.16423886937409904, 39.09541550158062506, 3.795296366450317205 ) ) ;
#73789 = CARTESIAN_POINT ( 'NONE',  ( 19.84674366389459266, 38.30059781766745175, 2.638427012816836559 ) ) ;
#73790 = CARTESIAN_POINT ( 'NONE',  ( 17.84635730667657327, 8.637910973973182749, 6.499999999999990230 ) ) ;
#73791 = CARTESIAN_POINT ( 'NONE',  ( 12.91533473730993009, 31.60535201082150891, -10.88017736071109987 ) ) ;
#73792 = CARTESIAN_POINT ( 'NONE',  ( 4.559911319644449179, 62.23035201082150536, -9.422509992056141925 ) ) ;
#73793 = LINE ( 'NONE', #74279, #12658 ) ;
#73794 = VERTEX_POINT ( 'NONE', #7149 ) ;
#73795 = CARTESIAN_POINT ( 'NONE',  ( 19.38216949554541557, 42.24863466993041783, -9.382169495545420901 ) ) ;
#73796 = CARTESIAN_POINT ( 'NONE',  ( 4.559911319644449179, 62.23035201082150536, -9.422509992056141925 ) ) ;
#73797 = ORIENTED_EDGE ( 'NONE', *, *, #41162, .T. ) ;
#73798 = EDGE_CURVE ( 'NONE', #38896, #538, #68150, .T. ) ;
#73799 =( NAMED_UNIT ( * ) SI_UNIT ( $, .STERADIAN. ) SOLID_ANGLE_UNIT ( ) );
#73800 = CARTESIAN_POINT ( 'NONE',  ( 7.361572987183169658, 9.967264484334119601, -9.846743663894592657 ) ) ;
#73801 = CARTESIAN_POINT ( 'NONE',  ( -0.2418659066527710233, 60.11633188102327807, 6.114288769123046308 ) ) ;
#73802 = VERTEX_POINT ( 'NONE', #89653 ) ;
#73803 = CARTESIAN_POINT ( 'NONE',  ( -1.926860441876563801, 12.66212336850780495, 1.004413902775740978E-15 ) ) ;
#73804 = CARTESIAN_POINT ( 'NONE',  ( 17.96484262340118221, 11.18868534415483929, -7.964842623401177768 ) ) ;
#73805 = VECTOR ( 'NONE', #72344, 1000.000000000000000 ) ;
#73806 = CARTESIAN_POINT ( 'NONE',  ( 1.472469842513823179, 1.425597817667451528, 4.923371831947296329 ) ) ;
#73807 = CARTESIAN_POINT ( 'NONE',  ( -2.266590686148945544, 21.38708216824730357, -7.082119434687050408 ) ) ;
#73808 = CARTESIAN_POINT ( 'NONE',  ( 20.88017736071110875, 25.77201867748816966, -2.915334737309920765 ) ) ;
#73809 = CARTESIAN_POINT ( 'NONE',  ( 14.92337183194729633, 62.67559781766745886, 8.527530157486181039 ) ) ;
#73810 = ORIENTED_EDGE ( 'NONE', *, *, #902, .T. ) ;
#73811 = CARTESIAN_POINT ( 'NONE',  ( 7.361572987183170547, 62.05059781766745886, 9.846743663894590881 ) ) ;
#73812 = VERTEX_POINT ( 'NONE', #28163 ) ;
#73813 = CARTESIAN_POINT ( 'NONE',  ( 17.20831665107776587, 2.883931151000785231, 7.208316651077764980 ) ) ;
#73814 = CARTESIAN_POINT ( 'NONE',  ( 18.52753015748618282, 63.92559781766745886, -4.923371831947291888 ) ) ;
#73815 = EDGE_CURVE ( 'NONE', #61124, #49583, #29625, .T. ) ;
#73817 = CARTESIAN_POINT ( 'NONE',  ( 0.000000000000000000, 14.49999999999999822, 0.000000000000000000 ) ) ;
#73816 = CARTESIAN_POINT ( 'NONE',  ( 12.91533473730993009, 11.60535201082150536, -10.88017736071109987 ) ) ;
#73818 = CARTESIAN_POINT ( 'NONE',  ( 10.00000000000000178, 69.31368534415484817, 10.88017736071110342 ) ) ;
#73819 = CARTESIAN_POINT ( 'NONE',  ( 7.084665262690076126, 24.10535201082150181, 10.88017736071109987 ) ) ;
#73820 = PRESENTATION_LAYER_ASSIGNMENT (  '', '', ( #81812 ) ) ;
#73821 = ADVANCED_FACE ( 'NONE', ( #67658, #20669, #37164 ), #83140, .F. ) ;
#73822 = ORIENTED_EDGE ( 'NONE', *, *, #77005, .T. ) ;
#73823 = CARTESIAN_POINT ( 'NONE',  ( 2.035157376598824452, 43.68868534415484106, 7.964842623401179544 ) ) ;
#73824 = CARTESIAN_POINT ( 'NONE',  ( -7.882504294824035362, 1.541599964002826617E-16, 12.32089577884786458 ) ) ;
#73825 = CARTESIAN_POINT ( 'NONE',  ( 0.6178305044545818747, 38.49863466993042493, -9.382169495545419124 ) ) ;
#73826 = CARTESIAN_POINT ( 'NONE',  ( 0.5774900079438590739, 42.64701867748816966, -5.440088680355550821 ) ) ;
#73827 = EDGE_CURVE ( 'NONE', #97731, #2418, #20169, .T. ) ;
#73828 = AXIS2_PLACEMENT_3D ( 'NONE', #38811, #97351, #36836 ) ;
#73829 = CIRCLE ( 'NONE', #5199, 15.00000000000000000 ) ;
#73830 = CARTESIAN_POINT ( 'NONE',  ( 12.63842701281683034, 57.46726448433411605, 9.846743663894596210 ) ) ;
#73831 = VERTEX_POINT ( 'NONE', #59145 ) ;
#73833 = CARTESIAN_POINT ( 'NONE',  ( -0.2838433074297238012, 13.12729635533385597, 9.500000000000000000 ) ) ;
#73832 = STYLED_ITEM ( 'NONE', ( #93872 ), #92244 ) ;
#73834 = CARTESIAN_POINT ( 'NONE',  ( 14.92337183194729633, 22.67559781766745175, 8.527530157486181039 ) ) ;
#73835 = VECTOR ( 'NONE', #37877, 1000.000000000000000 ) ;
#73836 = CARTESIAN_POINT ( 'NONE',  ( 16.40814093676324603, 12.45696800326375353, -11.09922568453594671 ) ) ;
#73838 = CARTESIAN_POINT ( 'NONE',  ( 5.076628168052704559, 60.17559781766745175, -8.527530157486179263 ) ) ;
#73837 = CARTESIAN_POINT ( 'NONE',  ( -13.80078213431832346, 90.89651191443149969, -7.751965754689354782 ) ) ;
#73839 = CARTESIAN_POINT ( 'NONE',  ( 17.96484262340118221, 16.18868534415483396, -7.964842623401177768 ) ) ;
#73840 = CARTESIAN_POINT ( 'NONE',  ( 5.076628168052704559, 55.17559781766745175, -8.527530157486179263 ) ) ;
#73841 = DIRECTION ( 'NONE',  ( -0.9762960071199316969, 0.000000000000000000, -0.2164396139381103701 ) ) ;
#73842 = DIRECTION ( 'NONE',  ( -0.000000000000000000, -1.000000000000000000, -0.000000000000000000 ) ) ;
#73843 = CARTESIAN_POINT ( 'NONE',  ( 1.472469842513823179, 10.59226448433411782, -4.923371831947296329 ) ) ;
#73844 = LINE ( 'NONE', #97361, #47363 ) ;
#73846 = ORIENTED_EDGE ( 'NONE', *, *, #13123, .F. ) ;
#73845 = CARTESIAN_POINT ( 'NONE',  ( -2.816281873526473856, 4.331968003263754419, 3.434112377981055619 ) ) ;
#73847 = VECTOR ( 'NONE', #75739, 1000.000000000000000 ) ;
#73848 = CARTESIAN_POINT ( 'NONE',  ( 7.264948169187374738, 14.76930270348881180, 13.05597881399723903 ) ) ;
#73849 = CARTESIAN_POINT ( 'NONE',  ( 21.09922568453594849, 41.20696800326375353, 6.408140936763242479 ) ) ;
#73850 = CARTESIAN_POINT ( 'NONE',  ( 18.52753015748617571, 28.09226448433411960, 4.923371831947298993 ) ) ;
#73851 = CARTESIAN_POINT ( 'NONE',  ( -5.093587308868599450, 15.00000000000000000, 15.16353404595993837 ) ) ;
#73852 = CARTESIAN_POINT ( 'NONE',  ( -2.266590686148945544, 56.38708216824731068, -7.082119434687050408 ) ) ;
#73853 = CARTESIAN_POINT ( 'NONE',  ( 0.1532563361054083140, 31.00893115100078390, 1.131784320476157264E-15 ) ) ;
#73854 = VERTEX_POINT ( 'NONE', #5181 ) ;
#73855 = CARTESIAN_POINT ( 'NONE',  ( -12.60874940350953111, 3.965829894984375834E-16, 7.160268045226943379 ) ) ;
#73856 = CARTESIAN_POINT ( 'NONE',  ( 13.79529636645030344, 58.26208216824728936, 14.16423886937410614 ) ) ;
#73857 = CARTESIAN_POINT ( 'NONE',  ( -9.098828036256710661, 88.10682954397121591, -5.081100641017341601 ) ) ;
#73858 = EDGE_CURVE ( 'NONE', #48625, #87096, #14665, .T. ) ;
#73859 = CARTESIAN_POINT ( 'NONE',  ( 17.96484262340118221, 24.93868534415484461, 7.964842623401181321 ) ) ;
#73860 =( GEOMETRIC_REPRESENTATION_CONTEXT ( 3 ) GLOBAL_UNCERTAINTY_ASSIGNED_CONTEXT ( ( #93196 ) ) GLOBAL_UNIT_ASSIGNED_CONTEXT ( ( #25423, #63868, #55409 ) ) REPRESENTATION_CONTEXT ( 'NONE', 'WORKASPACE' ) );
#73861 = CARTESIAN_POINT ( 'NONE',  ( 22.26659068614895176, 34.72041550158063927, -7.082119434687042414 ) ) ;
#73862 = CARTESIAN_POINT ( 'NONE',  ( 24.16423886937409904, 59.09541550158063217, 3.795296366450317205 ) ) ;
#73863 = CARTESIAN_POINT ( 'NONE',  ( 0.2751277870542909731, 22.28217586085237656, -6.499999999999992006 ) ) ;
#73864 = CARTESIAN_POINT ( 'NONE',  ( 12.63842701281683922, 9.550597817667449974, -9.846743663894590881 ) ) ;
#73865 = CARTESIAN_POINT ( 'NONE',  ( 0.1532563361054083140, 66.00893115100079456, 1.131784320476157264E-15 ) ) ;
#73866 = ORIENTED_EDGE ( 'NONE', *, *, #19545, .T. ) ;
#73867 = CARTESIAN_POINT ( 'NONE',  ( 15.44008868035555793, 46.39701867748817676, -9.422509992056140149 ) ) ;
#73868 = CARTESIAN_POINT ( 'NONE',  ( 10.94841663143097144, -97.13876569039521769, 3.750000000000000000 ) ) ;
#73869 = CARTESIAN_POINT ( 'NONE',  ( 12.63842701281683922, 59.55059781766744464, -9.846743663894590881 ) ) ;
#73870 = DIRECTION ( 'NONE',  ( 0.000000000000000000, 1.000000000000000000, -0.000000000000000000 ) ) ;
#73871 = CARTESIAN_POINT ( 'NONE',  ( 2.791683348922240793, 66.63393115100079456, 7.208316651077764092 ) ) ;
#73873 = CARTESIAN_POINT ( 'NONE',  ( 14.48718990079892066, 15.00000000000000000, 0.6093675230841449908 ) ) ;
#73872 =( BOUNDED_CURVE ( )  B_SPLINE_CURVE ( 3, ( #28175, #42691, #66163, #74153 ),
 .UNSPECIFIED., .F., .F. ) 
 B_SPLINE_CURVE_WITH_KNOTS ( ( 4, 4 ),
 ( 3.141592653589793116, 4.712388980384696779 ),
 .UNSPECIFIED. ) 
 CURVE ( )  GEOMETRIC_REPRESENTATION_ITEM ( )  RATIONAL_B_SPLINE_CURVE ( ( 1.000000000000000000, 0.8047378541243632721, 0.8047378541243632721, 1.000000000000000000 ) ) 
 REPRESENTATION_ITEM ( '' )  );
#73874 = CIRCLE ( 'NONE', #33963, 1.000000000000007772 ) ;
#73875 = CARTESIAN_POINT ( 'NONE',  ( 19.72487221294571569, 14.78217586085237656, 6.499999999999995559 ) ) ;
#73876 = ORIENTED_EDGE ( 'NONE', *, *, #88262, .F. ) ;
#73877 = CARTESIAN_POINT ( 'NONE',  ( -4.164238869374098151, 36.59541550158063217, -3.795296366450310543 ) ) ;
#73878 = DIRECTION ( 'NONE',  ( -0.6087614290087242086, 0.000000000000000000, 0.7933533402912323895 ) ) ;
#73879 = CARTESIAN_POINT ( 'NONE',  ( 20.88017736071110164, 20.35535201082150891, 2.915334737309930979 ) ) ;
#73880 = CARTESIAN_POINT ( 'NONE',  ( 21.09922568453595559, 42.04030133659708213, -6.408140936763230044 ) ) ;
#73881 = CARTESIAN_POINT ( 'NONE',  ( 15.44008868035555260, 9.730352010821505360, 9.422509992056143702 ) ) ;
#73882 = CARTESIAN_POINT ( 'NONE',  ( -2.816281873526473856, 39.12363466993041783, 9.499525473075851096E-16 ) ) ;
#73883 = CARTESIAN_POINT ( 'NONE',  ( 13.43411237798105340, 60.58196800326376064, 12.81628187352647963 ) ) ;
#73884 = ORIENTED_EDGE ( 'NONE', *, *, #30154, .F. ) ;
#73885 = CARTESIAN_POINT ( 'NONE',  ( 4.657035931881701174, -8.268334176800257396, -3.999999999999194866 ) ) ;
#73886 = CARTESIAN_POINT ( 'NONE',  ( 14.09394518620610270, 4.258544466044566969E-16, 3.407449058785454898 ) ) ;
#73887 = CARTESIAN_POINT ( 'NONE',  ( 2.917880565312950480, 25.97041550158063572, -12.26659068614894821 ) ) ;
#73888 = CARTESIAN_POINT ( 'NONE',  ( -0.3689425029237881626, 2.428748834913967869, 10.36894250292379027 ) ) ;
#73889 = DIRECTION ( 'NONE',  ( -0.000000000000000000, 1.000000000000000000, -0.000000000000000000 ) ) ;
#73890 = CARTESIAN_POINT ( 'NONE',  ( -0.8801773607110991993, 27.85535201082150181, -2.915334737309923874 ) ) ;
#73891 = DIRECTION ( 'NONE',  ( 0.000000000000000000, -3.035766082959409891E-14, 1.000000000000000000 ) ) ;
#73892 = CARTESIAN_POINT ( 'NONE',  ( 20.15039907845753220, 34.72266099184918176, 6.262539305110077059 ) ) ;
#73893 = CARTESIAN_POINT ( 'NONE',  ( 17.96484262340118221, 56.18868534415484817, -7.964842623401177768 ) ) ;
#73894 = CARTESIAN_POINT ( 'NONE',  ( 4.559911319644449179, 48.89701867748817676, 9.422509992056141925 ) ) ;
#73895 = CARTESIAN_POINT ( 'NONE',  ( 10.00000000000000178, 15.37363466993042138, 12.81628187352647608 ) ) ;
#73896 = CARTESIAN_POINT ( 'NONE',  ( 3.836325488036183451, 15.00000000000000000, -14.50112432709422627 ) ) ;
#73897 = CARTESIAN_POINT ( 'NONE',  ( -2.174473938468922896, 0.000000000000000000, -5.000947681547216916 ) ) ;
#73898 = CARTESIAN_POINT ( 'NONE',  ( 14.92337183194729988, 19.34226448433411960, -8.527530157486177487 ) ) ;
#73899 = CARTESIAN_POINT ( 'NONE',  ( 0.5774900079438590739, 37.64701867748817676, -5.440088680355550821 ) ) ;
#73900 = VECTOR ( 'NONE', #89887, 1000.000000000000000 ) ;
#73901 = CARTESIAN_POINT ( 'NONE',  ( 0.6178305044545838731, 9.748634669930416052, 9.382169495545420901 ) ) ;
#73902 = FACE_OUTER_BOUND ( 'NONE', #66547, .T. ) ;
#73903 = VECTOR ( 'NONE', #61076, 1000.000000000000000 ) ;
#73904 = CARTESIAN_POINT ( 'NONE',  ( 18.52753015748617571, 28.09226448433411960, 4.923371831947298993 ) ) ;
#73905 = CARTESIAN_POINT ( 'NONE',  ( -2.816281873526473856, 44.33196800326375353, 3.434112377981055619 ) ) ;
#73906 = CIRCLE ( 'NONE', #30789, 15.00000000000000000 ) ;
#73907 = CARTESIAN_POINT ( 'NONE',  ( 18.52753015748618282, 3.925597817667451306, -4.923371831947291888 ) ) ;
#73908 = PRESENTATION_LAYER_ASSIGNMENT (  '', '', ( #70717 ) ) ;
#73909 = ORIENTED_EDGE ( 'NONE', *, *, #50981, .F. ) ;
#73910 = CYLINDRICAL_SURFACE ( 'NONE', #588, 0.5000000000000004441 ) ;
#73911 = CARTESIAN_POINT ( 'NONE',  ( 1.472469842513823179, 35.59226448433412315, -4.923371831947296329 ) ) ;
#73912 = CARTESIAN_POINT ( 'NONE',  ( 0.5774900079438590739, 17.64701867748817321, -5.440088680355550821 ) ) ;
#73914 = CARTESIAN_POINT ( 'NONE',  ( 2.917880565312948704, 32.63708216824730357, 12.26659068614894643 ) ) ;
#73913 = SURFACE_STYLE_USAGE ( .BOTH. , #28416 ) ;
#73915 = CARTESIAN_POINT ( 'NONE',  ( 19.84674366389459266, 33.30059781766744464, 2.638427012816836559 ) ) ;
#73916 = CARTESIAN_POINT ( 'NONE',  ( 12.91533473730992121, 14.52201867748817143, 10.88017736071110164 ) ) ;
#73917 = CARTESIAN_POINT ( 'NONE',  ( 17.08211943468705130, 63.47041550158063927, 12.26659068614894998 ) ) ;
#73918 = ORIENTED_EDGE ( 'NONE', *, *, #40647, .T. ) ;
#73919 = PRESENTATION_LAYER_ASSIGNMENT (  '', '', ( #2081 ) ) ;
#73920 = CARTESIAN_POINT ( 'NONE',  ( 4.559911319644449179, 27.23035201082150536, -9.422509992056141925 ) ) ;
#73921 = EDGE_CURVE ( 'NONE', #63872, #35357, #75139, .T. ) ;
#73922 = CARTESIAN_POINT ( 'NONE',  ( 0.5774900079438590739, 37.64701867748817676, -5.440088680355550821 ) ) ;
#73924 = CARTESIAN_POINT ( 'NONE',  ( -0.8801773607111009756, 38.06368534415484106, 1.068504757029289695E-15 ) ) ;
#73923 = CYLINDRICAL_SURFACE ( 'NONE', #64808, 0.5000000000000004441 ) ;
#73925 = VERTEX_POINT ( 'NONE', #74142 ) ;
#73926 = CARTESIAN_POINT ( 'NONE',  ( 0.1532563361054100626, 60.80059781766744464, -2.638427012816831230 ) ) ;
#73927 = CARTESIAN_POINT ( 'NONE',  ( 20.88017736071110875, 40.77201867748818387, -2.915334737309920765 ) ) ;
#73928 = DIRECTION ( 'NONE',  ( -1.000000000000000000, 0.000000000000000000, 0.000000000000000000 ) ) ;
#73929 = CARTESIAN_POINT ( 'NONE',  ( 10.00000000000000178, 60.37363466993041783, 12.81628187352647608 ) ) ;
#73930 = LINE ( 'NONE', #98443, #66752 ) ;
#73931 = CARTESIAN_POINT ( 'NONE',  ( 13.79529636645031943, 35.34541550158063927, -14.16423886937409904 ) ) ;
#73932 = CARTESIAN_POINT ( 'NONE',  ( 2.035157376598822676, 57.43868534415484106, -7.964842623401177768 ) ) ;
#73933 = CARTESIAN_POINT ( 'NONE',  ( 0.1532563361054100626, 65.80059781766745175, -2.638427012816831230 ) ) ;
#73934 = CARTESIAN_POINT ( 'NONE',  ( 0.000000000000000000, 0.5000000000000004441, 0.000000000000000000 ) ) ;
#73935 = CARTESIAN_POINT ( 'NONE',  ( 17.20831665107776587, 49.13393115100078745, -7.208316651077762316 ) ) ;
#73936 = ORIENTED_EDGE ( 'NONE', *, *, #12478, .F. ) ;
#73937 = LINE ( 'NONE', #3982, #90983 ) ;
#73938 = VECTOR ( 'NONE', #33232, 1000.000000000000114 ) ;
#73939 = CARTESIAN_POINT ( 'NONE',  ( 18.52753015748618282, 18.92559781766745175, -4.923371831947291888 ) ) ;
#73940 = CARTESIAN_POINT ( 'NONE',  ( -5.204170427930421283E-15, -12.12636533006957507, -12.81628187352647608 ) ) ;
#73941 = CARTESIAN_POINT ( 'NONE',  ( 12.91533473730993009, 21.60535201082150536, -10.88017736071109987 ) ) ;
#73942 = CARTESIAN_POINT ( 'NONE',  ( 19.84674366389459266, 18.30059781766745175, 2.638427012816836559 ) ) ;
#73943 = CARTESIAN_POINT ( 'NONE',  ( 17.96484262340118221, 59.93868534415484106, 7.964842623401181321 ) ) ;
#73945 = CARTESIAN_POINT ( 'NONE',  ( 10.00000000000000000, 57.87363466993042493, -12.81628187352647608 ) ) ;
#73944 = CARTESIAN_POINT ( 'NONE',  ( 7.084665262690076126, 29.10535201082150181, 10.88017736071109987 ) ) ;
#73946 = CARTESIAN_POINT ( 'NONE',  ( 6.204703633549690345, 45.76208216824729647, -14.16423886937410259 ) ) ;
#73947 = AXIS2_PLACEMENT_3D ( 'NONE', #7949, #77901, #9413 ) ;
#73948 = EDGE_CURVE ( 'NONE', #68711, #81557, #37652, .T. ) ;
#73949 = FACE_OUTER_BOUND ( 'NONE', #34934, .T. ) ;
#73950 = ORIENTED_EDGE ( 'NONE', *, *, #41939, .T. ) ;
#73951 = CARTESIAN_POINT ( 'NONE',  ( 16.40814093676323893, 0.7903013365970867898, 11.09922568453595026 ) ) ;
#73952 = CARTESIAN_POINT ( 'NONE',  ( 7.084665262690076126, 12.02201867748817143, -10.88017736071110164 ) ) ;
#73953 = EDGE_CURVE ( 'NONE', #41669, #18731, #16196, .T. ) ;
#73954 = CARTESIAN_POINT ( 'NONE',  ( -0.8801773607111009756, 48.06368534415484817, 1.068504757029289695E-15 ) ) ;
#73955 = CARTESIAN_POINT ( 'NONE',  ( 7.361572987183170547, 57.05059781766744464, 9.846743663894590881 ) ) ;
#73956 = ORIENTED_EDGE ( 'NONE', *, *, #82899, .T. ) ;
#73957 = CARTESIAN_POINT ( 'NONE',  ( 14.92337183194729633, 17.67559781766745175, 8.527530157486181039 ) ) ;
#73958 = CARTESIAN_POINT ( 'NONE',  ( 0.1532563361054082862, 16.21726448433411960, 2.638427012816831674 ) ) ;
#73959 = CARTESIAN_POINT ( 'NONE',  ( 1.472469842513823179, 35.59226448433412315, -4.923371831947296329 ) ) ;
#73960 = CARTESIAN_POINT ( 'NONE',  ( 5.076628168052703671, 11.84226448433411960, 8.527530157486179263 ) ) ;
#73961 = CARTESIAN_POINT ( 'NONE',  ( 17.20831665107776587, 14.13393115100078568, -7.208316651077762316 ) ) ;
#73962 = CARTESIAN_POINT ( 'NONE',  ( -7.072497013529895682, -84.40007040885102185, 2.750000000000805578 ) ) ;
#73964 = CARTESIAN_POINT ( 'NONE',  ( -1.780824192092605562, 15.00000000000000000, 14.89391369643512064 ) ) ;
#73963 = CARTESIAN_POINT ( 'NONE',  ( 17.96484262340118221, 64.93868534415483396, 7.964842623401181321 ) ) ;
#73965 = CARTESIAN_POINT ( 'NONE',  ( 0.1532563361054083140, 6.008931151000784787, 1.131784320476157264E-15 ) ) ;
#73967 = ORIENTED_EDGE ( 'NONE', *, *, #51700, .T. ) ;
#73966 = CARTESIAN_POINT ( 'NONE',  ( 17.20831665107776587, 22.88393115100078745, 7.208316651077764980 ) ) ;
#73968 = CARTESIAN_POINT ( 'NONE',  ( 13.82671409943296226, 15.00000000000000000, -3.447387012295225261 ) ) ;
#73969 = CARTESIAN_POINT ( 'NONE',  ( 6.565887622018943937, 3.081968003263753531, -12.81628187352647608 ) ) ;
#73970 = VECTOR ( 'NONE', #65392, 1000.000000000000000 ) ;
#73971 = CARTESIAN_POINT ( 'NONE',  ( 0.000000000000000000, 0.000000000000000000, -13.74999999999999467 ) ) ;
#73972 = EDGE_CURVE ( 'NONE', #20878, #40989, #36159, .T. ) ;
#73973 = CARTESIAN_POINT ( 'NONE',  ( 20.36894250292379738, 19.92874883491396787, -10.36894250292379027 ) ) ;
#73974 = CARTESIAN_POINT ( 'NONE',  ( -19.64999999999999858, 92.00000000000000000, 8.000000000000000000 ) ) ;
#73975 = TOROIDAL_SURFACE ( 'NONE', #21321, 14.49999999999999822, 0.5000000000000000000 ) ;
#73976 = CARTESIAN_POINT ( 'NONE',  ( 10.00000000000000000, 15.55374883491396787, -14.16423886937410082 ) ) ;
#73977 = CARTESIAN_POINT ( 'NONE',  ( -2.266590686148945544, 46.38708216824730357, -7.082119434687050408 ) ) ;
#73978 = CARTESIAN_POINT ( 'NONE',  ( 12.00809552683958614, 15.00000000000000000, -8.989195838243546177 ) ) ;
#73980 = CARTESIAN_POINT ( 'NONE',  ( 2.035157376598822676, 67.43868534415484817, -7.964842623401177768 ) ) ;
#73979 = CARTESIAN_POINT ( 'NONE',  ( 6.204703633549690345, 17.84541550158063217, 14.16423886937410082 ) ) ;
#73981 = CARTESIAN_POINT ( 'NONE',  ( 10.00000000000000178, 34.31368534415484106, 10.88017736071110342 ) ) ;
#73982 = DIRECTION ( 'NONE',  ( 0.000000000000000000, -0.000000000000000000, -1.000000000000000000 ) ) ;
#73983 = CARTESIAN_POINT ( 'NONE',  ( 0.1532563361054082862, 31.21726448433412315, 2.638427012816831674 ) ) ;
#73985 = CARTESIAN_POINT ( 'NONE',  ( 19.84674366389459621, 33.50893115100078745, 7.409399052514197653E-17 ) ) ;
#73984 = CARTESIAN_POINT ( 'NONE',  ( 7.084665262690076126, 67.02201867748817676, -10.88017736071110164 ) ) ;
#73986 = CARTESIAN_POINT ( 'NONE',  ( 4.559911319644449179, 8.897018677488173211, 9.422509992056141925 ) ) ;
#73987 = CARTESIAN_POINT ( 'NONE',  ( 19.38216949554541202, 55.99863466993041072, 9.382169495545424454 ) ) ;
#73988 = CARTESIAN_POINT ( 'NONE',  ( 10.00000000000000000, 44.75893115100078745, -9.846743663894594434 ) ) ;
#73989 = CARTESIAN_POINT ( 'NONE',  ( 10.00000000000000000, 37.87363466993041783, -12.81628187352647608 ) ) ;
#73990 = B_SPLINE_CURVE_WITH_KNOTS ( 'NONE', 3,
 ( #49738, #41293, #3277, #9795, #94760, #33741 ),
 .UNSPECIFIED., .F., .F.,
 ( 4, 2, 4 ),
 ( 3.409110551496095454E-05, 0.0004400426677367853790, 0.0008459942299586097492 ),
 .UNSPECIFIED. ) ;
#73991 = CARTESIAN_POINT ( 'NONE',  ( 3.795296366450314540, -26.73791783175269643, 14.16423886937410082 ) ) ;
#73992 = CARTESIAN_POINT ( 'NONE',  ( 7.084665262690076126, 49.10535201082149825, 10.88017736071109987 ) ) ;
#73993 = CARTESIAN_POINT ( 'NONE',  ( 14.92337183194729988, 44.34226448433412315, -8.527530157486177487 ) ) ;
#73994 = CARTESIAN_POINT ( 'NONE',  ( 17.08211943468705130, 28.47041550158063572, 12.26659068614894998 ) ) ;
#73995 = EDGE_LOOP ( 'NONE', ( #17266, #64441, #21441, #58002 ) ) ;
#73996 = CARTESIAN_POINT ( 'NONE',  ( 19.42250999205614193, 50.14701867748817676, 5.440088680355555262 ) ) ;
#73997 = CARTESIAN_POINT ( 'NONE',  ( 10.91036564011094256, 14.76984962000323875, 10.20716212663568889 ) ) ;
#73998 = CARTESIAN_POINT ( 'NONE',  ( 17.08211943468705840, 50.13708216824730357, -12.26659068614894466 ) ) ;
#73999 = CARTESIAN_POINT ( 'NONE',  ( -2.816281873526471635, -1.084698663402913210, -3.434112377981056508 ) ) ;
#74000 = B_SPLINE_CURVE_WITH_KNOTS ( 'NONE', 3,
 ( #35156, #58149, #50670, #18214 ),
 .UNSPECIFIED., .F., .F.,
 ( 4, 4 ),
 ( 0.000000000000000000, 0.001036303429213241475 ),
 .UNSPECIFIED. ) ;
#74001 = CARTESIAN_POINT ( 'NONE',  ( 14.56368227077856758, 14.76930270348881180, 3.337246381125283712 ) ) ;
#74002 = CARTESIAN_POINT ( 'NONE',  ( -0.8801773607110991993, 57.85535201082149825, -2.915334737309923874 ) ) ;
#74003 = CARTESIAN_POINT ( 'NONE',  ( -46.30928139467842897, 104.0823827281712255, 5.529860068218143354 ) ) ;
#74004 = CARTESIAN_POINT ( 'NONE',  ( 6.565887622018943937, 25.16530133659708213, 12.81628187352647430 ) ) ;
#74005 = CARTESIAN_POINT ( 'NONE',  ( 10.00000000000000178, 57.25893115100078745, 9.846743663894594434 ) ) ;
#74006 = CARTESIAN_POINT ( 'NONE',  ( -9.422509992056145478, 32.64701867748817676, -5.440088680355541939 ) ) ;
#74007 = CARTESIAN_POINT ( 'NONE',  ( 17.96484262340118221, 4.938685344154837509, 7.964842623401181321 ) ) ;
#74008 = LINE ( 'NONE', #74502, #15265 ) ;
#74009 = EDGE_LOOP ( 'NONE', ( #55395, #69791, #85755, #83576, #95586, #10966 ) ) ;
#74010 = CARTESIAN_POINT ( 'NONE',  ( -0.8801773607111008646, 3.272018677488171434, 2.915334737309923430 ) ) ;
#74011 = CARTESIAN_POINT ( 'NONE',  ( 20.10421743870887212, 65.60736173766201773, -6.337391062633413341 ) ) ;
#74012 = CARTESIAN_POINT ( 'NONE',  ( 2.035157376598822676, 67.43868534415484817, -7.964842623401177768 ) ) ;
#74013 = CARTESIAN_POINT ( 'NONE',  ( 14.92337183194729988, 4.342264484334117824, -8.527530157486177487 ) ) ;
#74014 = CARTESIAN_POINT ( 'NONE',  ( 19.84674366389459266, 38.71726448433412315, -2.638427012816827677 ) ) ;
#74015 = CARTESIAN_POINT ( 'NONE',  ( 17.96484262340118221, 31.18868534415483751, -7.964842623401177768 ) ) ;
#74016 = CARTESIAN_POINT ( 'NONE',  ( 10.00000000000000000, 2.873634669930420049, -12.81628187352647608 ) ) ;
#74018 = CARTESIAN_POINT ( 'NONE',  ( -3.420591144908350589, 0.5000000000000004441, -14.60477854057960556 ) ) ;
#74017 = CARTESIAN_POINT ( 'NONE',  ( 4.559911319644449179, 37.23035201082150536, -9.422509992056141925 ) ) ;
#74019 = CARTESIAN_POINT ( 'NONE',  ( 17.85158348494336877, 64.73726573380444904, -6.500000000000001776 ) ) ;
#74020 = CARTESIAN_POINT ( 'NONE',  ( 0.6178305044545838731, 39.74863466993041072, 9.382169495545420901 ) ) ;
#74021 = ORIENTED_EDGE ( 'NONE', *, *, #45654, .F. ) ;
#74022 = CARTESIAN_POINT ( 'NONE',  ( 17.96484262340118221, 66.18868534415483396, -7.964842623401177768 ) ) ;
#74023 = CARTESIAN_POINT ( 'NONE',  ( 19.38216949554541557, 32.24863466993041783, -9.382169495545420901 ) ) ;
#74024 = FACE_OUTER_BOUND ( 'NONE', #51186, .T. ) ;
#74025 = CARTESIAN_POINT ( 'NONE',  ( 7.084665262690076126, 37.02201867748817676, -10.88017736071110164 ) ) ;
#74026 = CARTESIAN_POINT ( 'NONE',  ( 17.20831665107776587, 62.88393115100078745, 7.208316651077764980 ) ) ;
#74027 = CARTESIAN_POINT ( 'NONE',  ( -0.3689425029237898834, 66.17874883491396076, -10.36894250292378850 ) ) ;
#74028 = CARTESIAN_POINT ( 'NONE',  ( 18.52753015748617571, 53.09226448433412315, 4.923371831947298993 ) ) ;
#74029 = CARTESIAN_POINT ( 'NONE',  ( 0.1532563361054083140, 16.00893115100078390, 1.131784320476157264E-15 ) ) ;
#74030 = CARTESIAN_POINT ( 'NONE',  ( 20.88017736071110875, 60.77201867748817676, -2.915334737309920765 ) ) ;
#74031 = CARTESIAN_POINT ( 'NONE',  ( 2.746530213673227803E-16, 21.83999999999999986, 0.000000000000000000 ) ) ;
#74032 = CARTESIAN_POINT ( 'NONE',  ( 6.204703633549690345, 25.76208216824730712, -14.16423886937410259 ) ) ;
#74033 = LINE ( 'NONE', #44028, #33041 ) ;
#74034 = EDGE_CURVE ( 'NONE', #60281, #1705, #22153, .T. ) ;
#74035 = CARTESIAN_POINT ( 'NONE',  ( -3.889970118577497082, -8.287734203612162176, -3.750000000000000444 ) ) ;
#74036 = ORIENTED_EDGE ( 'NONE', *, *, #1141, .T. ) ;
#74037 = CARTESIAN_POINT ( 'NONE',  ( 2.917880565312950480, 55.97041550158063217, -12.26659068614894821 ) ) ;
#74038 = CARTESIAN_POINT ( 'NONE',  ( -4.164238869374099927, 67.01208216824728936, 3.795296366450308767 ) ) ;
#74039 = CARTESIAN_POINT ( 'NONE',  ( 19.84674366389459266, 33.30059781766744464, 2.638427012816836559 ) ) ;
#74040 = CARTESIAN_POINT ( 'NONE',  ( 4.431036607602587551, 14.63606876205557050, -14.33059365769914528 ) ) ;
#74041 = DIRECTION ( 'NONE',  ( -0.8320502943378436100, 0.5547001962252291474, -0.000000000000000000 ) ) ;
#74042 = CARTESIAN_POINT ( 'NONE',  ( 17.96484262340118221, 14.93868534415483751, 7.964842623401181321 ) ) ;
#74043 = CARTESIAN_POINT ( 'NONE',  ( 13.79529636645031943, 60.34541550158063927, -14.16423886937409904 ) ) ;
#74044 = CARTESIAN_POINT ( 'NONE',  ( 14.92337183194729633, 27.67559781766745530, 8.527530157486181039 ) ) ;
#74045 = DIRECTION ( 'NONE',  ( 0.000000000000000000, 0.000000000000000000, 1.000000000000000000 ) ) ;
#74046 = CARTESIAN_POINT ( 'NONE',  ( 1.472469842513823179, 15.59226448433411960, -4.923371831947296329 ) ) ;
#74047 = TOROIDAL_SURFACE ( 'NONE', #66056, 2.799999999999999822, 0.2000000000000000111 ) ;
#74048 = CARTESIAN_POINT ( 'NONE',  ( 18.52753015748618282, 3.925597817667451306, -4.923371831947291888 ) ) ;
#74049 = CARTESIAN_POINT ( 'NONE',  ( -8.527530157486182816, 15.59226448433412315, -4.923371831947288335 ) ) ;
#74050 = ORIENTED_EDGE ( 'NONE', *, *, #73538, .T. ) ;
#74051 = VERTEX_POINT ( 'NONE', #13655 ) ;
#74052 = FILL_AREA_STYLE ('',( #58559 ) ) ;
#74053 = ORIENTED_EDGE ( 'NONE', *, *, #74963, .F. ) ;
#74054 = CARTESIAN_POINT ( 'NONE',  ( 14.92337183194729633, 42.67559781766745886, 8.527530157486181039 ) ) ;
#74055 = CARTESIAN_POINT ( 'NONE',  ( -0.3689425029237898834, 21.17874883491396432, -10.36894250292378850 ) ) ;
#74057 = CARTESIAN_POINT ( 'NONE',  ( 4.559911319644449179, 23.89701867748817321, 9.422509992056141925 ) ) ;
#74056 = CARTESIAN_POINT ( 'NONE',  ( 19.42250999205614548, 20.98035201082150891, -5.440088680355545492 ) ) ;
#74059 = CARTESIAN_POINT ( 'NONE',  ( 10.00000000000000000, 17.87363466993041783, -12.81628187352647608 ) ) ;
#74058 = CARTESIAN_POINT ( 'NONE',  ( 12.63842701281683922, 59.55059781766744464, -9.846743663894590881 ) ) ;
#74060 = CARTESIAN_POINT ( 'NONE',  ( -0.3689425029237898834, 11.17874883491396787, -10.36894250292378850 ) ) ;
#74061 = EDGE_CURVE ( 'NONE', #54254, #12471, #6984, .T. ) ;
#74062 = CARTESIAN_POINT ( 'NONE',  ( 6.565887622018943937, 33.08196800326374643, -12.81628187352647608 ) ) ;
#74063 = VERTEX_POINT ( 'NONE', #82644 ) ;
#74064 = CARTESIAN_POINT ( 'NONE',  ( 17.20831665107776587, 27.88393115100078390, 7.208316651077764980 ) ) ;
#74065 = CARTESIAN_POINT ( 'NONE',  ( 20.88017736071110875, 5.772018677488170546, -2.915334737309920765 ) ) ;
#74066 = ORIENTED_EDGE ( 'NONE', *, *, #45729, .F. ) ;
#74067 = CARTESIAN_POINT ( 'NONE',  ( 24.16423886937410614, 64.51208216824728936, -3.795296366450302550 ) ) ;
#74068 = ORIENTED_EDGE ( 'NONE', *, *, #65937, .T. ) ;
#74069 = CARTESIAN_POINT ( 'NONE',  ( 12.91533473730993009, 51.60535201082149825, -10.88017736071109987 ) ) ;
#74070 = CARTESIAN_POINT ( 'NONE',  ( 7.084665262690076126, 59.10535201082150536, 10.88017736071109987 ) ) ;
#74071 = CARTESIAN_POINT ( 'NONE',  ( 12.91533473730992121, 54.52201867748816255, 10.88017736071110164 ) ) ;
#74072 = CARTESIAN_POINT ( 'NONE',  ( -11.39601241150444189, 15.00000000000000000, -11.22534175661882294 ) ) ;
#74073 = CARTESIAN_POINT ( 'NONE',  ( 7.084665262690076126, 44.10535201082151247, 10.88017736071109987 ) ) ;
#74074 = CARTESIAN_POINT ( 'NONE',  ( 1.114591949025029338, 4.390405144365474573E-16, -14.45709807627964416 ) ) ;
#74075 = CARTESIAN_POINT ( 'NONE',  ( 0.000000000000000000, 99.99999999999998579, 8.000000000000000000 ) ) ;
#74076 = CARTESIAN_POINT ( 'NONE',  ( 12.63842701281683922, 34.55059781766745886, -9.846743663894590881 ) ) ;
#74077 = ORIENTED_EDGE ( 'NONE', *, *, #56250, .F. ) ;
#74078 = CARTESIAN_POINT ( 'NONE',  ( 5.076628168052704559, 55.17559781766745175, -8.527530157486179263 ) ) ;
#74079 = CARTESIAN_POINT ( 'NONE',  ( 14.47650479471827722, 14.49999999999999112, -3.928206833722049929 ) ) ;
#74080 = CARTESIAN_POINT ( 'NONE',  ( -2.266590686148945544, 11.38708216824730179, -7.082119434687050408 ) ) ;
#74081 = ORIENTED_EDGE ( 'NONE', *, *, #21978, .T. ) ;
#74082 = EDGE_CURVE ( 'NONE', #27101, #6459, #73721, .T. ) ;
#74083 = CARTESIAN_POINT ( 'NONE',  ( 14.04391541078763161, 4.402316570082688340E-16, 3.608107528142934228 ) ) ;
#74084 = CARTESIAN_POINT ( 'NONE',  ( -4.261098476312686678, -13.83548126352581065, 3.750000000000000888 ) ) ;
#74085 = CARTESIAN_POINT ( 'NONE',  ( 14.26139399674454822, 15.00000000000000000, -2.619664342929791445 ) ) ;
#74086 = CARTESIAN_POINT ( 'NONE',  ( -0.3689425029237881626, 62.42874883491396787, 10.36894250292379027 ) ) ;
#74087 = ORIENTED_EDGE ( 'NONE', *, *, #95280, .T. ) ;
#74088 = DIRECTION ( 'NONE',  ( -0.06975647374412544122, -0.9975640502598241977, 0.000000000000000000 ) ) ;
#74089 = CARTESIAN_POINT ( 'NONE',  ( 0.1532563361054100626, 50.80059781766745175, -2.638427012816831230 ) ) ;
#74090 = FACE_OUTER_BOUND ( 'NONE', #12803, .T. ) ;
#74091 = CARTESIAN_POINT ( 'NONE',  ( -1.099225684535947600, 19.54030133659708568, 6.408140936763237150 ) ) ;
#74093 = EDGE_CURVE ( 'NONE', #33481, #31750, #9605, .T. ) ;
#74092 = CARTESIAN_POINT ( 'NONE',  ( 1.472469842513823179, 15.59226448433411960, -4.923371831947296329 ) ) ;
#74094 = DIRECTION ( 'NONE',  ( 0.000000000000000000, -1.000000000000000000, 0.000000000000000000 ) ) ;
#74095 = CARTESIAN_POINT ( 'NONE',  ( 14.92337183194729988, 14.34226448433411782, -8.527530157486177487 ) ) ;
#74096 = CARTESIAN_POINT ( 'NONE',  ( 21.09922568453594849, 1.206968003263753531, 6.408140936763242479 ) ) ;
#74097 = CARTESIAN_POINT ( 'NONE',  ( 2.603489959281601873, 25.43575266056827289, -6.500000000000015987 ) ) ;
#74098 = VECTOR ( 'NONE', #84445, 1000.000000000000000 ) ;
#74099 = EDGE_LOOP ( 'NONE', ( #98391, #61271, #57315, #20273, #9133, #82444 ) ) ;
#74100 = CARTESIAN_POINT ( 'NONE',  ( 20.88017736071110519, 15.56368534415483751, 2.639326808657452039E-16 ) ) ;
#74101 = CARTESIAN_POINT ( 'NONE',  ( 13.79529636645031943, 5.345415501580634832, -14.16423886937409904 ) ) ;
#74102 = CARTESIAN_POINT ( 'NONE',  ( 17.20831665107776587, 22.88393115100078745, 7.208316651077764980 ) ) ;
#74103 = CARTESIAN_POINT ( 'NONE',  ( 2.035157376598824452, 58.68868534415482685, 7.964842623401179544 ) ) ;
#74105 =( LENGTH_UNIT ( ) NAMED_UNIT ( * ) SI_UNIT ( .MILLI., .METRE. ) );
#74104 = CARTESIAN_POINT ( 'NONE',  ( 16.40814093676323893, 30.79030133659708923, 11.09922568453595026 ) ) ;
#74106 =( NAMED_UNIT ( * ) SI_UNIT ( $, .STERADIAN. ) SOLID_ANGLE_UNIT ( ) );
#74107 = CIRCLE ( 'NONE', #70930, 14.49999999999999822 ) ;
#74108 = DIRECTION ( 'NONE',  ( 0.9961946980917461003, -0.08715574274765176821, 0.000000000000000000 ) ) ;
#74109 = CARTESIAN_POINT ( 'NONE',  ( 0.1532563361054100626, 60.80059781766744464, -2.638427012816831230 ) ) ;
#74110 = CARTESIAN_POINT ( 'NONE',  ( 12.63842701281683034, 12.46726448433411782, 9.846743663894596210 ) ) ;
#74111 = CARTESIAN_POINT ( 'NONE',  ( -10.88017736071109987, -21.72798132251182679, 2.915334737309934532 ) ) ;
#74112 = CARTESIAN_POINT ( 'NONE',  ( -1.099225684535947600, 18.70696800326375353, -6.408140936763238038 ) ) ;
#74113 = CARTESIAN_POINT ( 'NONE',  ( 1.932340009482121035, 51.49127512925449679, -6.499999999999929834 ) ) ;
#74115 = FACE_OUTER_BOUND ( 'NONE', #2986, .T. ) ;
#74114 = CARTESIAN_POINT ( 'NONE',  ( 7.084665262690076126, 39.10535201082150536, 10.88017736071109987 ) ) ;
#74116 = CARTESIAN_POINT ( 'NONE',  ( 0.000000000000000000, -97.00000000000000000, 2.750000000000000000 ) ) ;
#74117 = CARTESIAN_POINT ( 'NONE',  ( -8.124115902427741176, 75.04369783535875627, 2.900000000000000355 ) ) ;
#74118 = CARTESIAN_POINT ( 'NONE',  ( 2.035157376598822676, 32.43868534415483396, -7.964842623401177768 ) ) ;
#74119 = CARTESIAN_POINT ( 'NONE',  ( 17.96484262340118221, 31.18868534415483751, -7.964842623401177768 ) ) ;
#74120 = CARTESIAN_POINT ( 'NONE',  ( 5.076628168052704559, 50.17559781766745886, -8.527530157486179263 ) ) ;
#74121 = CARTESIAN_POINT ( 'NONE',  ( -0.8801773607111009756, 58.06368534415484106, 1.068504757029289695E-15 ) ) ;
#74122 = CARTESIAN_POINT ( 'NONE',  ( -0.3689425029237881626, 37.42874883491396787, 10.36894250292379027 ) ) ;
#74123 = CARTESIAN_POINT ( 'NONE',  ( -10.14667048435152097, 15.00000000000000000, 10.35833375027034542 ) ) ;
#74124 = CARTESIAN_POINT ( 'NONE',  ( 7.361572987183170547, 32.05059781766745175, 9.846743663894590881 ) ) ;
#74125 = CARTESIAN_POINT ( 'NONE',  ( 6.565887622018943937, -1.918031996736246692, -12.81628187352647608 ) ) ;
#74126 = ORIENTED_EDGE ( 'NONE', *, *, #49280, .T. ) ;
#74127 = CARTESIAN_POINT ( 'NONE',  ( 19.42250999205614193, 20.14701867748817321, 5.440088680355555262 ) ) ;
#74128 = CARTESIAN_POINT ( 'NONE',  ( 20.24186590665277663, 6.760286857231743163, 6.114288769123037426 ) ) ;
#74129 = CARTESIAN_POINT ( 'NONE',  ( -0.8801773607110991993, 2.855352010821504471, -2.915334737309923874 ) ) ;
#74130 = CARTESIAN_POINT ( 'NONE',  ( -0.8801773607111008646, 18.27201867748817321, 2.915334737309923430 ) ) ;
#74131 = CARTESIAN_POINT ( 'NONE',  ( 7.361572987183169658, 4.967264484334119601, -9.846743663894592657 ) ) ;
#74132 = CARTESIAN_POINT ( 'NONE',  ( 20.36894250292379738, 19.92874883491396787, -10.36894250292379027 ) ) ;
#74133 = MANIFOLD_SOLID_BREP ( 'Fillet3', #76155 ) ;
#74134 = CARTESIAN_POINT ( 'NONE',  ( 2.791683348922237240, 20.38393115100078745, -7.208316651077763204 ) ) ;
#74135 = CARTESIAN_POINT ( 'NONE',  ( 18.52753015748617571, 63.09226448433412315, 4.923371831947298993 ) ) ;
#74136 = CARTESIAN_POINT ( 'NONE',  ( 20.88017736071110519, 30.56368534415484106, 2.639326808657452039E-16 ) ) ;
#74137 = DIRECTION ( 'NONE',  ( -0.000000000000000000, 1.000000000000000000, 0.000000000000000000 ) ) ;
#74138 = CARTESIAN_POINT ( 'NONE',  ( -45.65232842522237178, 104.2922929041766338, -5.788770647549307924 ) ) ;
#74139 = AXIS2_PLACEMENT_3D ( 'NONE', #32223, #62724, #62232 ) ;
#74140 = ADVANCED_FACE ( 'NONE', ( #24625 ), #29175, .T. ) ;
#74141 = ORIENTED_EDGE ( 'NONE', *, *, #41586, .T. ) ;
#74142 = CARTESIAN_POINT ( 'NONE',  ( -0.1503990784575263973, 27.22266099184919241, -6.262539305110081500 ) ) ;
#74143 = CARTESIAN_POINT ( 'NONE',  ( 14.92337183194729633, 42.67559781766745886, 8.527530157486181039 ) ) ;
#74144 = EDGE_LOOP ( 'NONE', ( #43834, #92056, #91061, #28217, #22796, #16084 ) ) ;
#74145 = ORIENTED_EDGE ( 'NONE', *, *, #30930, .F. ) ;
#74146 = LINE ( 'NONE', #36164, #19798 ) ;
#74147 = CARTESIAN_POINT ( 'NONE',  ( 20.36894250292379382, 23.67874883491397142, 10.36894250292379205 ) ) ;
#74148 = CARTESIAN_POINT ( 'NONE',  ( 2.917880565312950480, 10.97041550158063572, -12.26659068614894821 ) ) ;
#74149 = CARTESIAN_POINT ( 'NONE',  ( 15.44008868035555260, 59.73035201082151247, 9.422509992056143702 ) ) ;
#74150 = CARTESIAN_POINT ( 'NONE',  ( -2.266590686148945544, 56.38708216824731068, -7.082119434687050408 ) ) ;
#74151 = CARTESIAN_POINT ( 'NONE',  ( 22.81628187352647785, 1.415301336597087012, 3.434112377981063169 ) ) ;
#74152 = CARTESIAN_POINT ( 'NONE',  ( 12.63842701281683034, 47.46726448433412315, 9.846743663894596210 ) ) ;
#74153 = CARTESIAN_POINT ( 'NONE',  ( -16.60833333333333073, 99.74999999999998579, 8.000000000000000000 ) ) ;
#74155 = CARTESIAN_POINT ( 'NONE',  ( 13.43411237798105340, 5.581968003263753531, 12.81628187352647963 ) ) ;
#74154 = CARTESIAN_POINT ( 'NONE',  ( 12.91533473730992121, 44.52201867748816966, 10.88017736071110164 ) ) ;
#74156 = CARTESIAN_POINT ( 'NONE',  ( 2.917880565312948704, 22.63708216824730002, 12.26659068614894643 ) ) ;
#74157 = CARTESIAN_POINT ( 'NONE',  ( 0.5774900079438607392, 13.48035201082150358, 5.440088680355550821 ) ) ;
#74158 = DIRECTION ( 'NONE',  ( 0.4305110968082926370, 0.000000000000000000, 0.9025852843498617384 ) ) ;
#74159 = FILL_AREA_STYLE_COLOUR ( '', #14050 ) ;
#74160 = CARTESIAN_POINT ( 'NONE',  ( 2.035157376598822676, 47.43868534415484817, -7.964842623401177768 ) ) ;
#74161 = CARTESIAN_POINT ( 'NONE',  ( -7.208316651077764980, -39.61606884899921255, -7.208316651077759651 ) ) ;
#74162 = VERTEX_POINT ( 'NONE', #8139 ) ;
#74163 = DIRECTION ( 'NONE',  ( 0.000000000000000000, -1.000000000000000000, 0.000000000000000000 ) ) ;
#74164 = ORIENTED_EDGE ( 'NONE', *, *, #21699, .T. ) ;
#74165 = ORIENTED_EDGE ( 'NONE', *, *, #90075, .T. ) ;
#74166 = CARTESIAN_POINT ( 'NONE',  ( 2.917880565312950480, 45.97041550158063927, -12.26659068614894821 ) ) ;
#74167 = CARTESIAN_POINT ( 'NONE',  ( 7.361572987183169658, 44.96726448433412315, -9.846743663894592657 ) ) ;
#74168 = CARTESIAN_POINT ( 'NONE',  ( 7.084665262690076126, 64.10535201082150536, 10.88017736071109987 ) ) ;
#74169 = CARTESIAN_POINT ( 'NONE',  ( -15.00000000000000000, 83.99999999999998579, 3.750000000000000000 ) ) ;
#74170 = CARTESIAN_POINT ( 'NONE',  ( 19.42250999205614548, 55.98035201082150536, -5.440088680355545492 ) ) ;
#74171 = EDGE_CURVE ( 'NONE', #25854, #13186, #62498, .T. ) ;
#74172 = MECHANICAL_DESIGN_GEOMETRIC_PRESENTATION_REPRESENTATION (  '', ( #5542 ), #45493 ) ;
#74173 = CIRCLE ( 'NONE', #39087, 14.49999999999999822 ) ;
#74174 = CARTESIAN_POINT ( 'NONE',  ( 12.81628187352647608, 11.41530133659708568, 3.434112377981052511 ) ) ;
#74175 = ORIENTED_EDGE ( 'NONE', *, *, #20672, .T. ) ;
#74176 =( BOUNDED_CURVE ( )  B_SPLINE_CURVE ( 3, ( #44441, #98964, #52926, #74943 ),
 .UNSPECIFIED., .F., .T. ) 
 B_SPLINE_CURVE_WITH_KNOTS ( ( 4, 4 ),
 ( 0.000000000000000000, 1.570796326794896558 ),
 .UNSPECIFIED. ) 
 CURVE ( )  GEOMETRIC_REPRESENTATION_ITEM ( )  RATIONAL_B_SPLINE_CURVE ( ( 1.000000000000000000, 0.8047378541243649375, 0.8047378541243649375, 1.000000000000000000 ) ) 
 REPRESENTATION_ITEM ( '' )  );
#74177 = CARTESIAN_POINT ( 'NONE',  ( 22.26659068614894466, 23.88708216824730357, 7.082119434687054849 ) ) ;
#74178 = ADVANCED_FACE ( 'NONE', ( #91129 ), #23149, .F. ) ;
#74179 = TOROIDAL_SURFACE ( 'NONE', #5552, 0.5000000000000000000, 0.2500000000000000000 ) ;
#74180 = CARTESIAN_POINT ( 'NONE',  ( -1.099225684535947600, 23.70696800326375708, -6.408140936763238038 ) ) ;
#74181 = ORIENTED_EDGE ( 'NONE', *, *, #73190, .F. ) ;
#74182 = CARTESIAN_POINT ( 'NONE',  ( 21.09922568453595559, 47.04030133659708923, -6.408140936763230044 ) ) ;
#74183 = CARTESIAN_POINT ( 'NONE',  ( 18.52753015748618282, 33.92559781766745886, -4.923371831947291888 ) ) ;
#74184 = CARTESIAN_POINT ( 'NONE',  ( 19.42250999205614193, 10.14701867748816966, 5.440088680355555262 ) ) ;
#74185 = CARTESIAN_POINT ( 'NONE',  ( 19.38216949554541557, 52.24863466993041072, -9.382169495545420901 ) ) ;
#74186 = CARTESIAN_POINT ( 'NONE',  ( -45.94000000000001194, 103.7452903794826682, 5.529860068218143354 ) ) ;
#74187 = CARTESIAN_POINT ( 'NONE',  ( 12.63842701281683034, 47.46726448433412315, 9.846743663894596210 ) ) ;
#74189 = ORIENTED_EDGE ( 'NONE', *, *, #22531, .T. ) ;
#74188 = DIRECTION ( 'NONE',  ( 0.000000000000000000, 1.000000000000000000, 0.000000000000000000 ) ) ;
#74190 =( GEOMETRIC_REPRESENTATION_CONTEXT ( 3 ) GLOBAL_UNCERTAINTY_ASSIGNED_CONTEXT ( ( #13140 ) ) GLOBAL_UNIT_ASSIGNED_CONTEXT ( ( #47808, #2836, #34263 ) ) REPRESENTATION_CONTEXT ( 'NONE', 'WORKASPACE' ) );
#74191 = CARTESIAN_POINT ( 'NONE',  ( -6.767445849361333643, 0.5000000000000004441, 13.38662304974491946 ) ) ;
#74192 = CARTESIAN_POINT ( 'NONE',  ( 0.5600000000000083800, 105.0000000000000000, 4.500000000000000888 ) ) ;
#74193 = CARTESIAN_POINT ( 'NONE',  ( -6.000000000000000000, 78.07179676972447169, 6.250000000000000000 ) ) ;
#74194 = DIRECTION ( 'NONE',  ( -0.000000000000000000, -1.000000000000000000, -0.000000000000000000 ) ) ;
#74195 = CARTESIAN_POINT ( 'NONE',  ( 12.63842701281683922, 19.55059781766745175, -9.846743663894590881 ) ) ;
#74196 = CARTESIAN_POINT ( 'NONE',  ( -2.816281873526473856, 29.33196800326376064, 3.434112377981055619 ) ) ;
#74197 = DIRECTION ( 'NONE',  ( 0.000000000000000000, 0.000000000000000000, 1.000000000000000000 ) ) ;
#74198 = VERTEX_POINT ( 'NONE', #84141 ) ;
#74199 = CARTESIAN_POINT ( 'NONE',  ( 2.791683348922240793, 61.63393115100079456, 7.208316651077764092 ) ) ;
#74200 = DIRECTION ( 'NONE',  ( 1.257568779154408793E-17, 1.000000000000000000, -0.000000000000000000 ) ) ;
#74201 = CARTESIAN_POINT ( 'NONE',  ( -2.266590686148945544, 16.38708216824730357, -7.082119434687050408 ) ) ;
#74202 = CARTESIAN_POINT ( 'NONE',  ( 12.63842701281683034, 47.46726448433412315, 9.846743663894596210 ) ) ;
#74203 = CARTESIAN_POINT ( 'NONE',  ( -2.816281873526471635, 43.91530133659708923, -3.434112377981056508 ) ) ;
#74204 = B_SPLINE_CURVE_WITH_KNOTS ( 'NONE', 3,
 ( #55326, #39356, #47817, #46354, #69850, #92343 ),
 .UNSPECIFIED., .F., .F.,
 ( 4, 2, 4 ),
 ( 3.409110551494476605E-05, 0.0004400426677367897700, 0.0008459942299586347943 ),
 .UNSPECIFIED. ) ;
#74206 = DIRECTION ( 'NONE',  ( 0.000000000000000000, 1.000000000000000000, 0.000000000000000000 ) ) ;
#74205 = CARTESIAN_POINT ( 'NONE',  ( 21.92686044187656691, 37.18830936912750929, 4.562052436263911564E-16 ) ) ;
#74207 = CARTESIAN_POINT ( 'NONE',  ( 19.42250999205614193, 65.14701867748817676, 5.440088680355555262 ) ) ;
#74208 = DIRECTION ( 'NONE',  ( 0.000000000000000000, -0.000000000000000000, -1.000000000000000000 ) ) ;
#74209 = TOROIDAL_SURFACE ( 'NONE', #43886, 10.65000000000026326, 0.2500000000000000000 ) ;
#74210 = CARTESIAN_POINT ( 'NONE',  ( 14.92337183194729988, 29.34226448433411960, -8.527530157486177487 ) ) ;
#74212 = EDGE_CURVE ( 'NONE', #59079, #42731, #10510, .T. ) ;
#74211 = CARTESIAN_POINT ( 'NONE',  ( 12.91533473730993009, 36.60535201082151247, -10.88017736071109987 ) ) ;
#74213 = CARTESIAN_POINT ( 'NONE',  ( 19.84674366389459621, 33.50893115100078745, 7.409399052514197653E-17 ) ) ;
#74214 = DIRECTION ( 'NONE',  ( 0.000000000000000000, 0.000000000000000000, -1.000000000000000000 ) ) ;
#74215 = CARTESIAN_POINT ( 'NONE',  ( 7.084665262690076126, 49.10535201082149825, 10.88017736071109987 ) ) ;
#74216 = ORIENTED_EDGE ( 'NONE', *, *, #73737, .F. ) ;
#74217 = CARTESIAN_POINT ( 'NONE',  ( -2.815433093577211832, 14.49999999999999112, 14.73340885523754551 ) ) ;
#74218 = CARTESIAN_POINT ( 'NONE',  ( 10.00000000000000000, 16.81368534415483751, -10.88017736071110342 ) ) ;
#74220 = CARTESIAN_POINT ( 'NONE',  ( 12.91533473730993009, 41.60535201082149825, -10.88017736071109987 ) ) ;
#74219 = CARTESIAN_POINT ( 'NONE',  ( 7.361572987183170547, 57.05059781766744464, 9.846743663894590881 ) ) ;
#74221 = LINE ( 'NONE', #53703, #53596 ) ;
#74222 = CARTESIAN_POINT ( 'NONE',  ( 15.44008868035555793, 61.39701867748817676, -9.422509992056140149 ) ) ;
#74224 = DIRECTION ( 'NONE',  ( 1.000000000000000000, -0.000000000000000000, 0.000000000000000000 ) ) ;
#74223 = CARTESIAN_POINT ( 'NONE',  ( -0.8801773607111009756, 33.06368534415484106, 1.068504757029289695E-15 ) ) ;
#74225 = CARTESIAN_POINT ( 'NONE',  ( 14.92337183194729988, 19.34226448433411960, -8.527530157486177487 ) ) ;
#74226 = CARTESIAN_POINT ( 'NONE',  ( -0.6999999999999957367, 99.99999999999998579, 8.000000000000000000 ) ) ;
#74227 = CARTESIAN_POINT ( 'NONE',  ( 7.082119434687047743, 10.13708216824730357, -12.26659068614894821 ) ) ;
#74228 = CARTESIAN_POINT ( 'NONE',  ( 10.00000000000000178, 47.25893115100078745, 9.846743663894594434 ) ) ;
#74229 = B_SPLINE_CURVE_WITH_KNOTS ( 'NONE', 3,
 ( #65896, #90868, #29869, #83380, #36401, #88907 ),
 .UNSPECIFIED., .F., .F.,
 ( 4, 2, 4 ),
 ( 0.0002800001862105966138, 0.0006862054174524880035, 0.001092410648694379285 ),
 .UNSPECIFIED. ) ;
#74230 = CARTESIAN_POINT ( 'NONE',  ( -2.266590686148945544, 67.22041550158063217, 7.082119434687048631 ) ) ;
#74231 = CARTESIAN_POINT ( 'NONE',  ( 20.15039907845753930, 70.00000000000000000, 6.262539305110068177 ) ) ;
#74232 = CARTESIAN_POINT ( 'NONE',  ( 24.16423886937410614, 9.303748834913967869, 8.672049930838204340E-16 ) ) ;
#74233 = CARTESIAN_POINT ( 'NONE',  ( 17.08211943468705130, 43.47041550158063927, 12.26659068614894998 ) ) ;
#74234 = B_SPLINE_CURVE_WITH_KNOTS ( 'NONE', 3,
 ( #32917, #70943, #48904, #1959 ),
 .UNSPECIFIED., .F., .F.,
 ( 4, 4 ),
 ( 5.974731160962075775E-17, 0.002562518741975290844 ),
 .UNSPECIFIED. ) ;
#74235 = CARTESIAN_POINT ( 'NONE',  ( 22.81628187352648496, 6.831968003263753531, -3.434112377981050290 ) ) ;
#74236 = VERTEX_POINT ( 'NONE', #76619 ) ;
#74237 = CARTESIAN_POINT ( 'NONE',  ( 2.035157376598824452, 13.68868534415483751, 7.964842623401179544 ) ) ;
#74238 = B_SPLINE_CURVE_WITH_KNOTS ( 'NONE', 3,
 ( #36890, #67378, #52864, #97907, #59869, #90857 ),
 .UNSPECIFIED., .F., .F.,
 ( 4, 2, 4 ),
 ( 4.906538933386797396E-18, 0.0002605067024380966511, 0.0005210134048761883149 ),
 .UNSPECIFIED. ) ;
#74239 = CARTESIAN_POINT ( 'NONE',  ( 17.20831665107776587, 42.88393115100077324, 7.208316651077764980 ) ) ;
#74241 = CARTESIAN_POINT ( 'NONE',  ( -10.93781366033354274, 14.49999999999999822, 10.26470809774057891 ) ) ;
#74240 = DIRECTION ( 'NONE',  ( -1.000000000000000000, 0.000000000000000000, 0.000000000000000000 ) ) ;
#74242 = AXIS2_PLACEMENT_3D ( 'NONE', #63267, #55283, #70801 ) ;
#74243 = ADVANCED_FACE ( 'NONE', ( #661 ), #2630, .F. ) ;
#74244 = CARTESIAN_POINT ( 'NONE',  ( 2.815433093577023538, 0.3640475087720981828, 14.73340885523752419 ) ) ;
#74245 = CARTESIAN_POINT ( 'NONE',  ( 19.38216949554541202, 20.99863466993042138, 9.382169495545424454 ) ) ;
#74246 = CARTESIAN_POINT ( 'NONE',  ( 0.1532563361054100626, 25.80059781766744820, -2.638427012816831230 ) ) ;
#74247 = ORIENTED_EDGE ( 'NONE', *, *, #7382, .T. ) ;
#74248 = CARTESIAN_POINT ( 'NONE',  ( 7.361572987183170547, 7.050597817667451750, 9.846743663894590881 ) ) ;
#74249 = DIRECTION ( 'NONE',  ( 1.000000000000000000, 2.107602052970794797E-16, -0.000000000000000000 ) ) ;
#74250 = FACE_OUTER_BOUND ( 'NONE', #7174, .T. ) ;
#74251 = CARTESIAN_POINT ( 'NONE',  ( 20.88017736071110519, 15.56368534415483751, 2.639326808657452039E-16 ) ) ;
#74252 = CARTESIAN_POINT ( 'NONE',  ( 10.00000000000000000, 40.55374883491397497, -14.16423886937410082 ) ) ;
#74253 = CARTESIAN_POINT ( 'NONE',  ( 7.084665262690076126, 39.10535201082150536, 10.88017736071109987 ) ) ;
#74254 = CARTESIAN_POINT ( 'NONE',  ( 7.084665262690076126, 59.10535201082150536, 10.88017736071109987 ) ) ;
#74255 = SURFACE_STYLE_USAGE ( .BOTH. , #20787 ) ;
#74256 = CARTESIAN_POINT ( 'NONE',  ( 19.84674366389459266, 18.71726448433411960, -2.638427012816827677 ) ) ;
#74257 = DIRECTION ( 'NONE',  ( -1.000000000000000000, 0.000000000000000000, 0.000000000000000000 ) ) ;
#74258 = CARTESIAN_POINT ( 'NONE',  ( 14.92337183194729633, 7.675597817667451750, 8.527530157486181039 ) ) ;
#74259 = CARTESIAN_POINT ( 'NONE',  ( -1.511515493404499644, 5.397528278722328023E-15, 1.315623007559852509 ) ) ;
#74260 = CARTESIAN_POINT ( 'NONE',  ( 19.84674366389459266, 38.30059781766745175, 2.638427012816836559 ) ) ;
#74261 = CARTESIAN_POINT ( 'NONE',  ( 0.1532563361054100626, 65.80059781766745175, -2.638427012816831230 ) ) ;
#74262 = CARTESIAN_POINT ( 'NONE',  ( 15.44008868035555260, 34.73035201082151247, 9.422509992056143702 ) ) ;
#74263 = EDGE_CURVE ( 'NONE', #69763, #86107, #91271, .T. ) ;
#74264 = UNCERTAINTY_MEASURE_WITH_UNIT (LENGTH_MEASURE( 1.000000000000000082E-05 ), #4608, 'distance_accuracy_value', 'NONE');
#74265 = VERTEX_POINT ( 'NONE', #4083 ) ;
#74266 = CARTESIAN_POINT ( 'NONE',  ( 6.565887622018943937, 63.08196800326376064, -12.81628187352647608 ) ) ;
#74267 = CIRCLE ( 'NONE', #72695, 14.49999999999999822 ) ;
#74268 = CARTESIAN_POINT ( 'NONE',  ( -1.099225684535947600, 43.70696800326375353, -6.408140936763238038 ) ) ;
#74270 = CARTESIAN_POINT ( 'NONE',  ( 1.472469842513823179, 35.59226448433412315, -4.923371831947296329 ) ) ;
#74269 = CARTESIAN_POINT ( 'NONE',  ( 2.917880565312948704, 57.63708216824731068, 12.26659068614894643 ) ) ;
#74271 = EDGE_CURVE ( 'NONE', #29532, #37612, #88054, .T. ) ;
#74272 = CARTESIAN_POINT ( 'NONE',  ( 10.00000000000000178, 2.258931151000784787, 9.846743663894594434 ) ) ;
#74273 = CARTESIAN_POINT ( 'NONE',  ( -4.164238869374098151, 21.59541550158063217, -3.795296366450310543 ) ) ;
#74274 = CARTESIAN_POINT ( 'NONE',  ( 6.204703633549690345, 45.76208216824729647, -14.16423886937410259 ) ) ;
#74275 = CARTESIAN_POINT ( 'NONE',  ( 18.52753015748618282, 43.92559781766745175, -4.923371831947291888 ) ) ;
#74276 = FILL_AREA_STYLE_COLOUR ( '', #15569 ) ;
#74277 = CARTESIAN_POINT ( 'NONE',  ( -0.8801773607110991993, 42.85535201082150536, -2.915334737309923874 ) ) ;
#74278 = CARTESIAN_POINT ( 'NONE',  ( 7.084665262690076126, 62.02201867748816966, -10.88017736071110164 ) ) ;
#74279 = CARTESIAN_POINT ( 'NONE',  ( 4.219999999999999751, 10.00000000000000000, -3.750000000000000000 ) ) ;
#74280 = ORIENTED_EDGE ( 'NONE', *, *, #26636, .T. ) ;
#74281 = CARTESIAN_POINT ( 'NONE',  ( 13.43411237798105340, 60.58196800326376064, 12.81628187352647963 ) ) ;
#74282 = ORIENTED_EDGE ( 'NONE', *, *, #43035, .T. ) ;
#74283 = CARTESIAN_POINT ( 'NONE',  ( 5.076628168052703671, 1.842264484334118047, 8.527530157486179263 ) ) ;
#74284 = ORIENTED_EDGE ( 'NONE', *, *, #34089, .F. ) ;
#74285 = AXIS2_PLACEMENT_3D ( 'NONE', #20376, #88870, #96889 ) ;
#74286 = CARTESIAN_POINT ( 'NONE',  ( -4.164238869374098151, 6.595415501580634832, -3.795296366450310543 ) ) ;
#74287 = CARTESIAN_POINT ( 'NONE',  ( 19.84674366389459266, 13.71726448433411782, -2.638427012816827677 ) ) ;
#74288 = CARTESIAN_POINT ( 'NONE',  ( -43.26219512195119421, 34.60975609756091842, -8.000000000000000000 ) ) ;
#74289 = ORIENTED_EDGE ( 'NONE', *, *, #24390, .T. ) ;
#74290 = CARTESIAN_POINT ( 'NONE',  ( 10.00000000000000178, 19.31368534415484106, 10.88017736071110342 ) ) ;
#74291 = CARTESIAN_POINT ( 'NONE',  ( 0.1532563361054082862, 1.217264484334118047, 2.638427012816831674 ) ) ;
#74292 = EDGE_CURVE ( 'NONE', #14873, #717, #59510, .T. ) ;
#74293 = AXIS2_PLACEMENT_3D ( 'NONE', #80663, #96165, #50655 ) ;
#74294 = ORIENTED_EDGE ( 'NONE', *, *, #63879, .T. ) ;
#74295 = CARTESIAN_POINT ( 'NONE',  ( 4.559911319644449179, 18.89701867748817321, 9.422509992056141925 ) ) ;
#74296 = CARTESIAN_POINT ( 'NONE',  ( 19.84674366389459266, 58.30059781766745886, 2.638427012816836559 ) ) ;
#74297 = VERTEX_POINT ( 'NONE', #79585 ) ;
#74298 = ADVANCED_FACE ( 'NONE', ( #50062 ), #72272, .F. ) ;
#74299 = CARTESIAN_POINT ( 'NONE',  ( 5.076628168052704559, 55.17559781766745175, -8.527530157486179263 ) ) ;
#74300 = ORIENTED_EDGE ( 'NONE', *, *, #85356, .F. ) ;
#74301 = MECHANICAL_DESIGN_GEOMETRIC_PRESENTATION_REPRESENTATION (  '', ( #27985 ), #39217 ) ;
#74302 = CARTESIAN_POINT ( 'NONE',  ( -0.8801773607111008646, 68.27201867748817676, 2.915334737309923430 ) ) ;
#74303 = CARTESIAN_POINT ( 'NONE',  ( 19.84674366389459266, 63.30059781766745886, 2.638427012816836559 ) ) ;
#74304 = CARTESIAN_POINT ( 'NONE',  ( 0.6178305044545838731, 39.74863466993041072, 9.382169495545420901 ) ) ;
#74306 = PRESENTATION_STYLE_ASSIGNMENT (( #68804 ) ) ;
#74305 =( NAMED_UNIT ( * ) SI_UNIT ( $, .STERADIAN. ) SOLID_ANGLE_UNIT ( ) );
#74307 = CARTESIAN_POINT ( 'NONE',  ( 7.084665262690076126, 69.10535201082151957, 10.88017736071109987 ) ) ;
#74308 = CARTESIAN_POINT ( 'NONE',  ( 17.96484262340118221, 24.93868534415484461, 7.964842623401181321 ) ) ;
#74309 = TOROIDAL_SURFACE ( 'NONE', #21664, 2.899999999999999467, 0.1000000000000000056 ) ;
#74310 = ORIENTED_EDGE ( 'NONE', *, *, #69675, .T. ) ;
#74311 = CARTESIAN_POINT ( 'NONE',  ( 13.43411237798106583, 52.66530133659708213, -12.81628187352647252 ) ) ;
#74312 = CARTESIAN_POINT ( 'NONE',  ( 19.42250999205614193, 40.14701867748817676, 5.440088680355555262 ) ) ;
#74313 = CARTESIAN_POINT ( 'NONE',  ( -8.157990163924880633, 0.2306972965111904472, 12.51739793958107860 ) ) ;
#74314 = VECTOR ( 'NONE', #61963, 1000.000000000000000 ) ;
#74315 = CARTESIAN_POINT ( 'NONE',  ( 6.565887622018943937, 43.08196800326374643, -12.81628187352647608 ) ) ;
#74316 = CARTESIAN_POINT ( 'NONE',  ( 0.5774900079438590739, 47.64701867748817676, -5.440088680355550821 ) ) ;
#74317 = CARTESIAN_POINT ( 'NONE',  ( 2.791683348922237240, 55.38393115100078745, -7.208316651077763204 ) ) ;
#74318 = DIRECTION ( 'NONE',  ( -0.000000000000000000, -0.000000000000000000, -1.000000000000000000 ) ) ;
#74319 = CARTESIAN_POINT ( 'NONE',  ( 0.1532563361054083140, 21.00893115100078745, 1.131784320476157264E-15 ) ) ;
#74320 = EDGE_CURVE ( 'NONE', #19684, #80817, #85068, .T. ) ;
#74321 = CARTESIAN_POINT ( 'NONE',  ( 22.81628187352647785, 1.623634669930420271, 6.195893100308588602E-16 ) ) ;
#74323 = CARTESIAN_POINT ( 'NONE',  ( 18.52753015748617571, 58.09226448433411605, 4.923371831947298993 ) ) ;
#74322 = DIRECTION ( 'NONE',  ( 0.000000000000000000, 0.000000000000000000, -1.000000000000000000 ) ) ;
#74324 = CARTESIAN_POINT ( 'NONE',  ( 7.084665262690076126, 19.10535201082150181, 10.88017736071109987 ) ) ;
#74325 = CARTESIAN_POINT ( 'NONE',  ( 18.52753015748617571, 53.09226448433412315, 4.923371831947298993 ) ) ;
#74326 = FILL_AREA_STYLE ('',( #59328 ) ) ;
#74327 = CARTESIAN_POINT ( 'NONE',  ( 18.52753015748618282, 13.92559781766745175, -4.923371831947291888 ) ) ;
#74328 = EDGE_CURVE ( 'NONE', #22776, #54527, #97864, .T. ) ;
#74330 = ORIENTED_EDGE ( 'NONE', *, *, #29234, .F. ) ;
#74329 = CARTESIAN_POINT ( 'NONE',  ( 19.38216949554541557, 7.248634669930421381, -9.382169495545420901 ) ) ;
#74331 = FACE_OUTER_BOUND ( 'NONE', #72181, .T. ) ;
#74332 = CARTESIAN_POINT ( 'NONE',  ( 0.6178305044545818747, 38.49863466993042493, -9.382169495545419124 ) ) ;
#74333 = VECTOR ( 'NONE', #90222, 1000.000000000000000 ) ;
#74334 = CARTESIAN_POINT ( 'NONE',  ( 17.20831665107776587, 32.88393115100078745, 7.208316651077764980 ) ) ;
#74335 = DIRECTION ( 'NONE',  ( 0.9762960071199331402, 0.000000000000000000, 0.2164396139381037087 ) ) ;
#74336 = CARTESIAN_POINT ( 'NONE',  ( 7.084665262690076126, 12.02201867748817321, -10.88017736071110164 ) ) ;
#74337 = CARTESIAN_POINT ( 'NONE',  ( 5.076628168052703671, 26.84226448433411960, 8.527530157486179263 ) ) ;
#74338 = DIRECTION ( 'NONE',  ( 0.000000000000000000, 1.000000000000000000, 0.000000000000000000 ) ) ;
#74339 = CARTESIAN_POINT ( 'NONE',  ( 24.16423886937409904, 64.09541550158064638, 3.795296366450317205 ) ) ;
#74340 = CARTESIAN_POINT ( 'NONE',  ( -42.94000000000001194, 92.00000000000000000, 9.000000000000000000 ) ) ;
#74341 = CARTESIAN_POINT ( 'NONE',  ( 19.42250999205614193, 25.14701867748817321, 5.440088680355555262 ) ) ;
#74342 = CARTESIAN_POINT ( 'NONE',  ( 20.36894250292379738, 49.92874883491396787, -10.36894250292379027 ) ) ;
#74343 = CARTESIAN_POINT ( 'NONE',  ( 20.36894250292379738, 49.92874883491396787, -10.36894250292379027 ) ) ;
#74344 = DIRECTION ( 'NONE',  ( 0.000000000000000000, 1.000000000000000000, 0.000000000000000000 ) ) ;
#74345 = CARTESIAN_POINT ( 'NONE',  ( 14.92337183194729633, 12.67559781766745353, 8.527530157486181039 ) ) ;
#74346 = CARTESIAN_POINT ( 'NONE',  ( 5.076628168052703671, 66.84226448433412315, 8.527530157486179263 ) ) ;
#74347 = ORIENTED_EDGE ( 'NONE', *, *, #34165, .T. ) ;
#74348 = CARTESIAN_POINT ( 'NONE',  ( 15.44008868035555260, 44.73035201082151247, 9.422509992056143702 ) ) ;
#74349 = AXIS2_PLACEMENT_3D ( 'NONE', #73736, #64746, #73242 ) ;
#74350 = FACE_OUTER_BOUND ( 'NONE', #57626, .T. ) ;
#74351 = DIRECTION ( 'NONE',  ( -0.000000000000000000, -1.000000000000000000, -0.000000000000000000 ) ) ;
#74352 = CARTESIAN_POINT ( 'NONE',  ( 14.92337183194729633, 62.67559781766745886, 8.527530157486181039 ) ) ;
#74353 = CARTESIAN_POINT ( 'NONE',  ( -2.266590686148945544, 2.220415501580634388, 7.082119434687048631 ) ) ;
#74354 = CARTESIAN_POINT ( 'NONE',  ( 17.20831665107776587, 22.88393115100078745, 7.208316651077764980 ) ) ;
#74355 = CARTESIAN_POINT ( 'NONE',  ( 6.880000000000009663, 40.99999999999999289, 6.500000000000000888 ) ) ;
#74356 =( GEOMETRIC_REPRESENTATION_CONTEXT ( 3 ) GLOBAL_UNCERTAINTY_ASSIGNED_CONTEXT ( ( #86338 ) ) GLOBAL_UNIT_ASSIGNED_CONTEXT ( ( #6784, #68285, #28781 ) ) REPRESENTATION_CONTEXT ( 'NONE', 'WORKASPACE' ) );
#74357 = CARTESIAN_POINT ( 'NONE',  ( 13.79529636645031943, 45.34541550158062506, -14.16423886937409904 ) ) ;
#74358 = ORIENTED_EDGE ( 'NONE', *, *, #11611, .F. ) ;
#74359 = CARTESIAN_POINT ( 'NONE',  ( 14.92337183194729988, 14.34226448433411782, -8.527530157486177487 ) ) ;
#74361 = DIRECTION ( 'NONE',  ( 0.000000000000000000, 1.000000000000000000, 0.000000000000000000 ) ) ;
#74360 = DIRECTION ( 'NONE',  ( -0.000000000000000000, 1.000000000000000000, 0.000000000000000000 ) ) ;
#74362 = CARTESIAN_POINT ( 'NONE',  ( 2.035157376598824452, 33.68868534415484106, 7.964842623401179544 ) ) ;
#74363 = CARTESIAN_POINT ( 'NONE',  ( 22.81628187352647785, 31.62363466993042138, 6.195893100308588602E-16 ) ) ;
#74364 = CARTESIAN_POINT ( 'NONE',  ( 10.00000000000000000, 1.813685344154837731, -10.88017736071110342 ) ) ;
#74365 = CARTESIAN_POINT ( 'NONE',  ( -1.099225684535947600, 29.54030133659708923, 6.408140936763237150 ) ) ;
#74366 = CARTESIAN_POINT ( 'NONE',  ( 21.09922568453595559, 57.04030133659708923, -6.408140936763230044 ) ) ;
#74367 = ORIENTED_EDGE ( 'NONE', *, *, #34774, .F. ) ;
#74368 = DIRECTION ( 'NONE',  ( 0.000000000000000000, 0.000000000000000000, 1.000000000000000000 ) ) ;
#74369 = CARTESIAN_POINT ( 'NONE',  ( -10.32525428031774339, -40.46312579907074536, -4.000000000000000000 ) ) ;
#74370 = CARTESIAN_POINT ( 'NONE',  ( -4.164238869374098151, 46.59541550158063927, -3.795296366450310543 ) ) ;
#74371 = CARTESIAN_POINT ( 'NONE',  ( 24.16423886937409904, 4.095415501580634832, 3.795296366450317205 ) ) ;
#74372 = CARTESIAN_POINT ( 'NONE',  ( 0.5774900079438590739, 12.64701867748817143, -5.440088680355550821 ) ) ;
#74373 = CARTESIAN_POINT ( 'NONE',  ( 12.91533473730993009, 16.60535201082150891, -10.88017736071109987 ) ) ;
#74374 = DIRECTION ( 'NONE',  ( 0.000000000000000000, 0.000000000000000000, -1.000000000000000000 ) ) ;
#74375 = DIRECTION ( 'NONE',  ( -1.000000000000000000, 0.000000000000000000, 0.000000000000000000 ) ) ;
#74376 = CARTESIAN_POINT ( 'NONE',  ( 7.084665262690076126, 52.02201867748816255, -10.88017736071110164 ) ) ;
#74377 = CARTESIAN_POINT ( 'NONE',  ( 10.00000000000000178, 49.31368534415484106, 10.88017736071110342 ) ) ;
#74378 = CARTESIAN_POINT ( 'NONE',  ( 21.09922568453594849, 16.20696800326375353, 6.408140936763242479 ) ) ;
#74379 = CARTESIAN_POINT ( 'NONE',  ( 4.084234479374286408, 0.000000000000000000, 3.613425430272956262 ) ) ;
#74380 = LINE ( 'NONE', #5907, #73900 ) ;
#74381 = CARTESIAN_POINT ( 'NONE',  ( 12.63842701281683922, 24.55059781766745175, -9.846743663894590881 ) ) ;
#74382 = EDGE_CURVE ( 'NONE', #25445, #13755, #80066, .T. ) ;
#74383 = CARTESIAN_POINT ( 'NONE',  ( 20.88017736071110875, 50.77201867748817676, -2.915334737309920765 ) ) ;
#74384 = VECTOR ( 'NONE', #63398, 1000.000000000000000 ) ;
#74385 = AXIS2_PLACEMENT_3D ( 'NONE', #29167, #75664, #59668 ) ;
#74386 = ADVANCED_FACE ( 'NONE', ( #95060 ), #72552, .T. ) ;
#74387 = CARTESIAN_POINT ( 'NONE',  ( -2.816281873526471635, 18.91530133659708213, -3.434112377981056508 ) ) ;
#74388 = CARTESIAN_POINT ( 'NONE',  ( 2.603489959281060973, 26.58210964143323096, 6.499999999999401368 ) ) ;
#74389 = AXIS2_PLACEMENT_3D ( 'NONE', #52305, #83794, #6808 ) ;
#74390 = EDGE_CURVE ( 'NONE', #32615, #97699, #89132, .T. ) ;
#74391 = CARTESIAN_POINT ( 'NONE',  ( 0.1532563361054082862, 36.21726448433410894, 2.638427012816831674 ) ) ;
#74392 = CARTESIAN_POINT ( 'NONE',  ( 10.00000000000000000, 42.87363466993042493, -12.81628187352647608 ) ) ;
#74393 = CARTESIAN_POINT ( 'NONE',  ( 19.84674366389459266, 23.71726448433412315, -2.638427012816827677 ) ) ;
#74394 = ORIENTED_EDGE ( 'NONE', *, *, #28363, .F. ) ;
#74395 = CARTESIAN_POINT ( 'NONE',  ( -0.3689425029237881626, 7.428748834913967869, 10.36894250292379027 ) ) ;
#74396 = CARTESIAN_POINT ( 'NONE',  ( 20.15039907845753930, 69.92552686551195507, -6.262539305110068177 ) ) ;
#74397 = CARTESIAN_POINT ( 'NONE',  ( 4.559911319644449179, 13.89701867748817143, 9.422509992056141925 ) ) ;
#74399 = CARTESIAN_POINT ( 'NONE',  ( 22.26659068614894466, 28.88708216824730357, 7.082119434687054849 ) ) ;
#74398 = FACE_OUTER_BOUND ( 'NONE', #10960, .T. ) ;
#74400 = CARTESIAN_POINT ( 'NONE',  ( 12.63842701281683034, 27.46726448433411250, 9.846743663894596210 ) ) ;
#74401 = CARTESIAN_POINT ( 'NONE',  ( 4.559911319644449179, 17.23035201082150536, -9.422509992056141925 ) ) ;
#74402 = CARTESIAN_POINT ( 'NONE',  ( -0.8801773607110991993, 12.85535201082150358, -2.915334737309923874 ) ) ;
#74403 = ORIENTED_EDGE ( 'NONE', *, *, #58413, .T. ) ;
#74404 = CARTESIAN_POINT ( 'NONE',  ( 0.5774900079438607392, 23.48035201082150536, 5.440088680355550821 ) ) ;
#74405 = EDGE_CURVE ( 'NONE', #85917, #55638, #71103, .T. ) ;
#74406 = CARTESIAN_POINT ( 'NONE',  ( 3.591859063236763294, 43.29030133659708923, -11.09922568453595026 ) ) ;
#74407 = CARTESIAN_POINT ( 'NONE',  ( -0.8801773607110991993, 37.85535201082151247, -2.915334737309923874 ) ) ;
#74408 = VERTEX_POINT ( 'NONE', #11084 ) ;
#74409 = CARTESIAN_POINT ( 'NONE',  ( 2.791683348922240793, 56.63393115100078035, 7.208316651077764092 ) ) ;
#74410 = CARTESIAN_POINT ( 'NONE',  ( -0.8801773607111009756, 43.06368534415484106, 1.068504757029289695E-15 ) ) ;
#74411 = CARTESIAN_POINT ( 'NONE',  ( 1.472469842513823179, 65.59226448433412315, -4.923371831947296329 ) ) ;
#74412 = SURFACE_STYLE_USAGE ( .BOTH. , #57452 ) ;
#74413 = DIRECTION ( 'NONE',  ( 0.000000000000000000, -1.000000000000000000, 0.000000000000000000 ) ) ;
#74414 = CARTESIAN_POINT ( 'NONE',  ( 6.204703633549690345, 50.76208216824730357, -14.16423886937410259 ) ) ;
#74415 = CARTESIAN_POINT ( 'NONE',  ( 20.88017736071110875, 50.77201867748817676, -2.915334737309920765 ) ) ;
#74416 = LINE ( 'NONE', #11959, #68927 ) ;
#74417 = CARTESIAN_POINT ( 'NONE',  ( 8.549759589250173875, 14.76984986101048847, 12.25250350990703652 ) ) ;
#74418 = CARTESIAN_POINT ( 'NONE',  ( 18.52753015748617571, 48.09226448433412315, 4.923371831947298993 ) ) ;
#74419 = CARTESIAN_POINT ( 'NONE',  ( 12.63842701281683034, 2.467264484334118269, 9.846743663894596210 ) ) ;
#74420 = CARTESIAN_POINT ( 'NONE',  ( 12.63842701281683922, 19.55059781766745175, -9.846743663894590881 ) ) ;
#74421 = ORIENTED_EDGE ( 'NONE', *, *, #75342, .F. ) ;
#74422 = EDGE_CURVE ( 'NONE', #14972, #96670, #44934, .T. ) ;
#74423 = CARTESIAN_POINT ( 'NONE',  ( 0.1532563361054083140, 26.00893115100078745, 1.131784320476157264E-15 ) ) ;
#74424 = CARTESIAN_POINT ( 'NONE',  ( -9.382169495545413795, -15.25136533006957684, 9.382169495545428006 ) ) ;
#74425 = CARTESIAN_POINT ( 'NONE',  ( 0.5774900079438607392, 28.48035201082150891, 5.440088680355550821 ) ) ;
#74426 = CARTESIAN_POINT ( 'NONE',  ( 19.84674366389459621, 23.50893115100078390, 7.409399052514197653E-17 ) ) ;
#74427 = CARTESIAN_POINT ( 'NONE',  ( -2.816281873526473856, 14.33196800326375531, 3.434112377981055619 ) ) ;
#74428 = CARTESIAN_POINT ( 'NONE',  ( 19.42250999205614193, 65.14701867748817676, 5.440088680355555262 ) ) ;
#74430 = CARTESIAN_POINT ( 'NONE',  ( 22.81628187352647785, 56.62363466993042493, 6.195893100308588602E-16 ) ) ;
#74429 = CARTESIAN_POINT ( 'NONE',  ( 17.96484262340118221, 36.18868534415484106, -7.964842623401177768 ) ) ;
#74431 = CARTESIAN_POINT ( 'NONE',  ( 2.917880565312948704, 47.63708216824730357, 12.26659068614894643 ) ) ;
#74432 = AXIS2_PLACEMENT_3D ( 'NONE', #70587, #48062, #40086 ) ;
#74433 = AXIS2_PLACEMENT_3D ( 'NONE', #27123, #49620, #81117 ) ;
#74434 = ADVANCED_FACE ( 'NONE', ( #42563 ), #38544, .T. ) ;
#74435 = CARTESIAN_POINT ( 'NONE',  ( -14.71525861348292175, 14.49999999999999822, 2.908807992686482713 ) ) ;
#74436 = ORIENTED_EDGE ( 'NONE', *, *, #82079, .F. ) ;
#74437 = CARTESIAN_POINT ( 'NONE',  ( 0.6178305044545838731, 4.748634669930420493, 9.382169495545420901 ) ) ;
#74438 = CARTESIAN_POINT ( 'NONE',  ( -0.8801773607111008646, 3.272018677488171434, 2.915334737309923430 ) ) ;
#74439 = CARTESIAN_POINT ( 'NONE',  ( 15.44008868035555793, 51.39701867748816966, -9.422509992056140149 ) ) ;
#74440 = VERTEX_POINT ( 'NONE', #86595 ) ;
#74441 = CARTESIAN_POINT ( 'NONE',  ( 0.1532563361054083140, 16.00893115100078390, 1.131784320476157264E-15 ) ) ;
#74442 = CARTESIAN_POINT ( 'NONE',  ( 17.96484262340118221, 56.18868534415484817, -7.964842623401177768 ) ) ;
#74443 = CARTESIAN_POINT ( 'NONE',  ( 0.1532563361054082862, 31.21726448433412315, 2.638427012816831674 ) ) ;
#74444 = CARTESIAN_POINT ( 'NONE',  ( 19.84674366389459266, 18.71726448433411960, -2.638427012816827677 ) ) ;
#74445 = VECTOR ( 'NONE', #24339, 1000.000000000000000 ) ;
#74446 = CARTESIAN_POINT ( 'NONE',  ( 18.52753015748617571, 8.092264484334117824, 4.923371831947298993 ) ) ;
#74448 = CARTESIAN_POINT ( 'NONE',  ( 0.6178305044545838731, 34.74863466993042493, 9.382169495545420901 ) ) ;
#74447 = CARTESIAN_POINT ( 'NONE',  ( -6.732636091893170693, -88.11213685669366669, 2.500000000000000888 ) ) ;
#74450 = LINE ( 'NONE', #5978, #15205 ) ;
#74449 = CARTESIAN_POINT ( 'NONE',  ( 0.1532563361054100626, 0.8005978176674514168, -2.638427012816831230 ) ) ;
#74451 = CARTESIAN_POINT ( 'NONE',  ( 11.01504402775471014, -96.09667835293565474, 3.750000000000000000 ) ) ;
#74453 = ORIENTED_EDGE ( 'NONE', *, *, #94367, .F. ) ;
#74452 = CARTESIAN_POINT ( 'NONE',  ( 7.361572987183169658, 29.96726448433411960, -9.846743663894592657 ) ) ;
#74454 =( BOUNDED_CURVE ( )  B_SPLINE_CURVE ( 2, ( #16500, #39003, #69498, #1014, #31475, #46977, #8982, #3467, #57431 ),
 .UNSPECIFIED., .F., .T. ) 
 B_SPLINE_CURVE_WITH_KNOTS ( ( 3, 2, 2, 2, 3 ),
 ( 0.6534289457926083511, 0.6547619047619047672, 0.6607142857142856984, 0.6666666666666666297, 0.6679996256359631568 ),
 .UNSPECIFIED. ) 
 CURVE ( )  GEOMETRIC_REPRESENTATION_ITEM ( )  RATIONAL_B_SPLINE_CURVE ( ( 0.9881565478350733400, 0.9923695281211490915, 1.000000000000000000, 0.9659258262890683122, 1.000000000000000000, 0.9659258262890683122, 1.000000000000000000, 0.9923695281211485364, 0.9881565478350726739 ) ) 
 REPRESENTATION_ITEM ( '' )  );
#74455 = CARTESIAN_POINT ( 'NONE',  ( 13.43411237798105340, 55.58196800326374643, 12.81628187352647963 ) ) ;
#74456 = CARTESIAN_POINT ( 'NONE',  ( 20.15039907845753575, 12.62777174578613071, -6.262539305110077059 ) ) ;
#74457 = CARTESIAN_POINT ( 'NONE',  ( 22.81628187352647785, 1.415301336597087012, 3.434112377981063169 ) ) ;
#74458 =( LENGTH_UNIT ( ) NAMED_UNIT ( * ) SI_UNIT ( .MILLI., .METRE. ) );
#74459 = AXIS2_PLACEMENT_3D ( 'NONE', #62637, #85162, #77156 ) ;
#74460 = CARTESIAN_POINT ( 'NONE',  ( 24.16423886937410614, 24.30374883491396787, 8.672049930838204340E-16 ) ) ;
#74461 = PRODUCT_DEFINITION_CONTEXT ( 'detailed design', #72970, 'design' ) ;
#74462 = DIRECTION ( 'NONE',  ( 0.6246950475544237324, 0.7808688094430306093, 0.000000000000000000 ) ) ;
#74463 = CARTESIAN_POINT ( 'NONE',  ( 6.204703633549690345, 30.76208216824730357, -14.16423886937410259 ) ) ;
#74464 = CARTESIAN_POINT ( 'NONE',  ( -4.164238869374098151, 41.59541550158061796, -3.795296366450310543 ) ) ;
#74465 = MANIFOLD_SOLID_BREP ( 'Fillet2', #28251 ) ;
#74466 = EDGE_CURVE ( 'NONE', #31523, #59916, #15242, .T. ) ;
#74467 = CARTESIAN_POINT ( 'NONE',  ( 10.00000000000000000, 15.55374883491396787, -14.16423886937410082 ) ) ;
#74469 = PLANE ( 'NONE',  #44612 ) ;
#74468 = CARTESIAN_POINT ( 'NONE',  ( 24.16423886937409904, 14.09541550158063217, 3.795296366450317205 ) ) ;
#74470 = CARTESIAN_POINT ( 'NONE',  ( 17.96484262340118221, 46.18868534415484106, -7.964842623401177768 ) ) ;
#74471 = CARTESIAN_POINT ( 'NONE',  ( 14.40939250469964961, 3.793246902777681429E-16, 1.618458416365853747 ) ) ;
#74472 = CARTESIAN_POINT ( 'NONE',  ( 2.791683348922240793, 31.63393115100078745, 7.208316651077764092 ) ) ;
#74474 = CARTESIAN_POINT ( 'NONE',  ( 14.92337183194729633, 27.67559781766745530, 8.527530157486181039 ) ) ;
#74473 = LINE ( 'NONE', #28970, #6972 ) ;
#74475 = CARTESIAN_POINT ( 'NONE',  ( 15.44008868035555260, 14.73035201082150536, 9.422509992056143702 ) ) ;
#74476 = CARTESIAN_POINT ( 'NONE',  ( 6.565887622018943937, 63.08196800326376064, -12.81628187352647608 ) ) ;
#74477 = CARTESIAN_POINT ( 'NONE',  ( 17.20831665107776587, 47.88393115100078745, 7.208316651077764980 ) ) ;
#74478 = EDGE_CURVE ( 'NONE', #91030, #23318, #75523, .T. ) ;
#74479 = DIRECTION ( 'NONE',  ( 0.000000000000000000, 0.000000000000000000, 1.000000000000000000 ) ) ;
#74480 = CARTESIAN_POINT ( 'NONE',  ( 18.52753015748617571, 28.09226448433411960, 4.923371831947298993 ) ) ;
#74482 = CARTESIAN_POINT ( 'NONE',  ( 22.81628187352648496, 41.83196800326375353, -3.434112377981050290 ) ) ;
#74481 = AXIS2_PLACEMENT_3D ( 'NONE', #16697, #86667, #1707 ) ;
#74483 = CARTESIAN_POINT ( 'NONE',  ( -14.16423886937410082, -18.19625116508602858, 4.336808689942017736E-15 ) ) ;
#74484 = CARTESIAN_POINT ( 'NONE',  ( 20.88017736071110875, 40.77201867748818387, -2.915334737309920765 ) ) ;
#74485 = CARTESIAN_POINT ( 'NONE',  ( 7.361572987183169658, 39.96726448433411605, -9.846743663894592657 ) ) ;
#74486 = CARTESIAN_POINT ( 'NONE',  ( -4.164238869374099039, 26.80374883491397142, 8.674139862899312516E-16 ) ) ;
#74487 = MECHANICAL_DESIGN_GEOMETRIC_PRESENTATION_REPRESENTATION (  '', ( #53621 ), #71295 ) ;
#74488 = VERTEX_POINT ( 'NONE', #35043 ) ;
#74489 = CARTESIAN_POINT ( 'NONE',  ( -2.930023131210709231, 0.000000000000000000, -4.599215049682199741 ) ) ;
#74490 = CARTESIAN_POINT ( 'NONE',  ( 2.035157376598824452, 48.68868534415483396, 7.964842623401179544 ) ) ;
#74491 = DIRECTION ( 'NONE',  ( 0.000000000000000000, 0.000000000000000000, 1.000000000000000000 ) ) ;
#74492 = CARTESIAN_POINT ( 'NONE',  ( 13.79529636645031943, 55.34541550158062506, -14.16423886937409904 ) ) ;
#74493 = CARTESIAN_POINT ( 'NONE',  ( 10.00000000000000178, 0.3736346699304200492, 12.81628187352647608 ) ) ;
#74494 = DIRECTION ( 'NONE',  ( 0.000000000000000000, 1.000000000000000000, 0.000000000000000000 ) ) ;
#74495 = CARTESIAN_POINT ( 'NONE',  ( 17.96484262340118221, 59.93868534415484106, 7.964842623401181321 ) ) ;
#74496 = DIRECTION ( 'NONE',  ( -0.000000000000000000, -1.000000000000000000, -0.000000000000000000 ) ) ;
#74497 = CARTESIAN_POINT ( 'NONE',  ( -1.099225684535947600, -0.4596986634029132657, 6.408140936763237150 ) ) ;
#74498 = CARTESIAN_POINT ( 'NONE',  ( -10.88017736071110342, 28.06368534415484817, 3.903127820947815962E-15 ) ) ;
#74499 = CARTESIAN_POINT ( 'NONE',  ( 4.559911319644449179, 12.23035201082150536, -9.422509992056141925 ) ) ;
#74500 = CARTESIAN_POINT ( 'NONE',  ( -0.8801773607110991993, 7.855352010821506248, -2.915334737309923874 ) ) ;
#74501 = CARTESIAN_POINT ( 'NONE',  ( 5.076628168052703671, 41.84226448433411605, 8.527530157486179263 ) ) ;
#74502 = CARTESIAN_POINT ( 'NONE',  ( 14.88232117145531141, 15.00000000000000000, -1.875237731503139438 ) ) ;
#74503 = VERTEX_POINT ( 'NONE', #58043 ) ;
#74504 = CIRCLE ( 'NONE', #72976, 15.00000000000000000 ) ;
#74505 = CARTESIAN_POINT ( 'NONE',  ( 17.96484262340118221, 4.938685344154837509, 7.964842623401181321 ) ) ;
#74506 = CARTESIAN_POINT ( 'NONE',  ( 22.81628187352648496, 1.831968003263753753, -3.434112377981050290 ) ) ;
#74507 = PLANE ( 'NONE',  #87964 ) ;
#74508 = CARTESIAN_POINT ( 'NONE',  ( 2.791683348922240793, 16.63393115100078745, 7.208316651077764092 ) ) ;
#74509 = EDGE_CURVE ( 'NONE', #81942, #1776, #66040, .T. ) ;
#74510 = CARTESIAN_POINT ( 'NONE',  ( 10.00000000000000000, 34.75893115100078745, -9.846743663894594434 ) ) ;
#74511 = CARTESIAN_POINT ( 'NONE',  ( 20.88017736071110875, 30.77201867748816966, -2.915334737309920765 ) ) ;
#74512 = ADVANCED_FACE ( 'NONE', ( #20053 ), #64819, .T. ) ;
#74513 = VECTOR ( 'NONE', #77159, 1000.000000000000000 ) ;
#74514 = CARTESIAN_POINT ( 'NONE',  ( 13.43411237798106583, 7.665301336597086568, -12.81628187352647252 ) ) ;
#74516 = PLANE ( 'NONE',  #52792 ) ;
#74515 = CARTESIAN_POINT ( 'NONE',  ( 4.559911319644449179, 52.23035201082151247, -9.422509992056141925 ) ) ;
#74517 = CARTESIAN_POINT ( 'NONE',  ( 10.00000000000000000, 57.87363466993042493, -12.81628187352647608 ) ) ;
#74518 = ORIENTED_EDGE ( 'NONE', *, *, #10862, .F. ) ;
#74519 = CARTESIAN_POINT ( 'NONE',  ( 2.035157376598824452, 68.68868534415484817, 7.964842623401179544 ) ) ;
#74521 = CARTESIAN_POINT ( 'NONE',  ( 10.00000000000000000, 0.5537488349139675359, -14.16423886937410082 ) ) ;
#74520 = CARTESIAN_POINT ( 'NONE',  ( -1.099225684535947600, 33.70696800326375353, -6.408140936763238038 ) ) ;
#74522 = CARTESIAN_POINT ( 'NONE',  ( 13.14228782657341732, 14.49999999999999112, 7.230509711182337540 ) ) ;
#74523 = CARTESIAN_POINT ( 'NONE',  ( 10.00000000000000178, 34.31368534415484106, 10.88017736071110342 ) ) ;
#74524 = DIRECTION ( 'NONE',  ( -0.9890158633619157147, 0.000000000000000000, -0.1478094111296180124 ) ) ;
#74525 = CARTESIAN_POINT ( 'NONE',  ( 19.84674366389459266, 58.71726448433411605, -2.638427012816827677 ) ) ;
#74526 = CARTESIAN_POINT ( 'NONE',  ( 7.361572987183169658, 19.96726448433411960, -9.846743663894592657 ) ) ;
#74527 = CARTESIAN_POINT ( 'NONE',  ( 14.92337183194729988, 4.342264484334117824, -8.527530157486177487 ) ) ;
#74528 = LINE ( 'NONE', #66038, #47513 ) ;
#74529 = CARTESIAN_POINT ( 'NONE',  ( 6.204703633549690345, 47.84541550158064638, 14.16423886937410082 ) ) ;
#74530 = CARTESIAN_POINT ( 'NONE',  ( 1.821158202401483406, 56.16688879859522388, 6.499999999999917399 ) ) ;
#74531 = CARTESIAN_POINT ( 'NONE',  ( 14.02068044289379500, 0.3640475087720986824, -5.331089937175662818 ) ) ;
#74532 = VECTOR ( 'NONE', #48236, 1000.000000000000000 ) ;
#74533 = ORIENTED_EDGE ( 'NONE', *, *, #56826, .T. ) ;
#74534 = CARTESIAN_POINT ( 'NONE',  ( 2.917880565312948704, 57.63708216824731068, 12.26659068614894643 ) ) ;
#74535 = CARTESIAN_POINT ( 'NONE',  ( 10.00000000000000000, 60.55374883491397497, -14.16423886937410082 ) ) ;
#74536 = CARTESIAN_POINT ( 'NONE',  ( 17.20831665107776587, 27.88393115100078390, 7.208316651077764980 ) ) ;
#74537 = CARTESIAN_POINT ( 'NONE',  ( 19.38216949554541557, 22.24863466993041428, -9.382169495545420901 ) ) ;
#74538 = CARTESIAN_POINT ( 'NONE',  ( 4.431036607602602651, 14.49999999999999112, -14.33059365769916305 ) ) ;
#74540 = CARTESIAN_POINT ( 'NONE',  ( 13.79529636645031943, 10.34541550158063394, -14.16423886937409904 ) ) ;
#74539 = CARTESIAN_POINT ( 'NONE',  ( 7.595945211628331251, 3.826527677142797770E-16, -12.35117874301642082 ) ) ;
#74541 = CARTESIAN_POINT ( 'NONE',  ( 2.035157376598824452, 18.68868534415484106, 7.964842623401179544 ) ) ;
#74542 = CARTESIAN_POINT ( 'NONE',  ( 6.204703633549690345, 52.84541550158062506, 14.16423886937410082 ) ) ;
#74543 = EDGE_CURVE ( 'NONE', #91314, #68676, #56164, .T. ) ;
#74544 = VECTOR ( 'NONE', #34727, 1000.000000000000000 ) ;
#74545 = CARTESIAN_POINT ( 'NONE',  ( 10.00000000000000000, 29.75893115100078745, -9.846743663894594434 ) ) ;
#74546 = DIRECTION ( 'NONE',  ( -0.000000000000000000, -1.000000000000000000, -0.000000000000000000 ) ) ;
#74547 = CARTESIAN_POINT ( 'NONE',  ( 18.52753015748618282, 3.925597817667451306, -4.923371831947291888 ) ) ;
#74548 = EDGE_CURVE ( 'NONE', #49599, #20937, #93918, .T. ) ;
#74549 = FACE_OUTER_BOUND ( 'NONE', #19585, .T. ) ;
#74550 = CARTESIAN_POINT ( 'NONE',  ( -4.923371831947302546, 15.17559781766746063, -8.527530157486173934 ) ) ;
#74551 = EDGE_LOOP ( 'NONE', ( #52444, #20073, #88071, #81168 ) ) ;
#74552 = VERTEX_POINT ( 'NONE', #71649 ) ;
#74553 = CARTESIAN_POINT ( 'NONE',  ( -6.742022620658060461, 14.95037102811560459, -13.12259272460513770 ) ) ;
#74554 = ORIENTED_EDGE ( 'NONE', *, *, #50943, .F. ) ;
#74555 = CARTESIAN_POINT ( 'NONE',  ( 2.791683348922237240, 45.38393115100079456, -7.208316651077763204 ) ) ;
#74556 = CARTESIAN_POINT ( 'NONE',  ( 24.16423886937410614, 19.30374883491397142, 8.672049930838204340E-16 ) ) ;
#74558 = CARTESIAN_POINT ( 'NONE',  ( 10.00000000000000178, 29.31368534415483751, 10.88017736071110342 ) ) ;
#74557 = CARTESIAN_POINT ( 'NONE',  ( 20.88017736071110875, 25.77201867748816966, -2.915334737309920765 ) ) ;
#74560 = CARTESIAN_POINT ( 'NONE',  ( 22.81628187352648496, 11.83196800326375531, -3.434112377981050290 ) ) ;
#74559 = CARTESIAN_POINT ( 'NONE',  ( 18.52753015748618282, 63.92559781766745886, -4.923371831947291888 ) ) ;
#74561 = CARTESIAN_POINT ( 'NONE',  ( 17.08211943468705130, 3.470415501580634388, 12.26659068614894998 ) ) ;
#74562 = AXIS2_PLACEMENT_3D ( 'NONE', #91570, #24066, #77050 ) ;
#74563 = VECTOR ( 'NONE', #73648, 1000.000000000000000 ) ;
#74564 = TOROIDAL_SURFACE ( 'NONE', #33018, 14.49999999999999822, 0.5000000000000000000 ) ;
#74565 = CARTESIAN_POINT ( 'NONE',  ( 19.38216949554541202, 30.99863466993042138, 9.382169495545424454 ) ) ;
#74566 = ORIENTED_EDGE ( 'NONE', *, *, #7017, .T. ) ;
#74567 = CARTESIAN_POINT ( 'NONE',  ( 18.52753015748618282, 33.92559781766745886, -4.923371831947291888 ) ) ;
#74568 = CARTESIAN_POINT ( 'NONE',  ( 20.88017736071110164, 10.35535201082150714, 2.915334737309930979 ) ) ;
#74569 = ORIENTED_EDGE ( 'NONE', *, *, #40068, .T. ) ;
#74570 = CARTESIAN_POINT ( 'NONE',  ( 0.5774900079438607392, 3.480352010821504916, 5.440088680355550821 ) ) ;
#74571 = ORIENTED_EDGE ( 'NONE', *, *, #68670, .T. ) ;
#74572 = CARTESIAN_POINT ( 'NONE',  ( 2.035157376598824452, 53.68868534415484817, 7.964842623401179544 ) ) ;
#74573 = CARTESIAN_POINT ( 'NONE',  ( 0.5774900079438607392, 58.48035201082151247, 5.440088680355550821 ) ) ;
#74574 = CARTESIAN_POINT ( 'NONE',  ( 7.084665262690076126, 47.02201867748818387, -10.88017736071110164 ) ) ;
#74575 = CARTESIAN_POINT ( 'NONE',  ( 0.5774900079438607392, 58.48035201082151247, 5.440088680355550821 ) ) ;
#74576 = CARTESIAN_POINT ( 'NONE',  ( -1.926860441876562247, 52.45379003517449235, -3.195792623639530650 ) ) ;
#74578 = ORIENTED_EDGE ( 'NONE', *, *, #90990, .F. ) ;
#74577 = CARTESIAN_POINT ( 'NONE',  ( 9.479672251262046601, -19.63639846206612560, 4.000000000000000888 ) ) ;
#74579 = B_SPLINE_CURVE_WITH_KNOTS ( 'NONE', 3,
 ( #26018, #48506, #87003, #41028, #34476, #85536 ),
 .UNSPECIFIED., .F., .F.,
 ( 4, 2, 4 ),
 ( 0.0002800003243993126178, 0.0006862055569927218634, 0.001092410789586131109 ),
 .UNSPECIFIED. ) ;
#74580 = CARTESIAN_POINT ( 'NONE',  ( 18.52753015748617571, 23.09226448433411960, 4.923371831947298993 ) ) ;
#74581 = ORIENTED_EDGE ( 'NONE', *, *, #94315, .F. ) ;
#74582 = CARTESIAN_POINT ( 'NONE',  ( 10.00000000000000000, 54.75893115100078745, -9.846743663894594434 ) ) ;
#74583 = DIRECTION ( 'NONE',  ( 0.000000000000000000, 1.000000000000000000, 0.000000000000000000 ) ) ;
#74584 = AXIS2_PLACEMENT_3D ( 'NONE', #32329, #61359, #68880 ) ;
#74585 = CARTESIAN_POINT ( 'NONE',  ( -2.266590686148945544, 6.387082168247300906, -7.082119434687050408 ) ) ;
#74586 = EDGE_LOOP ( 'NONE', ( #26513, #32137, #1967 ) ) ;
#74587 = CARTESIAN_POINT ( 'NONE',  ( -11.39900937121540814, 12.73119725676927771, -1.484196799168450376 ) ) ;
#74588 = CARTESIAN_POINT ( 'NONE',  ( -7.037762026445613550, -86.26090966542943761, 3.750000000000001332 ) ) ;
#74590 = CARTESIAN_POINT ( 'NONE',  ( 12.63842701281683034, 37.46726448433411605, 9.846743663894596210 ) ) ;
#74589 = CARTESIAN_POINT ( 'NONE',  ( 9.779999999999990479, 18.00000000000000000, 0.000000000000000000 ) ) ;
#74591 = CARTESIAN_POINT ( 'NONE',  ( 20.88017736071110875, 10.77201867748817143, -2.915334737309920765 ) ) ;
#74592 = CARTESIAN_POINT ( 'NONE',  ( 0.000000000000000000, 0.5000000000000004441, 0.000000000000000000 ) ) ;
#74593 = VERTEX_POINT ( 'NONE', #81104 ) ;
#74594 = FACE_OUTER_BOUND ( 'NONE', #82852, .T. ) ;
#74595 = CARTESIAN_POINT ( 'NONE',  ( 19.84674366389459266, 43.30059781766744464, 2.638427012816836559 ) ) ;
#74596 = DIRECTION ( 'NONE',  ( 0.7489557207890082946, 0.000000000000000000, -0.6626200482157305061 ) ) ;
#74597 = CARTESIAN_POINT ( 'NONE',  ( 10.00000000000000000, 12.87363466993042138, -12.81628187352647608 ) ) ;
#74598 = CARTESIAN_POINT ( 'NONE',  ( 1.472469842513823179, 16.42559781766745175, 4.923371831947296329 ) ) ;
#74599 = ADVANCED_FACE ( 'NONE', ( #95114 ), #25666, .F. ) ;
#74600 = DIRECTION ( 'NONE',  ( -0.5547001962252291474, -0.8320502943378437211, -0.000000000000000000 ) ) ;
#74601 = CARTESIAN_POINT ( 'NONE',  ( 14.92337183194729988, 19.34226448433411960, -8.527530157486177487 ) ) ;
#74602 = CARTESIAN_POINT ( 'NONE',  ( 0.1532563361054083140, 66.00893115100079456, 1.131784320476157264E-15 ) ) ;
#74603 = FILL_AREA_STYLE_COLOUR ( '', #89022 ) ;
#74604 = COLOUR_RGB ( '', 0.08235294, 0.09019608, 0.10196078) ;
#74605 = VERTEX_POINT ( 'NONE', #95622 ) ;
#74606 = CARTESIAN_POINT ( 'NONE',  ( 17.96484262340118221, 9.938685344154839285, 7.964842623401181321 ) ) ;
#74607 = CARTESIAN_POINT ( 'NONE',  ( 2.917880565312950480, 5.970415501580634832, -12.26659068614894821 ) ) ;
#74608 = CARTESIAN_POINT ( 'NONE',  ( 12.63842701281683922, 24.55059781766745175, -9.846743663894590881 ) ) ;
#74609 = CARTESIAN_POINT ( 'NONE',  ( 10.00000000000000178, 54.31368534415484106, 10.88017736071110342 ) ) ;
#74610 = CARTESIAN_POINT ( 'NONE',  ( -1.099225684535947600, 38.70696800326375353, -6.408140936763238038 ) ) ;
#74611 = CARTESIAN_POINT ( 'NONE',  ( 20.88017736071110519, 20.56368534415484106, 2.639326808657452039E-16 ) ) ;
#74612 = DIRECTION ( 'NONE',  ( -0.8949343616020323244, -0.000000000000000000, 0.4461978131097944500 ) ) ;
#74613 = CARTESIAN_POINT ( 'NONE',  ( 13.34343830728402125, 14.63606867471890816, 6.852200678592722305 ) ) ;
#74614 = VECTOR ( 'NONE', #1777, 1000.000000000000000 ) ;
#74615 = CARTESIAN_POINT ( 'NONE',  ( 13.43411237798105340, 5.581968003263753531, 12.81628187352647963 ) ) ;
#74616 = CARTESIAN_POINT ( 'NONE',  ( 6.565887622018943937, -1.918031996736246692, -12.81628187352647608 ) ) ;
#74617 = CARTESIAN_POINT ( 'NONE',  ( 2.791683348922240793, 26.63393115100078745, 7.208316651077764092 ) ) ;
#74618 = CARTESIAN_POINT ( 'NONE',  ( 2.915334737309928315, -5.477981322511826789, 10.88017736071109987 ) ) ;
#74619 = CARTESIAN_POINT ( 'NONE',  ( 22.81628187352647785, 41.41530133659708923, 3.434112377981063169 ) ) ;
#74620 = DIRECTION ( 'NONE',  ( -0.000000000000000000, 1.000000000000000000, -0.000000000000000000 ) ) ;
#74622 = CARTESIAN_POINT ( 'NONE',  ( -8.134956207566176545, -0.03417435944610275333, 13.77315809598633756 ) ) ;
#74621 = CARTESIAN_POINT ( 'NONE',  ( 20.88017736071110875, 40.77201867748818387, -2.915334737309920765 ) ) ;
#74623 = AXIS2_PLACEMENT_3D ( 'NONE', #31662, #77654, #716 ) ;
#74624 = CARTESIAN_POINT ( 'NONE',  ( 14.19749592853504438, 15.00000000000000000, -7.369430493279943484 ) ) ;
#74625 = CARTESIAN_POINT ( 'NONE',  ( 20.88017736071110164, 45.35535201082149115, 2.915334737309930979 ) ) ;
#74626 = CARTESIAN_POINT ( 'NONE',  ( 19.42250999205614193, 25.14701867748817321, 5.440088680355555262 ) ) ;
#74627 = CARTESIAN_POINT ( 'NONE',  ( 12.63842701281683034, 62.46726448433410894, 9.846743663894596210 ) ) ;
#74628 = ADVANCED_FACE ( 'NONE', ( #72121 ), #49793, .T. ) ;
#74629 = CARTESIAN_POINT ( 'NONE',  ( 0.5774900079438590739, 52.64701867748817676, -5.440088680355550821 ) ) ;
#74630 = B_SPLINE_CURVE_WITH_KNOTS ( 'NONE', 3,
 ( #63162, #86181, #39706, #93670, #48163, #24208 ),
 .UNSPECIFIED., .F., .F.,
 ( 4, 2, 4 ),
 ( 3.409110551494477282E-05, 0.0004400426677367911795, 0.0008459942299586376132 ),
 .UNSPECIFIED. ) ;
#74631 = ADVANCED_FACE ( 'NONE', ( #19129 ), #41654, .T. ) ;
#74632 = CARTESIAN_POINT ( 'NONE',  ( 1.472469842513823179, 40.59226448433411605, -4.923371831947296329 ) ) ;
#74633 = CARTESIAN_POINT ( 'NONE',  ( 10.00000000000000178, 65.37363466993042493, 12.81628187352647608 ) ) ;
#74634 = CARTESIAN_POINT ( 'NONE',  ( 16.40814093676323893, 15.79030133659708746, 11.09922568453595026 ) ) ;
#74635 = ORIENTED_EDGE ( 'NONE', *, *, #72374, .T. ) ;
#74636 = CARTESIAN_POINT ( 'NONE',  ( 15.44008868035555260, 19.73035201082150536, 9.422509992056143702 ) ) ;
#74637 = FACE_OUTER_BOUND ( 'NONE', #35343, .T. ) ;
#74638 = CARTESIAN_POINT ( 'NONE',  ( 7.084665262690076126, 14.10535201082150358, 10.88017736071109987 ) ) ;
#74639 = CARTESIAN_POINT ( 'NONE',  ( 19.84674366389459266, 3.717264484334118713, -2.638427012816827677 ) ) ;
#74640 = CARTESIAN_POINT ( 'NONE',  ( 24.16423886937409904, 24.09541550158063927, 3.795296366450317205 ) ) ;
#74641 = MANIFOLD_SOLID_BREP ( 'Fillet9', #31460 ) ;
#74642 = CARTESIAN_POINT ( 'NONE',  ( 1.472469842513823179, 10.59226448433411782, -4.923371831947296329 ) ) ;
#74643 = CARTESIAN_POINT ( 'NONE',  ( 0.1532563361054083140, 61.00893115100078745, 1.131784320476157264E-15 ) ) ;
#74644 = CARTESIAN_POINT ( 'NONE',  ( 10.00000000000000000, 51.81368534415484106, -10.88017736071110342 ) ) ;
#74645 = CARTESIAN_POINT ( 'NONE',  ( 0.1955144967548735624, 34.32703681773342197, -6.500000000002695622 ) ) ;
#74646 = DIRECTION ( 'NONE',  ( -1.000000000000000000, 6.608470384673550777E-17, 0.000000000000000000 ) ) ;
#74647 = VERTEX_POINT ( 'NONE', #21608 ) ;
#74648 = CARTESIAN_POINT ( 'NONE',  ( -4.250000000000000000, 37.00000000000000000, 4.000000000000000000 ) ) ;
#74649 = CARTESIAN_POINT ( 'NONE',  ( 0.1532563361054083140, 46.00893115100079456, 1.131784320476157264E-15 ) ) ;
#74650 = VERTEX_POINT ( 'NONE', #6104 ) ;
#74651 = VERTEX_POINT ( 'NONE', #83582 ) ;
#74652 = LINE ( 'NONE', #98172, #82101 ) ;
#74653 = CARTESIAN_POINT ( 'NONE',  ( -0.3689425029237881626, 17.42874883491397142, 10.36894250292379027 ) ) ;
#74654 = CARTESIAN_POINT ( 'NONE',  ( 17.08211943468705840, 30.13708216824730357, -12.26659068614894466 ) ) ;
#74655 = CARTESIAN_POINT ( 'NONE',  ( -0.8801773607111009756, 63.06368534415484106, 1.068504757029289695E-15 ) ) ;
#74656 = CARTESIAN_POINT ( 'NONE',  ( 0.5774900079438590739, 2.647018677488171434, -5.440088680355550821 ) ) ;
#74657 = CARTESIAN_POINT ( 'NONE',  ( -2.816281873526473856, 4.123634669930420493, 9.499525473075851096E-16 ) ) ;
#74658 = CARTESIAN_POINT ( 'NONE',  ( 2.791683348922240793, 51.63393115100078745, 7.208316651077764092 ) ) ;
#74659 = CARTESIAN_POINT ( 'NONE',  ( -11.42361443008651634, -90.30744058743700009, 3.750000000000000000 ) ) ;
#74661 = CARTESIAN_POINT ( 'NONE',  ( 3.591859063236761518, -0.04303199673624671928, 11.09922568453594849 ) ) ;
#74660 = CARTESIAN_POINT ( 'NONE',  ( 0.5774900079438590739, 47.64701867748817676, -5.440088680355550821 ) ) ;
#74662 = CARTESIAN_POINT ( 'NONE',  ( 24.16423886937410614, 19.51208216824729647, -3.795296366450302550 ) ) ;
#74663 = CARTESIAN_POINT ( 'NONE',  ( 2.035157376598824452, 18.68868534415484106, 7.964842623401179544 ) ) ;
#74664 = COLOUR_RGB ( '', 0.72549020, 0.75294118, 0.79215686) ;
#74665 = CARTESIAN_POINT ( 'NONE',  ( -0.8801773607111009756, 23.06368534415484106, 1.068504757029289695E-15 ) ) ;
#74666 = LINE ( 'NONE', #6176, #81116 ) ;
#74667 = CARTESIAN_POINT ( 'NONE',  ( -0.8801773607110991993, 42.85535201082150536, -2.915334737309923874 ) ) ;
#74668 = AXIS2_PLACEMENT_3D ( 'NONE', #26265, #241, #59714 ) ;
#74669 = CARTESIAN_POINT ( 'NONE',  ( 21.09922568453594849, 46.20696800326376064, 6.408140936763242479 ) ) ;
#74670 = CARTESIAN_POINT ( 'NONE',  ( -8.527530157486182816, -19.40773551566587685, -4.923371831947288335 ) ) ;
#74671 = ORIENTED_EDGE ( 'NONE', *, *, #7250, .T. ) ;
#74672 = CARTESIAN_POINT ( 'NONE',  ( 20.04068437667225666, 4.719743609177204924, 6.396802510829709298 ) ) ;
#74673 = VERTEX_POINT ( 'NONE', #98105 ) ;
#74674 = VERTEX_POINT ( 'NONE', #74085 ) ;
#74675 = DIRECTION ( 'NONE',  ( 1.000000000000000000, 0.000000000000000000, 0.000000000000000000 ) ) ;
#74676 = CARTESIAN_POINT ( 'NONE',  ( 6.204703633549690345, 45.76208216824729647, -14.16423886937410259 ) ) ;
#74678 = CARTESIAN_POINT ( 'NONE',  ( 7.361572987183169658, 49.96726448433410894, -9.846743663894592657 ) ) ;
#74677 = CARTESIAN_POINT ( 'NONE',  ( 12.63842701281683922, 24.55059781766745175, -9.846743663894590881 ) ) ;
#74679 = CARTESIAN_POINT ( 'NONE',  ( 0.5774900079438607392, 68.48035201082150536, 5.440088680355550821 ) ) ;
#74680 = EDGE_CURVE ( 'NONE', #18387, #31163, #65101, .T. ) ;
#74681 = LINE ( 'NONE', #73680, #83138 ) ;
#74682 = STYLED_ITEM ( 'NONE', ( #94686 ), #15201 ) ;
#74683 = CARTESIAN_POINT ( 'NONE',  ( 4.559911319644449179, 68.89701867748817676, 9.422509992056141925 ) ) ;
#74684 = CARTESIAN_POINT ( 'NONE',  ( 6.408140936763236262, 27.45696800326376419, -11.09922568453595026 ) ) ;
#74685 = VERTEX_POINT ( 'NONE', #74589 ) ;
#74686 = CARTESIAN_POINT ( 'NONE',  ( 22.26659068614894466, 28.88708216824730357, 7.082119434687054849 ) ) ;
#74687 = B_SPLINE_CURVE_WITH_KNOTS ( 'NONE', 3,
 ( #42266, #95758, #50750, #87746, #42753, #13231 ),
 .UNSPECIFIED., .F., .F.,
 ( 4, 2, 4 ),
 ( 3.409110551494648044E-05, 0.0004400426677367923179, 0.0008459942299586381553 ),
 .UNSPECIFIED. ) ;
#74688 = CARTESIAN_POINT ( 'NONE',  ( 16.40814093676324603, 27.45696800326375708, -11.09922568453594671 ) ) ;
#74689 = VERTEX_POINT ( 'NONE', #81590 ) ;
#74690 = CARTESIAN_POINT ( 'NONE',  ( 13.43411237798106583, 47.66530133659709634, -12.81628187352647252 ) ) ;
#74691 = AXIS2_PLACEMENT_3D ( 'NONE', #84642, #92143, #23668 ) ;
#74692 = CARTESIAN_POINT ( 'NONE',  ( 4.559911319644449179, 13.89701867748817321, 9.422509992056141925 ) ) ;
#74693 = CARTESIAN_POINT ( 'NONE',  ( 1.472469842513823179, 36.42559781766745175, 4.923371831947296329 ) ) ;
#74694 = CARTESIAN_POINT ( 'NONE',  ( -0.8801773607110991993, 7.855352010821504471, -2.915334737309923874 ) ) ;
#74695 = CARTESIAN_POINT ( 'NONE',  ( 13.34343830728399283, 0.5000000000000004441, 6.852200678592689442 ) ) ;
#74696 = CARTESIAN_POINT ( 'NONE',  ( 0.000000000000000000, 15.00000000000000000, 0.000000000000000000 ) ) ;
#74697 = CARTESIAN_POINT ( 'NONE',  ( 1.472469842513823179, 41.42559781766745886, 4.923371831947296329 ) ) ;
#74698 = CARTESIAN_POINT ( 'NONE',  ( 1.472469842513823179, 51.42559781766745886, 4.923371831947296329 ) ) ;
#74699 = VECTOR ( 'NONE', #42523, 1000.000000000000114 ) ;
#74701 = ORIENTED_EDGE ( 'NONE', *, *, #48492, .F. ) ;
#74700 = LINE ( 'NONE', #53672, #39304 ) ;
#74702 = FACE_OUTER_BOUND ( 'NONE', #3114, .T. ) ;
#74703 = LINE ( 'NONE', #59196, #1993 ) ;
#74704 = LINE ( 'NONE', #6214, #18012 ) ;
#74705 = FACE_OUTER_BOUND ( 'NONE', #61247, .T. ) ;
#74706 = CARTESIAN_POINT ( 'NONE',  ( 10.00000000000000178, 17.25893115100078745, 9.846743663894594434 ) ) ;
#74707 = DIRECTION ( 'NONE',  ( 0.000000000000000000, 0.000000000000000000, 1.000000000000000000 ) ) ;
#74708 = CARTESIAN_POINT ( 'NONE',  ( 13.43411237798106583, 37.66530133659708923, -12.81628187352647252 ) ) ;
#74709 = DIRECTION ( 'NONE',  ( -0.000000000000000000, -0.000000000000000000, -1.000000000000000000 ) ) ;
#74710 = VERTEX_POINT ( 'NONE', #7093 ) ;
#74711 = CARTESIAN_POINT ( 'NONE',  ( 0.1532563361054082862, 56.21726448433411605, 2.638427012816831674 ) ) ;
#74712 = CARTESIAN_POINT ( 'NONE',  ( -14.29541133317247414, 0.2306972965111896978, 4.345028136609434988 ) ) ;
#74713 = CARTESIAN_POINT ( 'NONE',  ( -0.3689425029237898834, 21.17874883491396432, -10.36894250292378850 ) ) ;
#74714 = CARTESIAN_POINT ( 'NONE',  ( 7.361572987183170547, 42.05059781766745886, 9.846743663894590881 ) ) ;
#74715 = CARTESIAN_POINT ( 'NONE',  ( 13.43411237798105340, 50.58196800326375353, 12.81628187352647963 ) ) ;
#74716 = CYLINDRICAL_SURFACE ( 'NONE', #27262, 6.999999999999995559 ) ;
#74717 = CARTESIAN_POINT ( 'NONE',  ( 7.361572987183170547, 2.050597817667451750, 9.846743663894590881 ) ) ;
#74718 = FACE_BOUND ( 'NONE', #32709, .T. ) ;
#74719 = CARTESIAN_POINT ( 'NONE',  ( 19.84674366389459266, 53.30059781766744464, 2.638427012816836559 ) ) ;
#74720 = CARTESIAN_POINT ( 'NONE',  ( 19.42250999205614193, 35.14701867748816966, 5.440088680355555262 ) ) ;
#74721 = EDGE_CURVE ( 'NONE', #31822, #1572, #43789, .T. ) ;
#74722 = CARTESIAN_POINT ( 'NONE',  ( 10.00000000000000178, 49.31368534415484106, 10.88017736071110342 ) ) ;
#74723 = VERTEX_POINT ( 'NONE', #35607 ) ;
#74724 = CARTESIAN_POINT ( 'NONE',  ( -9.724225243420933751, 2.502569995908613620, -5.657147814151106680 ) ) ;
#74725 = CARTESIAN_POINT ( 'NONE',  ( 12.91533473730992121, 19.52201867748816611, 10.88017736071110164 ) ) ;
#74727 = CARTESIAN_POINT ( 'NONE',  ( -0.8801773607111008646, 43.27201867748817676, 2.915334737309923430 ) ) ;
#74726 = CARTESIAN_POINT ( 'NONE',  ( 5.076628168052704559, 50.17559781766745886, -8.527530157486179263 ) ) ;
#74728 = FACE_OUTER_BOUND ( 'NONE', #97943, .T. ) ;
#74729 = CARTESIAN_POINT ( 'NONE',  ( 2.035157376598824452, 58.68868534415482685, 7.964842623401179544 ) ) ;
#74730 = CARTESIAN_POINT ( 'NONE',  ( 12.30000000000000249, 99.99999999999998579, 8.000000000000000000 ) ) ;
#74732 = DIRECTION ( 'NONE',  ( -0.000000000000000000, -0.000000000000000000, -1.000000000000000000 ) ) ;
#74731 = CARTESIAN_POINT ( 'NONE',  ( 19.42250999205614548, 25.98035201082150891, -5.440088680355545492 ) ) ;
#74733 = CARTESIAN_POINT ( 'NONE',  ( 1.472469842513823179, 10.59226448433411782, -4.923371831947296329 ) ) ;
#74734 = CARTESIAN_POINT ( 'NONE',  ( 18.52753015748618282, 28.92559781766745175, -4.923371831947291888 ) ) ;
#74735 =( NAMED_UNIT ( * ) SI_UNIT ( $, .STERADIAN. ) SOLID_ANGLE_UNIT ( ) );
#74736 = CARTESIAN_POINT ( 'NONE',  ( -14.16423886937410082, 16.80374883491397853, 4.336808689942017736E-15 ) ) ;
#74737 = CARTESIAN_POINT ( 'NONE',  ( 12.63842701281683922, 59.55059781766744464, -9.846743663894590881 ) ) ;
#74739 = DIRECTION ( 'NONE',  ( 0.000000000000000000, 0.000000000000000000, 1.000000000000000000 ) ) ;
#74738 = CARTESIAN_POINT ( 'NONE',  ( -4.164238869374099927, 67.01208216824728936, 3.795296366450308767 ) ) ;
#74740 = DIRECTION ( 'NONE',  ( 1.000000000000000000, 0.000000000000000000, 0.000000000000000000 ) ) ;
#74741 = CARTESIAN_POINT ( 'NONE',  ( 13.79529636645030344, 3.262082168247301350, 14.16423886937410614 ) ) ;
#74742 = CARTESIAN_POINT ( 'NONE',  ( -4.164238869374099039, 46.80374883491397497, 8.674139862899312516E-16 ) ) ;
#74743 = AXIS2_PLACEMENT_3D ( 'NONE', #82414, #13938, #59907 ) ;
#74744 = CARTESIAN_POINT ( 'NONE',  ( 3.591859063236761518, 4.956968003263753531, 11.09922568453594849 ) ) ;
#74745 = ORIENTED_EDGE ( 'NONE', *, *, #96468, .T. ) ;
#74746 = CARTESIAN_POINT ( 'NONE',  ( 19.84674366389459621, 8.508931151000785675, 7.409399052514197653E-17 ) ) ;
#74747 = ADVANCED_FACE ( 'NONE', ( #89596 ), #62564, .T. ) ;
#74748 = CARTESIAN_POINT ( 'NONE',  ( 10.00000000000000178, 9.313685344154839285, 10.88017736071110342 ) ) ;
#74749 = CARTESIAN_POINT ( 'NONE',  ( 19.84674366389459266, 53.30059781766744464, 2.638427012816836559 ) ) ;
#74751 = LINE ( 'NONE', #51262, #39112 ) ;
#74750 = CARTESIAN_POINT ( 'NONE',  ( 6.432108699068923130, -88.20011490510430008, 2.750000000000000000 ) ) ;
#74752 = DIRECTION ( 'NONE',  ( 0.000000000000000000, 1.000000000000000000, -0.000000000000000000 ) ) ;
#74753 = CARTESIAN_POINT ( 'NONE',  ( 2.913501739333662854, 4.325554204331052541E-16, 14.20427779279537184 ) ) ;
#74754 = CARTESIAN_POINT ( 'NONE',  ( 3.591859063236761518, 24.95696800326375353, 11.09922568453594849 ) ) ;
#74755 = CARTESIAN_POINT ( 'NONE',  ( 10.00000000000000000, 29.75893115100078745, -9.846743663894594434 ) ) ;
#74757 = ORIENTED_EDGE ( 'NONE', *, *, #47359, .T. ) ;
#74756 = EDGE_CURVE ( 'NONE', #73854, #37098, #97723, .T. ) ;
#74758 = CARTESIAN_POINT ( 'NONE',  ( 5.076628168052703671, 11.84226448433411960, 8.527530157486179263 ) ) ;
#74759 = CARTESIAN_POINT ( 'NONE',  ( 9.479665769801981057, -19.63627307883762185, -4.000000000000000000 ) ) ;
#74760 = CARTESIAN_POINT ( 'NONE',  ( -46.75594628505023564, 100.8419086298434877, -9.092420010817928500 ) ) ;
#74761 = CARTESIAN_POINT ( 'NONE',  ( 12.91533473730993009, 11.60535201082150536, -10.88017736071109987 ) ) ;
#74762 = CARTESIAN_POINT ( 'NONE',  ( 2.917880565312950480, 45.97041550158063927, -12.26659068614894821 ) ) ;
#74763 = AXIS2_PLACEMENT_3D ( 'NONE', #65060, #88070, #25627 ) ;
#74764 = CARTESIAN_POINT ( 'NONE',  ( -0.8801773607110991993, 67.85535201082151957, -2.915334737309923874 ) ) ;
#74765 = DIRECTION ( 'NONE',  ( 0.000000000000000000, 0.000000000000000000, -1.000000000000000000 ) ) ;
#74766 = CARTESIAN_POINT ( 'NONE',  ( 18.52753015748617571, 23.09226448433411960, 4.923371831947298993 ) ) ;
#74767 = CARTESIAN_POINT ( 'NONE',  ( 20.88017736071110519, 5.563685344154837509, 2.639326808657452039E-16 ) ) ;
#74768 = CARTESIAN_POINT ( 'NONE',  ( 7.361572987183169658, 4.967264484334119601, -9.846743663894592657 ) ) ;
#74769 = FACE_OUTER_BOUND ( 'NONE', #46875, .T. ) ;
#74770 = CARTESIAN_POINT ( 'NONE',  ( 5.076628168052703671, 41.84226448433411605, 8.527530157486179263 ) ) ;
#74771 = CARTESIAN_POINT ( 'NONE',  ( 10.00000000000000000, 36.81368534415484106, -10.88017736071110342 ) ) ;
#74772 = VECTOR ( 'NONE', #22779, 1000.000000000000114 ) ;
#74773 = MECHANICAL_DESIGN_GEOMETRIC_PRESENTATION_REPRESENTATION (  '', ( #34794 ), #15697 ) ;
#74774 = ORIENTED_EDGE ( 'NONE', *, *, #77311, .T. ) ;
#74775 = CARTESIAN_POINT ( 'NONE',  ( 0.6178305044545838731, 59.74863466993041783, 9.382169495545420901 ) ) ;
#74776 = CARTESIAN_POINT ( 'NONE',  ( 9.742785792574936821, 5.005135511184879427, 5.624999999999997335 ) ) ;
#74777 = CARTESIAN_POINT ( 'NONE',  ( 10.00000000000000178, 7.258931151000785675, 9.846743663894594434 ) ) ;
#74778 = CARTESIAN_POINT ( 'NONE',  ( 22.81628187352648496, 41.83196800326375353, -3.434112377981050290 ) ) ;
#74780 = CARTESIAN_POINT ( 'NONE',  ( 5.076628168052703671, 36.84226448433412315, 8.527530157486179263 ) ) ;
#74779 = CARTESIAN_POINT ( 'NONE',  ( 7.084665262690076126, 9.105352010821503583, 10.88017736071109987 ) ) ;
#74781 = CARTESIAN_POINT ( 'NONE',  ( 0.4195498155886338565, 0.5000000000000023315, 10.00000000000000000 ) ) ;
#74782 = DIRECTION ( 'NONE',  ( 0.000000000000000000, 1.000000000000000000, 0.000000000000000000 ) ) ;
#74783 = CARTESIAN_POINT ( 'NONE',  ( -4.164238869374099927, 22.01208216824730357, 3.795296366450308767 ) ) ;
#74784 = CARTESIAN_POINT ( 'NONE',  ( 2.917880565312948704, 47.63708216824730357, 12.26659068614894643 ) ) ;
#74785 = CARTESIAN_POINT ( 'NONE',  ( 14.92337183194729633, 42.67559781766745886, 8.527530157486181039 ) ) ;
#74786 = CARTESIAN_POINT ( 'NONE',  ( 4.864290147396342689, -17.52197929138388588, -2.500000000000000000 ) ) ;
#74787 = CARTESIAN_POINT ( 'NONE',  ( 10.00000000000000178, 34.31368534415484106, 10.88017736071110342 ) ) ;
#74788 = CARTESIAN_POINT ( 'NONE',  ( 5.076628168052703671, 1.842264484334118047, 8.527530157486179263 ) ) ;
#74789 = CARTESIAN_POINT ( 'NONE',  ( -3.628626192037550435, -3.642031182890759666, 3.999999999999193090 ) ) ;
#74790 = ORIENTED_EDGE ( 'NONE', *, *, #67432, .F. ) ;
#74791 = CARTESIAN_POINT ( 'NONE',  ( 22.81628187352647785, 56.62363466993042493, 6.195893100308588602E-16 ) ) ;
#74792 = EDGE_LOOP ( 'NONE', ( #26378, #94340, #71122, #54070, #85598 ) ) ;
#74793 = CARTESIAN_POINT ( 'NONE',  ( 19.42250999205614548, 60.98035201082151247, -5.440088680355545492 ) ) ;
#74794 = VERTEX_POINT ( 'NONE', #68089 ) ;
#74795 = CARTESIAN_POINT ( 'NONE',  ( 17.08211943468705840, 10.13708216824730179, -12.26659068614894466 ) ) ;
#74796 = CARTESIAN_POINT ( 'NONE',  ( 5.076628168052704559, 10.17559781766745175, -8.527530157486179263 ) ) ;
#74797 = EDGE_CURVE ( 'NONE', #76544, #46091, #43364, .T. ) ;
#74798 = EDGE_LOOP ( 'NONE', ( #4493, #21855, #57447, #56245 ) ) ;
#74799 = CARTESIAN_POINT ( 'NONE',  ( 17.96484262340118221, 14.93868534415483751, 7.964842623401181321 ) ) ;
#74800 = EDGE_LOOP ( 'NONE', ( #38450, #37704, #94608, #7203 ) ) ;
#74801 = CARTESIAN_POINT ( 'NONE',  ( 0.5774900079438607392, 33.48035201082150536, 5.440088680355550821 ) ) ;
#74802 =( NAMED_UNIT ( * ) SI_UNIT ( $, .STERADIAN. ) SOLID_ANGLE_UNIT ( ) );
#74803 = ORIENTED_EDGE ( 'NONE', *, *, #92438, .T. ) ;
#74804 = EDGE_CURVE ( 'NONE', #28677, #35851, #30066, .T. ) ;
#74805 = CARTESIAN_POINT ( 'NONE',  ( 5.076628168052704559, 60.17559781766745175, -8.527530157486179263 ) ) ;
#74806 = VERTEX_POINT ( 'NONE', #97129 ) ;
#74807 = CARTESIAN_POINT ( 'NONE',  ( 7.084665262690076126, 69.10535201082151957, 10.88017736071109987 ) ) ;
#74808 = CARTESIAN_POINT ( 'NONE',  ( 19.84674366389459621, 63.50893115100078745, 7.409399052514197653E-17 ) ) ;
#74810 = CARTESIAN_POINT ( 'NONE',  ( 0.1922240491738455570, 58.18878173731742010, 6.499999999999968914 ) ) ;
#74809 = CARTESIAN_POINT ( 'NONE',  ( 0.5774900079438590739, 22.64701867748817321, -5.440088680355550821 ) ) ;
#74811 = CARTESIAN_POINT ( 'NONE',  ( 0.5774900079438590739, 67.64701867748817676, -5.440088680355550821 ) ) ;
#74812 = CARTESIAN_POINT ( 'NONE',  ( -0.8801773607110991993, 12.85535201082150358, -2.915334737309923874 ) ) ;
#74813 = AXIS2_PLACEMENT_3D ( 'NONE', #39880, #1905, #75904 ) ;
#74814 = ORIENTED_EDGE ( 'NONE', *, *, #50608, .T. ) ;
#74815 = CARTESIAN_POINT ( 'NONE',  ( 10.00000000000000000, 52.87363466993041783, -12.81628187352647608 ) ) ;
#74816 = CARTESIAN_POINT ( 'NONE',  ( 15.44008868035555260, 49.73035201082150536, 9.422509992056143702 ) ) ;
#74817 = CARTESIAN_POINT ( 'NONE',  ( -46.94000000000000483, 101.3580217190410337, -7.614242055628325012 ) ) ;
#74818 = CARTESIAN_POINT ( 'NONE',  ( 0.6178305044545838731, 49.74863466993041072, 9.382169495545420901 ) ) ;
#74819 = CARTESIAN_POINT ( 'NONE',  ( 10.00000000000000178, 44.31368534415484106, 10.88017736071110342 ) ) ;
#74820 = CARTESIAN_POINT ( 'NONE',  ( 0.1532563361054083140, 56.00893115100078745, 1.131784320476157264E-15 ) ) ;
#74821 = CARTESIAN_POINT ( 'NONE',  ( 19.50000000000000711, 105.0000000000000000, -4.500000000000000888 ) ) ;
#74822 = VECTOR ( 'NONE', #87428, 1000.000000000000000 ) ;
#74823 = CARTESIAN_POINT ( 'NONE',  ( 18.52753015748617571, 18.09226448433411960, 4.923371831947298993 ) ) ;
#74824 = CARTESIAN_POINT ( 'NONE',  ( 10.00000000000000178, 0.3736346699304200492, 12.81628187352647608 ) ) ;
#74826 = CARTESIAN_POINT ( 'NONE',  ( 7.361572987183169658, 64.96726448433412315, -9.846743663894592657 ) ) ;
#74825 = DIRECTION ( 'NONE',  ( 1.000000000000000000, 0.000000000000000000, 0.000000000000000000 ) ) ;
#74827 = CARTESIAN_POINT ( 'NONE',  ( 12.91533473730992121, 39.52201867748817676, 10.88017736071110164 ) ) ;
#74828 = CARTESIAN_POINT ( 'NONE',  ( 0.1532563361054082862, 46.21726448433411605, 2.638427012816831674 ) ) ;
#74829 = DIRECTION ( 'NONE',  ( 1.000000000000000000, 0.000000000000000000, 0.000000000000000000 ) ) ;
#74831 = CARTESIAN_POINT ( 'NONE',  ( 7.361572987183169658, 19.96726448433411960, -9.846743663894592657 ) ) ;
#74830 =( GEOMETRIC_REPRESENTATION_CONTEXT ( 3 ) GLOBAL_UNCERTAINTY_ASSIGNED_CONTEXT ( ( #41353 ) ) GLOBAL_UNIT_ASSIGNED_CONTEXT ( ( #84750, #17736, #70740 ) ) REPRESENTATION_CONTEXT ( 'NONE', 'WORKASPACE' ) );
#74832 = CARTESIAN_POINT ( 'NONE',  ( 19.84674366389459621, 8.508931151000785675, 7.409399052514197653E-17 ) ) ;
#74833 = EDGE_CURVE ( 'NONE', #87186, #14534, #37101, .T. ) ;
#74835 = ORIENTED_EDGE ( 'NONE', *, *, #4128, .T. ) ;
#74834 = CARTESIAN_POINT ( 'NONE',  ( 13.43411237798106583, 2.665301336597086568, -12.81628187352647252 ) ) ;
#74836 = CIRCLE ( 'NONE', #38182, 15.00000000000000000 ) ;
#74837 = SURFACE_STYLE_FILL_AREA ( #57856 ) ;
#74838 = FACE_OUTER_BOUND ( 'NONE', #89021, .T. ) ;
#74839 = CARTESIAN_POINT ( 'NONE',  ( 0.1532563361054100626, 60.80059781766744464, -2.638427012816831230 ) ) ;
#74840 = CARTESIAN_POINT ( 'NONE',  ( 21.09922568453595559, 47.04030133659708923, -6.408140936763230044 ) ) ;
#74841 = CARTESIAN_POINT ( 'NONE',  ( 2.791683348922240793, 36.63393115100078035, 7.208316651077764092 ) ) ;
#74842 = CARTESIAN_POINT ( 'NONE',  ( 5.113979357139876392, -17.50950876244384702, -2.500000000001608491 ) ) ;
#74844 = EDGE_CURVE ( 'NONE', #24915, #37516, #40251, .T. ) ;
#74843 = CARTESIAN_POINT ( 'NONE',  ( 0.5774900079438607392, 8.480352010821505360, 5.440088680355550821 ) ) ;
#74845 = CARTESIAN_POINT ( 'NONE',  ( 2.791683348922240793, 31.63393115100078745, 7.208316651077764092 ) ) ;
#74846 = ORIENTED_EDGE ( 'NONE', *, *, #8053, .T. ) ;
#74847 = CARTESIAN_POINT ( 'NONE',  ( 3.969999999999999751, 36.75000000000000000, 2.500000000000000000 ) ) ;
#74848 = CARTESIAN_POINT ( 'NONE',  ( 19.42250999205614193, 5.147018677488171434, 5.440088680355555262 ) ) ;
#74849 = CARTESIAN_POINT ( 'NONE',  ( -12.16982443903231292, 90.48687232357865184, -7.214476785723133112 ) ) ;
#74850 = CARTESIAN_POINT ( 'NONE',  ( -0.8801773607110991993, 22.85535201082150181, -2.915334737309923874 ) ) ;
#74851 = CARTESIAN_POINT ( 'NONE',  ( -4.164238869374099927, 47.01208216824729647, 3.795296366450308767 ) ) ;
#74853 = CARTESIAN_POINT ( 'NONE',  ( 3.969999999999999751, 36.75000000000000000, 2.750000000000000000 ) ) ;
#74852 = CARTESIAN_POINT ( 'NONE',  ( -4.164238869374099927, 57.01208216824731068, 3.795296366450308767 ) ) ;
#74854 =( LENGTH_UNIT ( ) NAMED_UNIT ( * ) SI_UNIT ( .MILLI., .METRE. ) );
#74855 = CARTESIAN_POINT ( 'NONE',  ( 0.1532563361054082862, 11.21726448433411605, 2.638427012816831674 ) ) ;
#74856 = CARTESIAN_POINT ( 'NONE',  ( 14.92337183194729633, 62.67559781766745886, 8.527530157486181039 ) ) ;
#74857 = VERTEX_POINT ( 'NONE', #67095 ) ;
#74858 = SURFACE_STYLE_FILL_AREA ( #11899 ) ;
#74859 = CARTESIAN_POINT ( 'NONE',  ( 0.1532563361054082862, 56.21726448433411605, 2.638427012816831674 ) ) ;
#74860 = LINE ( 'NONE', #82856, #33142 ) ;
#74861 = CARTESIAN_POINT ( 'NONE',  ( 12.63842701281683034, 62.46726448433410894, 9.846743663894596210 ) ) ;
#74862 = CARTESIAN_POINT ( 'NONE',  ( -2.266590686148945544, 12.22041550158063394, 7.082119434687048631 ) ) ;
#74863 = CARTESIAN_POINT ( 'NONE',  ( 10.00000000000000000, 24.75893115100078745, -9.846743663894594434 ) ) ;
#74864 = ORIENTED_EDGE ( 'NONE', *, *, #81198, .F. ) ;
#74865 = CARTESIAN_POINT ( 'NONE',  ( -4.164238869374098151, 46.59541550158063927, -3.795296366450310543 ) ) ;
#74866 = CARTESIAN_POINT ( 'NONE',  ( 18.52753015748617571, 3.092264484334118269, 4.923371831947298993 ) ) ;
#74868 = CARTESIAN_POINT ( 'NONE',  ( 3.469446951953614189E-15, 9.171802177851546389, 11.25000000000000355 ) ) ;
#74867 = DIRECTION ( 'NONE',  ( 0.02970531260815257105, -0.9995586998285053149, 0.000000000000000000 ) ) ;
#74869 = CARTESIAN_POINT ( 'NONE',  ( -0.8801773607111009756, 38.06368534415484106, 1.068504757029289695E-15 ) ) ;
#74870 = CARTESIAN_POINT ( 'NONE',  ( 16.40814093676323893, 40.79030133659708923, 11.09922568453595026 ) ) ;
#74871 = CARTESIAN_POINT ( 'NONE',  ( 0.6178305044545838731, 34.74863466993042493, 9.382169495545420901 ) ) ;
#74872 = CARTESIAN_POINT ( 'NONE',  ( 10.00000000000000178, 60.37363466993041783, 12.81628187352647608 ) ) ;
#74874 = ORIENTED_EDGE ( 'NONE', *, *, #43686, .T. ) ;
#74873 = EDGE_CURVE ( 'NONE', #23769, #1162, #25835, .T. ) ;
#74875 = FACE_OUTER_BOUND ( 'NONE', #19598, .T. ) ;
#74876 = CARTESIAN_POINT ( 'NONE',  ( 4.999999999999999112, 0.000000000000000000, -6.000000000000000000 ) ) ;
#74877 = CARTESIAN_POINT ( 'NONE',  ( -4.164238869374099927, 37.01208216824731068, 3.795296366450308767 ) ) ;
#74878 = CARTESIAN_POINT ( 'NONE',  ( 0.5774900079438590739, 2.647018677488170990, -5.440088680355550821 ) ) ;
#74879 = CARTESIAN_POINT ( 'NONE',  ( 20.88017736071110875, 25.77201867748816966, -2.915334737309920765 ) ) ;
#74880 = LINE ( 'NONE', #42910, #76559 ) ;
#74881 = AXIS2_PLACEMENT_3D ( 'NONE', #95165, #42668, #18698 ) ;
#74882 = DIRECTION ( 'NONE',  ( -0.000000000000000000, -1.000000000000000000, -0.000000000000000000 ) ) ;
#74883 = CARTESIAN_POINT ( 'NONE',  ( 2.035157376598824452, 53.68868534415484817, 7.964842623401179544 ) ) ;
#74884 = CARTESIAN_POINT ( 'NONE',  ( 7.084665262690076126, 49.10535201082149825, 10.88017736071109987 ) ) ;
#74885 = CARTESIAN_POINT ( 'NONE',  ( 0.6178305044545818747, 28.49863466993041783, -9.382169495545419124 ) ) ;
#74886 = CARTESIAN_POINT ( 'NONE',  ( 66.76470751278411342, 44.49999999999998579, -9.500000000000000000 ) ) ;
#74887 = CARTESIAN_POINT ( 'NONE',  ( 7.361572987183169658, 19.96726448433411960, -9.846743663894592657 ) ) ;
#74888 = CARTESIAN_POINT ( 'NONE',  ( 4.559911319644449179, 57.23035201082150536, -9.422509992056141925 ) ) ;
#74889 = CARTESIAN_POINT ( 'NONE',  ( 0.6178305044545818747, 18.49863466993041428, -9.382169495545419124 ) ) ;
#74890 = CARTESIAN_POINT ( 'NONE',  ( -0.8801773607111009756, 43.27201867748816966, 2.915334737309923874 ) ) ;
#74891 = CARTESIAN_POINT ( 'NONE',  ( 20.88017736071110519, 10.56368534415483751, 2.639326808657452039E-16 ) ) ;
#74892 = CARTESIAN_POINT ( 'NONE',  ( 2.791683348922237240, 35.38393115100079456, -7.208316651077763204 ) ) ;
#74893 = CARTESIAN_POINT ( 'NONE',  ( 0.6178305044545818747, 63.49863466993043204, -9.382169495545419124 ) ) ;
#74895 =( NAMED_UNIT ( * ) SI_UNIT ( $, .STERADIAN. ) SOLID_ANGLE_UNIT ( ) );
#74894 = CARTESIAN_POINT ( 'NONE',  ( 14.92337183194729633, 12.67559781766745353, 8.527530157486181039 ) ) ;
#74896 = CARTESIAN_POINT ( 'NONE',  ( 24.16423886937410614, 4.512082168247300906, -3.795296366450302550 ) ) ;
#74897 = CARTESIAN_POINT ( 'NONE',  ( 2.603489959281613420, 35.43575266056827644, -6.500000000000031086 ) ) ;
#74898 = CARTESIAN_POINT ( 'NONE',  ( 20.88017736071110519, 15.56368534415483751, 2.639326808657452039E-16 ) ) ;
#74899 = CARTESIAN_POINT ( 'NONE',  ( 7.084665262690076126, 2.022018677488170990, -10.88017736071110164 ) ) ;
#74900 = CARTESIAN_POINT ( 'NONE',  ( 1.472469842513823179, 50.59226448433411605, -4.923371831947296329 ) ) ;
#74901 = B_SPLINE_CURVE_WITH_KNOTS ( 'NONE', 3,
 ( #13994, #43967, #59962, #44469, #82970, #74471 ),
 .UNSPECIFIED., .F., .F.,
 ( 4, 2, 4 ),
 ( 3.409110551495225382E-05, 0.0004400426677367789280, 0.0008459942299586055208 ),
 .UNSPECIFIED. ) ;
#74902 = COLOUR_RGB ( '', 0.72549020, 0.75294118, 0.79215686) ;
#74903 = CARTESIAN_POINT ( 'NONE',  ( 0.5774900079438590739, 37.64701867748817676, -5.440088680355550821 ) ) ;
#74904 = CARTESIAN_POINT ( 'NONE',  ( -0.8801773607111009756, 18.06368534415484106, 1.068504757029289695E-15 ) ) ;
#74905 = ORIENTED_EDGE ( 'NONE', *, *, #41909, .T. ) ;
#74906 = CARTESIAN_POINT ( 'NONE',  ( 2.035157376598822676, 27.43868534415483396, -7.964842623401177768 ) ) ;
#74908 = CARTESIAN_POINT ( 'NONE',  ( 16.40814093676324603, 42.45696800326375353, -11.09922568453594671 ) ) ;
#74907 = MECHANICAL_DESIGN_GEOMETRIC_PRESENTATION_REPRESENTATION (  '', ( #46164 ), #89252 ) ;
#74909 = EDGE_CURVE ( 'NONE', #56172, #17129, #39147, .T. ) ;
#74910 = CARTESIAN_POINT ( 'NONE',  ( 7.084665262690076126, 34.10535201082151247, 10.88017736071109987 ) ) ;
#74912 = CARTESIAN_POINT ( 'NONE',  ( 10.00000000000000000, 41.81368534415484106, -10.88017736071110342 ) ) ;
#74911 = CARTESIAN_POINT ( 'NONE',  ( 0.1532563361054100626, 45.80059781766745175, -2.638427012816831230 ) ) ;
#74913 = CIRCLE ( 'NONE', #19034, 15.00000000000000000 ) ;
#74914 = ORIENTED_EDGE ( 'NONE', *, *, #85954, .T. ) ;
#74915 = CARTESIAN_POINT ( 'NONE',  ( 10.00000000000000000, 59.75893115100078745, -9.846743663894594434 ) ) ;
#74916 = CARTESIAN_POINT ( 'NONE',  ( 10.00000000000000000, 36.81368534415484106, -10.88017736071110342 ) ) ;
#74917 = CARTESIAN_POINT ( 'NONE',  ( 0.1532563361054083140, 66.00893115100079456, 1.131784320476157264E-15 ) ) ;
#74918 =( NAMED_UNIT ( * ) SI_UNIT ( $, .STERADIAN. ) SOLID_ANGLE_UNIT ( ) );
#74919 = DIRECTION ( 'NONE',  ( 0.000000000000000000, 0.000000000000000000, -1.000000000000000000 ) ) ;
#74920 = CARTESIAN_POINT ( 'NONE',  ( 24.16423886937410614, 44.30374883491397497, 8.672049930838204340E-16 ) ) ;
#74921 = CARTESIAN_POINT ( 'NONE',  ( 0.5774900079438607392, 58.48035201082151247, 5.440088680355550821 ) ) ;
#74922 = DIRECTION ( 'NONE',  ( 0.000000000000000000, 1.000000000000000000, 0.000000000000000000 ) ) ;
#74923 = DIRECTION ( 'NONE',  ( 1.000000000000000000, 0.000000000000000000, 0.000000000000000000 ) ) ;
#74924 = CARTESIAN_POINT ( 'NONE',  ( 1.472469842513823179, 56.42559781766745886, 4.923371831947296329 ) ) ;
#74925 = CARTESIAN_POINT ( 'NONE',  ( 0.000000000000000000, 0.5000000000000004441, 0.000000000000000000 ) ) ;
#74926 = CARTESIAN_POINT ( 'NONE',  ( 2.791683348922237240, 25.38393115100078390, -7.208316651077763204 ) ) ;
#74927 = ORIENTED_EDGE ( 'NONE', *, *, #28407, .T. ) ;
#74928 = CARTESIAN_POINT ( 'NONE',  ( 5.076628168052704559, 25.17559781766745175, -8.527530157486179263 ) ) ;
#74929 = CARTESIAN_POINT ( 'NONE',  ( -5.204170427930421283E-15, -22.12636533006957507, -12.81628187352647608 ) ) ;
#74930 = CARTESIAN_POINT ( 'NONE',  ( 19.42250999205614548, 20.98035201082150891, -5.440088680355545492 ) ) ;
#74931 = CARTESIAN_POINT ( 'NONE',  ( 0.1532563361054100626, 25.80059781766744820, -2.638427012816831230 ) ) ;
#74932 = CARTESIAN_POINT ( 'NONE',  ( 10.00000000000000000, 12.87363466993042138, -12.81628187352647608 ) ) ;
#74933 = DIRECTION ( 'NONE',  ( -0.08715574274765139351, -0.9961946980917461003, 0.000000000000000000 ) ) ;
#74935 = CARTESIAN_POINT ( 'NONE',  ( 4.559911319644449179, 7.230352010821504471, -9.422509992056141925 ) ) ;
#74934 = CARTESIAN_POINT ( 'NONE',  ( 2.035157376598824452, 33.68868534415484106, 7.964842623401179544 ) ) ;
#74936 = CARTESIAN_POINT ( 'NONE',  ( -4.164238869374099927, 47.01208216824729647, 3.795296366450308767 ) ) ;
#74937 = AXIS2_PLACEMENT_3D ( 'NONE', #94849, #72826, #4364 ) ;
#74938 = CARTESIAN_POINT ( 'NONE',  ( -43.49071039140426365, 106.3659493636330069, 5.092460419850055153 ) ) ;
#74939 = EDGE_LOOP ( 'NONE', ( #69483, #47357, #54413, #60558, #15429, #17188 ) ) ;
#74940 = CARTESIAN_POINT ( 'NONE',  ( -1.099225684535947600, 9.540301336597087456, 6.408140936763237150 ) ) ;
#74941 = CARTESIAN_POINT ( 'NONE',  ( 17.96484262340118221, 4.938685344154837509, 7.964842623401181321 ) ) ;
#74942 = CARTESIAN_POINT ( 'NONE',  ( 10.00000000000000178, 44.31368534415484106, 10.88017736071110342 ) ) ;
#74943 = CARTESIAN_POINT ( 'NONE',  ( 9.779999999999988702, 27.00436609429084811, 3.000000000000000000 ) ) ;
#74944 = VERTEX_POINT ( 'NONE', #51102 ) ;
#74945 = VECTOR ( 'NONE', #20381, 1000.000000000000000 ) ;
#74946 = CARTESIAN_POINT ( 'NONE',  ( 12.91533473730993009, 51.60535201082149825, -10.88017736071109987 ) ) ;
#74947 = CARTESIAN_POINT ( 'NONE',  ( 14.92337183194729633, 32.67559781766745175, 8.527530157486181039 ) ) ;
#74948 = CARTESIAN_POINT ( 'NONE',  ( 0.1532563361054083140, 21.00893115100078745, 1.131784320476157264E-15 ) ) ;
#74949 = CARTESIAN_POINT ( 'NONE',  ( 18.52753015748618282, 8.925597817667451750, -4.923371831947291888 ) ) ;
#74951 = CARTESIAN_POINT ( 'NONE',  ( 13.43411237798106583, 37.66530133659708923, -12.81628187352647252 ) ) ;
#74950 = CARTESIAN_POINT ( 'NONE',  ( -7.079903288618116797, -69.52484394646381816, 2.750000000000000000 ) ) ;
#74953 = CARTESIAN_POINT ( 'NONE',  ( -0.1503990784575242878, 34.24884699246889141, -6.262539305110083276 ) ) ;
#74952 = CARTESIAN_POINT ( 'NONE',  ( 12.91533473730993009, 66.60535201082150536, -10.88017736071109987 ) ) ;
#74954 = CARTESIAN_POINT ( 'NONE',  ( 10.89309004150372751, -97.65096242295280149, 3.749999999996625810 ) ) ;
#74956 = ORIENTED_EDGE ( 'NONE', *, *, #49763, .T. ) ;
#74955 = CARTESIAN_POINT ( 'NONE',  ( 14.92337183194729633, 27.67559781766745530, 8.527530157486181039 ) ) ;
#74957 = EDGE_CURVE ( 'NONE', #95213, #25245, #19471, .T. ) ;
#74958 = CARTESIAN_POINT ( 'NONE',  ( 22.81628187352647785, 51.62363466993042493, 6.195893100308588602E-16 ) ) ;
#74959 = DIRECTION ( 'NONE',  ( -0.000000000000000000, -1.000000000000000000, -0.000000000000000000 ) ) ;
#74960 = CARTESIAN_POINT ( 'NONE',  ( -2.816281873526473856, -0.8763653300695799508, 9.499525473075851096E-16 ) ) ;
#74961 = EDGE_CURVE ( 'NONE', #17245, #36257, #8278, .T. ) ;
#74963 = EDGE_CURVE ( 'NONE', #67464, #44301, #84075, .T. ) ;
#74962 = CARTESIAN_POINT ( 'NONE',  ( 24.16423886937410614, 39.30374883491396787, 8.672049930838204340E-16 ) ) ;
#74964 = CARTESIAN_POINT ( 'NONE',  ( -14.64921366071501119, 0.04962891916449908153, 1.748670679918064241 ) ) ;
#74965 = CARTESIAN_POINT ( 'NONE',  ( 10.00000000000000178, 28.05374883491396787, 14.16423886937410082 ) ) ;
#74966 = CARTESIAN_POINT ( 'NONE',  ( 22.26659068614894466, 43.88708216824729647, 7.082119434687054849 ) ) ;
#74967 = CARTESIAN_POINT ( 'NONE',  ( 2.917880565312950480, 5.970415501580634832, -12.26659068614894821 ) ) ;
#74969 = CARTESIAN_POINT ( 'NONE',  ( -13.68546037613094057, 90.96609652458319317, -7.941826699654800592 ) ) ;
#74968 = CARTESIAN_POINT ( 'NONE',  ( 24.16423886937410614, 14.51208216824730179, -3.795296366450302550 ) ) ;
#74970 = CARTESIAN_POINT ( 'NONE',  ( 0.5774900079438607392, 43.48035201082151247, 5.440088680355550821 ) ) ;
#74971 = CARTESIAN_POINT ( 'NONE',  ( 8.629999999999995453, 41.24999999999999289, -6.250000000000000000 ) ) ;
#74972 = CARTESIAN_POINT ( 'NONE',  ( 7.361572987183169658, 24.96726448433412315, -9.846743663894592657 ) ) ;
#74974 = CARTESIAN_POINT ( 'NONE',  ( 2.791683348922240793, 26.63393115100078745, 7.208316651077764092 ) ) ;
#74973 = CARTESIAN_POINT ( 'NONE',  ( 20.88017736071110164, 65.35535201082150536, 2.915334737309930979 ) ) ;
#74975 = EDGE_CURVE ( 'NONE', #32046, #48910, #40049, .T. ) ;
#74976 = CARTESIAN_POINT ( 'NONE',  ( 2.035157376598822676, 22.43868534415483396, -7.964842623401177768 ) ) ;
#74977 = CARTESIAN_POINT ( 'NONE',  ( 19.38216949554541557, 52.24863466993041072, -9.382169495545420901 ) ) ;
#74978 = CARTESIAN_POINT ( 'NONE',  ( 70.19910379943081580, 41.67447916666664298, -10.00000000000000000 ) ) ;
#74979 = DIRECTION ( 'NONE',  ( 1.257402221000611116E-16, -1.000000000000000000, 0.000000000000000000 ) ) ;
#74980 = CARTESIAN_POINT ( 'NONE',  ( 19.84674366389459621, 28.50893115100078745, 7.409399052514197653E-17 ) ) ;
#74981 = CARTESIAN_POINT ( 'NONE',  ( -1.099225684535947600, 39.54030133659708923, 6.408140936763237150 ) ) ;
#74982 = CARTESIAN_POINT ( 'NONE',  ( -3.795296366450322534, -14.23791783175269110, -14.16423886937409904 ) ) ;
#74983 =( BOUNDED_SURFACE ( )  B_SPLINE_SURFACE ( 3, 2, ( 
 ( #7842, #16321, #98863 ),
 ( #38339, #22352, #31302 ),
 ( #53320, #44825, #84336 ),
 ( #75331, #6844, #68834 ),
 ( #69322, #67849, #52827 ),
 ( #76810, #98367, #45839 ),
 ( #82835, #83334, #92310 ),
 ( #45331, #75830, #46323 ),
 ( #365, #74842, #30317 ),
 ( #30813, #7351, #61803 ),
 ( #15354, #29823, #15838 ),
 ( #23342, #61312, #37852 ),
 ( #84815, #53824, #6343 ),
 ( #68342, #91318, #8325 ),
 ( #60819, #22846, #38829 ),
 ( #843, #60333, #36854 ),
 ( #67345, #97871, #29331 ),
 ( #90322, #21860, #52340 ) ),
 .UNSPECIFIED., .F., .F., .F. ) 
 B_SPLINE_SURFACE_WITH_KNOTS ( ( 4, 2, 2, 2, 2, 2, 2, 2, 4 ),
 ( 3, 3 ),
 ( 0.000000000000000000, 0.002783459421176835875, 0.005566918842353671751, 0.01113383768470734350, 0.02226767536941468700, 0.04453535073882937401, 0.06680302610824406795, 0.07793686379295140798, 0.08907070147765874801 ),
 ( 0.000000000000000000, 1.000000000000000000 ),
 .UNSPECIFIED. ) 
 GEOMETRIC_REPRESENTATION_ITEM ( )  RATIONAL_B_SPLINE_SURFACE ( (
 ( 1.000000000000000000, 0.7071067811865482389, 1.000000000000000000),
 ( 1.000000000000000000, 0.7071067811865482389, 1.000000000000000000),
 ( 1.000000000000000000, 0.7071067811865482389, 1.000000000000000000),
 ( 1.000000000000000000, 0.7071067811865482389, 1.000000000000000000),
 ( 1.000000000000000000, 0.7071067811865482389, 1.000000000000000000),
 ( 1.000000000000000000, 0.7071067811865482389, 1.000000000000000000),
 ( 1.000000000000000000, 0.7071067811865469066, 1.000000000000000000),
 ( 1.000000000000000000, 0.7071067811865469066, 1.000000000000000000),
 ( 1.000000000000000000, 0.7071067811865471286, 1.000000000000000000),
 ( 1.000000000000000000, 0.7071067811865471286, 1.000000000000000000),
 ( 1.000000000000000000, 0.7071067811865456854, 1.000000000000000000),
 ( 1.000000000000000000, 0.7071067811865456854, 1.000000000000000000),
 ( 1.000000000000000000, 0.7071067811865482389, 1.000000000000000000),
 ( 1.000000000000000000, 0.7071067811865482389, 1.000000000000000000),
 ( 1.000000000000000000, 0.7071067811865493491, 1.000000000000000000),
 ( 1.000000000000000000, 0.7071067811865493491, 1.000000000000000000),
 ( 1.000000000000000000, 0.7071067811865482389, 1.000000000000000000),
 ( 1.000000000000000000, 0.7071067811865482389, 1.000000000000000000) ) ) 
 REPRESENTATION_ITEM ( '' )  SURFACE ( )  );
#74984 = CARTESIAN_POINT ( 'NONE',  ( 0.5774900079438607392, 38.48035201082150536, 5.440088680355550821 ) ) ;
#74985 = CARTESIAN_POINT ( 'NONE',  ( 14.92337183194729988, 39.34226448433412315, -8.527530157486177487 ) ) ;
#74986 = CARTESIAN_POINT ( 'NONE',  ( 10.00000000000000000, 30.55374883491397142, -14.16423886937410082 ) ) ;
#74987 = VERTEX_POINT ( 'NONE', #70549 ) ;
#74988 = FILL_AREA_STYLE_COLOUR ( '', #28377 ) ;
#74989 = CARTESIAN_POINT ( 'NONE',  ( 7.084665262690076126, 69.10535201082151957, 10.88017736071109987 ) ) ;
#74990 = CARTESIAN_POINT ( 'NONE',  ( 0.5774900079438607392, 63.48035201082149825, 5.440088680355550821 ) ) ;
#74991 = CARTESIAN_POINT ( 'NONE',  ( 10.00000000000000178, 53.05374883491396787, 14.16423886937410082 ) ) ;
#74992 = CARTESIAN_POINT ( 'NONE',  ( 5.076628168052703671, 61.84226448433412315, 8.527530157486179263 ) ) ;
#74993 = CARTESIAN_POINT ( 'NONE',  ( -0.03932841506541361054, 53.12161441960503794, 6.397827110479011203 ) ) ;
#74994 = CARTESIAN_POINT ( 'NONE',  ( 7.084665262690076126, 54.10535201082151247, 10.88017736071109987 ) ) ;
#74995 = EDGE_CURVE ( 'NONE', #93612, #43655, #47042, .T. ) ;
#74996 = DIRECTION ( 'NONE',  ( 0.000000000000000000, 0.000000000000000000, 1.000000000000000000 ) ) ;
#74997 = AXIS2_PLACEMENT_3D ( 'NONE', #96921, #20907, #73891 ) ;
#74998 = CARTESIAN_POINT ( 'NONE',  ( 2.915334737309921209, 31.60535201082150891, -10.88017736071110164 ) ) ;
#74999 = CARTESIAN_POINT ( 'NONE',  ( 0.5774900079438590739, 12.64701867748817143, -5.440088680355550821 ) ) ;
#75000 = CARTESIAN_POINT ( 'NONE',  ( 0.5774900079438590739, 12.64701867748817321, -5.440088680355550821 ) ) ;
#75001 = CARTESIAN_POINT ( 'NONE',  ( 12.63842701281683034, 42.46726448433412315, 9.846743663894596210 ) ) ;
#75002 = CARTESIAN_POINT ( 'NONE',  ( 10.00000000000000000, 52.87363466993041783, -12.81628187352647608 ) ) ;
#75003 = ORIENTED_EDGE ( 'NONE', *, *, #75431, .T. ) ;
#75004 = CARTESIAN_POINT ( 'NONE',  ( 17.96484262340118221, 11.18868534415483929, -7.964842623401177768 ) ) ;
#75005 = CARTESIAN_POINT ( 'NONE',  ( 10.00000000000000000, 22.87363466993042138, -12.81628187352647608 ) ) ;
#75006 = CARTESIAN_POINT ( 'NONE',  ( -13.50249619331281892, 15.00000000000000711, 5.623250243473404630 ) ) ;
#75007 = CARTESIAN_POINT ( 'NONE',  ( 12.63842701281683922, 9.550597817667449974, -9.846743663894590881 ) ) ;
#75008 = CARTESIAN_POINT ( 'NONE',  ( 17.20831665107776587, 44.13393115100078745, -7.208316651077762316 ) ) ;
#75009 = CARTESIAN_POINT ( 'NONE',  ( -0.8801773607111009756, 33.06368534415484106, 1.068504757029289695E-15 ) ) ;
#75010 = CARTESIAN_POINT ( 'NONE',  ( -2.816281873526473856, 14.33196800326375531, 3.434112377981055619 ) ) ;
#75012 = CARTESIAN_POINT ( 'NONE',  ( -5.204170427930421283E-15, 11.41212336850781739, -11.92686044187656513 ) ) ;
#75011 = CARTESIAN_POINT ( 'NONE',  ( 19.42250999205614548, 50.98035201082151247, -5.440088680355545492 ) ) ;
#75013 = CARTESIAN_POINT ( 'NONE',  ( 2.831191079880678085, 79.91181047996344944, 12.00000000000000000 ) ) ;
#75014 = CARTESIAN_POINT ( 'NONE',  ( 6.565887622018943937, 55.16530133659709634, 12.81628187352647430 ) ) ;
#75015 = ORIENTED_EDGE ( 'NONE', *, *, #67305, .F. ) ;
#75016 = CARTESIAN_POINT ( 'NONE',  ( 20.88017736071110519, 60.56368534415484106, 2.639326808657452039E-16 ) ) ;
#75018 = CARTESIAN_POINT ( 'NONE',  ( 6.204703633549690345, 2.845415501580634388, 14.16423886937410082 ) ) ;
#75017 = CARTESIAN_POINT ( 'NONE',  ( 22.81628187352647785, 31.62363466993042138, 6.195893100308588602E-16 ) ) ;
#75019 = CARTESIAN_POINT ( 'NONE',  ( 19.84674366389459621, 8.508931151000785675, 7.409399052514197653E-17 ) ) ;
#75020 = CARTESIAN_POINT ( 'NONE',  ( 2.035157376598824452, 33.68868534415484106, 7.964842623401179544 ) ) ;
#75021 = DIRECTION ( 'NONE',  ( 0.000000000000000000, 0.000000000000000000, 1.000000000000000000 ) ) ;
#75022 = CARTESIAN_POINT ( 'NONE',  ( 14.92337183194729988, 64.34226448433412315, -8.527530157486177487 ) ) ;
#75023 = CARTESIAN_POINT ( 'NONE',  ( 10.00000000000000000, 19.75893115100078390, -9.846743663894594434 ) ) ;
#75024 = CARTESIAN_POINT ( 'NONE',  ( 5.076628168052704559, 0.1755978176674514724, -8.527530157486179263 ) ) ;
#75025 = CARTESIAN_POINT ( 'NONE',  ( -3.750000000000000000, 10.25000000000000000, -2.500000000000000000 ) ) ;
#75026 = CARTESIAN_POINT ( 'NONE',  ( 22.26659068614894466, 43.88708216824729647, 7.082119434687054849 ) ) ;
#75027 = DIRECTION ( 'NONE',  ( -0.000000000000000000, -0.000000000000000000, -1.000000000000000000 ) ) ;
#75028 = CARTESIAN_POINT ( 'NONE',  ( -4.537879770859267303, -17.56524742835268782, -3.749999999998386180 ) ) ;
#75029 = ORIENTED_EDGE ( 'NONE', *, *, #14061, .F. ) ;
#75030 = ORIENTED_EDGE ( 'NONE', *, *, #15576, .F. ) ;
#75031 = CARTESIAN_POINT ( 'NONE',  ( -0.3689425029237881626, 57.42874883491397497, 10.36894250292379027 ) ) ;
#75032 = CARTESIAN_POINT ( 'NONE',  ( 13.79529636645030344, 63.26208216824730357, 14.16423886937410614 ) ) ;
#75033 = CARTESIAN_POINT ( 'NONE',  ( 14.92337183194729988, 34.34226448433411605, -8.527530157486177487 ) ) ;
#75034 = CARTESIAN_POINT ( 'NONE',  ( 19.38216949554541557, 27.24863466993041783, -9.382169495545420901 ) ) ;
#75035 =( LENGTH_UNIT ( ) NAMED_UNIT ( * ) SI_UNIT ( .MILLI., .METRE. ) );
#75037 = CARTESIAN_POINT ( 'NONE',  ( 20.36894250292379738, 4.928748834913967869, -10.36894250292379027 ) ) ;
#75036 = DIRECTION ( 'NONE',  ( -0.000000000000000000, -1.000000000000000000, -0.000000000000000000 ) ) ;
#75038 = CARTESIAN_POINT ( 'NONE',  ( 20.88017736071110875, 15.77201867748817143, -2.915334737309920765 ) ) ;
#75039 = CARTESIAN_POINT ( 'NONE',  ( 13.79529636645031943, 50.34541550158064638, -14.16423886937409904 ) ) ;
#75040 = CARTESIAN_POINT ( 'NONE',  ( 1.472469842513823179, 26.42559781766745175, 4.923371831947296329 ) ) ;
#75041 = DIRECTION ( 'NONE',  ( -0.4924235601034707144, 0.000000000000000000, 0.8703556959398975890 ) ) ;
#75042 = CARTESIAN_POINT ( 'NONE',  ( 12.63842701281683034, 17.46726448433411250, 9.846743663894596210 ) ) ;
#75043 = CARTESIAN_POINT ( 'NONE',  ( 2.638427012816835227, 17.46726448433411960, 9.846743663894590881 ) ) ;
#75044 = ORIENTED_EDGE ( 'NONE', *, *, #1053, .F. ) ;
#75045 = ORIENTED_EDGE ( 'NONE', *, *, #40802, .F. ) ;
#75046 = DIRECTION ( 'NONE',  ( 0.06975647374412452528, 0.9975640502598243087, 0.000000000000000000 ) ) ;
#75047 = ORIENTED_EDGE ( 'NONE', *, *, #65118, .T. ) ;
#75048 = CARTESIAN_POINT ( 'NONE',  ( 18.52753015748618282, 48.92559781766745886, -4.923371831947291888 ) ) ;
#75049 = CARTESIAN_POINT ( 'NONE',  ( 22.26659068614895176, 19.72041550158063572, -7.082119434687042414 ) ) ;
#75051 = CARTESIAN_POINT ( 'NONE',  ( -0.8801773607111008646, 38.27201867748816255, 2.915334737309923430 ) ) ;
#75050 = CARTESIAN_POINT ( 'NONE',  ( 4.559911319644449179, 17.23035201082150536, -9.422509992056141925 ) ) ;
#75053 = CARTESIAN_POINT ( 'NONE',  ( 0.6178305044545818747, 23.49863466993041783, -9.382169495545419124 ) ) ;
#75052 = SURFACE_STYLE_USAGE ( .BOTH. , #97098 ) ;
#75054 = CARTESIAN_POINT ( 'NONE',  ( 2.917880565312948704, 7.637082168247301794, 12.26659068614894643 ) ) ;
#75055 = EDGE_CURVE ( 'NONE', #63345, #55238, #61554, .T. ) ;
#75056 = CARTESIAN_POINT ( 'NONE',  ( 2.035157376598822676, 67.43868534415484817, -7.964842623401177768 ) ) ;
#75057 = B_SPLINE_CURVE_WITH_KNOTS ( 'NONE', 3,
 ( #12396, #94911, #4910, #57887, #19899, #42902 ),
 .UNSPECIFIED., .F., .F.,
 ( 4, 2, 4 ),
 ( 3.409110551494634492E-05, 0.0004400426677367926974, 0.0008459942299586390227 ),
 .UNSPECIFIED. ) ;
#75058 = CARTESIAN_POINT ( 'NONE',  ( 3.591859063236763294, 38.29030133659708923, -11.09922568453595026 ) ) ;
#75059 = ORIENTED_EDGE ( 'NONE', *, *, #81167, .F. ) ;
#75060 = CARTESIAN_POINT ( 'NONE',  ( 0.1532563361054083140, 41.00893115100078745, 1.131784320476157264E-15 ) ) ;
#75061 = CARTESIAN_POINT ( 'NONE',  ( 4.559911319644449179, 12.23035201082150714, -9.422509992056141925 ) ) ;
#75062 = B_SPLINE_CURVE_WITH_KNOTS ( 'NONE', 3,
 ( #19678, #87671, #42675, #26199 ),
 .UNSPECIFIED., .F., .F.,
 ( 4, 4 ),
 ( 0.000000000000000000, 0.002657014572711318551 ),
 .UNSPECIFIED. ) ;
#75063 = CARTESIAN_POINT ( 'NONE',  ( -2.266590686148945544, 66.38708216824730357, -7.082119434687050408 ) ) ;
#75064 = ORIENTED_EDGE ( 'NONE', *, *, #35785, .T. ) ;
#75065 = CARTESIAN_POINT ( 'NONE',  ( 17.96484262340118221, 41.18868534415484106, -7.964842623401177768 ) ) ;
#75066 = TOROIDAL_SURFACE ( 'NONE', #91050, 14.49999999999999822, 0.5000000000000000000 ) ;
#75067 = CARTESIAN_POINT ( 'NONE',  ( 7.084665262690076126, 52.02201867748816255, -10.88017736071110164 ) ) ;
#75068 = FACE_OUTER_BOUND ( 'NONE', #36145, .T. ) ;
#75069 = CARTESIAN_POINT ( 'NONE',  ( 12.63842701281683034, 2.467264484334118269, 9.846743663894596210 ) ) ;
#75070 = ADVANCED_FACE ( 'NONE', ( #55548 ), #77056, .T. ) ;
#75071 = CARTESIAN_POINT ( 'NONE',  ( 20.88017736071110519, 60.56368534415484106, 2.639326808657452039E-16 ) ) ;
#75072 = CIRCLE ( 'NONE', #92693, 0.5000000000000009992 ) ;
#75073 = CARTESIAN_POINT ( 'NONE',  ( -0.3289641300568009741, 52.24545670184113533, -5.963430220938281678 ) ) ;
#75075 = ORIENTED_EDGE ( 'NONE', *, *, #84249, .T. ) ;
#75074 = DIRECTION ( 'NONE',  ( 0.000000000000000000, -1.000000000000000000, 0.000000000000000000 ) ) ;
#75076 = EDGE_CURVE ( 'NONE', #39153, #38225, #8568, .T. ) ;
#75077 = CARTESIAN_POINT ( 'NONE',  ( 0.1532563361054100626, 25.80059781766744820, -2.638427012816831230 ) ) ;
#75078 = ORIENTED_EDGE ( 'NONE', *, *, #81442, .T. ) ;
#75079 = DIRECTION ( 'NONE',  ( -0.000000000000000000, -1.000000000000000000, -0.000000000000000000 ) ) ;
#75080 = EDGE_CURVE ( 'NONE', #84641, #56002, #85056, .T. ) ;
#75081 = CARTESIAN_POINT ( 'NONE',  ( -2.266590686148945544, 7.220415501580634832, 7.082119434687048631 ) ) ;
#75082 = SURFACE_STYLE_FILL_AREA ( #13598 ) ;
#75083 = CARTESIAN_POINT ( 'NONE',  ( -0.03447792253739101476, 35.15514106990691090, 6.401564815979742917 ) ) ;
#75084 = DIRECTION ( 'NONE',  ( 0.000000000000000000, 1.000000000000000000, 0.000000000000000000 ) ) ;
#75085 = CARTESIAN_POINT ( 'NONE',  ( 2.035157376598822676, 12.43868534415483751, -7.964842623401177768 ) ) ;
#75086 = DIRECTION ( 'NONE',  ( 0.000000000000000000, 0.000000000000000000, 1.000000000000000000 ) ) ;
#75087 = ORIENTED_EDGE ( 'NONE', *, *, #30245, .F. ) ;
#75088 = CARTESIAN_POINT ( 'NONE',  ( 17.35999999999999943, 37.99999999999997868, 10.00000000000000000 ) ) ;
#75089 = CARTESIAN_POINT ( 'NONE',  ( 12.63842701281683922, 44.55059781766745175, -9.846743663894590881 ) ) ;
#75090 = DIRECTION ( 'NONE',  ( 0.000000000000000000, 0.000000000000000000, -1.000000000000000000 ) ) ;
#75091 = CARTESIAN_POINT ( 'NONE',  ( -2.816281873526473856, 19.33196800326375708, 3.434112377981055619 ) ) ;
#75092 = CARTESIAN_POINT ( 'NONE',  ( 12.63842701281683922, 4.550597817667451750, -9.846743663894590881 ) ) ;
#75093 = FACE_OUTER_BOUND ( 'NONE', #89317, .T. ) ;
#75094 = CARTESIAN_POINT ( 'NONE',  ( 16.40814093676324603, 7.456968003263754419, -11.09922568453594671 ) ) ;
#75095 = CARTESIAN_POINT ( 'NONE',  ( 0.1532563361054082862, 26.21726448433411960, 2.638427012816831674 ) ) ;
#75096 = ORIENTED_EDGE ( 'NONE', *, *, #29158, .F. ) ;
#75097 = EDGE_CURVE ( 'NONE', #64078, #13373, #79583, .T. ) ;
#75098 = EDGE_LOOP ( 'NONE', ( #71243, #90245, #36684, #42019 ) ) ;
#75099 = CARTESIAN_POINT ( 'NONE',  ( 10.00000000000000000, 21.81368534415484106, -10.88017736071110342 ) ) ;
#75100 = CARTESIAN_POINT ( 'NONE',  ( 6.204703633549690345, 25.76208216824730712, -14.16423886937410259 ) ) ;
#75101 = CARTESIAN_POINT ( 'NONE',  ( 14.92337183194729633, 32.67559781766745175, 8.527530157486181039 ) ) ;
#75102 = CARTESIAN_POINT ( 'NONE',  ( 10.00000000000000000, 56.81368534415484106, -10.88017736071110342 ) ) ;
#75104 = SURFACE_STYLE_USAGE ( .BOTH. , #28121 ) ;
#75103 = CARTESIAN_POINT ( 'NONE',  ( 6.565887622018943937, 38.08196800326376064, -12.81628187352647608 ) ) ;
#75105 = CARTESIAN_POINT ( 'NONE',  ( 12.91533473730992121, 9.522018677488171434, 10.88017736071110164 ) ) ;
#75106 = ADVANCED_FACE ( 'NONE', ( #62533 ), #75343, .T. ) ;
#75107 = CYLINDRICAL_SURFACE ( 'NONE', #93322, 15.00000000000000000 ) ;
#75108 = CARTESIAN_POINT ( 'NONE',  ( 4.547378612396773434, 0.000000000000000000, -3.009844244835506721 ) ) ;
#75109 = CARTESIAN_POINT ( 'NONE',  ( -2.816281873526471635, 8.915301336597083903, -3.434112377981056508 ) ) ;
#75110 = CARTESIAN_POINT ( 'NONE',  ( 1.472469842513823179, 65.59226448433412315, -4.923371831947296329 ) ) ;
#75111 = CARTESIAN_POINT ( 'NONE',  ( 10.00000000000000178, 22.25893115100078745, 9.846743663894594434 ) ) ;
#75112 = CARTESIAN_POINT ( 'NONE',  ( -10.88017736071110164, -7.144647989178493752, -2.915334737309917212 ) ) ;
#75113 = CARTESIAN_POINT ( 'NONE',  ( 22.81628187352648496, 41.83196800326375353, -3.434112377981050290 ) ) ;
#75114 = LINE ( 'NONE', #14640, #97935 ) ;
#75116 = LINE ( 'NONE', #67631, #54383 ) ;
#75115 = CARTESIAN_POINT ( 'NONE',  ( 15.44008868035555793, 36.39701867748816966, -9.422509992056140149 ) ) ;
#75117 = PLANE ( 'NONE',  #72110 ) ;
#75118 = CARTESIAN_POINT ( 'NONE',  ( 19.80777595082616926, 20.68878173731740944, -6.499999999999961808 ) ) ;
#75119 = CARTESIAN_POINT ( 'NONE',  ( 19.42250999205614548, 40.98035201082150536, -5.440088680355545492 ) ) ;
#75120 = CARTESIAN_POINT ( 'NONE',  ( 15.44008868035555260, 44.73035201082151247, 9.422509992056143702 ) ) ;
#75121 = CARTESIAN_POINT ( 'NONE',  ( 17.20831665107776587, 62.88393115100078745, 7.208316651077764980 ) ) ;
#75122 = CARTESIAN_POINT ( 'NONE',  ( -0.8801773607111009756, 53.06368534415484106, 1.068504757029289695E-15 ) ) ;
#75123 = UNCERTAINTY_MEASURE_WITH_UNIT (LENGTH_MEASURE( 1.000000000000000082E-05 ), #2327, 'distance_accuracy_value', 'NONE');
#75124 = CARTESIAN_POINT ( 'NONE',  ( 18.52753015748618282, 33.92559781766745886, -4.923371831947291888 ) ) ;
#75125 = CARTESIAN_POINT ( 'NONE',  ( -0.8801773607111008646, 13.27201867748817143, 2.915334737309923430 ) ) ;
#75126 = VECTOR ( 'NONE', #1488, 1000.000000000000114 ) ;
#75127 = CARTESIAN_POINT ( 'NONE',  ( 3.591859063236761518, 9.956968003263753531, 11.09922568453594849 ) ) ;
#75128 = ORIENTED_EDGE ( 'NONE', *, *, #31526, .F. ) ;
#75129 = CARTESIAN_POINT ( 'NONE',  ( 4.559911319644449179, 28.89701867748817321, 9.422509992056141925 ) ) ;
#75130 = CIRCLE ( 'NONE', #63981, 0.2500000000000002220 ) ;
#75131 = CARTESIAN_POINT ( 'NONE',  ( 2.035157376598822676, 32.43868534415483396, -7.964842623401177768 ) ) ;
#75132 = CARTESIAN_POINT ( 'NONE',  ( 0.5774900079438607392, 63.48035201082149825, 5.440088680355550821 ) ) ;
#75133 = CARTESIAN_POINT ( 'NONE',  ( -0.3689425029237881626, 32.42874883491395366, 10.36894250292379027 ) ) ;
#75134 = CARTESIAN_POINT ( 'NONE',  ( 17.20831665107776587, 9.133931151000787452, -7.208316651077762316 ) ) ;
#75135 = CARTESIAN_POINT ( 'NONE',  ( -0.8801773607111009756, 53.06368534415484106, 1.068504757029289695E-15 ) ) ;
#75136 = CARTESIAN_POINT ( 'NONE',  ( 19.39188664607695500, 45.83703382326400799, -6.499999999999968026 ) ) ;
#75137 = CARTESIAN_POINT ( 'NONE',  ( 24.16423886937409904, 4.095415501580634832, 3.795296366450317205 ) ) ;
#75138 = ORIENTED_EDGE ( 'NONE', *, *, #16959, .T. ) ;
#75139 = LINE ( 'NONE', #97675, #83285 ) ;
#75140 = CARTESIAN_POINT ( 'NONE',  ( 0.1532563361054083140, 61.00893115100078745, 1.131784320476157264E-15 ) ) ;
#75141 = ORIENTED_EDGE ( 'NONE', *, *, #55889, .F. ) ;
#75142 = VERTEX_POINT ( 'NONE', #32537 ) ;
#75143 = DIRECTION ( 'NONE',  ( -0.000000000000000000, 0.000000000000000000, 1.000000000000000000 ) ) ;
#75144 = CARTESIAN_POINT ( 'NONE',  ( 13.79529636645031943, 25.34541550158063572, -14.16423886937409904 ) ) ;
#75145 = CARTESIAN_POINT ( 'NONE',  ( 13.79529636645030344, 18.26208216824730002, 14.16423886937410614 ) ) ;
#75146 = CARTESIAN_POINT ( 'NONE',  ( 10.00000000000000178, 64.31368534415483396, 10.88017736071110342 ) ) ;
#75147 = CARTESIAN_POINT ( 'NONE',  ( -2.266590686148945544, 62.22041550158063927, 7.082119434687048631 ) ) ;
#75148 = CARTESIAN_POINT ( 'NONE',  ( 10.00000000000000178, 5.373634669930420493, 12.81628187352647608 ) ) ;
#75149 = CARTESIAN_POINT ( 'NONE',  ( 17.20831665107776587, 49.13393115100078745, -7.208316651077762316 ) ) ;
#75150 = CARTESIAN_POINT ( 'NONE',  ( -8.107943641816854452, -3.126452786863499256, 3.750000000000000000 ) ) ;
#75152 = CARTESIAN_POINT ( 'NONE',  ( -2.816281873526473856, 9.331968003263753531, 3.434112377981055619 ) ) ;
#75151 = CARTESIAN_POINT ( 'NONE',  ( 10.00000000000000178, 44.31368534415484106, 10.88017736071110342 ) ) ;
#75153 = CARTESIAN_POINT ( 'NONE',  ( 17.08211943468705840, 15.13708216824730179, -12.26659068614894466 ) ) ;
#75154 = CARTESIAN_POINT ( 'NONE',  ( 2.035157376598822676, 12.43868534415483751, -7.964842623401177768 ) ) ;
#75155 = CARTESIAN_POINT ( 'NONE',  ( 4.559911319644449179, 18.89701867748817321, 9.422509992056141925 ) ) ;
#75156 = CARTESIAN_POINT ( 'NONE',  ( 20.88017736071110875, 45.77201867748816966, -2.915334737309920765 ) ) ;
#75157 = CARTESIAN_POINT ( 'NONE',  ( 16.40814093676323893, 45.79030133659708923, 11.09922568453595026 ) ) ;
#75158 = CARTESIAN_POINT ( 'NONE',  ( 7.208316651077762316, -20.86606884899920544, -7.208316651077764980 ) ) ;
#75159 = VERTEX_POINT ( 'NONE', #69074 ) ;
#75160 = CARTESIAN_POINT ( 'NONE',  ( -46.34323875807881166, 103.6109741468810483, -6.190393423093146552 ) ) ;
#75161 = CARTESIAN_POINT ( 'NONE',  ( 7.361572987183170547, 32.05059781766745175, 9.846743663894590881 ) ) ;
#75162 = ORIENTED_EDGE ( 'NONE', *, *, #66486, .T. ) ;
#75163 = VECTOR ( 'NONE', #55055, 1000.000000000000000 ) ;
#75164 = CARTESIAN_POINT ( 'NONE',  ( 19.72487221294571569, 60.71833443783937412, -6.499999999999990230 ) ) ;
#75166 = CARTESIAN_POINT ( 'NONE',  ( 4.559911319644449179, 7.230352010821505360, -9.422509992056141925 ) ) ;
#75165 = CARTESIAN_POINT ( 'NONE',  ( 24.16423886937410614, 49.51208216824730357, -3.795296366450302550 ) ) ;
#75168 = CARTESIAN_POINT ( 'NONE',  ( 14.92337183194729633, 42.67559781766745886, 8.527530157486181039 ) ) ;
#75167 = CARTESIAN_POINT ( 'NONE',  ( 19.84674366389459621, 28.50893115100078745, 7.409399052514197653E-17 ) ) ;
#75169 = DIRECTION ( 'NONE',  ( 0.000000000000000000, -1.000000000000000000, 0.000000000000000000 ) ) ;
#75170 = EDGE_CURVE ( 'NONE', #91555, #85493, #66456, .T. ) ;
#75171 = CARTESIAN_POINT ( 'NONE',  ( 12.63842701281683034, 2.467264484334118269, 9.846743663894596210 ) ) ;
#75172 = CIRCLE ( 'NONE', #11283, 0.2500000000000002220 ) ;
#75173 = CARTESIAN_POINT ( 'NONE',  ( -6.408140936763232709, 19.95696800326377129, 11.09922568453595026 ) ) ;
#75174 = ORIENTED_EDGE ( 'NONE', *, *, #88860, .F. ) ;
#75175 = CARTESIAN_POINT ( 'NONE',  ( 6.204703633549690345, 37.84541550158063927, 14.16423886937410082 ) ) ;
#75176 = ORIENTED_EDGE ( 'NONE', *, *, #86726, .T. ) ;
#75177 = CARTESIAN_POINT ( 'NONE',  ( -2.816281873526473856, 29.33196800326376064, 3.434112377981055619 ) ) ;
#75178 = ORIENTED_EDGE ( 'NONE', *, *, #34165, .F. ) ;
#75179 = CARTESIAN_POINT ( 'NONE',  ( -2.816281873526471635, 63.91530133659708923, -3.434112377981056508 ) ) ;
#75180 = CARTESIAN_POINT ( 'NONE',  ( 0.1532563361054082862, 31.21726448433412315, 2.638427012816831674 ) ) ;
#75181 = CARTESIAN_POINT ( 'NONE',  ( -0.8801773607110991993, 32.85535201082151247, -2.915334737309923874 ) ) ;
#75182 = CARTESIAN_POINT ( 'NONE',  ( 20.24186590665275531, 32.61633188102328518, -6.114288769123075618 ) ) ;
#75183 = LINE ( 'NONE', #91170, #89490 ) ;
#75184 = CARTESIAN_POINT ( 'NONE',  ( 5.076628168052704559, 40.17559781766745175, -8.527530157486179263 ) ) ;
#75185 = CARTESIAN_POINT ( 'NONE',  ( 12.63842701281683922, 54.55059781766745175, -9.846743663894590881 ) ) ;
#75187 = AXIS2_PLACEMENT_3D ( 'NONE', #79559, #11059, #86080 ) ;
#75186 = CARTESIAN_POINT ( 'NONE',  ( -3.866399090317375720, 14.95077488074853811, 14.23717170745768712 ) ) ;
#75188 = ORIENTED_EDGE ( 'NONE', *, *, #61432, .F. ) ;
#75189 = EDGE_CURVE ( 'NONE', #69767, #89063, #39035, .T. ) ;
#75190 = CARTESIAN_POINT ( 'NONE',  ( 18.17884179759847996, 18.66688879859523453, -6.499999999999984901 ) ) ;
#75191 = DIRECTION ( 'NONE',  ( 1.000000000000000000, -7.138779736530071317E-16, 0.000000000000000000 ) ) ;
#75192 = CARTESIAN_POINT ( 'NONE',  ( 18.72515096720568195, 21.07228050351032422, -6.500000000000018652 ) ) ;
#75193 = CARTESIAN_POINT ( 'NONE',  ( 0.000000000000000000, 14.49999999999999822, 0.000000000000000000 ) ) ;
#75194 = CARTESIAN_POINT ( 'NONE',  ( 7.361572987183169658, 14.96726448433411960, -9.846743663894592657 ) ) ;
#75195 = ADVANCED_FACE ( 'NONE', ( #84568 ), #54571, .T. ) ;
#75196 = CARTESIAN_POINT ( 'NONE',  ( 22.81628187352647785, 36.41530133659707502, 3.434112377981063169 ) ) ;
#75197 = CARTESIAN_POINT ( 'NONE',  ( -7.750000000000000000, 41.24999999999999289, -6.250000000000000000 ) ) ;
#75198 = AXIS2_PLACEMENT_3D ( 'NONE', #34422, #3465, #94934 ) ;
#75199 = VERTEX_POINT ( 'NONE', #92543 ) ;
#75200 = CARTESIAN_POINT ( 'NONE',  ( 1.472469842513823179, 60.59226448433412315, -4.923371831947296329 ) ) ;
#75201 = CARTESIAN_POINT ( 'NONE',  ( 0.000000000000000000, 14.49999999999999822, 0.000000000000000000 ) ) ;
#75202 = CARTESIAN_POINT ( 'NONE',  ( 12.63842701281683922, 34.55059781766745886, -9.846743663894590881 ) ) ;
#75203 = CARTESIAN_POINT ( 'NONE',  ( 17.08211943468705130, 38.47041550158063217, 12.26659068614894998 ) ) ;
#75204 = CARTESIAN_POINT ( 'NONE',  ( 0.1532563361054082862, 41.21726448433411605, 2.638427012816831674 ) ) ;
#75205 = CARTESIAN_POINT ( 'NONE',  ( -2.816281873526473856, 49.33196800326374643, 3.434112377981055619 ) ) ;
#75206 = DIRECTION ( 'NONE',  ( 0.000000000000000000, -1.000000000000000000, 0.000000000000000000 ) ) ;
#75207 = CARTESIAN_POINT ( 'NONE',  ( 14.92337183194729633, 12.67559781766745353, 8.527530157486181039 ) ) ;
#75208 = FILL_AREA_STYLE_COLOUR ( '', #55196 ) ;
#75209 = CARTESIAN_POINT ( 'NONE',  ( 12.63842701281683922, 54.55059781766745175, -9.846743663894590881 ) ) ;
#75210 = CARTESIAN_POINT ( 'NONE',  ( 2.035157376598824452, 38.68868534415483396, 7.964842623401179544 ) ) ;
#75211 = CARTESIAN_POINT ( 'NONE',  ( 2.791683348922237240, 45.38393115100079456, -7.208316651077763204 ) ) ;
#75212 = ITEM_DEFINED_TRANSFORMATION ( 'NONE', 'NONE', #72671,  #27931 ) ;
#75213 = FACE_OUTER_BOUND ( 'NONE', #49554, .T. ) ;
#75214 = CARTESIAN_POINT ( 'NONE',  ( 20.88017736071110164, 50.35535201082151247, 2.915334737309930979 ) ) ;
#75215 = ORIENTED_EDGE ( 'NONE', *, *, #51184, .T. ) ;
#75216 = CARTESIAN_POINT ( 'NONE',  ( 6.761389522993794365, 0.2306972965111908080, 13.32372569557304764 ) ) ;
#75217 = CARTESIAN_POINT ( 'NONE',  ( -0.8801773607110991993, 17.85535201082150536, -2.915334737309923874 ) ) ;
#75219 = CARTESIAN_POINT ( 'NONE',  ( 12.91533473730992121, 44.52201867748816966, 10.88017736071110164 ) ) ;
#75218 = CARTESIAN_POINT ( 'NONE',  ( 7.361572987183170547, 67.05059781766746596, 9.846743663894590881 ) ) ;
#75220 = SURFACE_STYLE_USAGE ( .BOTH. , #84224 ) ;
#75221 = CARTESIAN_POINT ( 'NONE',  ( 4.559911319644449179, 67.23035201082150536, -9.422509992056141925 ) ) ;
#75222 = CARTESIAN_POINT ( 'NONE',  ( 13.78891971893207291, 14.63606857305789966, 5.904717858191650848 ) ) ;
#75224 = CARTESIAN_POINT ( 'NONE',  ( 0.000000000000000000, 80.32179676972448590, 4.000000000000000000 ) ) ;
#75223 = CARTESIAN_POINT ( 'NONE',  ( 0.5774900079438590739, 37.64701867748817676, -5.440088680355550821 ) ) ;
#75225 = CARTESIAN_POINT ( 'NONE',  ( 5.076628168052703671, 11.84226448433411960, 8.527530157486179263 ) ) ;
#75226 = CARTESIAN_POINT ( 'NONE',  ( 1.472469842513823179, 26.42559781766745175, 4.923371831947296329 ) ) ;
#75227 = DIRECTION ( 'NONE',  ( 1.049065152435176504E-16, -1.000000000000000000, 0.000000000000000000 ) ) ;
#75228 = CARTESIAN_POINT ( 'NONE',  ( 14.16423886937410437, 19.09541550158063572, 3.795296366450304770 ) ) ;
#75229 = CARTESIAN_POINT ( 'NONE',  ( 7.361572987183169658, 64.96726448433412315, -9.846743663894592657 ) ) ;
#75231 = DIRECTION ( 'NONE',  ( -1.000000000000000000, 0.000000000000000000, 0.000000000000000000 ) ) ;
#75230 = CARTESIAN_POINT ( 'NONE',  ( -0.3689425029237881626, 67.42874883491396076, 10.36894250292379027 ) ) ;
#75232 = AXIS2_PLACEMENT_3D ( 'NONE', #25331, #70331, #54809 ) ;
#75234 = COLOUR_RGB ( '', 0.31764706, 0.68627451, 0.89019608) ;
#75233 = CARTESIAN_POINT ( 'NONE',  ( 19.80427997160309417, 27.75733960839543712, -6.499999999999987566 ) ) ;
#75235 = CARTESIAN_POINT ( 'NONE',  ( -0.3689425029237881626, 17.42874883491397142, 10.36894250292379027 ) ) ;
#75236 = CARTESIAN_POINT ( 'NONE',  ( -2.266590686148945544, 56.38708216824731068, -7.082119434687050408 ) ) ;
#75237 = CARTESIAN_POINT ( 'NONE',  ( 20.03447792253739124, 32.65514106990688958, -6.401564815979717160 ) ) ;
#75238 = AXIS2_PLACEMENT_3D ( 'NONE', #84476, #55451, #1482 ) ;
#75239 = ORIENTED_EDGE ( 'NONE', *, *, #18543, .F. ) ;
#75240 = CARTESIAN_POINT ( 'NONE',  ( 1.472469842513823179, 30.59226448433411960, -4.923371831947296329 ) ) ;
#75241 = CARTESIAN_POINT ( 'NONE',  ( -0.8801773607111009756, 8.063685344154837509, 1.068504757029289695E-15 ) ) ;
#75242 = CARTESIAN_POINT ( 'NONE',  ( 14.92337183194729633, 52.67559781766745175, 8.527530157486181039 ) ) ;
#75244 = DIRECTION ( 'NONE',  ( 0.000000000000000000, 1.000000000000000000, 0.000000000000000000 ) ) ;
#75243 = CARTESIAN_POINT ( 'NONE',  ( 6.880000000000009663, 40.74999999999999289, 4.000000000000000000 ) ) ;
#75245 = CARTESIAN_POINT ( 'NONE',  ( 8.629999999999995453, 41.24999999999999289, -6.250000000000000000 ) ) ;
#75246 = CARTESIAN_POINT ( 'NONE',  ( 6.565887622018943937, 43.08196800326374643, -12.81628187352647608 ) ) ;
#75247 = B_SPLINE_CURVE_WITH_KNOTS ( 'NONE', 3,
 ( #27935, #20451, #26956, #81434, #57456, #19464 ),
 .UNSPECIFIED., .F., .F.,
 ( 4, 2, 4 ),
 ( 0.000000000000000000, 0.0002701661927229340350, 0.0005403323854458680700 ),
 .UNSPECIFIED. ) ;
#75248 = CARTESIAN_POINT ( 'NONE',  ( 14.92337183194729633, 47.67559781766745175, 8.527530157486181039 ) ) ;
#75249 = ORIENTED_EDGE ( 'NONE', *, *, #6952, .T. ) ;
#75250 = CARTESIAN_POINT ( 'NONE',  ( 0.1532563361054082862, 6.217264484334118713, 2.638427012816831674 ) ) ;
#75251 = CARTESIAN_POINT ( 'NONE',  ( 10.76563361875039782, -96.07941716639480489, -4.000000000000000000 ) ) ;
#75252 = DIRECTION ( 'NONE',  ( 0.000000000000000000, 1.000000000000000000, 0.000000000000000000 ) ) ;
#75253 = CARTESIAN_POINT ( 'NONE',  ( 20.88017736071110164, 15.35535201082150358, 2.915334737309930979 ) ) ;
#75254 = CARTESIAN_POINT ( 'NONE',  ( 2.917880565312948704, 57.63708216824731068, 12.26659068614894643 ) ) ;
#75255 = CARTESIAN_POINT ( 'NONE',  ( -0.8801773607111008646, 68.27201867748817676, 2.915334737309923430 ) ) ;
#75256 =( LENGTH_UNIT ( ) NAMED_UNIT ( * ) SI_UNIT ( .MILLI., .METRE. ) );
#75257 = CARTESIAN_POINT ( 'NONE',  ( 5.076628168052703671, 26.84226448433411960, 8.527530157486179263 ) ) ;
#75258 = CARTESIAN_POINT ( 'NONE',  ( 4.559911319644449179, 7.230352010821504471, -9.422509992056141925 ) ) ;
#75259 = CARTESIAN_POINT ( 'NONE',  ( 17.20831665107776587, 7.883931151000784787, 7.208316651077764980 ) ) ;
#75260 =( BOUNDED_SURFACE ( )  B_SPLINE_SURFACE ( 1, 2, ( 
 ( #58530, #20549, #43529, #81527, #5555, #66534, #42079, #72542, #28534, #51533, #59028, #6042, #65535, #4075, #34538, #95559, #27048, #96058, #57546, #8505, #6524, #91000, #69502, #69012, #60010, #29502, #15035, #7535, #30991, #52515, #38026, #45508, #84010, #37534, #7028, #84505, #76504, #46493, #52030, #82523, #83516, #38515, #75019, #91995, #67530, #68519, #76992, #98551, #49, #30497, #23526, #53499, #8018, #2508, #63465, #94450, #63937, #41481, #55977, #40488, #54967, #62969, #24505, #55485, #3471, #92973, #47961, #93474, #25964, #77476, #70489, #17976, #62468, #32960, #54479, #48461, #71476, #18464, #85489, #2009, #79457, #56465, #16998, #93967, #78471, #31966, #32474, #71948, #33927, #25000, #85985, #86951, #48949, #47477, #33441, #16505, #46982, #77977, #2991, #17496, #64433, #10956, #9985, #70986, #24007, #78959, #25492, #84989, #10470, #40979, #9484, #86478, #8987, #39504, #69993, #1520, #39987, #56941, #27916, #72430, #88431, #72928, #57921, #3956, #49936, #28418, #64918, #34426, #35915, #12918, #4457, #19930, #57436, #74400, #50425, #58408, #36417, #80932, #87443, #96445, #42445, #51416, #43900, #73413, #95445, #12426, #58913, #88924, #5444, #50920, #42932, #20433, #18958, #4941, #34922, #5924, #96945, #81416, #79940, #35421, #43415, #73915, #65915, #94941, #66414, #26442, #89412, #87928, #20927, #81905, #13414, #49436, #26937, #11447, #41964, #19445, #80443, #11940, #65420, #95944, #27427, #60387, #52400, #55222, #90885, #47223, #62719, #59400, #17249, #21921, #97934, #85242, #16748, #23773, #85736, #14418, #82900, #1762, #93219, #67405, #54238, #37420, #9734, #66909, #6399, #77726, #51913, #59893, #29391, #36913, #32218, #84751, #8740, #54722, #92734, #1278, #16256, #90383, #46738, #47725, #28895, #78223, #67906, #9238, #77236, #44887, #70246, #69750, #75390, #39261, #44401, #31731, #62227, #98430, #29885, #6908, #97429, #89903, #24258, #39749, #21419, #24743, #82398, #13923, #74900, #40234, #86226, #2750, #57186, #93715, #71712, #18717, #79703, #11697, #80184, #57681, #72190, #56704, #71227, #79207, #40725, #3223, #19690, #10232, #64185, #10717, #42206, #25250, #86719, #34180, #78722, #49199, #70742, #64672, #87683, #34678, #33206, #18223, #95694, #72673, #63700, #11201, #94705, #48212, #48703, #88177, #50177, #41234, #33687, #4208, #65174, #94203, #49680, #32713, #63211, #25733, #19197, #26211, #80687, #27178, #87194, #41721, #2258, #95182, #3719, #55734, #26690, #17737, #56225, #58667, #90638, #21172, #89169, #28663, #29147, #35677, #20680, #43665, #36170, #59653, #89662, #96694, #81175, #12183, #81658 ),
 ( #22163, #13167, #51675, #5685, #51174, #98177, #66670, #90144, #6658, #4707, #60141, #66161, #43175, #21674, #52160, #97195, #29633, #74151, #59155, #44653, #37174, #12675, #82153, #13665, #52645, #42689, #50683, #82653, #27676, #44149, #74657, #6168, #36672, #67160, #14169, #97685, #75148, #67667, #73168, #65670, #58161, #88672, #20180, #77116, #54117, #1151, #84630, #7157, #68160, #84151, #16630, #91638, #23156, #76140, #39633, #31611, #53631, #22662, #7666, #38157, #15657, #46140, #76626, #92612, #77605, #93599, #32601, #18111, #79089, #34063, #25136, #10601, #41115, #87085, #71111, #55614, #57076, #49088, #87572, #72559, #4092, #33574, #64559, #34556, #95069, #65050, #64068, #49560, #85617, #86111, #17622, #26573, #9614, #94583, #18595, #79591, #19084, #80072, #95576, #11092, #11578, #48092, #94094, #78605, #42092, #17134, #10114, #47613, #25615, #78108, #40115, #2638, #70616, #33092, #63585, #56108, #21059, #74537, #21558, #88558, #5071, #82538, #59540, #20061, #97080, #51051, #35050, #35558, #44538, #6541, #66048, #96575, #97568, #90034, #50563, #36556, #19572, #80573, #96076, #67046, #28052, #75034, #52047, #58547, #20566, #14056, #82040, #43545, #37050, #81541, #5574, #67549, #13051, #27063, #36049, #66552, #59044, #44037, #12069, #42571, #81058, #12562, #51553, #73055, #13551, #4588, #84521, #23540, #31006, #46032, #37550, #53515, #16521, #60026, #77489, #66, #8519, #84026, #60525, #1032, #561, #68040, #69027, #75531, #76517, #15547, #30513, #61016, #98566, #54012, #16018, #30020, #8032, #90521, #46507, #46995, #61503, #77007, #22057, #92010, #7045, #91527, #76023, #23041, #91015, #53018, #31493, #22548, #83533, #39021, #69517, #7554, #38531, #15051, #9001, #61997, #92496, #39517, #24025, #52530, #54493, #45525, #85008, #98061, #29519, #38044, #83038, #14555, #45024, #68535, #25981, #93982, #94464, #31979, #78972, #17511, #79956, #71962, #56478, #54982, #25504, #3006, #48963, #48474, #11460, #41493, #70010, #79473, #62982, #33942, #40994, #10483, #10972, #9497, #64446, #32974, #55991, #94953, #62485, #1535, #70997, #26455, #86492, #55499, #56954, #17992, #87457, #18972, #92989, #24523, #86000, #2025, #85501, #17011, #47489, #77992, #78486, #10000, #39999, #93488, #2521, #35435, #12441, #82413, #41979, #80456, #42949, #72442, #3971, #11955, #20943, #26951, #34937, #72941, #42459, #5941, #65930, #81430, #28431, #66426, #73929, #88937, #4471, #96458, #59412, #34441, #21432, #73428, #51430, #27929, #65435, #43914, #43428, #95959, #12934, #19459, #20446, #58423, #4955, #50936, #27441, #96959, #58929, #57935, #5457 ) ),
 .UNSPECIFIED., .F., .F., .F. ) 
 B_SPLINE_SURFACE_WITH_KNOTS ( ( 2, 2 ),
 ( 3, 2, 2, 2, 2, 2, 2, 2, 2, 2, 2, 2, 2, 2, 2, 2, 2, 2, 2, 2, 2, 2, 2, 2, 2, 2, 2, 2, 2, 2, 2, 2, 2, 2, 2, 2, 2, 2, 2, 2, 2, 2, 2, 2, 2, 2, 2, 2, 2, 2, 2, 2, 2, 2, 2, 2, 2, 2, 2, 2, 2, 2, 2, 2, 2, 2, 2, 2, 2, 2, 2, 2, 2, 2, 2, 2, 2, 2, 2, 2, 2, 2, 2, 2, 2, 2, 2, 2, 2, 2, 2, 2, 2, 2, 2, 2, 2, 2, 2, 2, 2, 2, 2, 2, 2, 2, 2, 2, 2, 2, 2, 2, 2, 2, 2, 2, 2, 2, 2, 2, 2, 2, 2, 2, 2, 2, 2, 2, 2, 2, 2, 2, 2, 2, 2, 2, 2, 2, 2, 2, 2, 2, 2, 2, 2, 2, 2, 2, 2, 2, 2, 2, 2, 2, 2, 2, 2, 2, 2, 2, 2, 2, 3 ),
 ( 0.000000000000000000, 1.000000000000000000 ),
 ( 0.000000000000000000, 0.005952380952380952051, 0.01190476190476190410, 0.01785714285714285615, 0.02380952380952380820, 0.02976190476190476025, 0.03571428571428571230, 0.04166666666666666435, 0.04761904761904761640, 0.05357142857142856845, 0.05952380952380952051, 0.06547619047619047949, 0.07142857142857142461, 0.07738095238095238360, 0.08333333333333332871, 0.08928571428571428770, 0.09523809523809523281, 0.1011904761904761918, 0.1071428571428571369, 0.1130952380952380959, 0.1190476190476190410, 0.1250000000000000000, 0.1309523809523809590, 0.1369047619047619180, 0.1428571428571428492, 0.1488095238095238082, 0.1547619047619047672, 0.1607142857142857262, 0.1666666666666666574, 0.1726190476190476164, 0.1785714285714285754, 0.1845238095238095344, 0.1904761904761904656, 0.1964285714285714246, 0.2023809523809523836, 0.2083333333333333426, 0.2142857142857142738, 0.2202380952380952328, 0.2261904761904761918, 0.2321428571428571508, 0.2380952380952380820, 0.2440476190476190410, 0.2500000000000000000, 0.2559523809523809312, 0.2619047619047619180, 0.2678571428571428492, 0.2738095238095238360, 0.2797619047619047672, 0.2857142857142856984, 0.2916666666666666852, 0.2976190476190476164, 0.3035714285714285476, 0.3095238095238095344, 0.3154761904761904656, 0.3214285714285714524, 0.3273809523809523836, 0.3333333333333333148, 0.3392857142857143016, 0.3452380952380952328, 0.3511904761904761640, 0.3571428571428571508, 0.3630952380952380820, 0.3690476190476190688, 0.3750000000000000000, 0.3809523809523809312, 0.3869047619047619180, 0.3928571428571428492, 0.3988095238095238360, 0.4047619047619047672, 0.4107142857142856984, 0.4166666666666666852, 0.4226190476190476164, 0.4285714285714285476, 0.4345238095238095344, 0.4404761904761904656, 0.4464285714285714524, 0.4523809523809523836, 0.4583333333333333148, 0.4642857142857143016, 0.4702380952380952328, 0.4761904761904761640, 0.4821428571428571508, 0.4880952380952380820, 0.4940476190476190688, 0.5000000000000000000, 0.5059523809523809312, 0.5119047619047618625, 0.5178571428571429047, 0.5238095238095238360, 0.5297619047619047672, 0.5357142857142856984, 0.5416666666666666297, 0.5476190476190476719, 0.5535714285714286031, 0.5595238095238095344, 0.5654761904761904656, 0.5714285714285713969, 0.5773809523809523281, 0.5833333333333333703, 0.5892857142857143016, 0.5952380952380952328, 0.6011904761904761640, 0.6071428571428570953, 0.6130952380952381375, 0.6190476190476190688, 0.6250000000000000000, 0.6309523809523809312, 0.6369047619047618625, 0.6428571428571429047, 0.6488095238095238360, 0.6547619047619047672, 0.6607142857142856984, 0.6666666666666666297, 0.6726190476190476719, 0.6785714285714286031, 0.6845238095238095344, 0.6904761904761904656, 0.6964285714285713969, 0.7023809523809523281, 0.7083333333333333703, 0.7142857142857143016, 0.7202380952380952328, 0.7261904761904761640, 0.7321428571428570953, 0.7380952380952381375, 0.7440476190476190688, 0.7500000000000000000, 0.7559523809523809312, 0.7619047619047618625, 0.7678571428571429047, 0.7738095238095238360, 0.7797619047619047672, 0.7857142857142856984, 0.7916666666666666297, 0.7976190476190476719, 0.8035714285714286031, 0.8095238095238095344, 0.8154761904761904656, 0.8214285714285713969, 0.8273809523809523281, 0.8333333333333333703, 0.8392857142857143016, 0.8452380952380952328, 0.8511904761904761640, 0.8571428571428570953, 0.8630952380952381375, 0.8690476190476190688, 0.8750000000000000000, 0.8809523809523809312, 0.8869047619047618625, 0.8928571428571429047, 0.8988095238095238360, 0.9047619047619047672, 0.9107142857142856984, 0.9166666666666666297, 0.9226190476190476719, 0.9285714285714286031, 0.9345238095238095344, 0.9404761904761904656, 0.9464285714285713969, 0.9523809523809523281, 0.9583333333333333703, 0.9642857142857143016 ),
 .UNSPECIFIED. ) 
 GEOMETRIC_REPRESENTATION_ITEM ( )  RATIONAL_B_SPLINE_SURFACE ( (
 ( 1.000000000000000000, 0.9659258262890683122, 1.000000000000000000, 0.9659258262890683122, 1.000000000000000000, 0.9659258262890683122, 1.000000000000000000, 0.9659258262890683122, 1.000000000000000000, 0.9659258262890683122, 1.000000000000000000, 0.9659258262890683122, 1.000000000000000000, 0.9659258262890683122, 1.000000000000000000, 0.9659258262890683122, 1.000000000000000000, 0.9659258262890683122, 1.000000000000000000, 0.9659258262890683122, 1.000000000000000000, 0.9659258262890683122, 1.000000000000000000, 0.9659258262890683122, 1.000000000000000000, 0.9659258262890683122, 1.000000000000000000, 0.9659258262890683122, 1.000000000000000000, 0.9659258262890683122, 1.000000000000000000, 0.9659258262890683122, 1.000000000000000000, 0.9659258262890683122, 1.000000000000000000, 0.9659258262890683122, 1.000000000000000000, 0.9659258262890683122, 1.000000000000000000, 0.9659258262890683122, 1.000000000000000000, 0.9659258262890683122, 1.000000000000000000, 0.9659258262890683122, 1.000000000000000000, 0.9659258262890683122, 1.000000000000000000, 0.9659258262890683122, 1.000000000000000000, 0.9659258262890683122, 1.000000000000000000, 0.9659258262890683122, 1.000000000000000000, 0.9659258262890683122, 1.000000000000000000, 0.9659258262890683122, 1.000000000000000000, 0.9659258262890683122, 1.000000000000000000, 0.9659258262890683122, 1.000000000000000000, 0.9659258262890683122, 1.000000000000000000, 0.9659258262890683122, 1.000000000000000000, 0.9659258262890683122, 1.000000000000000000, 0.9659258262890683122, 1.000000000000000000, 0.9659258262890683122, 1.000000000000000000, 0.9659258262890683122, 1.000000000000000000, 0.9659258262890683122, 1.000000000000000000, 0.9659258262890683122, 1.000000000000000000, 0.9659258262890683122, 1.000000000000000000, 0.9659258262890683122, 1.000000000000000000, 0.9659258262890683122, 1.000000000000000000, 0.9659258262890683122, 1.000000000000000000, 0.9659258262890683122, 1.000000000000000000, 0.9659258262890683122, 1.000000000000000000, 0.9659258262890683122, 1.000000000000000000, 0.9659258262890683122, 1.000000000000000000, 0.9659258262890683122, 1.000000000000000000, 0.9659258262890683122, 1.000000000000000000, 0.9659258262890683122, 1.000000000000000000, 0.9659258262890683122, 1.000000000000000000, 0.9659258262890683122, 1.000000000000000000, 0.9659258262890683122, 1.000000000000000000, 0.9659258262890683122, 1.000000000000000000, 0.9659258262890683122, 1.000000000000000000, 0.9659258262890683122, 1.000000000000000000, 0.9659258262890683122, 1.000000000000000000, 0.9659258262890683122, 1.000000000000000000, 0.9659258262890683122, 1.000000000000000000, 0.9659258262890683122, 1.000000000000000000, 0.9659258262890683122, 1.000000000000000000, 0.9659258262890683122, 1.000000000000000000, 0.9659258262890683122, 1.000000000000000000, 0.9659258262890683122, 1.000000000000000000, 0.9659258262890683122, 1.000000000000000000, 0.9659258262890683122, 1.000000000000000000, 0.9659258262890683122, 1.000000000000000000, 0.9659258262890683122, 1.000000000000000000, 0.9659258262890683122, 1.000000000000000000, 0.9659258262890683122, 1.000000000000000000, 0.9659258262890683122, 1.000000000000000000, 0.9659258262890683122, 1.000000000000000000, 0.9659258262890683122, 1.000000000000000000, 0.9659258262890683122, 1.000000000000000000, 0.9659258262890683122, 1.000000000000000000, 0.9659258262890683122, 1.000000000000000000, 0.9659258262890683122, 1.000000000000000000, 0.9659258262890683122, 1.000000000000000000, 0.9659258262890683122, 1.000000000000000000, 0.9659258262890683122, 1.000000000000000000, 0.9659258262890683122, 1.000000000000000000, 0.9659258262890683122, 1.000000000000000000, 0.9659258262890683122, 1.000000000000000000, 0.9659258262890683122, 1.000000000000000000, 0.9659258262890683122, 1.000000000000000000, 0.9659258262890683122, 1.000000000000000000, 0.9659258262890683122, 1.000000000000000000, 0.9659258262890683122, 1.000000000000000000, 0.9659258262890683122, 1.000000000000000000, 0.9659258262890683122, 1.000000000000000000, 0.9659258262890683122, 1.000000000000000000, 0.9659258262890683122, 1.000000000000000000, 0.9659258262890683122, 1.000000000000000000, 0.9659258262890683122, 1.000000000000000000, 0.9659258262890683122, 1.000000000000000000, 0.9659258262890683122, 1.000000000000000000, 0.9659258262890683122, 1.000000000000000000, 0.9659258262890683122, 1.000000000000000000, 0.9659258262890683122, 1.000000000000000000, 0.9659258262890683122, 1.000000000000000000, 0.9659258262890683122, 1.000000000000000000, 0.9659258262890683122, 1.000000000000000000, 0.9659258262890683122, 1.000000000000000000, 0.9659258262890683122, 1.000000000000000000, 0.9659258262890683122, 1.000000000000000000, 0.9659258262890683122, 1.000000000000000000, 0.9659258262890683122, 1.000000000000000000, 0.9659258262890683122, 1.000000000000000000, 0.9659258262890683122, 1.000000000000000000, 0.9659258262890683122, 1.000000000000000000, 0.9659258262890683122, 1.000000000000000000, 0.9659258262890683122, 1.000000000000000000, 0.9659258262890683122, 1.000000000000000000, 0.9659258262890683122, 1.000000000000000000, 0.9659258262890683122, 1.000000000000000000, 0.9659258262890683122, 1.000000000000000000, 0.9659258262890683122, 1.000000000000000000, 0.9659258262890683122, 1.000000000000000000, 0.9659258262890683122, 1.000000000000000000, 0.9659258262890683122, 1.000000000000000000, 0.9659258262890683122, 1.000000000000000000, 0.9659258262890683122, 1.000000000000000000, 0.9659258262890683122, 1.000000000000000000, 0.9659258262890683122, 1.000000000000000000, 0.9659258262890683122, 1.000000000000000000, 0.9659258262890683122, 1.000000000000000000, 0.9659258262890683122, 1.000000000000000000, 0.9659258262890683122, 1.000000000000000000, 0.9659258262890683122, 1.000000000000000000, 0.9659258262890683122, 1.000000000000000000, 0.9659258262890683122, 1.000000000000000000, 0.9659258262890683122, 1.000000000000000000, 0.9659258262890683122, 1.000000000000000000, 0.9659258262890683122, 1.000000000000000000, 0.9659258262890683122, 1.000000000000000000, 0.9659258262890683122, 1.000000000000000000, 0.9659258262890683122, 1.000000000000000000, 0.9659258262890683122, 1.000000000000000000, 0.9659258262890683122, 1.000000000000000000, 0.9659258262890683122, 1.000000000000000000, 0.9659258262890683122, 1.000000000000000000, 0.9659258262890683122, 1.000000000000000000, 0.9659258262890683122, 1.000000000000000000, 0.9659258262890683122, 1.000000000000000000, 0.9659258262890683122, 1.000000000000000000, 0.9659258262890683122, 1.000000000000000000, 0.9659258262890683122, 1.000000000000000000, 0.9659258262890683122, 1.000000000000000000, 0.9659258262890683122, 1.000000000000000000, 0.9659258262890683122, 1.000000000000000000, 0.9659258262890683122, 1.000000000000000000, 0.9659258262890683122, 1.000000000000000000, 0.9659258262890683122, 1.000000000000000000, 0.9659258262890683122, 1.000000000000000000, 0.9659258262890683122, 1.000000000000000000, 0.9659258262890683122, 1.000000000000000000, 0.9659258262890683122, 1.000000000000000000, 0.9659258262890683122, 1.000000000000000000, 0.9659258262890683122, 1.000000000000000000, 0.9659258262890683122, 1.000000000000000000, 0.9659258262890683122, 1.000000000000000000, 0.9659258262890683122, 1.000000000000000000, 0.9659258262890683122, 1.000000000000000000),
 ( 1.000000000000000000, 0.9659258262890683122, 1.000000000000000000, 0.9659258262890683122, 1.000000000000000000, 0.9659258262890683122, 1.000000000000000000, 0.9659258262890683122, 1.000000000000000000, 0.9659258262890683122, 1.000000000000000000, 0.9659258262890683122, 1.000000000000000000, 0.9659258262890683122, 1.000000000000000000, 0.9659258262890683122, 1.000000000000000000, 0.9659258262890683122, 1.000000000000000000, 0.9659258262890683122, 1.000000000000000000, 0.9659258262890683122, 1.000000000000000000, 0.9659258262890683122, 1.000000000000000000, 0.9659258262890683122, 1.000000000000000000, 0.9659258262890683122, 1.000000000000000000, 0.9659258262890683122, 1.000000000000000000, 0.9659258262890683122, 1.000000000000000000, 0.9659258262890683122, 1.000000000000000000, 0.9659258262890683122, 1.000000000000000000, 0.9659258262890683122, 1.000000000000000000, 0.9659258262890683122, 1.000000000000000000, 0.9659258262890683122, 1.000000000000000000, 0.9659258262890683122, 1.000000000000000000, 0.9659258262890683122, 1.000000000000000000, 0.9659258262890683122, 1.000000000000000000, 0.9659258262890683122, 1.000000000000000000, 0.9659258262890683122, 1.000000000000000000, 0.9659258262890683122, 1.000000000000000000, 0.9659258262890683122, 1.000000000000000000, 0.9659258262890683122, 1.000000000000000000, 0.9659258262890683122, 1.000000000000000000, 0.9659258262890683122, 1.000000000000000000, 0.9659258262890683122, 1.000000000000000000, 0.9659258262890683122, 1.000000000000000000, 0.9659258262890683122, 1.000000000000000000, 0.9659258262890683122, 1.000000000000000000, 0.9659258262890683122, 1.000000000000000000, 0.9659258262890683122, 1.000000000000000000, 0.9659258262890683122, 1.000000000000000000, 0.9659258262890683122, 1.000000000000000000, 0.9659258262890683122, 1.000000000000000000, 0.9659258262890683122, 1.000000000000000000, 0.9659258262890683122, 1.000000000000000000, 0.9659258262890683122, 1.000000000000000000, 0.9659258262890683122, 1.000000000000000000, 0.9659258262890683122, 1.000000000000000000, 0.9659258262890683122, 1.000000000000000000, 0.9659258262890683122, 1.000000000000000000, 0.9659258262890683122, 1.000000000000000000, 0.9659258262890683122, 1.000000000000000000, 0.9659258262890683122, 1.000000000000000000, 0.9659258262890683122, 1.000000000000000000, 0.9659258262890683122, 1.000000000000000000, 0.9659258262890683122, 1.000000000000000000, 0.9659258262890683122, 1.000000000000000000, 0.9659258262890683122, 1.000000000000000000, 0.9659258262890683122, 1.000000000000000000, 0.9659258262890683122, 1.000000000000000000, 0.9659258262890683122, 1.000000000000000000, 0.9659258262890683122, 1.000000000000000000, 0.9659258262890683122, 1.000000000000000000, 0.9659258262890683122, 1.000000000000000000, 0.9659258262890683122, 1.000000000000000000, 0.9659258262890683122, 1.000000000000000000, 0.9659258262890683122, 1.000000000000000000, 0.9659258262890683122, 1.000000000000000000, 0.9659258262890683122, 1.000000000000000000, 0.9659258262890683122, 1.000000000000000000, 0.9659258262890683122, 1.000000000000000000, 0.9659258262890683122, 1.000000000000000000, 0.9659258262890683122, 1.000000000000000000, 0.9659258262890683122, 1.000000000000000000, 0.9659258262890683122, 1.000000000000000000, 0.9659258262890683122, 1.000000000000000000, 0.9659258262890683122, 1.000000000000000000, 0.9659258262890683122, 1.000000000000000000, 0.9659258262890683122, 1.000000000000000000, 0.9659258262890683122, 1.000000000000000000, 0.9659258262890683122, 1.000000000000000000, 0.9659258262890683122, 1.000000000000000000, 0.9659258262890683122, 1.000000000000000000, 0.9659258262890683122, 1.000000000000000000, 0.9659258262890683122, 1.000000000000000000, 0.9659258262890683122, 1.000000000000000000, 0.9659258262890683122, 1.000000000000000000, 0.9659258262890683122, 1.000000000000000000, 0.9659258262890683122, 1.000000000000000000, 0.9659258262890683122, 1.000000000000000000, 0.9659258262890683122, 1.000000000000000000, 0.9659258262890683122, 1.000000000000000000, 0.9659258262890683122, 1.000000000000000000, 0.9659258262890683122, 1.000000000000000000, 0.9659258262890683122, 1.000000000000000000, 0.9659258262890683122, 1.000000000000000000, 0.9659258262890683122, 1.000000000000000000, 0.9659258262890683122, 1.000000000000000000, 0.9659258262890683122, 1.000000000000000000, 0.9659258262890683122, 1.000000000000000000, 0.9659258262890683122, 1.000000000000000000, 0.9659258262890683122, 1.000000000000000000, 0.9659258262890683122, 1.000000000000000000, 0.9659258262890683122, 1.000000000000000000, 0.9659258262890683122, 1.000000000000000000, 0.9659258262890683122, 1.000000000000000000, 0.9659258262890683122, 1.000000000000000000, 0.9659258262890683122, 1.000000000000000000, 0.9659258262890683122, 1.000000000000000000, 0.9659258262890683122, 1.000000000000000000, 0.9659258262890683122, 1.000000000000000000, 0.9659258262890683122, 1.000000000000000000, 0.9659258262890683122, 1.000000000000000000, 0.9659258262890683122, 1.000000000000000000, 0.9659258262890683122, 1.000000000000000000, 0.9659258262890683122, 1.000000000000000000, 0.9659258262890683122, 1.000000000000000000, 0.9659258262890683122, 1.000000000000000000, 0.9659258262890683122, 1.000000000000000000, 0.9659258262890683122, 1.000000000000000000, 0.9659258262890683122, 1.000000000000000000, 0.9659258262890683122, 1.000000000000000000, 0.9659258262890683122, 1.000000000000000000, 0.9659258262890683122, 1.000000000000000000, 0.9659258262890683122, 1.000000000000000000, 0.9659258262890683122, 1.000000000000000000, 0.9659258262890683122, 1.000000000000000000, 0.9659258262890683122, 1.000000000000000000, 0.9659258262890683122, 1.000000000000000000, 0.9659258262890683122, 1.000000000000000000, 0.9659258262890683122, 1.000000000000000000, 0.9659258262890683122, 1.000000000000000000, 0.9659258262890683122, 1.000000000000000000, 0.9659258262890683122, 1.000000000000000000, 0.9659258262890683122, 1.000000000000000000, 0.9659258262890683122, 1.000000000000000000, 0.9659258262890683122, 1.000000000000000000, 0.9659258262890683122, 1.000000000000000000, 0.9659258262890683122, 1.000000000000000000, 0.9659258262890683122, 1.000000000000000000, 0.9659258262890683122, 1.000000000000000000, 0.9659258262890683122, 1.000000000000000000, 0.9659258262890683122, 1.000000000000000000, 0.9659258262890683122, 1.000000000000000000, 0.9659258262890683122, 1.000000000000000000, 0.9659258262890683122, 1.000000000000000000, 0.9659258262890683122, 1.000000000000000000, 0.9659258262890683122, 1.000000000000000000, 0.9659258262890683122, 1.000000000000000000, 0.9659258262890683122, 1.000000000000000000, 0.9659258262890683122, 1.000000000000000000, 0.9659258262890683122, 1.000000000000000000, 0.9659258262890683122, 1.000000000000000000, 0.9659258262890683122, 1.000000000000000000, 0.9659258262890683122, 1.000000000000000000, 0.9659258262890683122, 1.000000000000000000, 0.9659258262890683122, 1.000000000000000000, 0.9659258262890683122, 1.000000000000000000, 0.9659258262890683122, 1.000000000000000000, 0.9659258262890683122, 1.000000000000000000, 0.9659258262890683122, 1.000000000000000000, 0.9659258262890683122, 1.000000000000000000, 0.9659258262890683122, 1.000000000000000000, 0.9659258262890683122, 1.000000000000000000, 0.9659258262890683122, 1.000000000000000000) ) ) 
 REPRESENTATION_ITEM ( '' )  SURFACE ( )  );
#75261 = DIRECTION ( 'NONE',  ( -1.257402221000611116E-16, 1.000000000000000000, 0.000000000000000000 ) ) ;
#75262 = CARTESIAN_POINT ( 'NONE',  ( 19.84674366389459621, 48.50893115100078745, 7.409399052514197653E-17 ) ) ;
#75263 = AXIS2_PLACEMENT_3D ( 'NONE', #28719, #89713, #29208 ) ;
#75264 = CARTESIAN_POINT ( 'NONE',  ( 15.44008868035555793, 36.39701867748816966, -9.422509992056140149 ) ) ;
#75265 = UNCERTAINTY_MEASURE_WITH_UNIT (LENGTH_MEASURE( 1.000000000000000082E-05 ), #40154, 'distance_accuracy_value', 'NONE');
#75266 = TOROIDAL_SURFACE ( 'NONE', #24176, 1.000000000000000000, 0.5000000000000000000 ) ;
#75267 = EDGE_LOOP ( 'NONE', ( #94632, #87447, #82551, #80304 ) ) ;
#75268 = CARTESIAN_POINT ( 'NONE',  ( 6.565887622018943937, 65.16530133659709634, 12.81628187352647430 ) ) ;
#75269 = FACE_OUTER_BOUND ( 'NONE', #36184, .T. ) ;
#75270 = CARTESIAN_POINT ( 'NONE',  ( 17.20831665107776587, 4.133931151000785675, -7.208316651077762316 ) ) ;
#75271 = CARTESIAN_POINT ( 'NONE',  ( 13.43411237798105340, 40.58196800326375353, 12.81628187352647963 ) ) ;
#75273 = CARTESIAN_POINT ( 'NONE',  ( 12.63842701281683034, 37.46726448433411605, 9.846743663894596210 ) ) ;
#75272 = CARTESIAN_POINT ( 'NONE',  ( -4.164238869374099927, 67.01208216824728936, 3.795296366450308767 ) ) ;
#75274 = CARTESIAN_POINT ( 'NONE',  ( -35.44000000000001194, 93.50000000000000000, -10.09898361729590199 ) ) ;
#75275 = CARTESIAN_POINT ( 'NONE',  ( 22.26659068614894466, 33.88708216824730357, 7.082119434687054849 ) ) ;
#75276 = CARTESIAN_POINT ( 'NONE',  ( 10.00000000000000000, 40.55374883491397497, -14.16423886937410082 ) ) ;
#75277 = CARTESIAN_POINT ( 'NONE',  ( 19.84674366389459266, 53.30059781766744464, 2.638427012816836559 ) ) ;
#75278 = COLOUR_RGB ( '', 0.31764706, 0.68627451, 0.89019608) ;
#75279 = CARTESIAN_POINT ( 'NONE',  ( 6.507517414235627129, -58.30789062356495833, -2.499999999999999112 ) ) ;
#75280 = CARTESIAN_POINT ( 'NONE',  ( 17.96484262340118221, 36.18868534415484106, -7.964842623401177768 ) ) ;
#75281 = CARTESIAN_POINT ( 'NONE',  ( -0.8801773607110991993, 67.85535201082151957, -2.915334737309923874 ) ) ;
#75282 = ORIENTED_EDGE ( 'NONE', *, *, #18314, .T. ) ;
#75283 = CARTESIAN_POINT ( 'NONE',  ( -1.099225684535947600, 64.54030133659709634, 6.408140936763237150 ) ) ;
#75284 = AXIS2_PLACEMENT_3D ( 'NONE', #25608, #95569, #12061 ) ;
#75285 = VERTEX_POINT ( 'NONE', #39569 ) ;
#75286 = CARTESIAN_POINT ( 'NONE',  ( 1.472469842513823179, 0.5922644843341181575, -4.923371831947296329 ) ) ;
#75287 = VERTEX_POINT ( 'NONE', #45575 ) ;
#75288 = CARTESIAN_POINT ( 'NONE',  ( -4.164238869374099039, 11.80374883491396965, 8.674139862899312516E-16 ) ) ;
#75289 = CARTESIAN_POINT ( 'NONE',  ( 7.361572987183170547, 12.05059781766744997, 9.846743663894590881 ) ) ;
#75290 = CARTESIAN_POINT ( 'NONE',  ( 10.00000000000000178, 34.31368534415484106, 10.88017736071110342 ) ) ;
#75291 = EDGE_CURVE ( 'NONE', #70287, #79425, #1580, .T. ) ;
#75292 = ORIENTED_EDGE ( 'NONE', *, *, #90022, .F. ) ;
#75293 = CARTESIAN_POINT ( 'NONE',  ( -0.8801773607111008646, 23.27201867748817676, 2.915334737309923430 ) ) ;
#75294 = VERTEX_POINT ( 'NONE', #93533 ) ;
#75295 = CARTESIAN_POINT ( 'NONE',  ( 20.88017736071110875, 30.77201867748816966, -2.915334737309920765 ) ) ;
#75296 = FILL_AREA_STYLE ('',( #68306 ) ) ;
#75297 = ORIENTED_EDGE ( 'NONE', *, *, #96550, .T. ) ;
#75298 = ORIENTED_EDGE ( 'NONE', *, *, #13814, .T. ) ;
#75299 = CARTESIAN_POINT ( 'NONE',  ( 7.084665262690076126, 67.02201867748817676, -10.88017736071110164 ) ) ;
#75300 = DIRECTION ( 'NONE',  ( -0.000000000000000000, 0.000000000000000000, 1.000000000000000000 ) ) ;
#75302 = DIRECTION ( 'NONE',  ( -1.000000000000000000, 0.000000000000000000, 0.000000000000000000 ) ) ;
#75301 = CARTESIAN_POINT ( 'NONE',  ( 0.5774900079438590739, 17.64701867748817321, -5.440088680355550821 ) ) ;
#75303 = CARTESIAN_POINT ( 'NONE',  ( 17.20831665107776587, 4.133931151000785675, -7.208316651077762316 ) ) ;
#75304 = CARTESIAN_POINT ( 'NONE',  ( 20.88017736071110164, 20.35535201082150891, 2.915334737309930979 ) ) ;
#75305 = COLOUR_RGB ( '', 0.72549020, 0.75294118, 0.79215686) ;
#75306 = ORIENTED_EDGE ( 'NONE', *, *, #16941, .T. ) ;
#75307 = EDGE_CURVE ( 'NONE', #66682, #14813, #64123, .T. ) ;
#75308 = CARTESIAN_POINT ( 'NONE',  ( 3.591859063236761518, 54.95696800326376064, 11.09922568453594849 ) ) ;
#75309 = CARTESIAN_POINT ( 'NONE',  ( 19.42250999205614548, 45.98035201082150536, -5.440088680355545492 ) ) ;
#75310 = CARTESIAN_POINT ( 'NONE',  ( -1.926860441876564023, 22.87045670184114599, 3.195792623639529761 ) ) ;
#75311 = EDGE_CURVE ( 'NONE', #43600, #85662, #33789, .T. ) ;
#75312 = CARTESIAN_POINT ( 'NONE',  ( 22.81628187352648496, 61.83196800326376774, -3.434112377981050290 ) ) ;
#75313 = CARTESIAN_POINT ( 'NONE',  ( 15.44008868035555793, 51.39701867748816966, -9.422509992056140149 ) ) ;
#75314 = CARTESIAN_POINT ( 'NONE',  ( 22.81628187352647785, 6.623634669930420493, 6.195893100308588602E-16 ) ) ;
#75315 = DIRECTION ( 'NONE',  ( -0.2840153447039234780, 0.000000000000000000, 0.9588197348681928300 ) ) ;
#75316 = CARTESIAN_POINT ( 'NONE',  ( 14.92337183194729633, 12.67559781766745353, 8.527530157486181039 ) ) ;
#75317 = DIRECTION ( 'NONE',  ( 0.000000000000000000, 0.000000000000000000, 1.000000000000000000 ) ) ;
#75318 = CARTESIAN_POINT ( 'NONE',  ( 0.6178305044545838731, 4.748634669930420493, 9.382169495545420901 ) ) ;
#75320 = CARTESIAN_POINT ( 'NONE',  ( 12.63842701281683034, 62.46726448433410894, 9.846743663894596210 ) ) ;
#75319 = CARTESIAN_POINT ( 'NONE',  ( 6.349999999999995204, -97.00000000000000000, 3.750000000000000000 ) ) ;
#75321 = CARTESIAN_POINT ( 'NONE',  ( 7.084665262690076126, 42.02201867748816966, -10.88017736071110164 ) ) ;
#75322 = CARTESIAN_POINT ( 'NONE',  ( 7.361572987183169658, 49.96726448433410894, -9.846743663894592657 ) ) ;
#75323 = CYLINDRICAL_SURFACE ( 'NONE', #85475, 0.5000000000000004441 ) ;
#75324 = CARTESIAN_POINT ( 'NONE',  ( 10.00000000000000178, 22.25893115100078745, 9.846743663894594434 ) ) ;
#75325 = CARTESIAN_POINT ( 'NONE',  ( 2.791683348922237240, 10.38393115100078390, -7.208316651077763204 ) ) ;
#75327 = VERTEX_POINT ( 'NONE', #71543 ) ;
#75326 = CARTESIAN_POINT ( 'NONE',  ( -1.099225684535947600, -1.293031996736246469, -6.408140936763238038 ) ) ;
#75328 = CIRCLE ( 'NONE', #38589, 2.750000000000002665 ) ;
#75329 = CARTESIAN_POINT ( 'NONE',  ( 10.00000000000000178, 4.313685344154837509, 10.88017736071110342 ) ) ;
#75330 = CARTESIAN_POINT ( 'NONE',  ( 19.84674366389459621, 58.50893115100078745, 7.409399052514197653E-17 ) ) ;
#75331 = CARTESIAN_POINT ( 'NONE',  ( 4.191189844333915282, -2.692444605285015946, -2.500000000000000888 ) ) ;
#75332 = CARTESIAN_POINT ( 'NONE',  ( -0.8801773607110991993, 2.855352010821504471, -2.915334737309923874 ) ) ;
#75333 = CARTESIAN_POINT ( 'NONE',  ( 2.791683348922240793, 51.63393115100078745, 7.208316651077764092 ) ) ;
#75334 = LINE ( 'NONE', #37856, #13660 ) ;
#75335 = CARTESIAN_POINT ( 'NONE',  ( -0.8801773607111008646, 3.272018677488171434, 2.915334737309923430 ) ) ;
#75336 = CARTESIAN_POINT ( 'NONE',  ( 6.579634127946608402, -87.99828267815712479, 2.500000000000000000 ) ) ;
#75337 = CARTESIAN_POINT ( 'NONE',  ( 15.44008868035555793, 21.39701867748817321, -9.422509992056140149 ) ) ;
#75338 = CARTESIAN_POINT ( 'NONE',  ( 6.204703633549690345, 55.76208216824730357, -14.16423886937410259 ) ) ;
#75340 = CARTESIAN_POINT ( 'NONE',  ( 14.04391541078763161, 15.00000000000000000, 3.608107528142933340 ) ) ;
#75339 = CARTESIAN_POINT ( 'NONE',  ( 20.36894250292379738, 64.92874883491397497, -10.36894250292379027 ) ) ;
#75341 = CARTESIAN_POINT ( 'NONE',  ( 1.472469842513823179, 5.592264484334118713, -4.923371831947296329 ) ) ;
#75342 = EDGE_CURVE ( 'NONE', #24454, #38399, #14707, .T. ) ;
#75343 = TOROIDAL_SURFACE ( 'NONE', #315, 14.49999999999999822, 0.5000000000000000000 ) ;
#75344 = CARTESIAN_POINT ( 'NONE',  ( 14.92337183194729988, 19.34226448433411960, -8.527530157486177487 ) ) ;
#75345 = CARTESIAN_POINT ( 'NONE',  ( -2.816281873526473856, 14.33196800326375531, 3.434112377981055619 ) ) ;
#75346 = EDGE_LOOP ( 'NONE', ( #31324, #66797, #71026, #94578 ) ) ;
#75347 = CARTESIAN_POINT ( 'NONE',  ( -14.94699059465102664, 0.5000000000000004441, 1.259949270174715696 ) ) ;
#75348 = EDGE_CURVE ( 'NONE', #93129, #97596, #72496, .T. ) ;
#75349 = DIRECTION ( 'NONE',  ( -0.6883545756937646809, -0.000000000000000000, 0.7253743710122776411 ) ) ;
#75350 = CARTESIAN_POINT ( 'NONE',  ( 19.84674366389459266, 63.30059781766745886, 2.638427012816836559 ) ) ;
#75351 = CARTESIAN_POINT ( 'NONE',  ( 24.16423886937410614, 9.512082168247301794, -3.795296366450302550 ) ) ;
#75352 = CARTESIAN_POINT ( 'NONE',  ( 17.20831665107776587, 29.13393115100078390, -7.208316651077762316 ) ) ;
#75353 = CARTESIAN_POINT ( 'NONE',  ( -13.14228782657345107, 0.5000000000000004441, 7.230509711182143917 ) ) ;
#75354 = VERTEX_POINT ( 'NONE', #26511 ) ;
#75355 = CARTESIAN_POINT ( 'NONE',  ( -4.164238869374098151, 41.59541550158061796, -3.795296366450310543 ) ) ;
#75356 = B_SPLINE_SURFACE_WITH_KNOTS ( 'NONE', 3, 1, ( 
 ( #41660, #3655 ),
 ( #34612, #87623 ),
 ( #95630, #42625 ),
 ( #59094, #30073 ),
 ( #28104, #82095 ) ),
 .UNSPECIFIED., .F., .F., .F.,
 ( 4, 1, 4 ),
 ( 2, 2 ),
 ( 0.000000000000000000, 0.4657625508283478322, 1.000000000000000000 ),
 ( 0.000000000000000000, 1.000000000000000000 ),
 .UNSPECIFIED. ) ;
#75357 = CARTESIAN_POINT ( 'NONE',  ( 19.84674366389459266, 13.30059781766745353, 2.638427012816836559 ) ) ;
#75359 = CARTESIAN_POINT ( 'NONE',  ( 6.829574850505126804, -88.00372650098204019, 2.750000000000002665 ) ) ;
#75358 = LINE ( 'NONE', #28861, #51443 ) ;
#75360 = CARTESIAN_POINT ( 'NONE',  ( 7.084665262690076126, 29.10535201082150181, 10.88017736071109987 ) ) ;
#75361 = CARTESIAN_POINT ( 'NONE',  ( 22.81628187352648496, 56.83196800326374643, -3.434112377981050290 ) ) ;
#75362 = CARTESIAN_POINT ( 'NONE',  ( 22.81628187352647785, 31.41530133659709279, 3.434112377981063169 ) ) ;
#75363 = CARTESIAN_POINT ( 'NONE',  ( 10.00000000000000000, -0.2410688489992152128, -9.846743663894594434 ) ) ;
#75364 = ORIENTED_EDGE ( 'NONE', *, *, #13059, .F. ) ;
#75365 = FACE_OUTER_BOUND ( 'NONE', #38707, .T. ) ;
#75366 = CARTESIAN_POINT ( 'NONE',  ( 4.326345305608627179, 0.000000000000000000, 3.319721512309613320 ) ) ;
#75367 = CARTESIAN_POINT ( 'NONE',  ( 10.00000000000000178, 38.05374883491396787, 14.16423886937410082 ) ) ;
#75368 = CARTESIAN_POINT ( 'NONE',  ( 7.084665262690076126, 7.022018677488169658, -10.88017736071110164 ) ) ;
#75369 = CARTESIAN_POINT ( 'NONE',  ( 0.5774900079438590739, 17.64701867748817321, -5.440088680355550821 ) ) ;
#75370 = CARTESIAN_POINT ( 'NONE',  ( -13.07964015051230788, 0.2306972965111898921, 7.222261988160647128 ) ) ;
#75371 = CARTESIAN_POINT ( 'NONE',  ( -13.69999999999999751, 99.99999999999998579, 8.000000000000000000 ) ) ;
#75372 = CARTESIAN_POINT ( 'NONE',  ( 15.44008868035555260, 54.73035201082150536, 9.422509992056143702 ) ) ;
#75373 = CARTESIAN_POINT ( 'NONE',  ( 10.00000000000000000, 61.81368534415484106, -10.88017736071110342 ) ) ;
#75374 = CARTESIAN_POINT ( 'NONE',  ( 10.00000000000000000, 27.87363466993042138, -12.81628187352647608 ) ) ;
#75375 = CARTESIAN_POINT ( 'NONE',  ( 15.64039516285221154, 89.00000000000000000, 9.500000000000000000 ) ) ;
#75376 = CARTESIAN_POINT ( 'NONE',  ( -3.115783986955356522, 15.00000000000000000, -14.16128137375399554 ) ) ;
#75377 = CARTESIAN_POINT ( 'NONE',  ( 2.791683348922237240, 20.38393115100078745, -7.208316651077763204 ) ) ;
#75378 = CARTESIAN_POINT ( 'NONE',  ( -0.8801773607110991993, 57.85535201082149825, -2.915334737309923874 ) ) ;
#75379 = CARTESIAN_POINT ( 'NONE',  ( -2.816281873526471635, 13.91530133659708746, -3.434112377981056508 ) ) ;
#75380 = CARTESIAN_POINT ( 'NONE',  ( 7.361572987183170547, 2.050597817667451750, 9.846743663894590881 ) ) ;
#75381 = CARTESIAN_POINT ( 'NONE',  ( 10.00000000000000178, 4.313685344154837509, 10.88017736071110342 ) ) ;
#75382 = CARTESIAN_POINT ( 'NONE',  ( 5.076628168052704559, 40.17559781766745175, -8.527530157486179263 ) ) ;
#75383 = CARTESIAN_POINT ( 'NONE',  ( 0.6178305044545838731, 59.74863466993041783, 9.382169495545420901 ) ) ;
#75384 = CARTESIAN_POINT ( 'NONE',  ( 1.472469842513823179, 15.59226448433411960, -4.923371831947296329 ) ) ;
#75385 = CARTESIAN_POINT ( 'NONE',  ( -2.266590686148945544, 1.387082168247301128, -7.082119434687050408 ) ) ;
#75386 = LINE ( 'NONE', #62716, #46103 ) ;
#75387 = CARTESIAN_POINT ( 'NONE',  ( 19.42250999205614193, 30.14701867748817321, 5.440088680355555262 ) ) ;
#75389 = CARTESIAN_POINT ( 'NONE',  ( 17.08211943468705130, 28.47041550158063572, 12.26659068614894998 ) ) ;
#75388 = CARTESIAN_POINT ( 'NONE',  ( 0.5774900079438607392, 3.480352010821504027, 5.440088680355550821 ) ) ;
#75390 = CARTESIAN_POINT ( 'NONE',  ( 10.00000000000000178, 47.25893115100078745, 9.846743663894594434 ) ) ;
#75391 = CARTESIAN_POINT ( 'NONE',  ( 2.035157376598824452, 33.68868534415484106, 7.964842623401179544 ) ) ;
#75392 = CARTESIAN_POINT ( 'NONE',  ( 7.084665262690076126, 12.02201867748817321, -10.88017736071110164 ) ) ;
#75393 = ORIENTED_EDGE ( 'NONE', *, *, #19435, .T. ) ;
#75394 = CARTESIAN_POINT ( 'NONE',  ( 15.44008868035555793, 21.39701867748817321, -9.422509992056140149 ) ) ;
#75395 = CARTESIAN_POINT ( 'NONE',  ( 16.40814093676323893, 40.79030133659708923, 11.09922568453595026 ) ) ;
#75396 = ADVANCED_FACE ( 'NONE', ( #79524 ), #50003, .F. ) ;
#75397 = CARTESIAN_POINT ( 'NONE',  ( 4.559911319644449179, 48.89701867748817676, 9.422509992056141925 ) ) ;
#75399 = CARTESIAN_POINT ( 'NONE',  ( -0.8801773607111008646, 38.27201867748816255, 2.915334737309923430 ) ) ;
#75398 = CARTESIAN_POINT ( 'NONE',  ( 24.35999999999999233, 37.99999999999997868, 10.00000000000000000 ) ) ;
#75400 = TOROIDAL_SURFACE ( 'NONE', #11521, 1.499999999999996669, 0.5000000000000000000 ) ;
#75401 = EDGE_LOOP ( 'NONE', ( #67646, #52454, #82222, #4597, #39163, #11115 ) ) ;
#75402 = CARTESIAN_POINT ( 'NONE',  ( 7.361572987183170547, 57.05059781766744464, 9.846743663894590881 ) ) ;
#75403 = CARTESIAN_POINT ( 'NONE',  ( 2.035157376598822676, 42.43868534415483396, -7.964842623401177768 ) ) ;
#75404 = CARTESIAN_POINT ( 'NONE',  ( 4.920853330076631060, -13.83152733636334020, 4.000000000001609379 ) ) ;
#75405 = DIRECTION ( 'NONE',  ( -0.000000000000000000, 0.000000000000000000, 1.000000000000000000 ) ) ;
#75406 = CARTESIAN_POINT ( 'NONE',  ( 20.03932841506543383, 30.62161441960502373, -6.397827110478934820 ) ) ;
#75407 = CARTESIAN_POINT ( 'NONE',  ( -0.3689425029237881626, 47.42874883491396787, 10.36894250292379027 ) ) ;
#75408 = CARTESIAN_POINT ( 'NONE',  ( 19.42250999205614548, 55.98035201082150536, -5.440088680355545492 ) ) ;
#75409 = EDGE_CURVE ( 'NONE', #67057, #83368, #71048, .T. ) ;
#75410 = CARTESIAN_POINT ( 'NONE',  ( 13.99999999999999822, 60.50000000000000711, -6.000000000000000000 ) ) ;
#75411 =( GEOMETRIC_REPRESENTATION_CONTEXT ( 3 ) GLOBAL_UNCERTAINTY_ASSIGNED_CONTEXT ( ( #63188 ) ) GLOBAL_UNIT_ASSIGNED_CONTEXT ( ( #49725, #34724, #94749 ) ) REPRESENTATION_CONTEXT ( 'NONE', 'WORKASPACE' ) );
#75412 = CARTESIAN_POINT ( 'NONE',  ( -5.200846386093611606, 0.000000000000000000, -1.639820566681014391 ) ) ;
#75413 = CARTESIAN_POINT ( 'NONE',  ( 19.84674366389459266, 58.71726448433411605, -2.638427012816827677 ) ) ;
#75414 = VECTOR ( 'NONE', #64120, 1000.000000000000000 ) ;
#75415 =( NAMED_UNIT ( * ) PLANE_ANGLE_UNIT ( ) SI_UNIT ( $, .RADIAN. ) );
#75416 = CARTESIAN_POINT ( 'NONE',  ( 0.1532563361054100626, 35.80059781766745175, -2.638427012816831230 ) ) ;
#75417 = ORIENTED_EDGE ( 'NONE', *, *, #67842, .T. ) ;
#75418 = AXIS2_PLACEMENT_3D ( 'NONE', #25138, #3119, #87087 ) ;
#75419 = CARTESIAN_POINT ( 'NONE',  ( 18.52753015748618282, 38.92559781766745175, -4.923371831947291888 ) ) ;
#75420 = CARTESIAN_POINT ( 'NONE',  ( 3.434112377981054287, -17.33469866340290721, -12.81628187352647608 ) ) ;
#75421 = CARTESIAN_POINT ( 'NONE',  ( 2.035157376598822676, 22.43868534415483396, -7.964842623401177768 ) ) ;
#75422 = CARTESIAN_POINT ( 'NONE',  ( 18.52753015748617571, 23.09226448433411960, 4.923371831947298993 ) ) ;
#75423 = ADVANCED_FACE ( 'NONE', ( #78538 ), #10529, .T. ) ;
#75424 = CARTESIAN_POINT ( 'NONE',  ( -1.099225684535947600, 24.54030133659708923, 6.408140936763237150 ) ) ;
#75426 = CARTESIAN_POINT ( 'NONE',  ( 20.88017736071110164, 60.35535201082151957, 2.915334737309930979 ) ) ;
#75425 = CARTESIAN_POINT ( 'NONE',  ( 4.559911319644449179, 68.89701867748817676, 9.422509992056141925 ) ) ;
#75428 = CARTESIAN_POINT ( 'NONE',  ( 4.559911319644449179, 2.230352010821504471, -9.422509992056141925 ) ) ;
#75427 = CARTESIAN_POINT ( 'NONE',  ( 20.88017736071110519, 30.56368534415484106, 2.639326808657452039E-16 ) ) ;
#75429 = CARTESIAN_POINT ( 'NONE',  ( -2.266590686148945544, 42.22041550158063217, 7.082119434687048631 ) ) ;
#75430 = AXIS2_PLACEMENT_3D ( 'NONE', #42679, #41227, #65660 ) ;
#75431 = EDGE_CURVE ( 'NONE', #80833, #14724, #84996, .T. ) ;
#75432 = CARTESIAN_POINT ( 'NONE',  ( -42.16485527613927076, 107.5383484153110061, 5.000000000000000000 ) ) ;
#75433 = VERTEX_POINT ( 'NONE', #14508 ) ;
#75434 = CARTESIAN_POINT ( 'NONE',  ( -2.816281873526473856, 19.12363466993042138, 9.499525473075851096E-16 ) ) ;
#75435 = CARTESIAN_POINT ( 'NONE',  ( 2.035157376598822676, 2.438685344154837953, -7.964842623401177768 ) ) ;
#75436 = CARTESIAN_POINT ( 'NONE',  ( 4.559911319644449179, 42.23035201082151247, -9.422509992056141925 ) ) ;
#75438 = EDGE_CURVE ( 'NONE', #24788, #55265, #34325, .T. ) ;
#75437 = DIRECTION ( 'NONE',  ( 0.000000000000000000, -1.000000000000000000, 0.000000000000000000 ) ) ;
#75439 = VERTEX_POINT ( 'NONE', #44490 ) ;
#75440 = AXIS2_PLACEMENT_3D ( 'NONE', #44019, #97553, #59524 ) ;
#75441 = CARTESIAN_POINT ( 'NONE',  ( 4.559911319644449179, 52.23035201082151247, -9.422509992056141925 ) ) ;
#75442 = CARTESIAN_POINT ( 'NONE',  ( 2.791683348922240793, 36.63393115100078035, 7.208316651077764092 ) ) ;
#75443 = CARTESIAN_POINT ( 'NONE',  ( 18.52753015748618282, 23.92559781766745530, -4.923371831947291888 ) ) ;
#75444 = CARTESIAN_POINT ( 'NONE',  ( 2.791683348922237240, 15.38393115100078212, -7.208316651077763204 ) ) ;
#75445 = CARTESIAN_POINT ( 'NONE',  ( 14.56332774647471062, 14.95077488074853456, 2.357028871694285765 ) ) ;
#75447 = DIRECTION ( 'NONE',  ( -1.000000000000000000, 0.000000000000000000, 0.000000000000000000 ) ) ;
#75446 = CARTESIAN_POINT ( 'NONE',  ( 10.00000000000000000, 9.758931151000785675, -9.846743663894594434 ) ) ;
#75448 = CARTESIAN_POINT ( 'NONE',  ( 6.284496703633148051, -36.06254290988034228, -4.000000000000000888 ) ) ;
#75450 = ORIENTED_EDGE ( 'NONE', *, *, #1622, .T. ) ;
#75449 = CARTESIAN_POINT ( 'NONE',  ( 1.472469842513823179, 36.42559781766745175, 4.923371831947296329 ) ) ;
#75451 = CARTESIAN_POINT ( 'NONE',  ( 3.591859063236761518, 54.95696800326376064, 11.09922568453594849 ) ) ;
#75452 = DIRECTION ( 'NONE',  ( 0.000000000000000000, 0.000000000000000000, 1.000000000000000000 ) ) ;
#75453 = CARTESIAN_POINT ( 'NONE',  ( 13.43411237798106583, 12.66530133659708746, -12.81628187352647252 ) ) ;
#75454 = CARTESIAN_POINT ( 'NONE',  ( 0.5774900079438607392, 58.48035201082151247, 5.440088680355550821 ) ) ;
#75455 = CARTESIAN_POINT ( 'NONE',  ( 10.00000000000000000, 35.55374883491396787, -14.16423886937410082 ) ) ;
#75456 = UNCERTAINTY_MEASURE_WITH_UNIT (LENGTH_MEASURE( 1.000000000000000082E-05 ), #47065, 'distance_accuracy_value', 'NONE');
#75457 = DIRECTION ( 'NONE',  ( -0.000000000000000000, -0.000000000000000000, 1.000000000000000000 ) ) ;
#75458 = CARTESIAN_POINT ( 'NONE',  ( -0.3689425029237881626, 32.42874883491395366, 10.36894250292379027 ) ) ;
#75459 = CARTESIAN_POINT ( 'NONE',  ( -4.164238869374099927, 47.01208216824729647, 3.795296366450308767 ) ) ;
#75460 = CARTESIAN_POINT ( 'NONE',  ( 6.204703633549690345, 7.845415501580634832, 14.16423886937410082 ) ) ;
#75462 = CARTESIAN_POINT ( 'NONE',  ( -1.926860441876563801, 37.66212336850780673, 1.004413902775740978E-15 ) ) ;
#75461 = CARTESIAN_POINT ( 'NONE',  ( -0.3689425029237898834, 11.17874883491396787, -10.36894250292378850 ) ) ;
#75463 = CARTESIAN_POINT ( 'NONE',  ( 19.42250999205614193, 50.14701867748817676, 5.440088680355555262 ) ) ;
#75464 = CARTESIAN_POINT ( 'NONE',  ( 0.2751277870542967463, 0.000000000000000000, 6.500000000000000888 ) ) ;
#75465 = CARTESIAN_POINT ( 'NONE',  ( 10.00000000000000000, 29.75893115100078745, -9.846743663894594434 ) ) ;
#75466 = B_SPLINE_CURVE_WITH_KNOTS ( 'NONE', 3,
 ( #91356, #15385, #52863, #97401, #44376, #21893, #59373, #75866, #60856, #6374 ),
 .UNSPECIFIED., .F., .F.,
 ( 4, 3, 3, 4 ),
 ( 1.011508913927958987E-17, 0.0006253016069560887779, 0.001250604074564930397, 0.002501455912506543935 ),
 .UNSPECIFIED. ) ;
#75468 = CARTESIAN_POINT ( 'NONE',  ( 0.1532563361054083140, 41.00893115100078745, 1.131784320476157264E-15 ) ) ;
#75467 = CARTESIAN_POINT ( 'NONE',  ( 0.5774900079438590739, 67.64701867748817676, -5.440088680355550821 ) ) ;
#75469 = CARTESIAN_POINT ( 'NONE',  ( -0.8801773607111008646, 18.27201867748817321, 2.915334737309923430 ) ) ;
#75470 = CARTESIAN_POINT ( 'NONE',  ( 22.81628187352648496, 61.83196800326376774, -3.434112377981050290 ) ) ;
#75471 = DIRECTION ( 'NONE',  ( 1.257568779154408793E-17, 1.000000000000000000, -0.000000000000000000 ) ) ;
#75472 = PLANE ( 'NONE',  #18689 ) ;
#75473 = EDGE_CURVE ( 'NONE', #32093, #51986, #62632, .T. ) ;
#75474 = CARTESIAN_POINT ( 'NONE',  ( 19.84674366389459266, 28.71726448433411960, -2.638427012816827677 ) ) ;
#75475 = CARTESIAN_POINT ( 'NONE',  ( 13.43411237798106583, 47.66530133659709634, -12.81628187352647252 ) ) ;
#75476 = CARTESIAN_POINT ( 'NONE',  ( 12.26659068614894466, -25.27958449841936073, -7.082119434687053960 ) ) ;
#75477 = VECTOR ( 'NONE', #58390, 1000.000000000000000 ) ;
#75478 = CARTESIAN_POINT ( 'NONE',  ( 0.5774900079438590739, 42.64701867748816966, -5.440088680355550821 ) ) ;
#75479 = CARTESIAN_POINT ( 'NONE',  ( 14.92337183194729633, 57.67559781766745886, 8.527530157486181039 ) ) ;
#75480 = CARTESIAN_POINT ( 'NONE',  ( -0.3689425029237898834, 26.17874883491396432, -10.36894250292378850 ) ) ;
#75481 = ORIENTED_EDGE ( 'NONE', *, *, #72602, .T. ) ;
#75482 = CARTESIAN_POINT ( 'NONE',  ( 0.1034006766821536916, 15.00000000000000000, -14.49963131600461352 ) ) ;
#75483 = CARTESIAN_POINT ( 'NONE',  ( 0.000000000000000000, 14.49999999999999822, 0.000000000000000000 ) ) ;
#75484 = CARTESIAN_POINT ( 'NONE',  ( 12.91533473730993009, 66.60535201082150536, -10.88017736071109987 ) ) ;
#75486 = AXIS2_PLACEMENT_3D ( 'NONE', #226, #30182, #91688 ) ;
#75485 = CARTESIAN_POINT ( 'NONE',  ( 22.26659068614895176, 64.72041550158064638, -7.082119434687042414 ) ) ;
#75487 = CARTESIAN_POINT ( 'NONE',  ( 17.20831665107776587, 64.13393115100079456, -7.208316651077762316 ) ) ;
#75488 = DIRECTION ( 'NONE',  ( 0.000000000000000000, 1.000000000000000000, 0.000000000000000000 ) ) ;
#75489 = CARTESIAN_POINT ( 'NONE',  ( 12.91533473730993009, 51.60535201082149825, -10.88017736071109987 ) ) ;
#75490 = CARTESIAN_POINT ( 'NONE',  ( 19.72487221294570858, 70.00000000000000000, 6.000000000000000000 ) ) ;
#75491 = CARTESIAN_POINT ( 'NONE',  ( 20.36894250292379382, 43.67874883491397497, 10.36894250292379205 ) ) ;
#75492 = CARTESIAN_POINT ( 'NONE',  ( 9.422509992056141925, 30.98035201082152668, -5.440088680355554374 ) ) ;
#75493 = CARTESIAN_POINT ( 'NONE',  ( 2.035157376598824452, 8.688685344154839285, 7.964842623401179544 ) ) ;
#75495 = CIRCLE ( 'NONE', #97853, 0.2499999999999995559 ) ;
#75494 = CARTESIAN_POINT ( 'NONE',  ( 2.035157376598822676, 22.43868534415483396, -7.964842623401177768 ) ) ;
#75496 = CARTESIAN_POINT ( 'NONE',  ( 19.84674366389459266, 53.30059781766744464, 2.638427012816836559 ) ) ;
#75497 = CARTESIAN_POINT ( 'NONE',  ( -2.816281873526473856, 54.12363466993041783, 9.499525473075851096E-16 ) ) ;
#75498 = DIRECTION ( 'NONE',  ( -0.000000000000000000, -1.000000000000000000, -0.000000000000000000 ) ) ;
#75499 = ORIENTED_EDGE ( 'NONE', *, *, #78931, .F. ) ;
#75500 = CARTESIAN_POINT ( 'NONE',  ( 20.88017736071110519, 15.56368534415483751, 2.639326808657452039E-16 ) ) ;
#75501 = CARTESIAN_POINT ( 'NONE',  ( 6.565887622018943937, 13.08196800326374998, -12.81628187352647608 ) ) ;
#75502 = DIRECTION ( 'NONE',  ( 0.9636304532086229502, 0.000000000000000000, -0.2672383760782571227 ) ) ;
#75503 = CARTESIAN_POINT ( 'NONE',  ( 17.20831665107776587, 49.13393115100078745, -7.208316651077762316 ) ) ;
#75504 = CARTESIAN_POINT ( 'NONE',  ( 4.559911319644449179, 38.89701867748817676, 9.422509992056141925 ) ) ;
#75505 = CARTESIAN_POINT ( 'NONE',  ( 10.00000000000000178, 15.37363466993042138, 12.81628187352647608 ) ) ;
#75507 = LINE ( 'NONE', #83014, #1715 ) ;
#75506 = CARTESIAN_POINT ( 'NONE',  ( 17.96484262340118221, 46.18868534415484106, -7.964842623401177768 ) ) ;
#75508 = EDGE_CURVE ( 'NONE', #90778, #74063, #78643, .T. ) ;
#75509 = CARTESIAN_POINT ( 'NONE',  ( 16.40814093676324603, 47.45696800326375353, -11.09922568453594671 ) ) ;
#75510 = ORIENTED_EDGE ( 'NONE', *, *, #11287, .T. ) ;
#75511 = CARTESIAN_POINT ( 'NONE',  ( 1.383448333479226466, 17.37718327197429247, -6.499999999999972466 ) ) ;
#75512 = CARTESIAN_POINT ( 'NONE',  ( 2.035157376598824452, 53.68868534415484817, 7.964842623401179544 ) ) ;
#75514 = CARTESIAN_POINT ( 'NONE',  ( -4.164238869374098151, 6.595415501580634832, -3.795296366450310543 ) ) ;
#75513 = CARTESIAN_POINT ( 'NONE',  ( 3.591859063236761518, 39.95696800326375353, 11.09922568453594849 ) ) ;
#75515 = CARTESIAN_POINT ( 'NONE',  ( 20.88017736071110519, 40.56368534415484106, 2.639326808657452039E-16 ) ) ;
#75516 = LINE ( 'NONE', #28536, #86772 ) ;
#75517 = CARTESIAN_POINT ( 'NONE',  ( 19.84674366389459266, 23.30059781766745530, 2.638427012816836559 ) ) ;
#75518 = CARTESIAN_POINT ( 'NONE',  ( 7.361572987183169658, -0.03273551566588185635, -9.846743663894592657 ) ) ;
#75519 = CARTESIAN_POINT ( 'NONE',  ( 20.36894250292379738, 44.92874883491396787, -10.36894250292379027 ) ) ;
#75520 = CARTESIAN_POINT ( 'NONE',  ( 12.25993886608607752, 0.3639311184075608718, -8.642563219313650791 ) ) ;
#75521 = TOROIDAL_SURFACE ( 'NONE', #78745, 7.250000000000002665, 0.2500000000000000000 ) ;
#75522 = EDGE_CURVE ( 'NONE', #31285, #44437, #96207, .T. ) ;
#75523 = LINE ( 'NONE', #90028, #46519 ) ;
#75524 = CARTESIAN_POINT ( 'NONE',  ( -7.366168427725257040, -80.69295184796105502, -4.000000000000000000 ) ) ;
#75525 = ORIENTED_EDGE ( 'NONE', *, *, #45198, .T. ) ;
#75526 = ORIENTED_EDGE ( 'NONE', *, *, #64113, .F. ) ;
#75527 = AXIS2_PLACEMENT_3D ( 'NONE', #50728, #66713, #88219 ) ;
#75528 = CARTESIAN_POINT ( 'NONE',  ( 10.00000000000000000, 55.55374883491396787, -14.16423886937410082 ) ) ;
#75529 = CARTESIAN_POINT ( 'NONE',  ( 24.16423886937410614, 59.30374883491397497, 8.672049930838204340E-16 ) ) ;
#75530 = CARTESIAN_POINT ( 'NONE',  ( 18.52753015748618282, 23.92559781766745530, -4.923371831947291888 ) ) ;
#75531 = CARTESIAN_POINT ( 'NONE',  ( 19.38216949554541202, 35.99863466993041072, 9.382169495545424454 ) ) ;
#75533 = CARTESIAN_POINT ( 'NONE',  ( 6.204703633549690345, 10.76208216824729824, -14.16423886937410259 ) ) ;
#75532 = CARTESIAN_POINT ( 'NONE',  ( 2.393480905993157215, 0.3640475087720930203, -14.80781041047751678 ) ) ;
#75534 = CARTESIAN_POINT ( 'NONE',  ( 12.91533473730993009, 16.60535201082150891, -10.88017736071109987 ) ) ;
#75535 = CARTESIAN_POINT ( 'NONE',  ( 6.204703633549690345, 55.76208216824730357, -14.16423886937410259 ) ) ;
#75536 = ADVANCED_FACE ( 'NONE', ( #17459 ), #62935, .T. ) ;
#75537 = EDGE_CURVE ( 'NONE', #78530, #54903, #1478, .T. ) ;
#75538 = CARTESIAN_POINT ( 'NONE',  ( 0.1532563361054083140, 46.00893115100079456, 1.131784320476157264E-15 ) ) ;
#75539 = CARTESIAN_POINT ( 'NONE',  ( 0.2751277870542978565, 12.28217586085238011, -6.500000000000002665 ) ) ;
#75540 = CARTESIAN_POINT ( 'NONE',  ( 17.20831665107776587, 29.13393115100078390, -7.208316651077762316 ) ) ;
#75541 = DIRECTION ( 'NONE',  ( 1.000000000000000000, -1.303078667400386302E-15, 0.000000000000000000 ) ) ;
#75542 = CARTESIAN_POINT ( 'NONE',  ( -8.527530157486182816, 10.59226448433412493, -4.923371831947288335 ) ) ;
#75543 = ORIENTED_EDGE ( 'NONE', *, *, #24173, .T. ) ;
#75544 = ORIENTED_EDGE ( 'NONE', *, *, #97379, .T. ) ;
#75545 = SURFACE_SIDE_STYLE ('',( #45036 ) ) ;
#75546 = ORIENTED_EDGE ( 'NONE', *, *, #25889, .F. ) ;
#75547 = CARTESIAN_POINT ( 'NONE',  ( 10.00000000000000178, 52.25893115100078745, 9.846743663894594434 ) ) ;
#75548 = CARTESIAN_POINT ( 'NONE',  ( -2.266590686148945544, 21.38708216824730357, -7.082119434687050408 ) ) ;
#75550 = CARTESIAN_POINT ( 'NONE',  ( 7.084665262690076126, 44.10535201082151247, 10.88017736071109987 ) ) ;
#75549 = CARTESIAN_POINT ( 'NONE',  ( 12.91533473730993009, 26.60535201082150536, -10.88017736071109987 ) ) ;
#75552 = CARTESIAN_POINT ( 'NONE',  ( 16.40814093676323893, 35.79030133659708923, 11.09922568453595026 ) ) ;
#75551 = CARTESIAN_POINT ( 'NONE',  ( 18.52753015748617571, 63.09226448433412315, 4.923371831947298993 ) ) ;
#75553 = CARTESIAN_POINT ( 'NONE',  ( -4.164238869374099039, 1.803748834913967647, 8.674139862899312516E-16 ) ) ;
#75554 = CARTESIAN_POINT ( 'NONE',  ( 0.5774900079438607392, 68.48035201082150536, 5.440088680355550821 ) ) ;
#75555 = TOROIDAL_SURFACE ( 'NONE', #43565, 14.49999999999999822, 0.5000000000000000000 ) ;
#75556 = EDGE_CURVE ( 'NONE', #62860, #86850, #91472, .T. ) ;
#75557 = CARTESIAN_POINT ( 'NONE',  ( 21.09922568453595559, 37.04030133659708923, -6.408140936763230044 ) ) ;
#75558 = ORIENTED_EDGE ( 'NONE', *, *, #37407, .T. ) ;
#75559 = CARTESIAN_POINT ( 'NONE',  ( 2.791683348922237240, 40.38393115100078035, -7.208316651077763204 ) ) ;
#75560 = CARTESIAN_POINT ( 'NONE',  ( 0.5774900079438590739, 12.64701867748817321, -5.440088680355550821 ) ) ;
#75561 = VERTEX_POINT ( 'NONE', #77941 ) ;
#75562 = EDGE_CURVE ( 'NONE', #75561, #87452, #40315, .T. ) ;
#75563 = CARTESIAN_POINT ( 'NONE',  ( -0.8801773607111009756, 13.06368534415483929, 1.068504757029289695E-15 ) ) ;
#75564 = VERTEX_POINT ( 'NONE', #15499 ) ;
#75565 = CARTESIAN_POINT ( 'NONE',  ( -0.8801773607111009756, 63.06368534415484106, 1.068504757029289695E-15 ) ) ;
#75566 = CARTESIAN_POINT ( 'NONE',  ( 10.00000000000000178, 54.31368534415484106, 10.88017736071110342 ) ) ;
#75567 = CARTESIAN_POINT ( 'NONE',  ( 4.559911319644449179, 67.23035201082150536, -9.422509992056141925 ) ) ;
#75568 = SURFACE_STYLE_FILL_AREA ( #6574 ) ;
#75569 = CARTESIAN_POINT ( 'NONE',  ( 0.5774900079438607392, 48.48035201082150536, 5.440088680355550821 ) ) ;
#75570 = CARTESIAN_POINT ( 'NONE',  ( -4.000000000000000000, 10.25000000000000000, 2.500000000000000000 ) ) ;
#75571 = CARTESIAN_POINT ( 'NONE',  ( 3.969999999999999751, 36.75000000000000000, 2.750000000000000000 ) ) ;
#75573 = VERTEX_POINT ( 'NONE', #53464 ) ;
#75572 = CARTESIAN_POINT ( 'NONE',  ( 11.10646695662389760, -65.08356741891232389, 4.000000000000000000 ) ) ;
#75574 = CARTESIAN_POINT ( 'NONE',  ( 10.00000000000000178, 47.25893115100078745, 9.846743663894594434 ) ) ;
#75575 = ORIENTED_EDGE ( 'NONE', *, *, #63202, .F. ) ;
#75576 = DIRECTION ( 'NONE',  ( -0.1822355254921513845, 0.000000000000000000, 0.9832549075639538394 ) ) ;
#75577 = CARTESIAN_POINT ( 'NONE',  ( -3.750000000000000000, 10.25000000000000000, -3.750000000000000000 ) ) ;
#75578 = CARTESIAN_POINT ( 'NONE',  ( -4.164238869374099039, 6.803748834913967869, 8.674139862899312516E-16 ) ) ;
#75579 = ORIENTED_EDGE ( 'NONE', *, *, #11408, .T. ) ;
#75580 = CARTESIAN_POINT ( 'NONE',  ( 10.58981376305282041, 15.00000000000000000, 9.535111140613782510 ) ) ;
#75581 = CARTESIAN_POINT ( 'NONE',  ( 0.1532563361054100626, 35.80059781766745175, -2.638427012816831230 ) ) ;
#75582 = CARTESIAN_POINT ( 'NONE',  ( 20.88017736071110875, 5.772018677488170546, -2.915334737309920765 ) ) ;
#75583 = CARTESIAN_POINT ( 'NONE',  ( 27.50000000000000355, 35.99999999999997158, -10.00000000000000000 ) ) ;
#75585 = EDGE_LOOP ( 'NONE', ( #42201, #89081, #62354, #23274, #66257 ) ) ;
#75584 = CARTESIAN_POINT ( 'NONE',  ( 10.00000000000000178, 45.37363466993041783, 12.81628187352647608 ) ) ;
#75586 = CARTESIAN_POINT ( 'NONE',  ( 9.402796353261145157, 14.49999999999999112, -11.68706210897763320 ) ) ;
#75587 = CARTESIAN_POINT ( 'NONE',  ( 12.63842701281683922, 39.55059781766744464, -9.846743663894590881 ) ) ;
#75588 = CARTESIAN_POINT ( 'NONE',  ( -7.750000000000000000, 80.07179676972448590, -4.250000000000000000 ) ) ;
#75589 = CARTESIAN_POINT ( 'NONE',  ( 6.565887622018943937, 20.16530133659708213, 12.81628187352647430 ) ) ;
#75590 = CARTESIAN_POINT ( 'NONE',  ( 19.84674366389459266, 18.30059781766745175, 2.638427012816836559 ) ) ;
#75591 = CARTESIAN_POINT ( 'NONE',  ( 0.3881751172101555181, 0.3700748648336783519, 6.487123156197995399 ) ) ;
#75592 = CARTESIAN_POINT ( 'NONE',  ( 10.00000000000000178, 0.3736346699304200492, 12.81628187352647608 ) ) ;
#75593 = CARTESIAN_POINT ( 'NONE',  ( 1.959929470562276732, 25.51528370094808551, -5.767676674365845635 ) ) ;
#75594 = AXIS2_PLACEMENT_3D ( 'NONE', #62899, #39915, #46908 ) ;
#75595 = ORIENTED_EDGE ( 'NONE', *, *, #54855, .F. ) ;
#75596 = EDGE_LOOP ( 'NONE', ( #4340, #95719, #52411, #17182, #83295, #79202 ) ) ;
#75597 = CARTESIAN_POINT ( 'NONE',  ( 7.084665262690076126, 24.10535201082150181, 10.88017736071109987 ) ) ;
#75598 = CARTESIAN_POINT ( 'NONE',  ( 20.36894250292379382, 13.67874883491396965, 10.36894250292379205 ) ) ;
#75599 = CARTESIAN_POINT ( 'NONE',  ( 10.00000000000000000, 29.75893115100078745, -9.846743663894594434 ) ) ;
#75600 = CARTESIAN_POINT ( 'NONE',  ( 0.1532563361054083140, 1.008931151000784787, 1.131784320476157264E-15 ) ) ;
#75602 = CARTESIAN_POINT ( 'NONE',  ( 0.000000000000000000, 15.00000000000000000, 13.75000000000001776 ) ) ;
#75601 = CARTESIAN_POINT ( 'NONE',  ( 0.6178305044545818747, 38.49863466993042493, -9.382169495545419124 ) ) ;
#75603 = CARTESIAN_POINT ( 'NONE',  ( 20.88017736071110164, 15.35535201082150358, 2.915334737309930979 ) ) ;
#75604 = LINE ( 'NONE', #76096, #77262 ) ;
#75605 = CARTESIAN_POINT ( 'NONE',  ( -2.816281873526473856, 9.331968003263753531, 3.434112377981055619 ) ) ;
#75606 = CARTESIAN_POINT ( 'NONE',  ( 10.00000000000000000, 2.873634669930420049, -12.81628187352647608 ) ) ;
#75607 = CARTESIAN_POINT ( 'NONE',  ( 18.52753015748618282, 23.92559781766745530, -4.923371831947291888 ) ) ;
#75608 = CARTESIAN_POINT ( 'NONE',  ( -10.88017736071109987, -16.72798132251182679, 2.915334737309934532 ) ) ;
#75609 = CARTESIAN_POINT ( 'NONE',  ( 10.00000000000000178, 30.37363466993042138, 12.81628187352647608 ) ) ;
#75610 = DIRECTION ( 'NONE',  ( 0.08715574274765129636, 0.9961946980917462113, 0.000000000000000000 ) ) ;
#75612 = FACE_OUTER_BOUND ( 'NONE', #28319, .T. ) ;
#75611 = CARTESIAN_POINT ( 'NONE',  ( 12.91533473730992121, 39.52201867748817676, 10.88017736071110164 ) ) ;
#75613 = CARTESIAN_POINT ( 'NONE',  ( -14.09394518620607606, 3.895088541583166744E-16, -3.407449058785548157 ) ) ;
#75614 = CARTESIAN_POINT ( 'NONE',  ( 17.62281668512002852, 28.28593319516823001, 6.499999999999993783 ) ) ;
#75615 = CARTESIAN_POINT ( 'NONE',  ( 2.035157376598824452, 38.68868534415483396, 7.964842623401179544 ) ) ;
#75616 = CARTESIAN_POINT ( 'NONE',  ( 2.035157376598822676, 47.43868534415484817, -7.964842623401177768 ) ) ;
#75617 = CARTESIAN_POINT ( 'NONE',  ( 20.15039907845753220, 60.60158574516643881, -6.262539305110077947 ) ) ;
#75618 = CARTESIAN_POINT ( 'NONE',  ( 10.00000000000000000, 61.81368534415484106, -10.88017736071110342 ) ) ;
#75619 = AXIS2_PLACEMENT_3D ( 'NONE', #22387, #82876, #37884 ) ;
#75620 = CIRCLE ( 'NONE', #37317, 0.2500000000000002220 ) ;
#75621 = CARTESIAN_POINT ( 'NONE',  ( 7.361572987183170547, 52.05059781766745175, 9.846743663894590881 ) ) ;
#75623 = DIRECTION ( 'NONE',  ( 0.000000000000000000, 1.000000000000000000, 0.000000000000000000 ) ) ;
#75622 = CARTESIAN_POINT ( 'NONE',  ( 10.00000000000000000, 6.813685344154838397, -10.88017736071110342 ) ) ;
#75624 = CARTESIAN_POINT ( 'NONE',  ( -2.816281873526473856, 9.123634669930421381, 9.499525473075851096E-16 ) ) ;
#75625 = ORIENTED_EDGE ( 'NONE', *, *, #56361, .F. ) ;
#75626 = CARTESIAN_POINT ( 'NONE',  ( 17.96484262340118221, 29.93868534415484106, 7.964842623401181321 ) ) ;
#75627 = SURFACE_STYLE_FILL_AREA ( #53612 ) ;
#75628 = CARTESIAN_POINT ( 'NONE',  ( 10.00000000000000178, 34.31368534415484106, 10.88017736071110342 ) ) ;
#75629 = CARTESIAN_POINT ( 'NONE',  ( 7.361572987183170547, 2.050597817667451750, 9.846743663894590881 ) ) ;
#75630 = CARTESIAN_POINT ( 'NONE',  ( -4.164238869374099927, 42.01208216824728936, 3.795296366450308767 ) ) ;
#75631 = CARTESIAN_POINT ( 'NONE',  ( 10.00000000000000000, 29.75893115100078745, -9.846743663894594434 ) ) ;
#75632 = CARTESIAN_POINT ( 'NONE',  ( 20.88017736071110519, 45.56368534415484106, 2.639326808657452039E-16 ) ) ;
#75633 = CARTESIAN_POINT ( 'NONE',  ( 0.2751277870542911952, 19.36607318730131055, -6.499999999999992006 ) ) ;
#75634 = FILL_AREA_STYLE ('',( #52146 ) ) ;
#75635 = EDGE_CURVE ( 'NONE', #13640, #89305, #29553, .T. ) ;
#75636 = ORIENTED_EDGE ( 'NONE', *, *, #68889, .T. ) ;
#75637 = DIRECTION ( 'NONE',  ( -0.000000000000000000, -0.000000000000000000, -1.000000000000000000 ) ) ;
#75638 = CARTESIAN_POINT ( 'NONE',  ( 18.52753015748617571, 53.09226448433412315, 4.923371831947298993 ) ) ;
#75640 = ORIENTED_EDGE ( 'NONE', *, *, #97600, .T. ) ;
#75639 = EDGE_CURVE ( 'NONE', #25555, #71703, #30795, .T. ) ;
#75641 = ORIENTED_EDGE ( 'NONE', *, *, #30643, .T. ) ;
#75642 = CARTESIAN_POINT ( 'NONE',  ( 6.204703633549690345, 25.76208216824730712, -14.16423886937410259 ) ) ;
#75643 = CARTESIAN_POINT ( 'NONE',  ( 24.16423886937410614, 24.30374883491396787, 8.672049930838204340E-16 ) ) ;
#75644 = CARTESIAN_POINT ( 'NONE',  ( 0.5774900079438607392, 58.48035201082151247, 5.440088680355550821 ) ) ;
#75645 = CARTESIAN_POINT ( 'NONE',  ( 20.36894250292379738, 64.92874883491397497, -10.36894250292379027 ) ) ;
#75646 = CARTESIAN_POINT ( 'NONE',  ( 10.00000000000000178, 52.25893115100078745, 9.846743663894594434 ) ) ;
#75647 = CARTESIAN_POINT ( 'NONE',  ( -9.823916613453683055, -32.16564667760975027, 4.000000000000000000 ) ) ;
#75649 = CARTESIAN_POINT ( 'NONE',  ( 19.38216949554541202, 25.99863466993042138, 9.382169495545424454 ) ) ;
#75648 = CARTESIAN_POINT ( 'NONE',  ( 15.44008868035555793, 41.39701867748817676, -9.422509992056140149 ) ) ;
#75650 = CARTESIAN_POINT ( 'NONE',  ( 24.16423886937410614, 14.51208216824730179, -3.795296366450302550 ) ) ;
#75651 = CARTESIAN_POINT ( 'NONE',  ( 12.91533473730993009, 11.60535201082150714, -10.88017736071109987 ) ) ;
#75652 = ADVANCED_FACE ( 'NONE', ( #30958 ), #38973, .T. ) ;
#75653 = CARTESIAN_POINT ( 'NONE',  ( 2.035157376598824452, 23.68868534415484461, 7.964842623401179544 ) ) ;
#75654 =( BOUNDED_CURVE ( )  B_SPLINE_CURVE ( 2, ( #30922, #68455, #98977, #91438, #7953, #69429, #60932, #53934, #52452 ),
 .UNSPECIFIED., .F., .F. ) 
 B_SPLINE_CURVE_WITH_KNOTS ( ( 3, 2, 2, 2, 3 ),
 ( 0.3329980797973742246, 0.3333333333333333703, 0.3392857142857143016, 0.3452380952380952328, 0.3455733487740543786 ),
 .UNSPECIFIED. ) 
 CURVE ( )  GEOMETRIC_REPRESENTATION_ITEM ( )  RATIONAL_B_SPLINE_CURVE ( ( 0.9963778908391760503, 0.9980808541467920403, 1.000000000000000000, 0.9659258262890682012, 1.000000000000000000, 0.9659258262890682012, 1.000000000000000000, 0.9980808541467920403, 0.9963778908391759392 ) ) 
 REPRESENTATION_ITEM ( '' )  );
#75655 = CARTESIAN_POINT ( 'NONE',  ( 19.84674366389459621, 53.50893115100078745, 7.409399052514197653E-17 ) ) ;
#75656 = CARTESIAN_POINT ( 'NONE',  ( 19.42250999205614548, 55.98035201082150536, -5.440088680355545492 ) ) ;
#75657 = CARTESIAN_POINT ( 'NONE',  ( 8.527530157486175710, -26.07440218233254470, -4.923371831947298993 ) ) ;
#75658 = ORIENTED_EDGE ( 'NONE', *, *, #12112, .T. ) ;
#75659 = DIRECTION ( 'NONE',  ( -0.000000000000000000, -0.000000000000000000, 1.000000000000000000 ) ) ;
#75660 = ORIENTED_EDGE ( 'NONE', *, *, #95525, .F. ) ;
#75661 = SURFACE_STYLE_USAGE ( .BOTH. , #45157 ) ;
#75662 = FACE_OUTER_BOUND ( 'NONE', #24499, .T. ) ;
#75663 = ORIENTED_EDGE ( 'NONE', *, *, #15488, .T. ) ;
#75664 = DIRECTION ( 'NONE',  ( -0.000000000000000000, -0.000000000000000000, 1.000000000000000000 ) ) ;
#75666 = CARTESIAN_POINT ( 'NONE',  ( 24.16423886937410614, 64.30374883491396076, 8.672049930838204340E-16 ) ) ;
#75665 = CARTESIAN_POINT ( 'NONE',  ( 13.79529636645031943, 65.34541550158063217, -14.16423886937409904 ) ) ;
#75668 = CARTESIAN_POINT ( 'NONE',  ( 19.84674366389459266, 63.30059781766745886, 2.638427012816836559 ) ) ;
#75667 = CARTESIAN_POINT ( 'NONE',  ( 5.076628168052703671, 26.84226448433411960, 8.527530157486179263 ) ) ;
#75669 = CARTESIAN_POINT ( 'NONE',  ( 21.92686044187656691, 49.95379003517448524, 3.195792623639537755 ) ) ;
#75670 = CARTESIAN_POINT ( 'NONE',  ( -0.8801773607111009756, 63.06368534415484106, 1.068504757029289695E-15 ) ) ;
#75671 = CARTESIAN_POINT ( 'NONE',  ( -12.81628187352647252, 19.33196800326376064, 3.434112377981066722 ) ) ;
#75672 = ORIENTED_EDGE ( 'NONE', *, *, #84873, .T. ) ;
#75673 = CARTESIAN_POINT ( 'NONE',  ( 22.26659068614895176, 29.72041550158063572, -7.082119434687042414 ) ) ;
#75674 = EDGE_CURVE ( 'NONE', #66451, #6038, #65838, .T. ) ;
#75675 = CARTESIAN_POINT ( 'NONE',  ( 6.204703633549690345, 40.76208216824731778, -14.16423886937410259 ) ) ;
#75676 = VERTEX_POINT ( 'NONE', #54445 ) ;
#75677 = CARTESIAN_POINT ( 'NONE',  ( 22.81628187352648496, 56.83196800326374643, -3.434112377981050290 ) ) ;
#75678 = CARTESIAN_POINT ( 'NONE',  ( 12.63842701281683922, 49.55059781766744464, -9.846743663894590881 ) ) ;
#75679 = CARTESIAN_POINT ( 'NONE',  ( 15.44008868035555260, 24.73035201082150891, 9.422509992056143702 ) ) ;
#75680 = CARTESIAN_POINT ( 'NONE',  ( 4.879999999999991900, 76.07179676972444327, -6.500000000000000888 ) ) ;
#75681 = CARTESIAN_POINT ( 'NONE',  ( -10.84451454130493708, 4.806230040756559413E-16, -9.625305416630981270 ) ) ;
#75682 = CARTESIAN_POINT ( 'NONE',  ( 17.20831665107776587, 57.88393115100078745, 7.208316651077764980 ) ) ;
#75683 = CARTESIAN_POINT ( 'NONE',  ( 1.472469842513823179, 45.59226448433412315, -4.923371831947296329 ) ) ;
#75684 = EDGE_CURVE ( 'NONE', #97143, #58843, #78438, .T. ) ;
#75686 = VERTEX_POINT ( 'NONE', #62431 ) ;
#75685 = DIRECTION ( 'NONE',  ( -1.000000000000000000, -0.000000000000000000, -0.000000000000000000 ) ) ;
#75687 = CARTESIAN_POINT ( 'NONE',  ( 17.39651004071842522, 19.08210964143329491, -6.499999999999992895 ) ) ;
#75688 = VECTOR ( 'NONE', #67155, 1000.000000000000114 ) ;
#75689 = DIRECTION ( 'NONE',  ( -0.9799247046208311440, 0.000000000000000000, 0.1993679344171901680 ) ) ;
#75690 =( LENGTH_UNIT ( ) NAMED_UNIT ( * ) SI_UNIT ( .MILLI., .METRE. ) );
#75691 = VERTEX_POINT ( 'NONE', #24467 ) ;
#75692 = CARTESIAN_POINT ( 'NONE',  ( 0.6076426042653185755, 7.375764716086007589, -6.500000000000003553 ) ) ;
#75693 = CARTESIAN_POINT ( 'NONE',  ( 1.472469842513823179, 31.42559781766745530, 4.923371831947296329 ) ) ;
#75694 = CARTESIAN_POINT ( 'NONE',  ( 0.2751277870542906956, 37.28217586085238366, -6.499999999999992006 ) ) ;
#75695 = CARTESIAN_POINT ( 'NONE',  ( -2.816281873526471635, 33.91530133659708213, -3.434112377981056508 ) ) ;
#75697 = DIRECTION ( 'NONE',  ( -0.000000000000000000, 0.000000000000000000, 1.000000000000000000 ) ) ;
#75696 = AXIS2_PLACEMENT_3D ( 'NONE', #49881, #94894, #41435 ) ;
#75698 = CARTESIAN_POINT ( 'NONE',  ( -14.82269085861165792, 15.00000000000000000, -2.299529454047158250 ) ) ;
#75699 = ORIENTED_EDGE ( 'NONE', *, *, #28828, .T. ) ;
#75700 = CARTESIAN_POINT ( 'NONE',  ( 5.076628168052704559, 55.17559781766745175, -8.527530157486179263 ) ) ;
#75701 = CARTESIAN_POINT ( 'NONE',  ( 0.1957200283969084964, 65.25733960839544068, 6.499999999999983125 ) ) ;
#75702 = CARTESIAN_POINT ( 'NONE',  ( 2.791683348922240793, 46.63393115100077324, 7.208316651077764092 ) ) ;
#75703 = CARTESIAN_POINT ( 'NONE',  ( -2.266590686148945544, 31.38708216824730002, -7.082119434687050408 ) ) ;
#75704 = CARTESIAN_POINT ( 'NONE',  ( 17.20831665107776587, 49.13393115100078745, -7.208316651077762316 ) ) ;
#75705 = CARTESIAN_POINT ( 'NONE',  ( 19.38216949554541202, 60.99863466993042493, 9.382169495545424454 ) ) ;
#75706 = CARTESIAN_POINT ( 'NONE',  ( 20.32896413005680003, 36.77164270246084499, 5.963430220938287007 ) ) ;
#75707 = CARTESIAN_POINT ( 'NONE',  ( 10.00000000000000178, 7.258931151000785675, 9.846743663894594434 ) ) ;
#75708 = CARTESIAN_POINT ( 'NONE',  ( 1.472469842513823179, 46.42559781766745175, 4.923371831947296329 ) ) ;
#75709 = CARTESIAN_POINT ( 'NONE',  ( 4.559911319644449179, 48.89701867748817676, 9.422509992056141925 ) ) ;
#75710 = CARTESIAN_POINT ( 'NONE',  ( 7.361572987183169658, 44.96726448433412315, -9.846743663894592657 ) ) ;
#75711 = DIRECTION ( 'NONE',  ( 1.000000000000000000, 0.000000000000000000, 0.000000000000000000 ) ) ;
#75712 = VERTEX_POINT ( 'NONE', #65384 ) ;
#75713 = CARTESIAN_POINT ( 'NONE',  ( 4.559911319644449179, 52.23035201082151247, -9.422509992056141925 ) ) ;
#75714 = ORIENTED_EDGE ( 'NONE', *, *, #28284, .F. ) ;
#75715 = CARTESIAN_POINT ( 'NONE',  ( -0.8801773607111009756, 18.06368534415484106, 1.068504757029289695E-15 ) ) ;
#75717 = CARTESIAN_POINT ( 'NONE',  ( 20.88017736071110519, 45.56368534415484106, 2.639326808657452039E-16 ) ) ;
#75716 = CARTESIAN_POINT ( 'NONE',  ( 21.09922568453594849, 1.206968003263753531, 6.408140936763242479 ) ) ;
#75718 = CYLINDRICAL_SURFACE ( 'NONE', #13704, 1.249999999999987121 ) ;
#75719 = DIRECTION ( 'NONE',  ( 1.000000000000000000, 0.000000000000000000, 0.000000000000000000 ) ) ;
#75721 = DIRECTION ( 'NONE',  ( -0.07626964003977962370, 0.9970872288863209532, 0.000000000000000000 ) ) ;
#75720 = CARTESIAN_POINT ( 'NONE',  ( 20.88017736071110164, 45.35535201082149115, 2.915334737309930979 ) ) ;
#75722 = CARTESIAN_POINT ( 'NONE',  ( 7.361572987183169658, 9.967264484334119601, -9.846743663894592657 ) ) ;
#75723 = ADVANCED_FACE ( 'NONE', ( #25932 ), #41211, .F. ) ;
#75724 = CARTESIAN_POINT ( 'NONE',  ( 2.791683348922240793, 36.63393115100078035, 7.208316651077764092 ) ) ;
#75725 = CARTESIAN_POINT ( 'NONE',  ( 6.000000000000000000, 11.00000000000000000, 6.000000000000000000 ) ) ;
#75726 = CARTESIAN_POINT ( 'NONE',  ( -12.26659068614894110, 22.22041550158063217, 7.082119434687058401 ) ) ;
#75727 = CARTESIAN_POINT ( 'NONE',  ( 18.52753015748617571, 63.09226448433412315, 4.923371831947298993 ) ) ;
#75728 = CARTESIAN_POINT ( 'NONE',  ( 10.00000000000000000, 6.813685344154838397, -10.88017736071110342 ) ) ;
#75729 = FACE_OUTER_BOUND ( 'NONE', #38172, .T. ) ;
#75730 = EDGE_CURVE ( 'NONE', #72124, #54543, #88192, .T. ) ;
#75731 = CARTESIAN_POINT ( 'NONE',  ( 17.08211943468705840, 20.13708216824730357, -12.26659068614894466 ) ) ;
#75732 = CARTESIAN_POINT ( 'NONE',  ( 6.204703633549690345, 52.84541550158062506, 14.16423886937410082 ) ) ;
#75733 = CARTESIAN_POINT ( 'NONE',  ( 4.559911319644449179, 7.230352010821504471, -9.422509992056141925 ) ) ;
#75734 = CARTESIAN_POINT ( 'NONE',  ( 14.92337183194729988, 29.34226448433411960, -8.527530157486177487 ) ) ;
#75735 = CARTESIAN_POINT ( 'NONE',  ( 2.035157376598822676, 27.43868534415483396, -7.964842623401177768 ) ) ;
#75736 = CARTESIAN_POINT ( 'NONE',  ( 14.92337183194729988, 49.34226448433411605, -8.527530157486177487 ) ) ;
#75738 = CARTESIAN_POINT ( 'NONE',  ( 69.60148758828984228, 0.4999999999999982792, 9.500000000000000000 ) ) ;
#75737 = CARTESIAN_POINT ( 'NONE',  ( -4.164238869374099039, 1.803748834913967647, 8.674139862899312516E-16 ) ) ;
#75739 = DIRECTION ( 'NONE',  ( 0.000000000000000000, 1.000000000000000000, -0.000000000000000000 ) ) ;
#75740 = CARTESIAN_POINT ( 'NONE',  ( -2.816281873526473856, 34.33196800326376064, 3.434112377981055619 ) ) ;
#75741 = CARTESIAN_POINT ( 'NONE',  ( 12.63842701281683034, 37.46726448433411605, 9.846743663894596210 ) ) ;
#75742 = EDGE_LOOP ( 'NONE', ( #77890, #17617, #74367, #55879 ) ) ;
#75743 = CARTESIAN_POINT ( 'NONE',  ( 17.20831665107776587, 14.13393115100078568, -7.208316651077762316 ) ) ;
#75744 = CARTESIAN_POINT ( 'NONE',  ( 10.89310702003767162, -97.65080520972955469, -4.000000000001574740 ) ) ;
#75745 = CARTESIAN_POINT ( 'NONE',  ( 19.72487221294570858, 16.86607318730074567, 6.500000000000000888 ) ) ;
#75746 = CARTESIAN_POINT ( 'NONE',  ( 2.035157376598824452, 3.688685344154837953, 7.964842623401179544 ) ) ;
#75747 = CARTESIAN_POINT ( 'NONE',  ( -4.164238869374098151, 51.59541550158063217, -3.795296366450310543 ) ) ;
#75748 = CARTESIAN_POINT ( 'NONE',  ( 4.559911319644449179, 42.23035201082151247, -9.422509992056141925 ) ) ;
#75749 = FILL_AREA_STYLE ('',( #68753 ) ) ;
#75750 = CARTESIAN_POINT ( 'NONE',  ( 1.274849032793998305, 2.555090184799397424, -6.499999999999581668 ) ) ;
#75751 = CARTESIAN_POINT ( 'NONE',  ( 5.076628168052703671, 21.84226448433411960, 8.527530157486179263 ) ) ;
#75752 = CARTESIAN_POINT ( 'NONE',  ( 2.035157376598824452, 3.688685344154837953, 7.964842623401179544 ) ) ;
#75753 = CARTESIAN_POINT ( 'NONE',  ( 7.361572987183169658, 44.96726448433412315, -9.846743663894592657 ) ) ;
#75754 = DIRECTION ( 'NONE',  ( -1.000000000000000000, -1.257402221000612102E-16, 0.000000000000000000 ) ) ;
#75755 = CARTESIAN_POINT ( 'NONE',  ( 0.1532563361054082862, 56.21726448433411605, 2.638427012816831674 ) ) ;
#75756 = CARTESIAN_POINT ( 'NONE',  ( 4.559911319644449179, 37.23035201082150536, -9.422509992056141925 ) ) ;
#75757 = ADVANCED_FACE ( 'NONE', ( #44368 ), #81380, .F. ) ;
#75758 = ORIENTED_EDGE ( 'NONE', *, *, #59560, .F. ) ;
#75759 = CARTESIAN_POINT ( 'NONE',  ( 21.09922568453594849, 56.20696800326375353, 6.408140936763242479 ) ) ;
#75760 = CARTESIAN_POINT ( 'NONE',  ( 3.014428414850134796, 4.380135511184874098, 11.24999999999999822 ) ) ;
#75761 = CIRCLE ( 'NONE', #7105, 3.699999999999999289 ) ;
#75762 = CARTESIAN_POINT ( 'NONE',  ( 18.52753015748618282, 8.925597817667451750, -4.923371831947291888 ) ) ;
#75763 = CARTESIAN_POINT ( 'NONE',  ( 21.09922568453594849, 51.20696800326375353, 6.408140936763242479 ) ) ;
#75765 = CARTESIAN_POINT ( 'NONE',  ( 2.791683348922237240, 45.38393115100079456, -7.208316651077763204 ) ) ;
#75764 = CARTESIAN_POINT ( 'NONE',  ( 4.559911319644449179, 7.230352010821505360, -9.422509992056141925 ) ) ;
#75766 = CARTESIAN_POINT ( 'NONE',  ( 1.683889348827610062E-15, 0.000000000000000000, 13.74999999999999467 ) ) ;
#75767 = AXIS2_PLACEMENT_3D ( 'NONE', #25457, #55940, #86439 ) ;
#75768 = ADVANCED_FACE ( 'NONE', ( #4907 ), #44852, .T. ) ;
#75769 = CARTESIAN_POINT ( 'NONE',  ( 24.16423886937410614, 49.51208216824730357, -3.795296366450302550 ) ) ;
#75770 = CARTESIAN_POINT ( 'NONE',  ( 10.00000000000000000, 59.75893115100078745, -9.846743663894594434 ) ) ;
#75771 = FACE_OUTER_BOUND ( 'NONE', #83926, .T. ) ;
#75772 = CARTESIAN_POINT ( 'NONE',  ( 20.88017736071110164, 55.35535201082149825, 2.915334737309930979 ) ) ;
#75773 = VECTOR ( 'NONE', #77078, 1000.000000000000114 ) ;
#75774 = CARTESIAN_POINT ( 'NONE',  ( 0.1532563361054082862, 1.217264484334117824, 2.638427012816831674 ) ) ;
#75775 =( NAMED_UNIT ( * ) PLANE_ANGLE_UNIT ( ) SI_UNIT ( $, .RADIAN. ) );
#75776 = ORIENTED_EDGE ( 'NONE', *, *, #52463, .F. ) ;
#75777 = CARTESIAN_POINT ( 'NONE',  ( 13.43411237798105340, 55.58196800326374643, 12.81628187352647963 ) ) ;
#75778 = CARTESIAN_POINT ( 'NONE',  ( 1.472469842513823179, 16.42559781766745175, 4.923371831947296329 ) ) ;
#75779 = ORIENTED_EDGE ( 'NONE', *, *, #14262, .F. ) ;
#75780 = CARTESIAN_POINT ( 'NONE',  ( -0.3689425029237881626, 2.428748834913967869, 10.36894250292379027 ) ) ;
#75781 = CARTESIAN_POINT ( 'NONE',  ( 1.472469842513823179, 0.5922644843341181575, -4.923371831947296329 ) ) ;
#75782 = CARTESIAN_POINT ( 'NONE',  ( 17.96484262340118221, 26.18868534415483396, -7.964842623401177768 ) ) ;
#75783 = CARTESIAN_POINT ( 'NONE',  ( 7.313705784284503686, 0.5000000000000004441, 13.09617149020748705 ) ) ;
#75784 = ORIENTED_EDGE ( 'NONE', *, *, #21862, .F. ) ;
#75785 = CARTESIAN_POINT ( 'NONE',  ( 15.44008868035555260, 29.73035201082150891, 9.422509992056143702 ) ) ;
#75786 = AXIS2_PLACEMENT_3D ( 'NONE', #31328, #37384, #69345 ) ;
#75787 = EDGE_CURVE ( 'NONE', #53779, #22610, #94546, .T. ) ;
#75788 = ORIENTED_EDGE ( 'NONE', *, *, #24777, .T. ) ;
#75789 = CARTESIAN_POINT ( 'NONE',  ( 12.91533473730993009, 36.60535201082151247, -10.88017736071109987 ) ) ;
#75790 = CARTESIAN_POINT ( 'NONE',  ( -6.000000000000009770, 40.99999999999999289, -6.250000000000000000 ) ) ;
#75791 = ORIENTED_EDGE ( 'NONE', *, *, #11802, .F. ) ;
#75792 = EDGE_CURVE ( 'NONE', #22141, #93500, #27521, .T. ) ;
#75793 = VERTEX_POINT ( 'NONE', #6366 ) ;
#75794 = CARTESIAN_POINT ( 'NONE',  ( 0.6178305044545818747, 13.49863466993041783, -9.382169495545419124 ) ) ;
#75795 = CARTESIAN_POINT ( 'NONE',  ( 14.35000000000000142, 98.49999999999998579, 8.000000000000000000 ) ) ;
#75796 = CARTESIAN_POINT ( 'NONE',  ( -0.8801773607111008646, 63.27201867748817676, 2.915334737309923430 ) ) ;
#75797 = SURFACE_STYLE_USAGE ( .BOTH. , #98334 ) ;
#75798 = SURFACE_STYLE_FILL_AREA ( #38308 ) ;
#75799 = CARTESIAN_POINT ( 'NONE',  ( 0.1532563361054082862, 11.21726448433411605, 2.638427012816831674 ) ) ;
#75800 = CARTESIAN_POINT ( 'NONE',  ( -0.8801773607111009756, 38.06368534415484106, 1.068504757029289695E-15 ) ) ;
#75801 = STYLED_ITEM ( 'NONE', ( #80189 ), #52070 ) ;
#75802 = VERTEX_POINT ( 'NONE', #67369 ) ;
#75803 = VERTEX_POINT ( 'NONE', #35878 ) ;
#75804 = CARTESIAN_POINT ( 'NONE',  ( 3.591859063236761518, 64.95696800326376774, 11.09922568453594849 ) ) ;
#75805 = CARTESIAN_POINT ( 'NONE',  ( -0.8801773607110991993, 47.85535201082150536, -2.915334737309923874 ) ) ;
#75806 = CARTESIAN_POINT ( 'NONE',  ( 2.148416515056634335, 7.237265733804436607, 6.499999999999997335 ) ) ;
#75807 = CARTESIAN_POINT ( 'NONE',  ( -2.816281873526473856, 59.12363466993042493, 9.499525473075851096E-16 ) ) ;
#75808 = CARTESIAN_POINT ( 'NONE',  ( -0.8801773607111008646, 63.27201867748817676, 2.915334737309923430 ) ) ;
#75809 = CARTESIAN_POINT ( 'NONE',  ( -1.099225684535947600, -0.4596986634029132657, 6.408140936763237150 ) ) ;
#75810 = FACE_OUTER_BOUND ( 'NONE', #71898, .T. ) ;
#75811 = CARTESIAN_POINT ( 'NONE',  ( 2.791683348922240793, 21.63393115100078745, 7.208316651077764092 ) ) ;
#75812 = CARTESIAN_POINT ( 'NONE',  ( 0.6178305044545838731, 54.74863466993042493, 9.382169495545420901 ) ) ;
#75813 = CARTESIAN_POINT ( 'NONE',  ( -7.750000000000000000, 1.019547802438458550, 4.000000000000000000 ) ) ;
#75814 = CARTESIAN_POINT ( 'NONE',  ( 14.92337183194729988, 9.342264484334119601, -8.527530157486177487 ) ) ;
#75816 = AXIS2_PLACEMENT_3D ( 'NONE', #56441, #48922, #57410 ) ;
#75815 = CARTESIAN_POINT ( 'NONE',  ( 0.6178305044545818747, 3.498634669930420049, -9.382169495545419124 ) ) ;
#75818 = CARTESIAN_POINT ( 'NONE',  ( 0.1532563361054082862, 61.21726448433412315, 2.638427012816831674 ) ) ;
#75817 = DIRECTION ( 'NONE',  ( 0.000000000000000000, 0.000000000000000000, 1.000000000000000000 ) ) ;
#75819 = CARTESIAN_POINT ( 'NONE',  ( 4.559911319644449179, 38.89701867748817676, 9.422509992056141925 ) ) ;
#75820 = CARTESIAN_POINT ( 'NONE',  ( 1.472469842513823179, 46.42559781766745175, 4.923371831947296329 ) ) ;
#75821 = DIRECTION ( 'NONE',  ( 0.5807029557109463225, 0.000000000000000000, -0.8141155183563145714 ) ) ;
#75822 = CARTESIAN_POINT ( 'NONE',  ( 7.361572987183170547, 22.05059781766745530, 9.846743663894590881 ) ) ;
#75823 = CARTESIAN_POINT ( 'NONE',  ( 17.20831665107776587, 2.883931151000785231, 7.208316651077764980 ) ) ;
#75825 = ORIENTED_EDGE ( 'NONE', *, *, #38119, .F. ) ;
#75824 = CARTESIAN_POINT ( 'NONE',  ( 6.565887622018943937, -1.918031996736246692, -12.81628187352647608 ) ) ;
#75826 = CARTESIAN_POINT ( 'NONE',  ( 7.084665262690076126, 2.022018677488170990, -10.88017736071110164 ) ) ;
#75827 =( LENGTH_UNIT ( ) NAMED_UNIT ( * ) SI_UNIT ( .MILLI., .METRE. ) );
#75828 = CARTESIAN_POINT ( 'NONE',  ( 17.20831665107776587, 57.88393115100078745, 7.208316651077764980 ) ) ;
#75829 = AXIS2_PLACEMENT_3D ( 'NONE', #27851, #96879, #89838 ) ;
#75830 = CARTESIAN_POINT ( 'NONE',  ( 4.919406150734204175, -13.80316667495554661, -2.499999999999999112 ) ) ;
#75831 = CARTESIAN_POINT ( 'NONE',  ( 19.42250999205614193, 5.147018677488171434, 5.440088680355555262 ) ) ;
#75832 = CARTESIAN_POINT ( 'NONE',  ( 18.52753015748618282, 43.92559781766745175, -4.923371831947291888 ) ) ;
#75833 = TOROIDAL_SURFACE ( 'NONE', #93462, 2.500000000000001776, 0.5000000000000000000 ) ;
#75834 = ORIENTED_EDGE ( 'NONE', *, *, #61902, .F. ) ;
#75835 = CARTESIAN_POINT ( 'NONE',  ( 17.96484262340118221, 6.188685344154837509, -7.964842623401177768 ) ) ;
#75836 = LINE ( 'NONE', #90327, #59939 ) ;
#75837 = CARTESIAN_POINT ( 'NONE',  ( 7.084665262690076126, 39.10535201082150536, 10.88017736071109987 ) ) ;
#75838 = CARTESIAN_POINT ( 'NONE',  ( 17.08211943468705130, 43.47041550158063927, 12.26659068614894998 ) ) ;
#75840 = CARTESIAN_POINT ( 'NONE',  ( 3.468686501387198362, 0.000000000000000000, -4.207853202970280648 ) ) ;
#75839 = CARTESIAN_POINT ( 'NONE',  ( 2.917880565312950480, 65.97041550158063217, -12.26659068614894821 ) ) ;
#75841 = CARTESIAN_POINT ( 'NONE',  ( 19.10478245763048832, 6.025762395770821733, -5.990408912944375608 ) ) ;
#75842 =( BOUNDED_CURVE ( )  B_SPLINE_CURVE ( 2, ( #71375, #3356, #25865, #94837, #17387, #41379, #84887, #62362, #47367 ),
 .UNSPECIFIED., .F., .T. ) 
 B_SPLINE_CURVE_WITH_KNOTS ( ( 3, 2, 2, 2, 3 ),
 ( 0.5462860886497512558, 0.5476190476190476719, 0.5535714285714286031, 0.5595238095238095344, 0.5608567684931060615 ),
 .UNSPECIFIED. ) 
 CURVE ( )  GEOMETRIC_REPRESENTATION_ITEM ( )  RATIONAL_B_SPLINE_CURVE ( ( 0.9881565478350734510, 0.9923695281211492025, 1.000000000000000000, 0.9659258262890683122, 1.000000000000000000, 0.9659258262890683122, 1.000000000000000000, 0.9923695281211484254, 0.9881565478350726739 ) ) 
 REPRESENTATION_ITEM ( '' )  );
#75843 = CARTESIAN_POINT ( 'NONE',  ( 0.1532563361054082862, 31.21726448433412315, 2.638427012816831674 ) ) ;
#75844 = CARTESIAN_POINT ( 'NONE',  ( 22.81628187352647785, 16.62363466993042138, 6.195893100308588602E-16 ) ) ;
#75845 = DIRECTION ( 'NONE',  ( -1.000000000000000000, 0.000000000000000000, 0.000000000000000000 ) ) ;
#75846 = ORIENTED_EDGE ( 'NONE', *, *, #36389, .T. ) ;
#75847 = DIRECTION ( 'NONE',  ( 0.000000000000000000, 1.000000000000000000, -0.000000000000000000 ) ) ;
#75848 = EDGE_CURVE ( 'NONE', #76346, #70990, #75358, .T. ) ;
#75849 = CARTESIAN_POINT ( 'NONE',  ( 14.97687855664608314, 0.5000000000000004441, -0.8325315005900512100 ) ) ;
#75850 = CARTESIAN_POINT ( 'NONE',  ( -9.206646936887572963, -19.70874149522336793, -3.750000000000000000 ) ) ;
#75851 = CARTESIAN_POINT ( 'NONE',  ( 20.36894250292379382, 8.678748834913967869, 10.36894250292379205 ) ) ;
#75852 = CARTESIAN_POINT ( 'NONE',  ( 0.1532563361054100626, 20.80059781766744464, -2.638427012816831230 ) ) ;
#75853 = CARTESIAN_POINT ( 'NONE',  ( 24.35999999999999233, 44.99999999999997868, 10.00000000000000000 ) ) ;
#75854 = ORIENTED_EDGE ( 'NONE', *, *, #93597, .T. ) ;
#75855 = VECTOR ( 'NONE', #63021, 1000.000000000000000 ) ;
#75856 = CARTESIAN_POINT ( 'NONE',  ( -4.164238869374099039, 51.80374883491396787, 8.674139862899312516E-16 ) ) ;
#75857 = CARTESIAN_POINT ( 'NONE',  ( 2.791683348922237240, 15.38393115100078212, -7.208316651077763204 ) ) ;
#75859 = CARTESIAN_POINT ( 'NONE',  ( 0.000000000000000000, 14.49999999999999822, 0.000000000000000000 ) ) ;
#75858 = CARTESIAN_POINT ( 'NONE',  ( 1.820328553599862786, 0.000000000000000000, 5.140449258537825195 ) ) ;
#75860 = CARTESIAN_POINT ( 'NONE',  ( 7.084665262690076126, 37.02201867748817676, -10.88017736071110164 ) ) ;
#75861 = CARTESIAN_POINT ( 'NONE',  ( 22.81628187352647785, 51.62363466993042493, 6.195893100308588602E-16 ) ) ;
#75862 = CARTESIAN_POINT ( 'NONE',  ( 17.96484262340118221, 9.938685344154837509, 7.964842623401181321 ) ) ;
#75863 = CARTESIAN_POINT ( 'NONE',  ( -2.816281873526473856, 29.33196800326376064, 3.434112377981055619 ) ) ;
#75864 = CARTESIAN_POINT ( 'NONE',  ( 0.9413316022086137824, 53.45508385108959004, 6.499999999999978684 ) ) ;
#75865 = VERTEX_POINT ( 'NONE', #59365 ) ;
#75866 = CARTESIAN_POINT ( 'NONE',  ( 2.153642693323437385, 11.13791097397318275, -6.499999999999995559 ) ) ;
#75867 = CARTESIAN_POINT ( 'NONE',  ( -3.750000000000000000, 37.00000000000000000, 2.750000000000000000 ) ) ;
#75868 = CARTESIAN_POINT ( 'NONE',  ( 24.16423886937410614, 39.51208216824731068, -3.795296366450302550 ) ) ;
#75869 = CARTESIAN_POINT ( 'NONE',  ( 20.36894250292379738, 19.92874883491396787, -10.36894250292379027 ) ) ;
#75870 = CARTESIAN_POINT ( 'NONE',  ( 7.084665262690076126, 2.022018677488170990, -10.88017736071110164 ) ) ;
#75871 = CARTESIAN_POINT ( 'NONE',  ( 0.5774900079438590739, 32.64701867748816966, -5.440088680355550821 ) ) ;
#75872 = CARTESIAN_POINT ( 'NONE',  ( -12.00809552683946357, 15.00000000000000000, -8.989195838243713155 ) ) ;
#75873 = FILL_AREA_STYLE_COLOUR ( '', #35213 ) ;
#75874 = CARTESIAN_POINT ( 'NONE',  ( 7.084665262690076126, 59.10535201082150536, 10.88017736071109987 ) ) ;
#75875 = CARTESIAN_POINT ( 'NONE',  ( 10.00000000000000178, 64.31368534415483396, 10.88017736071110342 ) ) ;
#75876 = CARTESIAN_POINT ( 'NONE',  ( 19.38216949554541557, 22.24863466993041428, -9.382169495545420901 ) ) ;
#75877 = DIRECTION ( 'NONE',  ( 0.000000000000000000, 0.000000000000000000, 1.000000000000000000 ) ) ;
#75878 = DIRECTION ( 'NONE',  ( 0.5075383629607025382, 0.000000000000000000, -0.8616291604415267091 ) ) ;
#75879 = CARTESIAN_POINT ( 'NONE',  ( 5.076628168052703671, 36.84226448433412315, 8.527530157486179263 ) ) ;
#75880 = CIRCLE ( 'NONE', #74285, 1.000000000000000888 ) ;
#75881 = B_SPLINE_CURVE_WITH_KNOTS ( 'NONE', 3,
 ( #9077, #92567, #85078, #16587, #30088, #85574 ),
 .UNSPECIFIED., .F., .F.,
 ( 4, 2, 4 ),
 ( 3.409110551496079869E-05, 0.0004400426677367856500, 0.0008459942299586105082 ),
 .UNSPECIFIED. ) ;
#75882 = ADVANCED_FACE ( 'NONE', ( #59860 ), #14383, .F. ) ;
#75883 = CARTESIAN_POINT ( 'NONE',  ( 21.09922568453595559, 22.04030133659708923, -6.408140936763230044 ) ) ;
#75884 = DIRECTION ( 'NONE',  ( -0.000000000000000000, 0.000000000000000000, 1.000000000000000000 ) ) ;
#75885 = CARTESIAN_POINT ( 'NONE',  ( -0.8801773607111009756, 13.06368534415483929, 1.068504757029289695E-15 ) ) ;
#75886 = CARTESIAN_POINT ( 'NONE',  ( 0.1532563361054082862, 41.21726448433411605, 2.638427012816831674 ) ) ;
#75887 = CARTESIAN_POINT ( 'NONE',  ( -1.099225684535947600, 59.54030133659708923, 6.408140936763237150 ) ) ;
#75888 = CARTESIAN_POINT ( 'NONE',  ( 0.1532563361054082862, 16.21726448433411960, 2.638427012816831674 ) ) ;
#75889 = ADVANCED_FACE ( 'NONE', ( #6872 ), #13106, .T. ) ;
#75890 = CARTESIAN_POINT ( 'NONE',  ( 5.815502996284953596, 14.76930270348881002, -13.76292046016122228 ) ) ;
#75891 = CARTESIAN_POINT ( 'NONE',  ( 0.5774900079438590739, 37.64701867748817676, -5.440088680355550821 ) ) ;
#75892 = CARTESIAN_POINT ( 'NONE',  ( 15.44008868035555260, 4.730352010821504471, 9.422509992056143702 ) ) ;
#75893 = CARTESIAN_POINT ( 'NONE',  ( 12.91533473730992121, 29.52201867748817321, 10.88017736071110164 ) ) ;
#75894 = CARTESIAN_POINT ( 'NONE',  ( 0.5774900079438607392, 13.48035201082150358, 5.440088680355550821 ) ) ;
#75895 = EDGE_LOOP ( 'NONE', ( #34705, #86553, #86242, #58924 ) ) ;
#75896 = CARTESIAN_POINT ( 'NONE',  ( 4.559911319644449179, 32.23035201082150536, -9.422509992056141925 ) ) ;
#75897 = CARTESIAN_POINT ( 'NONE',  ( 22.81628187352648496, 41.83196800326375353, -3.434112377981050290 ) ) ;
#75898 = CARTESIAN_POINT ( 'NONE',  ( 12.91533473730992121, 44.52201867748816966, 10.88017736071110164 ) ) ;
#75900 = CARTESIAN_POINT ( 'NONE',  ( 2.035157376598822676, 57.43868534415484106, -7.964842623401177768 ) ) ;
#75899 = CARTESIAN_POINT ( 'NONE',  ( 2.603489959281613420, 45.43575266056827644, -6.500000000000031086 ) ) ;
#75901 = ORIENTED_EDGE ( 'NONE', *, *, #85467, .T. ) ;
#75902 = CARTESIAN_POINT ( 'NONE',  ( 7.084665262690076126, 37.02201867748817676, -10.88017736071110164 ) ) ;
#75903 = CARTESIAN_POINT ( 'NONE',  ( 5.680373671027947324, -28.65980262291034819, 3.749999999996780353 ) ) ;
#75904 = DIRECTION ( 'NONE',  ( -0.08715574274765112983, -0.9961946980917461003, 0.000000000000000000 ) ) ;
#75906 = CARTESIAN_POINT ( 'NONE',  ( 24.16423886937409904, 49.09541550158063217, 3.795296366450317205 ) ) ;
#75905 = PRODUCT_DEFINITION_FORMATION_WITH_SPECIFIED_SOURCE ( 'ANY', '', #98572, .NOT_KNOWN. ) ;
#75907 = CARTESIAN_POINT ( 'NONE',  ( 19.42250999205614193, 65.14701867748817676, 5.440088680355555262 ) ) ;
#75908 = DIRECTION ( 'NONE',  ( 0.000000000000000000, 0.000000000000000000, 1.000000000000000000 ) ) ;
#75909 = AXIS2_PLACEMENT_3D ( 'NONE', #35228, #27731, #19744 ) ;
#75910 = CARTESIAN_POINT ( 'NONE',  ( 18.52753015748617571, 58.09226448433411605, 4.923371831947298993 ) ) ;
#75911 = CARTESIAN_POINT ( 'NONE',  ( -14.49440716394874151, 15.00000000000000000, 0.4026921475165272657 ) ) ;
#75912 = CARTESIAN_POINT ( 'NONE',  ( 17.20831665107776587, 39.13393115100079456, -7.208316651077762316 ) ) ;
#75913 = ORIENTED_EDGE ( 'NONE', *, *, #98121, .F. ) ;
#75914 = CARTESIAN_POINT ( 'NONE',  ( 19.84674366389459266, 38.30059781766745175, 2.638427012816836559 ) ) ;
#75915 = CARTESIAN_POINT ( 'NONE',  ( -3.434112377981067610, -21.91803199673624647, -12.81628187352647252 ) ) ;
#75916 = CARTESIAN_POINT ( 'NONE',  ( 10.00000000000000178, 29.31368534415483751, 10.88017736071110342 ) ) ;
#75917 = CARTESIAN_POINT ( 'NONE',  ( 7.361572987183170547, 42.05059781766745886, 9.846743663894590881 ) ) ;
#75918 = CARTESIAN_POINT ( 'NONE',  ( 6.565887622018943937, 25.16530133659708213, 12.81628187352647430 ) ) ;
#75919 = CARTESIAN_POINT ( 'NONE',  ( 0.5774900079438607392, 58.48035201082151247, 5.440088680355550821 ) ) ;
#75921 = CARTESIAN_POINT ( 'NONE',  ( -2.816281873526473856, 64.33196800326376774, 3.434112377981055619 ) ) ;
#75920 = CARTESIAN_POINT ( 'NONE',  ( 12.91533473730992121, 39.52201867748817676, 10.88017736071110164 ) ) ;
#75922 = CARTESIAN_POINT ( 'NONE',  ( 24.16423886937410614, 64.51208216824728936, -3.795296366450302550 ) ) ;
#75923 = EDGE_CURVE ( 'NONE', #61157, #58317, #72403, .T. ) ;
#75924 = AXIS2_PLACEMENT_3D ( 'NONE', #39726, #31706, #9709 ) ;
#75925 = FACE_OUTER_BOUND ( 'NONE', #36064, .T. ) ;
#75926 = VERTEX_POINT ( 'NONE', #391 ) ;
#75927 = CARTESIAN_POINT ( 'NONE',  ( 16.40814093676323893, 15.79030133659708746, 11.09922568453595026 ) ) ;
#75928 = CARTESIAN_POINT ( 'NONE',  ( 17.96484262340118221, 9.938685344154837509, 7.964842623401181321 ) ) ;
#75929 = CARTESIAN_POINT ( 'NONE',  ( 19.42250999205614193, 45.14701867748817676, 5.440088680355555262 ) ) ;
#75930 = DIRECTION ( 'NONE',  ( 0.000000000000000000, 0.000000000000000000, 1.000000000000000000 ) ) ;
#75931 = B_SPLINE_CURVE_WITH_KNOTS ( 'NONE', 3,
 ( #70680, #62167, #9185, #69688, #23721, #18167, #70187, #730, #31184, #39201, #17196, #1704, #40673, #92196, #1222, #33150, #62662, #9678 ),
 .UNSPECIFIED., .F., .F.,
 ( 4, 2, 2, 2, 2, 2, 2, 2, 4 ),
 ( 0.000000000000000000, 0.01113508862748988255, 0.02227017725497976511, 0.04454035450995957185, 0.06681053176493938206, 0.07794562039242927676, 0.08351316470617423104, 0.08629693686304670819, 0.08908070901991918533 ),
 .UNSPECIFIED. ) ;
#75932 = ORIENTED_EDGE ( 'NONE', *, *, #77125, .T. ) ;
#75933 = CARTESIAN_POINT ( 'NONE',  ( 7.084665262690076126, 62.02201867748816966, -10.88017736071110164 ) ) ;
#75934 = CARTESIAN_POINT ( 'NONE',  ( 7.361572987183170547, 37.05059781766744464, 9.846743663894590881 ) ) ;
#75935 = CARTESIAN_POINT ( 'NONE',  ( 14.92337183194729633, 22.67559781766745175, 8.527530157486181039 ) ) ;
#75936 = CARTESIAN_POINT ( 'NONE',  ( 18.52753015748617571, 18.09226448433411960, 4.923371831947298993 ) ) ;
#75937 = SPHERICAL_SURFACE ( 'NONE', #65192, 5.999999999999998224 ) ;
#75938 = STYLED_ITEM ( 'NONE', ( #42641 ), #54290 ) ;
#75939 = DIRECTION ( 'NONE',  ( 0.000000000000000000, 0.000000000000000000, 1.000000000000000000 ) ) ;
#75941 = CARTESIAN_POINT ( 'NONE',  ( 12.22506292814015261, 0.2306972965111908358, 8.589871424854795379 ) ) ;
#75940 = CARTESIAN_POINT ( 'NONE',  ( 18.52753015748618282, 13.92559781766745175, -4.923371831947291888 ) ) ;
#75942 = DIRECTION ( 'NONE',  ( 0.000000000000000000, 1.000000000000000000, 0.000000000000000000 ) ) ;
#75944 = ORIENTED_EDGE ( 'NONE', *, *, #78748, .F. ) ;
#75943 = CARTESIAN_POINT ( 'NONE',  ( 1.472469842513823179, 26.42559781766745175, 4.923371831947296329 ) ) ;
#75945 = CARTESIAN_POINT ( 'NONE',  ( 22.81628187352647785, 61.62363466993041783, 6.195893100308588602E-16 ) ) ;
#75946 = CARTESIAN_POINT ( 'NONE',  ( 2.827051895225787703, 0.2301501044984899935, -14.67071941139712443 ) ) ;
#75947 = CARTESIAN_POINT ( 'NONE',  ( 22.81628187352647785, 6.623634669930420493, 6.195893100308588602E-16 ) ) ;
#75948 = AXIS2_PLACEMENT_3D ( 'NONE', #17226, #77703, #63186 ) ;
#75949 = CARTESIAN_POINT ( 'NONE',  ( -0.8801773607110991993, 57.85535201082149825, -2.915334737309923874 ) ) ;
#75950 = CARTESIAN_POINT ( 'NONE',  ( 10.00000000000000000, 30.55374883491397142, -14.16423886937410082 ) ) ;
#75951 = CARTESIAN_POINT ( 'NONE',  ( -12.23643000159001382, 90.44368800334291336, 7.046674173435446775 ) ) ;
#75952 = CARTESIAN_POINT ( 'NONE',  ( -4.164238869374098151, 26.59541550158063217, -3.795296366450310543 ) ) ;
#75953 = CARTESIAN_POINT ( 'NONE',  ( 22.26659068614894466, 53.88708216824731068, 7.082119434687054849 ) ) ;
#75954 = CARTESIAN_POINT ( 'NONE',  ( -4.164238869374098151, 6.595415501580634832, -3.795296366450310543 ) ) ;
#75955 = CARTESIAN_POINT ( 'NONE',  ( 6.204703633549690345, 32.84541550158063927, 14.16423886937410082 ) ) ;
#75956 = CARTESIAN_POINT ( 'NONE',  ( 7.084665262690076126, 42.02201867748816966, -10.88017736071110164 ) ) ;
#75957 = CARTESIAN_POINT ( 'NONE',  ( 3.469446951953614189E-15, 4.171802177851546389, 11.25000000000000355 ) ) ;
#75959 = CARTESIAN_POINT ( 'NONE',  ( 17.20831665107776587, 44.13393115100078745, -7.208316651077762316 ) ) ;
#75958 = DIRECTION ( 'NONE',  ( -0.000000000000000000, -0.000000000000000000, -1.000000000000000000 ) ) ;
#75960 = CARTESIAN_POINT ( 'NONE',  ( -0.8801773607111009756, 18.06368534415484106, 1.068504757029289695E-15 ) ) ;
#75961 = CARTESIAN_POINT ( 'NONE',  ( 0.6178305044545818747, 63.49863466993043204, -9.382169495545419124 ) ) ;
#75962 = CARTESIAN_POINT ( 'NONE',  ( 0.1532563361054083140, 66.00893115100079456, 1.131784320476157264E-15 ) ) ;
#75963 = CARTESIAN_POINT ( 'NONE',  ( 5.448048636097843733, 0.000000000000000000, 0.2378669404634861928 ) ) ;
#75964 = EDGE_CURVE ( 'NONE', #5021, #39466, #5206, .T. ) ;
#75965 = CARTESIAN_POINT ( 'NONE',  ( 0.1532563361054082862, 31.21726448433412315, 2.638427012816831674 ) ) ;
#75966 = CARTESIAN_POINT ( 'NONE',  ( 3.591859063236763294, 58.29030133659708923, -11.09922568453595026 ) ) ;
#75968 =( GEOMETRIC_REPRESENTATION_CONTEXT ( 3 ) GLOBAL_UNCERTAINTY_ASSIGNED_CONTEXT ( ( #11434 ) ) GLOBAL_UNIT_ASSIGNED_CONTEXT ( ( #57163, #80164, #20654 ) ) REPRESENTATION_CONTEXT ( 'NONE', 'WORKASPACE' ) );
#75967 = CARTESIAN_POINT ( 'NONE',  ( 3.469446951953614189E-15, -16.94625116508602858, 14.16423886937410259 ) ) ;
#75969 = CARTESIAN_POINT ( 'NONE',  ( 12.91533473730993009, 46.60535201082150536, -10.88017736071109987 ) ) ;
#75970 = CARTESIAN_POINT ( 'NONE',  ( 7.361572987183170547, 47.05059781766745175, 9.846743663894590881 ) ) ;
#75971 = AXIS2_PLACEMENT_3D ( 'NONE', #26340, #9882, #19340 ) ;
#75972 = CARTESIAN_POINT ( 'NONE',  ( 17.08211943468705840, 35.13708216824730357, -12.26659068614894466 ) ) ;
#75973 = ORIENTED_EDGE ( 'NONE', *, *, #25547, .F. ) ;
#75974 = CARTESIAN_POINT ( 'NONE',  ( -13.40508947812170781, 4.272460637706398645E-16, 5.527528931046010285 ) ) ;
#75975 = CIRCLE ( 'NONE', #85546, 0.2500000000000002220 ) ;
#75976 = CARTESIAN_POINT ( 'NONE',  ( -0.8801773607111009756, 63.06368534415484106, 1.068504757029289695E-15 ) ) ;
#75977 = CARTESIAN_POINT ( 'NONE',  ( 2.917880565312950480, 55.97041550158063217, -12.26659068614894821 ) ) ;
#75978 = CARTESIAN_POINT ( 'NONE',  ( 3.591859063236761518, 14.95696800326375531, 11.09922568453594849 ) ) ;
#75979 = FACE_OUTER_BOUND ( 'NONE', #70493, .T. ) ;
#75980 = CARTESIAN_POINT ( 'NONE',  ( 12.91533473730993009, 56.60535201082151247, -10.88017736071109987 ) ) ;
#75981 = CARTESIAN_POINT ( 'NONE',  ( 0.000000000000000000, 15.00000000000000000, 0.000000000000000000 ) ) ;
#75982 = CARTESIAN_POINT ( 'NONE',  ( -46.67091953292581508, 101.1773697441846736, -8.660634561519810148 ) ) ;
#75983 = CARTESIAN_POINT ( 'NONE',  ( 10.00000000000000178, 53.05374883491396787, 14.16423886937410082 ) ) ;
#75984 = CARTESIAN_POINT ( 'NONE',  ( -7.964842623401172439, 28.68868534415483751, 7.964842623401183097 ) ) ;
#75985 = CARTESIAN_POINT ( 'NONE',  ( 20.88017736071110164, 15.35535201082150358, 2.915334737309930979 ) ) ;
#75986 = CARTESIAN_POINT ( 'NONE',  ( 17.96484262340118221, 21.18868534415483396, -7.964842623401177768 ) ) ;
#75987 = CARTESIAN_POINT ( 'NONE',  ( 7.361572987183170547, 62.05059781766745886, 9.846743663894590881 ) ) ;
#75988 = CARTESIAN_POINT ( 'NONE',  ( 10.00000000000000000, 47.87363466993042493, -12.81628187352647608 ) ) ;
#75989 = CARTESIAN_POINT ( 'NONE',  ( 0.2751277870542870319, 54.36607318730131055, -6.499999999999985789 ) ) ;
#75990 = ORIENTED_EDGE ( 'NONE', *, *, #62351, .T. ) ;
#75991 = CARTESIAN_POINT ( 'NONE',  ( 19.42250999205614193, 20.14701867748817321, 5.440088680355555262 ) ) ;
#75992 = CARTESIAN_POINT ( 'NONE',  ( 0.6178305044545818747, 18.49863466993041428, -9.382169495545419124 ) ) ;
#75993 = PLANE ( 'NONE',  #86409 ) ;
#75994 = TOROIDAL_SURFACE ( 'NONE', #47221, 2.500000000000001776, 0.5000000000000000000 ) ;
#75995 = EDGE_CURVE ( 'NONE', #39993, #24774, #46345, .T. ) ;
#75996 = CARTESIAN_POINT ( 'NONE',  ( 19.84674366389459621, 43.50893115100078745, 7.409399052514197653E-17 ) ) ;
#75997 = CARTESIAN_POINT ( 'NONE',  ( 17.96484262340118221, 39.93868534415484106, 7.964842623401181321 ) ) ;
#75998 = CARTESIAN_POINT ( 'NONE',  ( 3.591859063236763294, 28.29030133659708568, -11.09922568453595026 ) ) ;
#76000 = DIRECTION ( 'NONE',  ( -1.000000000000000000, 0.000000000000000000, 0.000000000000000000 ) ) ;
#75999 = CARTESIAN_POINT ( 'NONE',  ( 0.5774900079438607392, 43.48035201082151247, 5.440088680355550821 ) ) ;
#76001 = DIRECTION ( 'NONE',  ( 0.000000000000000000, 0.000000000000000000, 1.000000000000000000 ) ) ;
#76002 = CARTESIAN_POINT ( 'NONE',  ( -1.099225684535947600, 49.54030133659708923, 6.408140936763237150 ) ) ;
#76003 = ORIENTED_EDGE ( 'NONE', *, *, #87724, .T. ) ;
#76004 = EDGE_CURVE ( 'NONE', #41516, #14084, #8833, .T. ) ;
#76005 = CARTESIAN_POINT ( 'NONE',  ( 20.88017736071110164, 55.35535201082149825, 2.915334737309930979 ) ) ;
#76007 = CARTESIAN_POINT ( 'NONE',  ( -0.3689425029237881626, 7.428748834913967869, 10.36894250292379027 ) ) ;
#76006 = CARTESIAN_POINT ( 'NONE',  ( -2.816281873526473856, 34.33196800326376064, 3.434112377981055619 ) ) ;
#76008 = CARTESIAN_POINT ( 'NONE',  ( 7.084665262690076126, 54.10535201082151247, 10.88017736071109987 ) ) ;
#76009 = CARTESIAN_POINT ( 'NONE',  ( -4.164238869374098151, 46.59541550158063927, -3.795296366450310543 ) ) ;
#76010 = CARTESIAN_POINT ( 'NONE',  ( 0.1532563361054082862, 66.21726448433413736, 2.638427012816831674 ) ) ;
#76011 = CARTESIAN_POINT ( 'NONE',  ( 7.361572987183170547, 17.05059781766745530, 9.846743663894590881 ) ) ;
#76012 = CARTESIAN_POINT ( 'NONE',  ( 17.20831665107776587, 4.133931151000785675, -7.208316651077762316 ) ) ;
#76013 = DIRECTION ( 'NONE',  ( 0.000000000000000000, 1.000000000000000000, 0.000000000000000000 ) ) ;
#76014 = CARTESIAN_POINT ( 'NONE',  ( -2.266590686148945544, 47.22041550158063927, 7.082119434687048631 ) ) ;
#76015 = AXIS2_PLACEMENT_3D ( 'NONE', #91221, #6748, #16225 ) ;
#76016 = CARTESIAN_POINT ( 'NONE',  ( 11.96291822454881348, 3.986488846351010315E-16, -8.193813980849080636 ) ) ;
#76017 = CARTESIAN_POINT ( 'NONE',  ( -0.8801773607111008646, 8.272018677488171434, 2.915334737309923430 ) ) ;
#76018 = CARTESIAN_POINT ( 'NONE',  ( -6.982525766850296911, -88.11956318484570261, -3.750000000000000000 ) ) ;
#76019 = VERTEX_POINT ( 'NONE', #61339 ) ;
#76020 = CARTESIAN_POINT ( 'NONE',  ( 12.91533473730993009, 6.605352010821504471, -10.88017736071109987 ) ) ;
#76021 = CARTESIAN_POINT ( 'NONE',  ( -4.164238869374098151, 66.59541550158060375, -3.795296366450310543 ) ) ;
#76022 = CARTESIAN_POINT ( 'NONE',  ( 19.84674366389459266, 38.71726448433412315, -2.638427012816827677 ) ) ;
#76023 = CARTESIAN_POINT ( 'NONE',  ( 3.591859063236761518, 39.95696800326375353, 11.09922568453594849 ) ) ;
#76024 = CARTESIAN_POINT ( 'NONE',  ( -4.391700990646977054, 14.76930270348881002, -14.28114200970196102 ) ) ;
#76026 = CARTESIAN_POINT ( 'NONE',  ( 13.79529636645030344, 8.262082168247300018, 14.16423886937410614 ) ) ;
#76025 = CARTESIAN_POINT ( 'NONE',  ( 2.393480905993150998, 0.5000000000000004441, -14.80781041047751323 ) ) ;
#76027 = CARTESIAN_POINT ( 'NONE',  ( 15.44008868035555793, 6.397018677488170546, -9.422509992056140149 ) ) ;
#76028 = CARTESIAN_POINT ( 'NONE',  ( 20.88017736071110875, 5.772018677488170546, -2.915334737309920765 ) ) ;
#76029 = CARTESIAN_POINT ( 'NONE',  ( 7.361572987183170547, 47.05059781766745175, 9.846743663894590881 ) ) ;
#76030 = DIRECTION ( 'NONE',  ( -0.09584575252021386438, 0.000000000000000000, -0.9953961983671798519 ) ) ;
#76031 = CARTESIAN_POINT ( 'NONE',  ( 0.1532563361054100626, 25.80059781766744820, -2.638427012816831230 ) ) ;
#76032 = CARTESIAN_POINT ( 'NONE',  ( 0.5774900079438607392, 33.48035201082150536, 5.440088680355550821 ) ) ;
#76033 = CARTESIAN_POINT ( 'NONE',  ( -4.923371831947292776, 11.84226448433412671, 8.527530157486181039 ) ) ;
#76034 = EDGE_LOOP ( 'NONE', ( #73731, #96332, #86136, #65971, #70141, #83713 ) ) ;
#76035 = EDGE_LOOP ( 'NONE', ( #29535, #79832, #72499, #58086, #20922, #91770 ) ) ;
#76036 = PLANE ( 'NONE',  #90890 ) ;
#76037 = ORIENTED_EDGE ( 'NONE', *, *, #70557, .T. ) ;
#76038 = CARTESIAN_POINT ( 'NONE',  ( 7.361572987183169658, 54.96726448433413026, -9.846743663894592657 ) ) ;
#76040 = CARTESIAN_POINT ( 'NONE',  ( 17.96484262340118221, 34.93868534415482685, 7.964842623401181321 ) ) ;
#76039 = CARTESIAN_POINT ( 'NONE',  ( -0.8801773607111008646, 28.27201867748817321, 2.915334737309923430 ) ) ;
#76042 = CARTESIAN_POINT ( 'NONE',  ( 16.40814093676324603, 37.45696800326376064, -11.09922568453594671 ) ) ;
#76041 = CARTESIAN_POINT ( 'NONE',  ( 0.1532563361054100626, 65.80059781766745175, -2.638427012816831230 ) ) ;
#76043 = CARTESIAN_POINT ( 'NONE',  ( 22.26659068614894466, 3.887082168247300906, 7.082119434687054849 ) ) ;
#76044 = ADVANCED_FACE ( 'NONE', ( #76832 ), #48288, .T. ) ;
#76045 = AXIS2_PLACEMENT_3D ( 'NONE', #13423, #66918, #43908 ) ;
#76046 = AXIS2_PLACEMENT_3D ( 'NONE', #89844, #37360, #67853 ) ;
#76048 = CARTESIAN_POINT ( 'NONE',  ( 16.40814093676323893, 40.79030133659708923, 11.09922568453595026 ) ) ;
#76047 = CIRCLE ( 'NONE', #42502, 15.00000000000000000 ) ;
#76049 = ORIENTED_EDGE ( 'NONE', *, *, #76248, .T. ) ;
#76050 = CARTESIAN_POINT ( 'NONE',  ( 19.84674366389459266, 48.71726448433413026, -2.638427012816827677 ) ) ;
#76051 = CARTESIAN_POINT ( 'NONE',  ( -0.8801773607111009756, 8.063685344154837509, 1.068504757029289695E-15 ) ) ;
#76052 = ORIENTED_EDGE ( 'NONE', *, *, #27469, .F. ) ;
#76053 = CARTESIAN_POINT ( 'NONE',  ( 2.035157376598824452, 18.68868534415484106, 7.964842623401179544 ) ) ;
#76054 = EDGE_CURVE ( 'NONE', #70343, #67870, #30340, .T. ) ;
#76055 = ORIENTED_EDGE ( 'NONE', *, *, #97449, .T. ) ;
#76056 = CARTESIAN_POINT ( 'NONE',  ( 20.88017736071110519, 55.56368534415484817, 2.639326808657452039E-16 ) ) ;
#76057 = CARTESIAN_POINT ( 'NONE',  ( 7.084665262690076126, 57.02201867748817676, -10.88017736071110164 ) ) ;
#76058 = CARTESIAN_POINT ( 'NONE',  ( 17.96484262340118221, 54.93868534415484106, 7.964842623401181321 ) ) ;
#76059 = CARTESIAN_POINT ( 'NONE',  ( -0.1503990784575242878, 29.24884699246888786, -6.262539305110083276 ) ) ;
#76060 =( GEOMETRIC_REPRESENTATION_CONTEXT ( 3 ) GLOBAL_UNCERTAINTY_ASSIGNED_CONTEXT ( ( #96312 ) ) GLOBAL_UNIT_ASSIGNED_CONTEXT ( ( #47990, #78005, #46520 ) ) REPRESENTATION_CONTEXT ( 'NONE', 'WORKASPACE' ) );
#76062 = ORIENTED_EDGE ( 'NONE', *, *, #39371, .F. ) ;
#76061 = CARTESIAN_POINT ( 'NONE',  ( 8.959592931132405624, -9.312622102011351544, 4.000000000000000888 ) ) ;
#76063 = CARTESIAN_POINT ( 'NONE',  ( 0.1532563361054100626, 40.80059781766745886, -2.638427012816831230 ) ) ;
#76064 = ORIENTED_EDGE ( 'NONE', *, *, #87825, .T. ) ;
#76065 = CARTESIAN_POINT ( 'NONE',  ( 0.000000000000000000, 0.5000000000000004441, 0.000000000000000000 ) ) ;
#76066 = PRESENTATION_STYLE_ASSIGNMENT (( #91063 ) ) ;
#76067 = CARTESIAN_POINT ( 'NONE',  ( 17.08211943468705840, 10.13708216824730179, -12.26659068614894466 ) ) ;
#76068 = CARTESIAN_POINT ( 'NONE',  ( -1.926860441876563801, 7.662123368507804066, 1.004413902775740978E-15 ) ) ;
#76069 = CARTESIAN_POINT ( 'NONE',  ( 0.000000000000000000, 0.000000000000000000, 0.000000000000000000 ) ) ;
#76070 = CARTESIAN_POINT ( 'NONE',  ( 10.00000000000000000, 1.813685344154838175, -10.88017736071110342 ) ) ;
#76071 = CARTESIAN_POINT ( 'NONE',  ( 14.99999999999997868, 80.07179676972448590, 6.250000000000000000 ) ) ;
#76073 = ORIENTED_EDGE ( 'NONE', *, *, #61400, .T. ) ;
#76072 = CARTESIAN_POINT ( 'NONE',  ( 13.43411237798106583, 47.66530133659709634, -12.81628187352647252 ) ) ;
#76074 = DIRECTION ( 'NONE',  ( -0.000000000000000000, -1.000000000000000000, -0.000000000000000000 ) ) ;
#76075 = CARTESIAN_POINT ( 'NONE',  ( 10.00000000000000178, 42.25893115100078745, 9.846743663894594434 ) ) ;
#76076 = FILL_AREA_STYLE ('',( #60582 ) ) ;
#76077 = VECTOR ( 'NONE', #13651, 1000.000000000000000 ) ;
#76078 = CARTESIAN_POINT ( 'NONE',  ( 21.09922568453595559, 17.04030133659708923, -6.408140936763230044 ) ) ;
#76079 = CARTESIAN_POINT ( 'NONE',  ( 12.63842701281683034, 22.46726448433411605, 9.846743663894596210 ) ) ;
#76080 = CARTESIAN_POINT ( 'NONE',  ( 0.000000000000000000, 0.5000000000000004441, 0.000000000000000000 ) ) ;
#76081 = EDGE_CURVE ( 'NONE', #74857, #48470, #39829, .T. ) ;
#76082 = CARTESIAN_POINT ( 'NONE',  ( 7.361572987183170547, 17.05059781766745530, 9.846743663894590881 ) ) ;
#76083 = CARTESIAN_POINT ( 'NONE',  ( 0.6178305044545838731, 19.74863466993042138, 9.382169495545420901 ) ) ;
#76084 = FACE_OUTER_BOUND ( 'NONE', #63459, .T. ) ;
#76085 = CARTESIAN_POINT ( 'NONE',  ( 18.52753015748617571, 8.092264484334117824, 4.923371831947298993 ) ) ;
#76086 = ORIENTED_EDGE ( 'NONE', *, *, #61197, .F. ) ;
#76087 = ADVANCED_FACE ( 'NONE', ( #16345 ), #54813, .F. ) ;
#76088 = VERTEX_POINT ( 'NONE', #70335 ) ;
#76089 = CARTESIAN_POINT ( 'NONE',  ( 12.91533473730993009, 21.60535201082150536, -10.88017736071109987 ) ) ;
#76090 = CARTESIAN_POINT ( 'NONE',  ( 22.26659068614895176, 19.72041550158063572, -7.082119434687042414 ) ) ;
#76091 = CARTESIAN_POINT ( 'NONE',  ( 1.472469842513823179, 45.59226448433412315, -4.923371831947296329 ) ) ;
#76092 = CARTESIAN_POINT ( 'NONE',  ( 5.076628168052703671, 1.842264484334118047, 8.527530157486179263 ) ) ;
#76094 = CARTESIAN_POINT ( 'NONE',  ( -7.045329894599615450, -66.66420243593404393, -3.750000000000000000 ) ) ;
#76093 = CARTESIAN_POINT ( 'NONE',  ( 10.00000000000000178, 35.37363466993042493, 12.81628187352647608 ) ) ;
#76095 = CARTESIAN_POINT ( 'NONE',  ( 12.91533473730993009, 11.60535201082150536, -10.88017736071109987 ) ) ;
#76096 = CARTESIAN_POINT ( 'NONE',  ( -14.02068044289371684, 15.00000000000000000, -5.331089937175857330 ) ) ;
#76097 = CARTESIAN_POINT ( 'NONE',  ( -2.816281873526471635, 13.91530133659708746, -3.434112377981056508 ) ) ;
#76098 = CARTESIAN_POINT ( 'NONE',  ( 10.00000000000000000, 12.87363466993042138, -12.81628187352647608 ) ) ;
#76099 = CARTESIAN_POINT ( 'NONE',  ( 5.076628168052704559, 25.17559781766745175, -8.527530157486179263 ) ) ;
#76100 = CARTESIAN_POINT ( 'NONE',  ( -7.964842623401179544, -17.56131465584515539, -7.964842623401174215 ) ) ;
#76101 = CARTESIAN_POINT ( 'NONE',  ( 0.6178305044545838731, 34.74863466993042493, 9.382169495545420901 ) ) ;
#76102 = SURFACE_SIDE_STYLE ('',( #46108 ) ) ;
#76103 = ADVANCED_FACE ( 'NONE', ( #62313 ), #15860, .F. ) ;
#76105 = CARTESIAN_POINT ( 'NONE',  ( 13.14228782657340844, 0.3640475087720989600, -7.230509711182238064 ) ) ;
#76104 = CARTESIAN_POINT ( 'NONE',  ( 12.91533473730992121, 44.52201867748816966, 10.88017736071110164 ) ) ;
#76106 = AXIS2_PLACEMENT_3D ( 'NONE', #18299, #17808, #8822 ) ;
#76107 = DIRECTION ( 'NONE',  ( -5.818595309480553908E-17, -1.000000000000000000, 0.000000000000000000 ) ) ;
#76108 = CARTESIAN_POINT ( 'NONE',  ( 2.035157376598822676, 67.43868534415484817, -7.964842623401177768 ) ) ;
#76109 = CARTESIAN_POINT ( 'NONE',  ( 20.88017736071110519, 40.56368534415484106, 2.639326808657452039E-16 ) ) ;
#76110 = CARTESIAN_POINT ( 'NONE',  ( 19.42250999205614548, 45.98035201082150536, -5.440088680355545492 ) ) ;
#76111 = CARTESIAN_POINT ( 'NONE',  ( 2.791683348922240793, 66.63393115100079456, 7.208316651077764092 ) ) ;
#76112 = CARTESIAN_POINT ( 'NONE',  ( -9.000000000000001776, 80.99999999999994316, 1.249999999999987121 ) ) ;
#76113 = TOROIDAL_SURFACE ( 'NONE', #56904, 20.49999999999999645, 0.5000000000000000000 ) ;
#76114 = UNCERTAINTY_MEASURE_WITH_UNIT (LENGTH_MEASURE( 1.000000000000000082E-05 ), #94242, 'distance_accuracy_value', 'NONE');
#76115 = CARTESIAN_POINT ( 'NONE',  ( 18.52753015748617571, 48.09226448433412315, 4.923371831947298993 ) ) ;
#76117 = CARTESIAN_POINT ( 'NONE',  ( 0.5600000000000083800, 105.0000000000000000, -5.000000000000000000 ) ) ;
#76116 = CARTESIAN_POINT ( 'NONE',  ( 0.5774900079438590739, 12.64701867748817143, -5.440088680355550821 ) ) ;
#76118 = CARTESIAN_POINT ( 'NONE',  ( 21.09922568453595559, 17.04030133659708923, -6.408140936763230044 ) ) ;
#76119 = ORIENTED_EDGE ( 'NONE', *, *, #6118, .F. ) ;
#76120 = CARTESIAN_POINT ( 'NONE',  ( 4.559911319644449179, 32.23035201082150536, -9.422509992056141925 ) ) ;
#76121 = EDGE_CURVE ( 'NONE', #15328, #24761, #23858, .T. ) ;
#76122 = B_SPLINE_CURVE_WITH_KNOTS ( 'NONE', 3,
 ( #94236, #3253, #24782, #87228, #48248, #10266 ),
 .UNSPECIFIED., .F., .F.,
 ( 4, 2, 4 ),
 ( 0.0002800313526655926139, 0.0006862368888107507007, 0.001092442424955908896 ),
 .UNSPECIFIED. ) ;
#76124 = DIRECTION ( 'NONE',  ( -0.07845909572784540154, 0.000000000000000000, 0.9969173337331279638 ) ) ;
#76123 = CARTESIAN_POINT ( 'NONE',  ( -1.099225684535947600, -0.4596986634029132657, 6.408140936763237150 ) ) ;
#76125 = CARTESIAN_POINT ( 'NONE',  ( 15.44008868035555260, 19.73035201082150536, 9.422509992056143702 ) ) ;
#76126 = CARTESIAN_POINT ( 'NONE',  ( 20.88017736071110875, 30.77201867748816966, -2.915334737309920765 ) ) ;
#76127 = CARTESIAN_POINT ( 'NONE',  ( -0.3689425029237881626, 37.42874883491396787, 10.36894250292379027 ) ) ;
#76128 = CARTESIAN_POINT ( 'NONE',  ( 17.20831665107776587, 32.88393115100078745, 7.208316651077764980 ) ) ;
#76129 = CARTESIAN_POINT ( 'NONE',  ( 2.035157376598824452, 48.68868534415483396, 7.964842623401179544 ) ) ;
#76130 = CARTESIAN_POINT ( 'NONE',  ( 20.36894250292379738, 9.928748834913966093, -10.36894250292379027 ) ) ;
#76131 = VECTOR ( 'NONE', #23960, 1000.000000000000000 ) ;
#76132 = CARTESIAN_POINT ( 'NONE',  ( 18.52753015748618282, 53.92559781766745175, -4.923371831947291888 ) ) ;
#76133 = AXIS2_PLACEMENT_3D ( 'NONE', #80063, #80564, #33564 ) ;
#76134 = ORIENTED_EDGE ( 'NONE', *, *, #75473, .T. ) ;
#76135 = EDGE_LOOP ( 'NONE', ( #68093, #53798, #39888 ) ) ;
#76136 = CARTESIAN_POINT ( 'NONE',  ( 10.00000000000000178, 38.05374883491396787, 14.16423886937410082 ) ) ;
#76138 = AXIS2_PLACEMENT_3D ( 'NONE', #81004, #50994, #43488 ) ;
#76137 = CARTESIAN_POINT ( 'NONE',  ( 13.79529636645030344, 28.26208216824729647, 14.16423886937410614 ) ) ;
#76139 = CARTESIAN_POINT ( 'NONE',  ( 7.084665262690076126, 67.02201867748817676, -10.88017736071110164 ) ) ;
#76140 = CARTESIAN_POINT ( 'NONE',  ( -2.816281873526471635, 8.915301336597083903, -3.434112377981056508 ) ) ;
#76141 = CARTESIAN_POINT ( 'NONE',  ( 10.00000000000000178, 42.25893115100078745, 9.846743663894594434 ) ) ;
#76142 = CARTESIAN_POINT ( 'NONE',  ( -8.897278993253172175, -15.56326597357423758, 3.750000000000000000 ) ) ;
#76144 = CARTESIAN_POINT ( 'NONE',  ( 19.38216949554541202, 20.99863466993042138, 9.382169495545424454 ) ) ;
#76143 = CARTESIAN_POINT ( 'NONE',  ( 0.5774900079438607392, 48.48035201082150536, 5.440088680355550821 ) ) ;
#76145 = CARTESIAN_POINT ( 'NONE',  ( 22.26659068614894466, 18.88708216824730002, 7.082119434687054849 ) ) ;
#76146 = B_SPLINE_CURVE_WITH_KNOTS ( 'NONE', 3,
 ( #61396, #61888, #8410, #46407, #76895, #69405 ),
 .UNSPECIFIED., .F., .F.,
 ( 4, 2, 4 ),
 ( 0.000000000000000000, 0.0002701661927229353360, 0.0005403323854458706721 ),
 .UNSPECIFIED. ) ;
#76147 = CARTESIAN_POINT ( 'NONE',  ( 17.96484262340118221, 9.938685344154839285, 7.964842623401181321 ) ) ;
#76148 = CARTESIAN_POINT ( 'NONE',  ( 2.035157376598824452, 28.68868534415484106, 7.964842623401179544 ) ) ;
#76149 = CARTESIAN_POINT ( 'NONE',  ( 2.035157376598822676, 62.43868534415483396, -7.964842623401177768 ) ) ;
#76150 = CARTESIAN_POINT ( 'NONE',  ( 19.38216949554541202, 45.99863466993041072, 9.382169495545424454 ) ) ;
#76151 = CARTESIAN_POINT ( 'NONE',  ( 3.469446951953614189E-15, -17.74106884899920900, 9.846743663894594434 ) ) ;
#76152 = ORIENTED_EDGE ( 'NONE', *, *, #42696, .F. ) ;
#76153 = CARTESIAN_POINT ( 'NONE',  ( 0.1558782227856947700, 15.00000000000000000, -14.62632331952783638 ) ) ;
#76154 = VERTEX_POINT ( 'NONE', #68859 ) ;
#76155 = CLOSED_SHELL ( 'NONE', ( #69885, #81404, #21909, #90987, #12766, #18110, #23830, #37728, #62112, #32897, #2897, #12595, #26279, #78964, #10269, #73268, #34091, #6469, #41742, #60845, #25972, #52619, #7036, #77148, #9556, #78148, #3093, #26969, #89630, #65233, #12759, #52437, #19868, #74631, #36423, #4321, #8958, #81803, #65322, #77087, #40246, #2978, #42968, #86630, #15153, #38971, #31283, #67513, #30755, #43327, #27462, #90875, #15841, #46683, #11327, #29676, #91020, #49566, #41691, #60068, #25660, #71132, #11854, #24979, #33216, #23180, #95738, #87950, #16422, #34592, #77031, #26728, #75070, #95609, #65850, #94268, #45324, #20079, #58933, #23014, #19100, #20572, #93975, #83901, #28088, #73705, #16864, #84997, #93564, #55796, #65361, #55181, #91661, #71192, #28035, #62251, #20450, #55307, #95683, #44043, #24749, #48086, #13371, #36135, #62644, #62029, #7130, #49240, #48558, #66779, #85111, #92555, #26233, #15640, #44448, #78122, #27339, #82120, #60946, #55066, #19431, #46801, #56014, #18183, #53385, #19831, #16060, #47247, #848, #80415, #6645, #93062, #12884, #35455, #29558, #51621, #23940, #30487, #91278, #60430, #49361, #92159, #19881, #38414, #43699, #42677, #87504, #13196, #53453, #1175, #2331, #38090, #30045, #63238, #56663, #91107, #56034, #2186, #31806, #62884, #10638, #64506, #36956, #86485, #35340, #75195, #36527, #12080, #77280, #96123, #79158, #13448, #90133, #16393, #80643, #92016, #4651, #40861, #4200, #29830, #82383, #33405, #144, #54290, #21696, #79132, #15201, #26911, #72940, #76824, #93637, #30196, #32648, #40986, #81586, #80046, #61780, #49642, #55723, #60882, #65330, #13909, #52070, #41388, #55104, #58465, #73259, #86608, #85915, #71516, #63828, #25021, #73503, #74512, #52588, #96951, #80618, #90027, #32638, #76858, #91888, #9315, #47653, #10682, #80374, #35604, #299, #32075, #13115, #32379, #26594, #92244, #86447, #64438, #60633, #55484, #59599, #47007, #65030, #32199, #63985, #88026, #76770, #42960, #90548, #55465, #29361, #31045, #75423, #47285, #13803, #86830, #93125, #11640, #3977, #10384, #35550, #57825, #52669, #56452, #17407, #9051, #32760, #65013, #10140, #40761, #82807, #22944, #65355, #6924, #92275, #46692, #38771, #32981, #54588, #96321, #29352, #7963, #383, #13572, #89114, #25072, #90277, #32722, #42135, #6563 ) ) ;
#76156 =( LENGTH_UNIT ( ) NAMED_UNIT ( * ) SI_UNIT ( .MILLI., .METRE. ) );
#76157 = ORIENTED_EDGE ( 'NONE', *, *, #13905, .F. ) ;
#76158 = CARTESIAN_POINT ( 'NONE',  ( 0.4400000000000020006, 1.019547802438468986, 4.000000000000000000 ) ) ;
#76160 = CARTESIAN_POINT ( 'NONE',  ( 20.36894250292379738, 59.92874883491397497, -10.36894250292379027 ) ) ;
#76159 = CARTESIAN_POINT ( 'NONE',  ( 10.00000000000000000, 55.55374883491396787, -14.16423886937410082 ) ) ;
#76162 = CARTESIAN_POINT ( 'NONE',  ( 0.1532563361054083140, 61.00893115100078745, 1.131784320476157264E-15 ) ) ;
#76161 = CARTESIAN_POINT ( 'NONE',  ( 12.63842701281683034, 27.46726448433411250, 9.846743663894596210 ) ) ;
#76163 = DIRECTION ( 'NONE',  ( -0.9961946980917453232, 0.08715574274766037244, 0.000000000000000000 ) ) ;
#76164 = EDGE_CURVE ( 'NONE', #80552, #81788, #75495, .T. ) ;
#76165 = CARTESIAN_POINT ( 'NONE',  ( 2.791683348922237240, 10.38393115100078390, -7.208316651077763204 ) ) ;
#76166 = CARTESIAN_POINT ( 'NONE',  ( 0.6178305044545818747, 33.49863466993042493, -9.382169495545419124 ) ) ;
#76167 = CARTESIAN_POINT ( 'NONE',  ( 3.469446951953614189E-15, 25.37363466993042138, 12.81628187352647608 ) ) ;
#76168 = VECTOR ( 'NONE', #55983, 1000.000000000000000 ) ;
#76169 = ORIENTED_EDGE ( 'NONE', *, *, #31605, .F. ) ;
#76170 = CARTESIAN_POINT ( 'NONE',  ( 10.00000000000000000, 35.55374883491396787, -14.16423886937410082 ) ) ;
#76171 = CARTESIAN_POINT ( 'NONE',  ( 17.08211943468705130, 48.47041550158063927, 12.26659068614894998 ) ) ;
#76172 = ORIENTED_EDGE ( 'NONE', *, *, #1722, .F. ) ;
#76173 = CARTESIAN_POINT ( 'NONE',  ( 3.591859063236761518, 59.95696800326375353, 11.09922568453594849 ) ) ;
#76174 = CARTESIAN_POINT ( 'NONE',  ( 7.084665262690076126, 24.10535201082150181, 10.88017736071109987 ) ) ;
#76175 = CARTESIAN_POINT ( 'NONE',  ( 19.84674366389459266, 48.71726448433413026, -2.638427012816827677 ) ) ;
#76176 = CARTESIAN_POINT ( 'NONE',  ( 10.00000000000000178, 24.31368534415484106, 10.88017736071110342 ) ) ;
#76177 = CARTESIAN_POINT ( 'NONE',  ( 13.07734668325339200, 2.778268066994105112E-16, 6.551438809693018506 ) ) ;
#76178 = DIRECTION ( 'NONE',  ( 0.000000000000000000, 0.000000000000000000, 1.000000000000000000 ) ) ;
#76179 = CARTESIAN_POINT ( 'NONE',  ( 10.00000000000000178, 52.25893115100078745, 9.846743663894594434 ) ) ;
#76180 = CARTESIAN_POINT ( 'NONE',  ( 1.472469842513823179, 46.42559781766745175, 4.923371831947296329 ) ) ;
#76182 = VERTEX_POINT ( 'NONE', #45860 ) ;
#76181 = CARTESIAN_POINT ( 'NONE',  ( 3.999999999999999112, 0.2999999999999981570, 4.898587196589411843E-16 ) ) ;
#76183 = CARTESIAN_POINT ( 'NONE',  ( 3.640395162852214650, 89.00000000000000000, -5.000000000000000000 ) ) ;
#76184 = CARTESIAN_POINT ( 'NONE',  ( 0.1532563361054100626, 5.800597817667452638, -2.638427012816831230 ) ) ;
#76185 = FILL_AREA_STYLE ('',( #77161 ) ) ;
#76186 = VERTEX_POINT ( 'NONE', #32309 ) ;
#76187 = AXIS2_PLACEMENT_3D ( 'NONE', #78537, #9546, #39071 ) ;
#76188 = CARTESIAN_POINT ( 'NONE',  ( 1.274849032794306947, 7.555090184799359676, -6.499999999999997335 ) ) ;
#76189 = CARTESIAN_POINT ( 'NONE',  ( 5.076628168052703671, 31.84226448433412315, 8.527530157486179263 ) ) ;
#76190 = CARTESIAN_POINT ( 'NONE',  ( -46.43582398220812024, 103.5217676819815580, 6.243076731245754019 ) ) ;
#76191 = CARTESIAN_POINT ( 'NONE',  ( 10.00000000000000178, 40.37363466993042493, 12.81628187352647608 ) ) ;
#76192 = CARTESIAN_POINT ( 'NONE',  ( 10.64017930668204670, 14.49999999999999112, 10.57291749337225362 ) ) ;
#76193 = DIRECTION ( 'NONE',  ( 0.000000000000000000, -0.000000000000000000, -1.000000000000000000 ) ) ;
#76194 = VECTOR ( 'NONE', #69553, 1000.000000000000000 ) ;
#76195 = VERTEX_POINT ( 'NONE', #24350 ) ;
#76196 = CARTESIAN_POINT ( 'NONE',  ( 0.1532563361054083140, 66.00893115100079456, 1.131784320476157264E-15 ) ) ;
#76197 = DIRECTION ( 'NONE',  ( -0.000000000000000000, -0.000000000000000000, -1.000000000000000000 ) ) ;
#76198 = CARTESIAN_POINT ( 'NONE',  ( 14.92337183194729988, 39.34226448433412315, -8.527530157486177487 ) ) ;
#76199 = CARTESIAN_POINT ( 'NONE',  ( -4.164238869374098151, 31.59541550158063927, -3.795296366450310543 ) ) ;
#76200 = CARTESIAN_POINT ( 'NONE',  ( 14.92337183194729988, 54.34226448433412315, -8.527530157486177487 ) ) ;
#76201 = DIRECTION ( 'NONE',  ( 0.6494480483301898754, 0.000000000000000000, -0.7604059656000257128 ) ) ;
#76202 = CARTESIAN_POINT ( 'NONE',  ( 0.1532563361054082862, 6.217264484334118713, 2.638427012816831674 ) ) ;
#76203 = EDGE_CURVE ( 'NONE', #19964, #19346, #85324, .T. ) ;
#76204 = AXIS2_PLACEMENT_3D ( 'NONE', #26003, #79493, #56497 ) ;
#76205 =( NAMED_UNIT ( * ) PLANE_ANGLE_UNIT ( ) SI_UNIT ( $, .RADIAN. ) );
#76206 = CARTESIAN_POINT ( 'NONE',  ( 2.791683348922237240, 50.38393115100078035, -7.208316651077763204 ) ) ;
#76207 = CARTESIAN_POINT ( 'NONE',  ( 7.084665262690076126, 52.02201867748816255, -10.88017736071110164 ) ) ;
#76208 = CIRCLE ( 'NONE', #96995, 0.2500000000000002220 ) ;
#76209 = AXIS2_PLACEMENT_3D ( 'NONE', #52521, #43057, #98052 ) ;
#76210 = APPLICATION_PROTOCOL_DEFINITION ( 'draft international standard', 'automotive_design', 1998, #26983 ) ;
#76211 = CARTESIAN_POINT ( 'NONE',  ( 0.8653096853334164562, -2.809184769568886286E-15, -14.59999144042651942 ) ) ;
#76212 = EDGE_CURVE ( 'NONE', #26051, #4700, #22873, .T. ) ;
#76213 = CARTESIAN_POINT ( 'NONE',  ( 4.559911319644449179, 47.23035201082150536, -9.422509992056141925 ) ) ;
#76214 = EDGE_CURVE ( 'NONE', #87207, #53171, #76351, .T. ) ;
#76215 = ADVANCED_FACE ( 'NONE', ( #7866 ), #868, .F. ) ;
#76216 = ORIENTED_EDGE ( 'NONE', *, *, #43822, .F. ) ;
#76217 = CARTESIAN_POINT ( 'NONE',  ( 64.56412365047461321, 28.99999999999999645, -9.500000000000000000 ) ) ;
#76218 = CARTESIAN_POINT ( 'NONE',  ( 0.5774900079438607392, 28.48035201082150891, 5.440088680355550821 ) ) ;
#76220 = CARTESIAN_POINT ( 'NONE',  ( 0.5774900079438590739, 57.64701867748817676, -5.440088680355550821 ) ) ;
#76219 = CARTESIAN_POINT ( 'NONE',  ( 3.591859063236761518, 4.956968003263753531, 11.09922568453594849 ) ) ;
#76221 = CARTESIAN_POINT ( 'NONE',  ( 0.000000000000000000, 15.00000000000000000, 0.000000000000000000 ) ) ;
#76222 = CARTESIAN_POINT ( 'NONE',  ( 19.84674366389459621, 13.50893115100078568, 7.409399052514197653E-17 ) ) ;
#76223 = SURFACE_SIDE_STYLE ('',( #45721 ) ) ;
#76225 = DIRECTION ( 'NONE',  ( -0.000000000000000000, -1.000000000000000000, -0.000000000000000000 ) ) ;
#76224 = CARTESIAN_POINT ( 'NONE',  ( -0.8801773607111008646, 33.27201867748817676, 2.915334737309923430 ) ) ;
#76226 = CARTESIAN_POINT ( 'NONE',  ( 18.52753015748617571, 13.09226448433411960, 4.923371831947298993 ) ) ;
#76227 = CARTESIAN_POINT ( 'NONE',  ( 7.361572987183169658, 39.96726448433411605, -9.846743663894592657 ) ) ;
#76228 = CARTESIAN_POINT ( 'NONE',  ( -6.349999999999995204, -97.00000000000000000, -3.750000000000000000 ) ) ;
#76229 = CARTESIAN_POINT ( 'NONE',  ( 14.16423886937410082, 24.51208216824729647, -3.795296366450314096 ) ) ;
#76230 = CARTESIAN_POINT ( 'NONE',  ( 22.81628187352648496, 1.831968003263753753, -3.434112377981050290 ) ) ;
#76231 = CARTESIAN_POINT ( 'NONE',  ( -2.266590686148945544, 62.22041550158063927, 7.082119434687048631 ) ) ;
#76232 = CARTESIAN_POINT ( 'NONE',  ( -15.94000000000001371, 93.50000000000000000, -9.500000000000000000 ) ) ;
#76233 = CARTESIAN_POINT ( 'NONE',  ( 24.16423886937409904, 24.09541550158063927, 3.795296366450317205 ) ) ;
#76234 = CARTESIAN_POINT ( 'NONE',  ( 20.36894250292379738, 54.92874883491396076, -10.36894250292379027 ) ) ;
#76235 = CARTESIAN_POINT ( 'NONE',  ( 0.1532563361054082862, 16.21726448433411960, 2.638427012816831674 ) ) ;
#76236 = CARTESIAN_POINT ( 'NONE',  ( 7.361572987183170547, 27.05059781766745175, 9.846743663894590881 ) ) ;
#76237 = CARTESIAN_POINT ( 'NONE',  ( 15.44008868035555793, 26.39701867748817321, -9.422509992056140149 ) ) ;
#76238 = CARTESIAN_POINT ( 'NONE',  ( 19.84674366389459621, 48.50893115100078745, 7.409399052514197653E-17 ) ) ;
#76240 = DIRECTION ( 'NONE',  ( 0.000000000000000000, 0.000000000000000000, -1.000000000000000000 ) ) ;
#76239 = CARTESIAN_POINT ( 'NONE',  ( 22.26659068614894466, 13.88708216824730179, 7.082119434687054849 ) ) ;
#76241 = PLANE ( 'NONE',  #67964 ) ;
#76242 = CIRCLE ( 'NONE', #52252, 15.00000000000000000 ) ;
#76243 = CARTESIAN_POINT ( 'NONE',  ( 0.1532563361054083140, 16.00893115100078390, 1.131784320476157264E-15 ) ) ;
#76244 = CARTESIAN_POINT ( 'NONE',  ( 6.565887622018943937, 35.16530133659708923, 12.81628187352647430 ) ) ;
#76245 = CARTESIAN_POINT ( 'NONE',  ( 0.1532563361054082862, 36.21726448433410894, 2.638427012816831674 ) ) ;
#76246 = ORIENTED_EDGE ( 'NONE', *, *, #82418, .T. ) ;
#76247 = CARTESIAN_POINT ( 'NONE',  ( 14.92337183194729633, 27.67559781766745530, 8.527530157486181039 ) ) ;
#76248 = EDGE_CURVE ( 'NONE', #2391, #23479, #59502, .T. ) ;
#76249 = CARTESIAN_POINT ( 'NONE',  ( 11.19532855852642328, -77.48518070173305716, -4.000000000000000000 ) ) ;
#76250 = LINE ( 'NONE', #5782, #33127 ) ;
#76251 = CARTESIAN_POINT ( 'NONE',  ( 22.26659068614894466, 53.88708216824731068, 7.082119434687054849 ) ) ;
#76252 = DIRECTION ( 'NONE',  ( -0.000000000000000000, -1.000000000000000000, -0.000000000000000000 ) ) ;
#76253 = CARTESIAN_POINT ( 'NONE',  ( 2.791683348922237240, 30.38393115100078390, -7.208316651077763204 ) ) ;
#76254 = CARTESIAN_POINT ( 'NONE',  ( 17.20831665107776587, 34.13393115100078745, -7.208316651077762316 ) ) ;
#76255 = CARTESIAN_POINT ( 'NONE',  ( 18.95785429995052951, 2.242161081720065230, 6.499999999999868550 ) ) ;
#76256 = CARTESIAN_POINT ( 'NONE',  ( 18.52753015748617571, 53.09226448433412315, 4.923371831947298993 ) ) ;
#76257 = CARTESIAN_POINT ( 'NONE',  ( 17.96484262340118221, 56.18868534415484817, -7.964842623401177768 ) ) ;
#76258 = AXIS2_PLACEMENT_3D ( 'NONE', #44749, #75252, #7764 ) ;
#76259 = ORIENTED_EDGE ( 'NONE', *, *, #427, .F. ) ;
#76260 = ORIENTED_EDGE ( 'NONE', *, *, #80594, .F. ) ;
#76261 = CARTESIAN_POINT ( 'NONE',  ( 13.43411237798106583, 57.66530133659708923, -12.81628187352647252 ) ) ;
#76262 = CARTESIAN_POINT ( 'NONE',  ( 11.24999999999999822, 5.630135511184877650, -3.014428414850134796 ) ) ;
#76263 = CARTESIAN_POINT ( 'NONE',  ( 0.1532563361054082862, 11.21726448433411605, 2.638427012816831674 ) ) ;
#76264 = CARTESIAN_POINT ( 'NONE',  ( 3.591859063236761518, 54.95696800326376064, 11.09922568453594849 ) ) ;
#76266 = CARTESIAN_POINT ( 'NONE',  ( 12.63842701281683922, 49.55059781766744464, -9.846743663894590881 ) ) ;
#76265 = CARTESIAN_POINT ( 'NONE',  ( 19.42250999205614193, 10.14701867748816966, 5.440088680355555262 ) ) ;
#76267 = CARTESIAN_POINT ( 'NONE',  ( 17.39651004071842522, 19.08210964143329491, -6.499999999999992895 ) ) ;
#76268 = CARTESIAN_POINT ( 'NONE',  ( 10.00000000000000000, 30.55374883491397142, -14.16423886937410082 ) ) ;
#76269 = CARTESIAN_POINT ( 'NONE',  ( 24.16423886937409904, 59.09541550158063217, 3.795296366450317205 ) ) ;
#76270 = CARTESIAN_POINT ( 'NONE',  ( 17.20831665107776587, 57.88393115100078745, 7.208316651077764980 ) ) ;
#76271 = CARTESIAN_POINT ( 'NONE',  ( 11.24699797944280100, 54.09857164847241506, 0.000000000000000000 ) ) ;
#76272 = CARTESIAN_POINT ( 'NONE',  ( 19.42250999205614548, 45.98035201082150536, -5.440088680355545492 ) ) ;
#76273 = CARTESIAN_POINT ( 'NONE',  ( 17.96484262340118221, 66.18868534415483396, -7.964842623401177768 ) ) ;
#76274 = AXIS2_PLACEMENT_3D ( 'NONE', #48718, #79221, #3236 ) ;
#76275 = CARTESIAN_POINT ( 'NONE',  ( -3.500000001642929792, 0.08393865083513252223, 4.000000000000000000 ) ) ;
#76276 = EDGE_LOOP ( 'NONE', ( #71256, #96347, #72555, #14164 ) ) ;
#76277 = CARTESIAN_POINT ( 'NONE',  ( -2.816281873526473856, 59.12363466993042493, 9.499525473075851096E-16 ) ) ;
#76278 = ORIENTED_EDGE ( 'NONE', *, *, #83822, .T. ) ;
#76279 = CARTESIAN_POINT ( 'NONE',  ( 14.92337183194729633, 7.675597817667451750, 8.527530157486181039 ) ) ;
#76280 = VERTEX_POINT ( 'NONE', #64274 ) ;
#76281 = CARTESIAN_POINT ( 'NONE',  ( -0.3689425029237898834, 21.17874883491396432, -10.36894250292378850 ) ) ;
#76282 = CARTESIAN_POINT ( 'NONE',  ( 2.791683348922237240, 25.38393115100078390, -7.208316651077763204 ) ) ;
#76283 = CARTESIAN_POINT ( 'NONE',  ( 12.91533473730993009, 26.60535201082150536, -10.88017736071109987 ) ) ;
#76284 =( GEOMETRIC_REPRESENTATION_CONTEXT ( 3 ) GLOBAL_UNCERTAINTY_ASSIGNED_CONTEXT ( ( #2368 ) ) GLOBAL_UNIT_ASSIGNED_CONTEXT ( ( #13505, #37500, #52969 ) ) REPRESENTATION_CONTEXT ( 'NONE', 'WORKASPACE' ) );
#76285 = ORIENTED_EDGE ( 'NONE', *, *, #45048, .T. ) ;
#76286 = TOROIDAL_SURFACE ( 'NONE', #6053, 14.49999999999999822, 0.5000000000000000000 ) ;
#76287 = CARTESIAN_POINT ( 'NONE',  ( 2.035157376598822676, 27.43868534415483396, -7.964842623401177768 ) ) ;
#76288 = ORIENTED_EDGE ( 'NONE', *, *, #18061, .T. ) ;
#76289 = CARTESIAN_POINT ( 'NONE',  ( 10.00000000000000178, 39.31368534415484106, 10.88017736071110342 ) ) ;
#76290 = SURFACE_STYLE_USAGE ( .BOTH. , #23308 ) ;
#76291 = ORIENTED_EDGE ( 'NONE', *, *, #90758, .F. ) ;
#76292 = EDGE_LOOP ( 'NONE', ( #23057, #220, #84287, #15456 ) ) ;
#76293 = CARTESIAN_POINT ( 'NONE',  ( 21.09922568453594849, 16.20696800326375353, 6.408140936763242479 ) ) ;
#76294 = CARTESIAN_POINT ( 'NONE',  ( 1.472469842513823179, 16.42559781766745175, 4.923371831947296329 ) ) ;
#76295 = CARTESIAN_POINT ( 'NONE',  ( 14.16722289976682170, 0.3640475087720934089, 4.928467845925620594 ) ) ;
#76296 = DIRECTION ( 'NONE',  ( 0.7009092642998425715, 0.000000000000000000, 0.7132504491541897806 ) ) ;
#76297 = CARTESIAN_POINT ( 'NONE',  ( 2.791683348922237240, 20.38393115100078745, -7.208316651077763204 ) ) ;
#76298 = CARTESIAN_POINT ( 'NONE',  ( 20.88017736071110519, 30.56368534415484106, 2.639326808657452039E-16 ) ) ;
#76299 = EDGE_CURVE ( 'NONE', #15068, #72111, #71799, .T. ) ;
#76300 = ORIENTED_EDGE ( 'NONE', *, *, #2134, .F. ) ;
#76301 = CARTESIAN_POINT ( 'NONE',  ( 32.56412365047463453, 14.00000000000001066, 9.500000000000000000 ) ) ;
#76302 = CARTESIAN_POINT ( 'NONE',  ( 4.559911319644449179, 57.23035201082150536, -9.422509992056141925 ) ) ;
#76303 = FACE_OUTER_BOUND ( 'NONE', #54369, .T. ) ;
#76304 = CARTESIAN_POINT ( 'NONE',  ( -1.099225684535947600, 58.70696800326375353, -6.408140936763238038 ) ) ;
#76305 = CARTESIAN_POINT ( 'NONE',  ( -0.8801773607110991993, 62.85535201082150536, -2.915334737309923874 ) ) ;
#76306 = CARTESIAN_POINT ( 'NONE',  ( -1.099225684535947600, 3.706968003263753531, -6.408140936763238038 ) ) ;
#76307 = DIRECTION ( 'NONE',  ( -0.000000000000000000, -0.000000000000000000, 1.000000000000000000 ) ) ;
#76308 = CARTESIAN_POINT ( 'NONE',  ( 17.20831665107776587, 34.13393115100078745, -7.208316651077762316 ) ) ;
#76309 = CARTESIAN_POINT ( 'NONE',  ( 6.565887622018943937, 55.16530133659709634, 12.81628187352647430 ) ) ;
#76310 = CARTESIAN_POINT ( 'NONE',  ( 1.274849032794292736, 37.55509018479936145, -6.499999999999977796 ) ) ;
#76311 = CARTESIAN_POINT ( 'NONE',  ( 12.63842701281683034, 12.46726448433411782, 9.846743663894596210 ) ) ;
#76312 = CARTESIAN_POINT ( 'NONE',  ( -1.099225684535947600, 19.54030133659708568, 6.408140936763237150 ) ) ;
#76314 = CARTESIAN_POINT ( 'NONE',  ( 0.000000000000000000, 15.00000000000000000, 0.000000000000000000 ) ) ;
#76313 = CARTESIAN_POINT ( 'NONE',  ( -46.43542959741873943, 103.9441885970218351, 5.610226944091865953 ) ) ;
#76315 = CARTESIAN_POINT ( 'NONE',  ( 10.00000000000000000, 36.81368534415484106, -10.88017736071110342 ) ) ;
#76316 = CARTESIAN_POINT ( 'NONE',  ( 18.52753015748618282, 63.92559781766745886, -4.923371831947291888 ) ) ;
#76317 = CARTESIAN_POINT ( 'NONE',  ( 10.00000000000000000, 24.75893115100078745, -9.846743663894594434 ) ) ;
#76318 = CARTESIAN_POINT ( 'NONE',  ( 12.63842701281683922, 4.550597817667451750, -9.846743663894590881 ) ) ;
#76319 = CARTESIAN_POINT ( 'NONE',  ( 2.035157376598822676, 17.43868534415483751, -7.964842623401177768 ) ) ;
#76320 = CARTESIAN_POINT ( 'NONE',  ( 13.43411237798106583, 17.66530133659708923, -12.81628187352647252 ) ) ;
#76321 = CIRCLE ( 'NONE', #98770, 10.00000000000000178 ) ;
#76322 = CARTESIAN_POINT ( 'NONE',  ( 5.076628168052703671, 61.84226448433412315, 8.527530157486179263 ) ) ;
#76323 = EDGE_CURVE ( 'NONE', #81201, #93263, #40328, .T. ) ;
#76324 = CARTESIAN_POINT ( 'NONE',  ( 20.88017736071110164, 10.35535201082150714, 2.915334737309930979 ) ) ;
#76325 = CARTESIAN_POINT ( 'NONE',  ( 14.92337183194729988, 49.34226448433411605, -8.527530157486177487 ) ) ;
#76326 = EDGE_CURVE ( 'NONE', #35833, #15318, #62814, .T. ) ;
#76327 = ORIENTED_EDGE ( 'NONE', *, *, #97574, .F. ) ;
#76328 = CARTESIAN_POINT ( 'NONE',  ( -8.124115902427741176, 75.04369783535875627, -2.900000000000000355 ) ) ;
#76329 = CARTESIAN_POINT ( 'NONE',  ( 2.917880565312948704, 67.63708216824730357, 12.26659068614894643 ) ) ;
#76330 = CARTESIAN_POINT ( 'NONE',  ( 19.90229974777923161, 69.67742753483354079, -6.500000000000000000 ) ) ;
#76331 = CARTESIAN_POINT ( 'NONE',  ( -0.8801773607110991993, 32.85535201082151247, -2.915334737309923874 ) ) ;
#76332 = PRESENTATION_LAYER_ASSIGNMENT (  '', '', ( #55642 ) ) ;
#76334 = DIRECTION ( 'NONE',  ( 1.000000000000000000, 0.000000000000000000, 0.000000000000000000 ) ) ;
#76333 = CARTESIAN_POINT ( 'NONE',  ( 10.00000000000000000, 60.55374883491397497, -14.16423886937410082 ) ) ;
#76335 = CARTESIAN_POINT ( 'NONE',  ( 18.52753015748618282, 23.92559781766745530, -4.923371831947291888 ) ) ;
#76336 = CARTESIAN_POINT ( 'NONE',  ( 21.09922568453594849, 11.20696800326375531, 6.408140936763242479 ) ) ;
#76337 = CARTESIAN_POINT ( 'NONE',  ( 24.35999999999999233, 37.99999999999997868, 10.00000000000000000 ) ) ;
#76338 = CARTESIAN_POINT ( 'NONE',  ( 6.767445849361251042, 0.3639308223168553624, -13.38662304974500472 ) ) ;
#76340 = CARTESIAN_POINT ( 'NONE',  ( 9.876730923139225737, 0.5000000000000004441, 11.28938378619069560 ) ) ;
#76339 = AXIS2_PLACEMENT_3D ( 'NONE', #68767, #298, #46260 ) ;
#76341 = VECTOR ( 'NONE', #87692, 1000.000000000000000 ) ;
#76342 = CARTESIAN_POINT ( 'NONE',  ( -8.000000002515021080, -0.01655697268385602355, -4.000000000000000000 ) ) ;
#76343 = CARTESIAN_POINT ( 'NONE',  ( 22.26659068614895176, 14.72041550158063572, -7.082119434687042414 ) ) ;
#76344 = CARTESIAN_POINT ( 'NONE',  ( 14.92337183194729988, 24.34226448433411960, -8.527530157486177487 ) ) ;
#76345 = CARTESIAN_POINT ( 'NONE',  ( -11.22915323889586858, 15.00000000000000000, 8.773176023390528044 ) ) ;
#76346 = VERTEX_POINT ( 'NONE', #18803 ) ;
#76347 = EDGE_CURVE ( 'NONE', #37030, #58432, #48364, .T. ) ;
#76348 = CARTESIAN_POINT ( 'NONE',  ( 13.79529636645030344, 48.26208216824728936, 14.16423886937410614 ) ) ;
#76349 = ADVANCED_FACE ( 'NONE', ( #48791 ), #80269, .T. ) ;
#76350 = CARTESIAN_POINT ( 'NONE',  ( 5.076628168052704559, 5.175597817667451750, -8.527530157486179263 ) ) ;
#76352 = DIRECTION ( 'NONE',  ( 0.000000000000000000, 0.000000000000000000, 1.000000000000000000 ) ) ;
#76351 = LINE ( 'NONE', #45353, #73835 ) ;
#76353 = CARTESIAN_POINT ( 'NONE',  ( 12.91533473730993009, 31.60535201082150891, -10.88017736071109987 ) ) ;
#76354 = CARTESIAN_POINT ( 'NONE',  ( 3.591859063236763294, 53.29030133659708923, -11.09922568453595026 ) ) ;
#76355 = CARTESIAN_POINT ( 'NONE',  ( 10.00000000000000178, 19.31368534415484106, 10.88017736071110342 ) ) ;
#76356 = CARTESIAN_POINT ( 'NONE',  ( 22.81628187352648496, 41.83196800326375353, -3.434112377981050290 ) ) ;
#76357 = CARTESIAN_POINT ( 'NONE',  ( 12.63842701281683922, 64.55059781766745175, -9.846743663894590881 ) ) ;
#76358 = CARTESIAN_POINT ( 'NONE',  ( 1.472469842513823179, 0.5922644843341181575, -4.923371831947296329 ) ) ;
#76359 = ORIENTED_EDGE ( 'NONE', *, *, #39383, .T. ) ;
#76360 =( NAMED_UNIT ( * ) PLANE_ANGLE_UNIT ( ) SI_UNIT ( $, .RADIAN. ) );
#76361 = EDGE_CURVE ( 'NONE', #35180, #59059, #17818, .T. ) ;
#76362 = CARTESIAN_POINT ( 'NONE',  ( 12.00809552683953463, 14.63595249122789177, 8.989195838243631442 ) ) ;
#76363 = CARTESIAN_POINT ( 'NONE',  ( 24.16423886937409904, 39.09541550158062506, 3.795296366450317205 ) ) ;
#76364 = CARTESIAN_POINT ( 'NONE',  ( 20.36894250292379738, 9.928748834913966093, -10.36894250292379027 ) ) ;
#76365 = CARTESIAN_POINT ( 'NONE',  ( 2.035157376598822676, 2.438685344154837953, -7.964842623401177768 ) ) ;
#76366 = CARTESIAN_POINT ( 'NONE',  ( 0.5774900079438590739, 37.64701867748817676, -5.440088680355550821 ) ) ;
#76367 = FACE_OUTER_BOUND ( 'NONE', #40897, .T. ) ;
#76368 = DIRECTION ( 'NONE',  ( 0.8038568606172162845, 0.000000000000000000, 0.5948227867513425915 ) ) ;
#76369 = CARTESIAN_POINT ( 'NONE',  ( 18.52753015748617571, 3.092264484334118269, 4.923371831947298993 ) ) ;
#76370 = CARTESIAN_POINT ( 'NONE',  ( 8.813102413620015341, 15.00000000000000000, 13.34940531570970457 ) ) ;
#76371 = CARTESIAN_POINT ( 'NONE',  ( -2.816281873526473856, 24.12363466993042138, 9.499525473075851096E-16 ) ) ;
#76372 = CARTESIAN_POINT ( 'NONE',  ( 1.707155281725170726, 62.90189080397286148, 6.499999999999955591 ) ) ;
#76373 = FACE_OUTER_BOUND ( 'NONE', #85641, .T. ) ;
#76374 = CARTESIAN_POINT ( 'NONE',  ( 14.92337183194729633, 32.67559781766745175, 8.527530157486181039 ) ) ;
#76375 = CARTESIAN_POINT ( 'NONE',  ( 4.559911319644449179, 13.89701867748817143, 9.422509992056141925 ) ) ;
#76376 = CARTESIAN_POINT ( 'NONE',  ( 0.6178305044545838731, 24.74863466993042493, 9.382169495545420901 ) ) ;
#76377 = CARTESIAN_POINT ( 'NONE',  ( 2.791683348922237240, 15.38393115100078212, -7.208316651077763204 ) ) ;
#76378 = CARTESIAN_POINT ( 'NONE',  ( 7.084665262690076126, 12.02201867748817143, -10.88017736071110164 ) ) ;
#76379 = CARTESIAN_POINT ( 'NONE',  ( 0.1532563361054083140, 41.00893115100078745, 1.131784320476157264E-15 ) ) ;
#76380 = CARTESIAN_POINT ( 'NONE',  ( 6.565887622018943937, 58.08196800326376064, -12.81628187352647608 ) ) ;
#76381 = CARTESIAN_POINT ( 'NONE',  ( 7.361572987183169658, 19.96726448433411960, -9.846743663894592657 ) ) ;
#76382 = CARTESIAN_POINT ( 'NONE',  ( 20.36894250292379738, 9.928748834913966093, -10.36894250292379027 ) ) ;
#76383 = CARTESIAN_POINT ( 'NONE',  ( 5.817157072110804350, 14.49999999999999112, -13.82608706751093663 ) ) ;
#76384 = CARTESIAN_POINT ( 'NONE',  ( 4.559911319644449179, 33.89701867748817676, 9.422509992056141925 ) ) ;
#76386 = CARTESIAN_POINT ( 'NONE',  ( 17.08211943468705840, 40.13708216824731068, -12.26659068614894466 ) ) ;
#76385 = CARTESIAN_POINT ( 'NONE',  ( -0.8801773607111008646, 8.272018677488171434, 2.915334737309923430 ) ) ;
#76387 = CARTESIAN_POINT ( 'NONE',  ( 12.91533473730993009, 36.60535201082151247, -10.88017736071109987 ) ) ;
#76388 = VECTOR ( 'NONE', #27772, 1000.000000000000000 ) ;
#76389 = CARTESIAN_POINT ( 'NONE',  ( 20.88017736071110519, 20.56368534415484106, 2.639326808657452039E-16 ) ) ;
#76390 = ORIENTED_EDGE ( 'NONE', *, *, #83383, .F. ) ;
#76391 = CARTESIAN_POINT ( 'NONE',  ( 20.88017736071110519, 45.56368534415484106, 2.639326808657452039E-16 ) ) ;
#76392 = CARTESIAN_POINT ( 'NONE',  ( 10.00000000000000178, 60.37363466993041783, 12.81628187352647608 ) ) ;
#76393 = CARTESIAN_POINT ( 'NONE',  ( 20.88017736071110519, 50.56368534415484106, 2.639326808657452039E-16 ) ) ;
#76394 = CARTESIAN_POINT ( 'NONE',  ( 4.559911319644449179, 57.23035201082150536, -9.422509992056141925 ) ) ;
#76395 = AXIS2_PLACEMENT_3D ( 'NONE', #97947, #43429, #81921 ) ;
#76396 = ORIENTED_EDGE ( 'NONE', *, *, #47195, .F. ) ;
#76397 = CARTESIAN_POINT ( 'NONE',  ( 7.084665262690076126, 57.02201867748817676, -10.88017736071110164 ) ) ;
#76398 = CARTESIAN_POINT ( 'NONE',  ( 4.657035931814768048, -8.268334176803392666, 3.749999999999597211 ) ) ;
#76399 = CARTESIAN_POINT ( 'NONE',  ( 4.265913727722096205, 0.04962886353675406703, 14.12300574719581903 ) ) ;
#76400 = CARTESIAN_POINT ( 'NONE',  ( -4.164238869374098151, 41.59541550158061796, -3.795296366450310543 ) ) ;
#76401 = CARTESIAN_POINT ( 'NONE',  ( 7.361572987183169658, -0.03273551566588185635, -9.846743663894592657 ) ) ;
#76402 = DIRECTION ( 'NONE',  ( 0.000000000000000000, 0.000000000000000000, 1.000000000000000000 ) ) ;
#76403 = CARTESIAN_POINT ( 'NONE',  ( -7.371420888394235149, -73.25401859617248590, -4.000000000000000888 ) ) ;
#76404 = CARTESIAN_POINT ( 'NONE',  ( 1.472469842513823179, 60.59226448433412315, -4.923371831947296329 ) ) ;
#76405 = CARTESIAN_POINT ( 'NONE',  ( 10.00000000000000178, 32.25893115100078745, 9.846743663894594434 ) ) ;
#76406 = EDGE_LOOP ( 'NONE', ( #58681, #19212, #20396, #94502, #62032 ) ) ;
#76407 = CARTESIAN_POINT ( 'NONE',  ( 10.00000000000000000, 34.75893115100078745, -9.846743663894594434 ) ) ;
#76408 = CARTESIAN_POINT ( 'NONE',  ( -9.382169495545413795, -5.251365330069575954, 9.382169495545428006 ) ) ;
#76409 = AXIS2_PLACEMENT_3D ( 'NONE', #43104, #14100, #97619 ) ;
#76410 = CARTESIAN_POINT ( 'NONE',  ( 0.5774900079438590739, 42.64701867748816966, -5.440088680355550821 ) ) ;
#76411 = CARTESIAN_POINT ( 'NONE',  ( 7.361572987183170547, 37.05059781766744464, 9.846743663894590881 ) ) ;
#76412 = CARTESIAN_POINT ( 'NONE',  ( 21.09922568453594849, 21.20696800326375353, 6.408140936763242479 ) ) ;
#76414 = CARTESIAN_POINT ( 'NONE',  ( 12.91533473730992121, 59.52201867748816966, 10.88017736071110164 ) ) ;
#76413 = LINE ( 'NONE', #44917, #19599 ) ;
#76416 = CARTESIAN_POINT ( 'NONE',  ( 2.035157376598822676, 2.438685344154837953, -7.964842623401177768 ) ) ;
#76415 = CARTESIAN_POINT ( 'NONE',  ( 20.88017736071110875, 40.77201867748818387, -2.915334737309920765 ) ) ;
#76417 = CARTESIAN_POINT ( 'NONE',  ( 2.917880565312948704, 52.63708216824730357, 12.26659068614894643 ) ) ;
#76418 = EDGE_CURVE ( 'NONE', #21351, #32629, #26286, .T. ) ;
#76419 = STYLED_ITEM ( 'NONE', ( #92019 ), #70810 ) ;
#76420 = CARTESIAN_POINT ( 'NONE',  ( 22.81628187352648496, 16.83196800326374998, -3.434112377981050290 ) ) ;
#76421 = CARTESIAN_POINT ( 'NONE',  ( 0.000000000000000000, 14.49999999999999822, 0.000000000000000000 ) ) ;
#76422 = ORIENTED_EDGE ( 'NONE', *, *, #81515, .F. ) ;
#76423 = CARTESIAN_POINT ( 'NONE',  ( 19.38216949554541557, 17.24863466993041783, -9.382169495545420901 ) ) ;
#76424 = CARTESIAN_POINT ( 'NONE',  ( 15.44008868035555793, 16.39701867748817321, -9.422509992056140149 ) ) ;
#76425 = CARTESIAN_POINT ( 'NONE',  ( 15.44008868035555793, 66.39701867748817676, -9.422509992056140149 ) ) ;
#76426 = ORIENTED_EDGE ( 'NONE', *, *, #72570, .T. ) ;
#76427 = CARTESIAN_POINT ( 'NONE',  ( -0.8801773607111008646, 68.27201867748817676, 2.915334737309923430 ) ) ;
#76428 =( BOUNDED_CURVE ( )  B_SPLINE_CURVE ( 2, ( #4187, #89147, #88650, #50159, #51153, #65154, #80668, #74128, #80167 ),
 .UNSPECIFIED., .F., .T. ) 
 B_SPLINE_CURVE_WITH_KNOTS ( ( 3, 2, 2, 2, 3 ),
 ( 0.8329980797973741691, 0.8333333333333333703, 0.8392857142857143016, 0.8452380952380952328, 0.8455733487740543231 ),
 .UNSPECIFIED. ) 
 CURVE ( )  GEOMETRIC_REPRESENTATION_ITEM ( )  RATIONAL_B_SPLINE_CURVE ( ( 0.9963778908391753841, 0.9980808541467917072, 1.000000000000000000, 0.9659258262890683122, 1.000000000000000000, 0.9659258262890683122, 1.000000000000000000, 0.9980808541467922623, 0.9963778908391764944 ) ) 
 REPRESENTATION_ITEM ( '' )  );
#76429 = CARTESIAN_POINT ( 'NONE',  ( 2.791683348922237240, 55.38393115100078745, -7.208316651077763204 ) ) ;
#76430 = CARTESIAN_POINT ( 'NONE',  ( 7.361572987183169658, 29.96726448433411960, -9.846743663894592657 ) ) ;
#76431 = CARTESIAN_POINT ( 'NONE',  ( 10.00000000000000000, 29.75893115100078745, -9.846743663894594434 ) ) ;
#76432 = DIRECTION ( 'NONE',  ( 1.000000000000000000, 0.000000000000000000, 0.000000000000000000 ) ) ;
#76434 = CARTESIAN_POINT ( 'NONE',  ( 10.00000000000000000, 42.87363466993042493, -12.81628187352647608 ) ) ;
#76433 = CARTESIAN_POINT ( 'NONE',  ( -14.03351048042393856, -0.03417435944610275333, -2.474486531753901541 ) ) ;
#76436 = CARTESIAN_POINT ( 'NONE',  ( 0.000000000000000000, 14.49999999999999822, 0.000000000000000000 ) ) ;
#76435 = CARTESIAN_POINT ( 'NONE',  ( 7.361572987183169658, 14.96726448433411960, -9.846743663894592657 ) ) ;
#76437 = DIRECTION ( 'NONE',  ( 0.000000000000000000, 0.000000000000000000, -1.000000000000000000 ) ) ;
#76439 = ORIENTED_EDGE ( 'NONE', *, *, #60822, .F. ) ;
#76438 = CARTESIAN_POINT ( 'NONE',  ( 14.92337183194729988, 49.34226448433411605, -8.527530157486177487 ) ) ;
#76440 = CARTESIAN_POINT ( 'NONE',  ( 8.235571585149866536, 3.243033628982648686, -8.235571585149871865 ) ) ;
#76441 = EDGE_CURVE ( 'NONE', #952, #30382, #58059, .T. ) ;
#76442 = CARTESIAN_POINT ( 'NONE',  ( 13.43411237798105340, 15.58196800326374998, 12.81628187352647963 ) ) ;
#76443 = CARTESIAN_POINT ( 'NONE',  ( 15.44008868035555793, 51.39701867748816966, -9.422509992056140149 ) ) ;
#76444 = CARTESIAN_POINT ( 'NONE',  ( 2.917880565312948704, 32.63708216824730357, 12.26659068614894643 ) ) ;
#76445 = EDGE_CURVE ( 'NONE', #66663, #71139, #87282, .T. ) ;
#76446 = DIRECTION ( 'NONE',  ( 0.000000000000000000, -1.000000000000000000, 0.000000000000000000 ) ) ;
#76447 = CARTESIAN_POINT ( 'NONE',  ( -4.164238869374099927, 27.01208216824730357, 3.795296366450308767 ) ) ;
#76448 = CARTESIAN_POINT ( 'NONE',  ( 22.26659068614895176, 59.72041550158063927, -7.082119434687042414 ) ) ;
#76449 = CARTESIAN_POINT ( 'NONE',  ( -0.3689425029237898834, 16.17874883491396076, -10.36894250292378850 ) ) ;
#76451 = DIRECTION ( 'NONE',  ( 0.9995586998285053149, 0.02970531260815256758, 0.000000000000000000 ) ) ;
#76450 = CARTESIAN_POINT ( 'NONE',  ( 17.08211943468705130, 23.47041550158063572, 12.26659068614894998 ) ) ;
#76452 = CARTESIAN_POINT ( 'NONE',  ( 2.035157376598822676, 42.43868534415483396, -7.964842623401177768 ) ) ;
#76453 = CARTESIAN_POINT ( 'NONE',  ( 19.80832241502128355, 24.75868815902069997, 6.499999999999992895 ) ) ;
#76454 = AXIS2_PLACEMENT_3D ( 'NONE', #14151, #23139, #30608 ) ;
#76456 = CARTESIAN_POINT ( 'NONE',  ( 19.84674366389459621, 48.50893115100078745, 7.409399052514197653E-17 ) ) ;
#76455 = CARTESIAN_POINT ( 'NONE',  ( 4.864310448992819502, -17.52237222647785941, 2.500000000000000000 ) ) ;
#76457 = CARTESIAN_POINT ( 'NONE',  ( 15.44008868035555260, 19.73035201082150536, 9.422509992056143702 ) ) ;
#76458 = DIRECTION ( 'NONE',  ( -0.000000000000000000, -0.000000000000000000, 1.000000000000000000 ) ) ;
#76459 = CARTESIAN_POINT ( 'NONE',  ( 5.076628168052704559, 65.17559781766745175, -8.527530157486179263 ) ) ;
#76460 = CARTESIAN_POINT ( 'NONE',  ( 19.65543155966253153, 85.76032626422811234, -5.359767647080686537 ) ) ;
#76461 = CARTESIAN_POINT ( 'NONE',  ( 7.361572987183170547, 27.05059781766745175, 9.846743663894590881 ) ) ;
#76462 = CARTESIAN_POINT ( 'NONE',  ( -2.816281873526473856, 59.12363466993042493, 9.499525473075851096E-16 ) ) ;
#76463 = CARTESIAN_POINT ( 'NONE',  ( 14.16423886937410259, -0.6962511650860301327, -2.602085213965210642E-15 ) ) ;
#76464 = CARTESIAN_POINT ( 'NONE',  ( 17.20831665107776587, 47.88393115100078745, 7.208316651077764980 ) ) ;
#76465 = CARTESIAN_POINT ( 'NONE',  ( 14.92337183194729633, 47.67559781766745175, 8.527530157486181039 ) ) ;
#76466 = CARTESIAN_POINT ( 'NONE',  ( 24.16423886937410614, 44.51208216824730357, -3.795296366450302550 ) ) ;
#76467 = ORIENTED_EDGE ( 'NONE', *, *, #35977, .F. ) ;
#76468 = CARTESIAN_POINT ( 'NONE',  ( 24.16423886937410614, 19.30374883491397142, 8.672049930838204340E-16 ) ) ;
#76469 = CARTESIAN_POINT ( 'NONE',  ( 10.00000000000000000, 61.81368534415484106, -10.88017736071110342 ) ) ;
#76470 = CARTESIAN_POINT ( 'NONE',  ( 34.56412365047464874, 28.99999999999999645, 10.00000000000000000 ) ) ;
#76471 = CARTESIAN_POINT ( 'NONE',  ( 24.16423886937410614, 54.51208216824730357, -3.795296366450302550 ) ) ;
#76472 = CARTESIAN_POINT ( 'NONE',  ( 19.38216949554541557, 17.24863466993041783, -9.382169495545420901 ) ) ;
#76473 = DIRECTION ( 'NONE',  ( 0.000000000000000000, 0.000000000000000000, -1.000000000000000000 ) ) ;
#76474 = CARTESIAN_POINT ( 'NONE',  ( 4.559911319644449179, 68.89701867748817676, 9.422509992056141925 ) ) ;
#76475 = CARTESIAN_POINT ( 'NONE',  ( -0.7375392941519102186, 14.49999999999999112, 14.98185688723476616 ) ) ;
#76476 = CARTESIAN_POINT ( 'NONE',  ( 9.879999999999988347, 26.99999999999999645, -2.900000000000000799 ) ) ;
#76477 = CARTESIAN_POINT ( 'NONE',  ( 3.591859063236763294, 33.29030133659708213, -11.09922568453595026 ) ) ;
#76478 = CARTESIAN_POINT ( 'NONE',  ( 2.917880565312950480, 60.97041550158063927, -12.26659068614894821 ) ) ;
#76479 = LINE ( 'NONE', #7993, #65555 ) ;
#76480 = CARTESIAN_POINT ( 'NONE',  ( 10.00000000000000000, 31.81368534415483751, -10.88017736071110342 ) ) ;
#76481 = CARTESIAN_POINT ( 'NONE',  ( 20.88017736071110875, 20.77201867748816611, -2.915334737309920765 ) ) ;
#76482 = CARTESIAN_POINT ( 'NONE',  ( 0.1532563361054100626, 55.80059781766745175, -2.638427012816831230 ) ) ;
#76483 = CARTESIAN_POINT ( 'NONE',  ( 7.361572987183169658, 59.96726448433410894, -9.846743663894592657 ) ) ;
#76484 = CARTESIAN_POINT ( 'NONE',  ( -2.816281873526473856, 54.33196800326376064, 3.434112377981055619 ) ) ;
#76485 = DIRECTION ( 'NONE',  ( 0.000000000000000000, 0.000000000000000000, 1.000000000000000000 ) ) ;
#76486 = EDGE_LOOP ( 'NONE', ( #86140, #69038, #16645, #48465, #69023, #2091 ) ) ;
#76487 = AXIS2_PLACEMENT_3D ( 'NONE', #25149, #33103, #33586 ) ;
#76488 = CARTESIAN_POINT ( 'NONE',  ( 4.559911319644449179, 13.89701867748817143, 9.422509992056141925 ) ) ;
#76489 = CARTESIAN_POINT ( 'NONE',  ( 0.6178305044545818747, 23.49863466993041783, -9.382169495545419124 ) ) ;
#76490 = CARTESIAN_POINT ( 'NONE',  ( 20.15039907845753575, 39.72266099184919597, 6.262539305110075283 ) ) ;
#76491 = AXIS2_PLACEMENT_3D ( 'NONE', #8400, #98942, #54378 ) ;
#76492 = CARTESIAN_POINT ( 'NONE',  ( 1.472469842513823179, 51.42559781766745886, 4.923371831947296329 ) ) ;
#76493 = CARTESIAN_POINT ( 'NONE',  ( 20.88017736071110875, 55.77201867748816966, -2.915334737309920765 ) ) ;
#76494 = CARTESIAN_POINT ( 'NONE',  ( 19.38216949554541557, 22.24863466993041428, -9.382169495545420901 ) ) ;
#76496 = CARTESIAN_POINT ( 'NONE',  ( 8.630000000000000782, 1.019547802438458550, -3.750000000000000000 ) ) ;
#76495 = CARTESIAN_POINT ( 'NONE',  ( 4.559911319644449179, 42.23035201082151247, -9.422509992056141925 ) ) ;
#76497 = CARTESIAN_POINT ( 'NONE',  ( 13.78891971893208357, 14.49999999999999822, -5.904717858191528279 ) ) ;
#76498 = CARTESIAN_POINT ( 'NONE',  ( 0.6178305044545838731, 49.74863466993041072, 9.382169495545420901 ) ) ;
#76499 = ORIENTED_EDGE ( 'NONE', *, *, #19629, .T. ) ;
#76500 = DIRECTION ( 'NONE',  ( -0.06975647374412544122, -0.9975640502598241977, -0.000000000000000000 ) ) ;
#76501 = CARTESIAN_POINT ( 'NONE',  ( 19.42250999205614193, 50.14701867748817676, 5.440088680355555262 ) ) ;
#76503 = CARTESIAN_POINT ( 'NONE',  ( 24.16423886937410614, 19.30374883491397142, 8.672049930838204340E-16 ) ) ;
#76502 = CARTESIAN_POINT ( 'NONE',  ( 22.81628187352647785, 41.41530133659708923, 3.434112377981063169 ) ) ;
#76504 = CARTESIAN_POINT ( 'NONE',  ( 10.00000000000000178, 7.258931151000785675, 9.846743663894594434 ) ) ;
#76505 = CARTESIAN_POINT ( 'NONE',  ( -0.1503990784575328643, 70.00000000000000000, -6.262539305110068177 ) ) ;
#76506 = CARTESIAN_POINT ( 'NONE',  ( 19.84674366389459266, 33.30059781766744464, 2.638427012816836559 ) ) ;
#76507 = CARTESIAN_POINT ( 'NONE',  ( 19.84674366389459266, 8.717264484334116048, -2.638427012816827677 ) ) ;
#76508 = DIRECTION ( 'NONE',  ( -0.000000000000000000, -0.000000000000000000, -1.000000000000000000 ) ) ;
#76509 = CARTESIAN_POINT ( 'NONE',  ( -0.3689425029237881626, 37.42874883491396787, 10.36894250292379027 ) ) ;
#76510 = CARTESIAN_POINT ( 'NONE',  ( 12.91533473730992121, 14.52201867748817143, 10.88017736071110164 ) ) ;
#76511 = DIRECTION ( 'NONE',  ( -0.000000000000000000, -1.000000000000000000, -0.000000000000000000 ) ) ;
#76512 = ORIENTED_EDGE ( 'NONE', *, *, #21963, .T. ) ;
#76513 = CARTESIAN_POINT ( 'NONE',  ( 17.96484262340118221, 14.93868534415484106, 7.964842623401181321 ) ) ;
#76514 = CARTESIAN_POINT ( 'NONE',  ( 19.42250999205614548, 10.98035201082150536, -5.440088680355545492 ) ) ;
#76515 = CARTESIAN_POINT ( 'NONE',  ( 0.1532563361054083140, 41.00893115100078745, 1.131784320476157264E-15 ) ) ;
#76516 = B_SPLINE_CURVE_WITH_KNOTS ( 'NONE', 3,
 ( #34393, #57400, #2472, #86921, #71443, #1971 ),
 .UNSPECIFIED., .F., .F.,
 ( 4, 2, 4 ),
 ( 3.409110551494654820E-05, 0.0004400426677367926431, 0.0008459942299586388059 ),
 .UNSPECIFIED. ) ;
#76517 = CARTESIAN_POINT ( 'NONE',  ( 21.09922568453594849, 36.20696800326375353, 6.408140936763242479 ) ) ;
#76519 = CARTESIAN_POINT ( 'NONE',  ( -4.164238869374099039, 11.80374883491396965, 8.674139862899312516E-16 ) ) ;
#76518 = CARTESIAN_POINT ( 'NONE',  ( 3.866352809135573221, 14.95037102884062996, 14.23757791217548707 ) ) ;
#76520 = CARTESIAN_POINT ( 'NONE',  ( 2.035157376598822676, 32.43868534415483396, -7.964842623401177768 ) ) ;
#76521 = CARTESIAN_POINT ( 'NONE',  ( 10.00000000000000000, 65.55374883491396076, -14.16423886937410082 ) ) ;
#76522 = CARTESIAN_POINT ( 'NONE',  ( 0.1532563361054083140, 41.00893115100078745, 1.131784320476157264E-15 ) ) ;
#76523 = CARTESIAN_POINT ( 'NONE',  ( 8.564643372776551189, 14.49999999999999112, 12.31449893000752915 ) ) ;
#76524 = CARTESIAN_POINT ( 'NONE',  ( 1.472469842513823179, 21.42559781766745175, 4.923371831947296329 ) ) ;
#76525 = DIRECTION ( 'NONE',  ( 0.000000000000000000, 0.000000000000000000, -1.000000000000000000 ) ) ;
#76526 = CARTESIAN_POINT ( 'NONE',  ( -6.408140936763232709, -40.04303199673623936, 11.09922568453595026 ) ) ;
#76527 = ORIENTED_EDGE ( 'NONE', *, *, #17730, .T. ) ;
#76528 = VECTOR ( 'NONE', #21153, 1000.000000000000000 ) ;
#76529 = DIRECTION ( 'NONE',  ( -0.9914448613738112703, 0.000000000000000000, 0.1305261922200445235 ) ) ;
#76530 = VERTEX_POINT ( 'NONE', #10808 ) ;
#76531 = CARTESIAN_POINT ( 'NONE',  ( 5.076628168052703671, 51.84226448433412315, 8.527530157486179263 ) ) ;
#76533 = CARTESIAN_POINT ( 'NONE',  ( 10.00000000000000178, 39.31368534415484106, 10.88017736071110342 ) ) ;
#76532 = CARTESIAN_POINT ( 'NONE',  ( 0.5774900079438590739, 32.64701867748816966, -5.440088680355550821 ) ) ;
#76535 = CARTESIAN_POINT ( 'NONE',  ( 19.38216949554541202, 30.99863466993042138, 9.382169495545424454 ) ) ;
#76534 =( NAMED_UNIT ( * ) SI_UNIT ( $, .STERADIAN. ) SOLID_ANGLE_UNIT ( ) );
#76536 = CARTESIAN_POINT ( 'NONE',  ( -2.266590686148945544, 22.22041550158063572, 7.082119434687048631 ) ) ;
#76537 = ADVANCED_FACE ( 'NONE', ( #63783 ), #11289, .F. ) ;
#76538 = CARTESIAN_POINT ( 'NONE',  ( 16.40814093676323893, 50.79030133659708923, 11.09922568453595026 ) ) ;
#76539 = VERTEX_POINT ( 'NONE', #94292 ) ;
#76540 = CARTESIAN_POINT ( 'NONE',  ( 7.361572987183169658, 44.96726448433412315, -9.846743663894592657 ) ) ;
#76541 = CARTESIAN_POINT ( 'NONE',  ( 10.00000000000000178, 24.31368534415484106, 10.88017736071110342 ) ) ;
#76542 = EDGE_LOOP ( 'NONE', ( #7661, #59203, #44137, #46778 ) ) ;
#76543 = CARTESIAN_POINT ( 'NONE',  ( 4.559911319644449179, 17.23035201082150536, -9.422509992056141925 ) ) ;
#76544 = VERTEX_POINT ( 'NONE', #70832 ) ;
#76545 = CARTESIAN_POINT ( 'NONE',  ( 17.96484262340118221, 56.18868534415484817, -7.964842623401177768 ) ) ;
#76546 = SURFACE_STYLE_USAGE ( .BOTH. , #9528 ) ;
#76547 = CARTESIAN_POINT ( 'NONE',  ( 18.72515096720570327, 6.072280503510315341, -6.499999999999985789 ) ) ;
#76548 = CARTESIAN_POINT ( 'NONE',  ( -0.8801773607111008646, 53.27201867748816966, 2.915334737309923430 ) ) ;
#76549 = CARTESIAN_POINT ( 'NONE',  ( -0.3289641300568005855, 29.27164270246084143, -5.963430220938281678 ) ) ;
#76550 = CARTESIAN_POINT ( 'NONE',  ( -46.48928645636214441, 103.2957187381728232, 6.397878122523972699 ) ) ;
#76552 = EDGE_LOOP ( 'NONE', ( #17378, #33423, #95078, #44644 ) ) ;
#76551 = DIRECTION ( 'NONE',  ( 0.7716245833877192206, 0.000000000000000000, -0.6360782202777647276 ) ) ;
#76553 = EDGE_CURVE ( 'NONE', #7375, #86520, #40818, .T. ) ;
#76554 = CARTESIAN_POINT ( 'NONE',  ( 0.1532563361054082862, 41.21726448433411605, 2.638427012816831674 ) ) ;
#76555 = ORIENTED_EDGE ( 'NONE', *, *, #15758, .T. ) ;
#76556 = CARTESIAN_POINT ( 'NONE',  ( 7.361572987183170547, 67.05059781766746596, 9.846743663894590881 ) ) ;
#76557 = B_SPLINE_CURVE_WITH_KNOTS ( 'NONE', 3,
 ( #90604, #82119, #143, #58634, #81624, #43629 ),
 .UNSPECIFIED., .F., .F.,
 ( 4, 2, 4 ),
 ( 3.409110551496222848E-05, 0.0004400426677368007205, 0.0008459942299586391311 ),
 .UNSPECIFIED. ) ;
#76558 = B_SPLINE_CURVE_WITH_KNOTS ( 'NONE', 3,
 ( #6765, #7267, #82253, #37278, #45249, #75745 ),
 .UNSPECIFIED., .F., .F.,
 ( 4, 2, 4 ),
 ( 0.000000000000000000, 0.0002626113303184730917, 0.0005252226606369461833 ),
 .UNSPECIFIED. ) ;
#76559 = VECTOR ( 'NONE', #73392, 1000.000000000000000 ) ;
#76560 = CARTESIAN_POINT ( 'NONE',  ( 20.36894250292379738, 24.92874883491396787, -10.36894250292379027 ) ) ;
#76561 = ORIENTED_EDGE ( 'NONE', *, *, #22957, .F. ) ;
#76562 = CARTESIAN_POINT ( 'NONE',  ( 4.879999999999994564, 43.00000000000000711, -4.250000000000000000 ) ) ;
#76564 = CARTESIAN_POINT ( 'NONE',  ( 4.559911319644449179, 57.23035201082150536, -9.422509992056141925 ) ) ;
#76563 = DIRECTION ( 'NONE',  ( 0.000000000000000000, -1.000000000000000000, 0.000000000000000000 ) ) ;
#76565 = CARTESIAN_POINT ( 'NONE',  ( 4.559911319644449179, 7.230352010821505360, -9.422509992056141925 ) ) ;
#76567 = EDGE_LOOP ( 'NONE', ( #61761, #66873, #83175, #31919 ) ) ;
#76566 = CARTESIAN_POINT ( 'NONE',  ( 0.6178305044545818747, 38.49863466993042493, -9.382169495545419124 ) ) ;
#76568 = DIRECTION ( 'NONE',  ( 0.000000000000000000, 0.000000000000000000, 1.000000000000000000 ) ) ;
#76569 = CARTESIAN_POINT ( 'NONE',  ( 10.00000000000000000, 27.87363466993042138, -12.81628187352647608 ) ) ;
#76570 = CARTESIAN_POINT ( 'NONE',  ( 12.63842701281683922, 24.55059781766745175, -9.846743663894590881 ) ) ;
#76571 = DIRECTION ( 'NONE',  ( -0.9366721892483995671, 0.000000000000000000, 0.3502073812594621027 ) ) ;
#76572 = CARTESIAN_POINT ( 'NONE',  ( 19.38216949554541557, 17.24863466993041783, -9.382169495545420901 ) ) ;
#76573 = CARTESIAN_POINT ( 'NONE',  ( 64.56412365047461321, 44.99999999999998579, -7.000000000000000000 ) ) ;
#76574 = CARTESIAN_POINT ( 'NONE',  ( 19.84674366389459266, 3.300597817667451750, 2.638427012816836559 ) ) ;
#76575 = ORIENTED_EDGE ( 'NONE', *, *, #91912, .T. ) ;
#76576 = VERTEX_POINT ( 'NONE', #57277 ) ;
#76577 = CARTESIAN_POINT ( 'NONE',  ( 2.035157376598824452, 18.68868534415484106, 7.964842623401179544 ) ) ;
#76578 = CARTESIAN_POINT ( 'NONE',  ( 24.16423886937409904, 24.09541550158063927, 3.795296366450317205 ) ) ;
#76579 = CARTESIAN_POINT ( 'NONE',  ( 12.63842701281683922, 34.55059781766745886, -9.846743663894590881 ) ) ;
#76580 = CARTESIAN_POINT ( 'NONE',  ( 15.44008868035555260, 64.73035201082151957, 9.422509992056143702 ) ) ;
#76582 = CARTESIAN_POINT ( 'NONE',  ( -7.118731320094870973, -71.92838106472885329, -2.750000000000000444 ) ) ;
#76581 = CARTESIAN_POINT ( 'NONE',  ( 21.09922568453594849, 46.20696800326376064, 6.408140936763242479 ) ) ;
#76583 = CARTESIAN_POINT ( 'NONE',  ( 12.91533473730992121, 19.52201867748816611, 10.88017736071110164 ) ) ;
#76584 = DIRECTION ( 'NONE',  ( 1.000000000000000000, 0.000000000000000000, 0.000000000000000000 ) ) ;
#76585 = STYLED_ITEM ( 'NONE', ( #71784 ), #5038 ) ;
#76586 = EDGE_CURVE ( 'NONE', #68599, #35522, #69079, .T. ) ;
#76587 = CARTESIAN_POINT ( 'NONE',  ( 19.38216949554541557, 12.24863466993041961, -9.382169495545420901 ) ) ;
#76588 = CARTESIAN_POINT ( 'NONE',  ( -2.816281873526471635, 13.91530133659708746, -3.434112377981056508 ) ) ;
#76589 = CARTESIAN_POINT ( 'NONE',  ( 18.52753015748617571, 28.09226448433411960, 4.923371831947298993 ) ) ;
#76590 = CARTESIAN_POINT ( 'NONE',  ( 10.88017736071110164, -14.64464798917848753, 2.915334737309921209 ) ) ;
#76591 = CARTESIAN_POINT ( 'NONE',  ( 21.09922568453595559, 32.04030133659708923, -6.408140936763230044 ) ) ;
#76592 = CARTESIAN_POINT ( 'NONE',  ( 17.84635730667656262, 23.63791097397319518, 6.500000000000021316 ) ) ;
#76594 = CARTESIAN_POINT ( 'NONE',  ( 11.62719953690064933, 0.5000000000000004441, -9.476720473301794456 ) ) ;
#76593 = CARTESIAN_POINT ( 'NONE',  ( 4.559911319644449179, 58.89701867748817676, 9.422509992056141925 ) ) ;
#76595 = COLOUR_RGB ( '', 0.40784314, 0.44705882, 0.49803922) ;
#76596 = EDGE_CURVE ( 'NONE', #87174, #26702, #59743, .T. ) ;
#76597 = LINE ( 'NONE', #38609, #5042 ) ;
#76598 = CARTESIAN_POINT ( 'NONE',  ( 18.06765999051784988, 28.99127512925449324, 6.500000000000019540 ) ) ;
#76599 = CARTESIAN_POINT ( 'NONE',  ( -0.8801773607111009756, 43.06368534415484106, 1.068504757029289695E-15 ) ) ;
#76600 = CARTESIAN_POINT ( 'NONE',  ( 0.5774900079438607392, 48.48035201082150536, 5.440088680355550821 ) ) ;
#76601 = DIRECTION ( 'NONE',  ( 0.000000000000000000, -1.000000000000000000, 0.000000000000000000 ) ) ;
#76602 = AXIS2_PLACEMENT_3D ( 'NONE', #15602, #84580, #47557 ) ;
#76603 = CARTESIAN_POINT ( 'NONE',  ( -0.1298530154764001854, 80.39370036920264795, 9.500000000000000000 ) ) ;
#76604 = CARTESIAN_POINT ( 'NONE',  ( 14.92337183194729633, 47.67559781766745175, 8.527530157486181039 ) ) ;
#76606 = CARTESIAN_POINT ( 'NONE',  ( 19.84674366389459266, 23.30059781766745530, 2.638427012816836559 ) ) ;
#76605 = CARTESIAN_POINT ( 'NONE',  ( -0.8801773607111009756, 13.06368534415483929, 1.068504757029289695E-15 ) ) ;
#76607 = CARTESIAN_POINT ( 'NONE',  ( 21.09922568453594849, 11.20696800326375531, 6.408140936763242479 ) ) ;
#76608 = ORIENTED_EDGE ( 'NONE', *, *, #45168, .F. ) ;
#76609 = CARTESIAN_POINT ( 'NONE',  ( 4.559911319644449179, 42.23035201082151247, -9.422509992056141925 ) ) ;
#76610 = EDGE_CURVE ( 'NONE', #72980, #41390, #41968, .T. ) ;
#76612 = LINE ( 'NONE', #8128, #34965 ) ;
#76611 = CARTESIAN_POINT ( 'NONE',  ( 7.361572987183169658, 64.96726448433412315, -9.846743663894592657 ) ) ;
#76613 = CARTESIAN_POINT ( 'NONE',  ( 2.035157376598822676, 7.438685344154837509, -7.964842623401177768 ) ) ;
#76614 = CARTESIAN_POINT ( 'NONE',  ( -0.8801773607111009756, 23.06368534415484106, 1.068504757029289695E-15 ) ) ;
#76615 = CARTESIAN_POINT ( 'NONE',  ( 22.26659068614895176, 34.72041550158063927, -7.082119434687042414 ) ) ;
#76616 = CARTESIAN_POINT ( 'NONE',  ( 19.84674366389459266, 33.30059781766744464, 2.638427012816836559 ) ) ;
#76617 = CARTESIAN_POINT ( 'NONE',  ( 0.5774900079438607392, 48.48035201082150536, 5.440088680355550821 ) ) ;
#76618 = CARTESIAN_POINT ( 'NONE',  ( -4.164238869374098151, 1.595415501580634388, -3.795296366450310543 ) ) ;
#76619 = CARTESIAN_POINT ( 'NONE',  ( 14.04391541078762984, 15.00000000000000000, -3.608107528142820986 ) ) ;
#76620 = CARTESIAN_POINT ( 'NONE',  ( 7.361572987183170547, 62.05059781766745886, 9.846743663894590881 ) ) ;
#76621 = VERTEX_POINT ( 'NONE', #75243 ) ;
#76622 = VERTEX_POINT ( 'NONE', #36764 ) ;
#76623 = CARTESIAN_POINT ( 'NONE',  ( -0.3689425029237898834, 41.17874883491397497, -10.36894250292378850 ) ) ;
#76624 = CARTESIAN_POINT ( 'NONE',  ( 17.08211943468705130, 28.47041550158063572, 12.26659068614894998 ) ) ;
#76625 = CARTESIAN_POINT ( 'NONE',  ( 5.076628168052703671, 1.842264484334118047, 8.527530157486179263 ) ) ;
#76626 = CARTESIAN_POINT ( 'NONE',  ( 16.40814093676323893, 10.79030133659708923, 11.09922568453595026 ) ) ;
#76627 = CARTESIAN_POINT ( 'NONE',  ( 1.472469842513823179, 56.42559781766745886, 4.923371831947296329 ) ) ;
#76628 = CARTESIAN_POINT ( 'NONE',  ( -11.05191079938102128, -57.06817940849487059, 4.000000000000000000 ) ) ;
#76630 = CARTESIAN_POINT ( 'NONE',  ( -2.816281873526471635, 13.91530133659708746, -3.434112377981056508 ) ) ;
#76629 = CARTESIAN_POINT ( 'NONE',  ( 7.084665262690076126, 57.02201867748817676, -10.88017736071110164 ) ) ;
#76631 = CARTESIAN_POINT ( 'NONE',  ( -4.164238869374098151, 26.59541550158063217, -3.795296366450310543 ) ) ;
#76632 = CARTESIAN_POINT ( 'NONE',  ( 19.42250999205614548, 10.98035201082150536, -5.440088680355545492 ) ) ;
#76633 = CARTESIAN_POINT ( 'NONE',  ( 20.88017736071110164, 30.35535201082151247, 2.915334737309930979 ) ) ;
#76634 = DIRECTION ( 'NONE',  ( 0.000000000000000000, 1.000000000000000000, 0.000000000000000000 ) ) ;
#76635 = CARTESIAN_POINT ( 'NONE',  ( 15.44008868035555793, 51.39701867748816966, -9.422509992056140149 ) ) ;
#76636 = CARTESIAN_POINT ( 'NONE',  ( 16.40814093676324603, 52.45696800326375353, -11.09922568453594671 ) ) ;
#76637 = CARTESIAN_POINT ( 'NONE',  ( -9.846743663894590881, -23.78273551566588395, 2.638427012816840111 ) ) ;
#76638 = ORIENTED_EDGE ( 'NONE', *, *, #98965, .T. ) ;
#76639 = PLANE ( 'NONE',  #74763 ) ;
#76640 = AXIS2_PLACEMENT_3D ( 'NONE', #33242, #54759, #9774 ) ;
#76641 = ORIENTED_EDGE ( 'NONE', *, *, #15283, .T. ) ;
#76642 = FACE_OUTER_BOUND ( 'NONE', #18876, .T. ) ;
#76644 = CARTESIAN_POINT ( 'NONE',  ( -2.266590686148945544, 66.38708216824730357, -7.082119434687050408 ) ) ;
#76643 = CARTESIAN_POINT ( 'NONE',  ( 20.36894250292379738, 54.92874883491396076, -10.36894250292379027 ) ) ;
#76646 = CARTESIAN_POINT ( 'NONE',  ( 18.52753015748618282, 63.92559781766745886, -4.923371831947291888 ) ) ;
#76645 = CARTESIAN_POINT ( 'NONE',  ( 18.52753015748617571, 18.09226448433411960, 4.923371831947298993 ) ) ;
#76647 = CARTESIAN_POINT ( 'NONE',  ( 0.000000000000000000, 0.5000000000000004441, 0.000000000000000000 ) ) ;
#76648 = AXIS2_PLACEMENT_3D ( 'NONE', #12451, #33951, #88947 ) ;
#76649 = EDGE_CURVE ( 'NONE', #75439, #90631, #83497, .T. ) ;
#76650 = ADVANCED_FACE ( 'NONE', ( #5773 ), #81745, .F. ) ;
#76651 = CARTESIAN_POINT ( 'NONE',  ( 16.40814093676324603, 2.456968003263753531, -11.09922568453594671 ) ) ;
#76652 = CARTESIAN_POINT ( 'NONE',  ( 12.81628187352647252, 21.83196800326374643, -3.434112377981059172 ) ) ;
#76653 = ORIENTED_EDGE ( 'NONE', *, *, #53491, .T. ) ;
#76654 = CARTESIAN_POINT ( 'NONE',  ( -4.164238869374099927, 37.01208216824731068, 3.795296366450308767 ) ) ;
#76655 = CARTESIAN_POINT ( 'NONE',  ( 20.36894250292379738, 49.92874883491396787, -10.36894250292379027 ) ) ;
#76656 = ORIENTED_EDGE ( 'NONE', *, *, #21238, .T. ) ;
#76657 = CARTESIAN_POINT ( 'NONE',  ( -2.816281873526473856, 59.12363466993042493, 9.499525473075851096E-16 ) ) ;
#76658 = CIRCLE ( 'NONE', #46333, 0.2500000000000002220 ) ;
#76659 = CARTESIAN_POINT ( 'NONE',  ( 12.91533473730992121, 29.52201867748817321, 10.88017736071110164 ) ) ;
#76660 = CARTESIAN_POINT ( 'NONE',  ( 14.92337183194729988, 49.34226448433411605, -8.527530157486177487 ) ) ;
#76661 = CARTESIAN_POINT ( 'NONE',  ( 20.88017736071110164, 20.35535201082150891, 2.915334737309930979 ) ) ;
#76662 = ADVANCED_FACE ( 'NONE', ( #51261 ), #73264, .F. ) ;
#76663 = CARTESIAN_POINT ( 'NONE',  ( 14.91937968691865457, 14.76930270348881180, -0.8063277559918125004 ) ) ;
#76664 = CARTESIAN_POINT ( 'NONE',  ( 2.791683348922237240, 50.38393115100078035, -7.208316651077763204 ) ) ;
#76665 = CARTESIAN_POINT ( 'NONE',  ( 17.20831665107776587, 54.13393115100079456, -7.208316651077762316 ) ) ;
#76667 = ORIENTED_EDGE ( 'NONE', *, *, #95856, .F. ) ;
#76666 = CARTESIAN_POINT ( 'NONE',  ( -6.689969769698787871, 15.00000000000000000, -12.58200319823979285 ) ) ;
#76668 = ADVANCED_FACE ( 'NONE', ( #67257 ), #90238, .F. ) ;
#76669 = CARTESIAN_POINT ( 'NONE',  ( 0.000000000000000000, 0.5000000000000004441, 0.000000000000000000 ) ) ;
#76670 = CARTESIAN_POINT ( 'NONE',  ( 14.92337183194729988, 4.342264484334117824, -8.527530157486177487 ) ) ;
#76671 = CARTESIAN_POINT ( 'NONE',  ( 18.29284471827480729, 60.40189080397281884, -6.499999999999946709 ) ) ;
#76672 = ORIENTED_EDGE ( 'NONE', *, *, #28457, .F. ) ;
#76673 = CARTESIAN_POINT ( 'NONE',  ( 18.52753015748617571, 33.09226448433411605, 4.923371831947298993 ) ) ;
#76674 = CARTESIAN_POINT ( 'NONE',  ( 0.000000000000000000, 14.49999999999999822, 0.000000000000000000 ) ) ;
#76675 = CARTESIAN_POINT ( 'NONE',  ( 21.09922568453595559, 42.04030133659708213, -6.408140936763230044 ) ) ;
#76676 = EDGE_CURVE ( 'NONE', #29627, #90281, #86636, .T. ) ;
#76677 = CARTESIAN_POINT ( 'NONE',  ( 0.000000000000000000, 15.00000000000000000, 0.000000000000000000 ) ) ;
#76678 = ORIENTED_EDGE ( 'NONE', *, *, #72341, .T. ) ;
#76679 = CARTESIAN_POINT ( 'NONE',  ( 5.076628168052704559, 65.17559781766745175, -8.527530157486179263 ) ) ;
#76680 = DIRECTION ( 'NONE',  ( 0.000000000000000000, 1.000000000000000000, 0.000000000000000000 ) ) ;
#76681 = CARTESIAN_POINT ( 'NONE',  ( 5.076628168052704559, 50.17559781766745886, -8.527530157486179263 ) ) ;
#76682 = CARTESIAN_POINT ( 'NONE',  ( -2.266590686148945544, 37.22041550158063217, 7.082119434687048631 ) ) ;
#76683 = CARTESIAN_POINT ( 'NONE',  ( 7.361572987183169658, 59.96726448433410894, -9.846743663894592657 ) ) ;
#76684 = CARTESIAN_POINT ( 'NONE',  ( 0.4195498155886434599, -2.441190589077521466E-17, 9.500000000000000000 ) ) ;
#76685 = CARTESIAN_POINT ( 'NONE',  ( 14.92337183194729988, 14.34226448433411782, -8.527530157486177487 ) ) ;
#76686 = CARTESIAN_POINT ( 'NONE',  ( 0.6178305044545818747, 53.49863466993041072, -9.382169495545419124 ) ) ;
#76687 = CARTESIAN_POINT ( 'NONE',  ( 7.361572987183170547, 42.05059781766745886, 9.846743663894590881 ) ) ;
#76688 = CARTESIAN_POINT ( 'NONE',  ( 4.559911319644449179, 47.23035201082150536, -9.422509992056141925 ) ) ;
#76689 = CARTESIAN_POINT ( 'NONE',  ( 19.84674366389459266, 38.30059781766745175, 2.638427012816836559 ) ) ;
#76690 = CARTESIAN_POINT ( 'NONE',  ( 0.7375392941518169598, 0.3639308982088801936, -14.98185688723474307 ) ) ;
#76691 = STYLED_ITEM ( 'NONE', ( #82763 ), #66347 ) ;
#76692 = B_SPLINE_CURVE_WITH_KNOTS ( 'NONE', 3,
 ( #89970, #12006, #21486, #13992, #44467, #74969, #6474, #60457, #45962, #7967, #965, #22477 ),
 .UNSPECIFIED., .F., .F.,
 ( 4, 2, 2, 2, 2, 4 ),
 ( 3.878959614448864246E-18, 4.389529495108911855E-05, 8.779058990217436108E-05, 0.0001755811798043448461, 0.0003511623596086858434, 0.0007023247192173684341 ),
 .UNSPECIFIED. ) ;
#76693 = CARTESIAN_POINT ( 'NONE',  ( 20.88017736071110875, 60.77201867748817676, -2.915334737309920765 ) ) ;
#76694 = EDGE_LOOP ( 'NONE', ( #41215, #39206, #26497, #96599, #2911, #36739 ) ) ;
#76695 = DIRECTION ( 'NONE',  ( 0.000000000000000000, -1.000000000000000000, 0.000000000000000000 ) ) ;
#76696 = CARTESIAN_POINT ( 'NONE',  ( 0.5774900079438590739, 22.64701867748817321, -5.440088680355550821 ) ) ;
#76697 = CIRCLE ( 'NONE', #30374, 15.00000000000000000 ) ;
#76699 = CARTESIAN_POINT ( 'NONE',  ( 17.96484262340118221, 54.93868534415484106, 7.964842623401181321 ) ) ;
#76698 = CARTESIAN_POINT ( 'NONE',  ( 19.38216949554541202, 0.9986346699304200492, 9.382169495545424454 ) ) ;
#76700 =( NAMED_UNIT ( * ) PLANE_ANGLE_UNIT ( ) SI_UNIT ( $, .RADIAN. ) );
#76701 = CARTESIAN_POINT ( 'NONE',  ( 17.39651004071841456, 14.08210964143329669, -6.500000000000003553 ) ) ;
#76702 = CARTESIAN_POINT ( 'NONE',  ( 20.15039907845753220, 24.72266099184919241, 6.262539305110077947 ) ) ;
#76704 = CARTESIAN_POINT ( 'NONE',  ( 5.093587308868497310, -0.03417435944610275333, -15.16353404595997567 ) ) ;
#76703 = CARTESIAN_POINT ( 'NONE',  ( -0.8801773607111009756, 43.06368534415484106, 1.068504757029289695E-15 ) ) ;
#76705 = CARTESIAN_POINT ( 'NONE',  ( 0.1532563361054083140, 41.00893115100078745, 1.131784320476157264E-15 ) ) ;
#76706 = CARTESIAN_POINT ( 'NONE',  ( 13.99999999999999822, 60.50000000000000711, -6.500000000000000888 ) ) ;
#76707 = CARTESIAN_POINT ( 'NONE',  ( -14.16423886937410082, 21.80374883491398208, 4.336808689942017736E-15 ) ) ;
#76708 = CARTESIAN_POINT ( 'NONE',  ( 1.472469842513823179, 60.59226448433412315, -4.923371831947296329 ) ) ;
#76709 = AXIS2_PLACEMENT_3D ( 'NONE', #79243, #79739, #11236 ) ;
#76710 = CARTESIAN_POINT ( 'NONE',  ( -0.8801773607110991993, 12.85535201082150358, -2.915334737309923874 ) ) ;
#76711 = LINE ( 'NONE', #60232, #72095 ) ;
#76712 = CARTESIAN_POINT ( 'NONE',  ( -4.164238869374099039, 21.80374883491396787, 8.674139862899312516E-16 ) ) ;
#76713 = EDGE_CURVE ( 'NONE', #105, #60118, #4787, .T. ) ;
#76714 = CARTESIAN_POINT ( 'NONE',  ( 13.79529636645031943, 55.34541550158062506, -14.16423886937409904 ) ) ;
#76715 = CARTESIAN_POINT ( 'NONE',  ( 18.52753015748618282, 33.92559781766745886, -4.923371831947291888 ) ) ;
#76716 = CARTESIAN_POINT ( 'NONE',  ( 7.361572987183170547, 17.05059781766745530, 9.846743663894590881 ) ) ;
#76717 = CARTESIAN_POINT ( 'NONE',  ( 10.00000000000000000, 6.813685344154838397, -10.88017736071110342 ) ) ;
#76718 = ORIENTED_EDGE ( 'NONE', *, *, #55889, .T. ) ;
#76719 = CARTESIAN_POINT ( 'NONE',  ( 1.472469842513823179, 31.42559781766745530, 4.923371831947296329 ) ) ;
#76720 = CARTESIAN_POINT ( 'NONE',  ( 20.88017736071110164, 25.35535201082150891, 2.915334737309930979 ) ) ;
#76721 = CARTESIAN_POINT ( 'NONE',  ( 19.84674366389459266, 58.30059781766745886, 2.638427012816836559 ) ) ;
#76722 = CARTESIAN_POINT ( 'NONE',  ( 24.16423886937409904, 14.09541550158063217, 3.795296366450317205 ) ) ;
#76723 = DIRECTION ( 'NONE',  ( 0.000000000000000000, 0.000000000000000000, -1.000000000000000000 ) ) ;
#76724 = CARTESIAN_POINT ( 'NONE',  ( 14.92337183194729988, 14.34226448433411782, -8.527530157486177487 ) ) ;
#76725 = CARTESIAN_POINT ( 'NONE',  ( 13.43411237798106583, 42.66530133659707502, -12.81628187352647252 ) ) ;
#76726 = CARTESIAN_POINT ( 'NONE',  ( 7.361572987183169658, 34.96726448433411605, -9.846743663894592657 ) ) ;
#76727 = VERTEX_POINT ( 'NONE', #44246 ) ;
#76728 = CARTESIAN_POINT ( 'NONE',  ( 5.076628168052703671, 26.84226448433411960, 8.527530157486179263 ) ) ;
#76729 = CARTESIAN_POINT ( 'NONE',  ( 11.01507687203709018, -96.09620168234333448, -4.000000000000224709 ) ) ;
#76730 = DIRECTION ( 'NONE',  ( -0.000000000000000000, 1.000000000000000000, 0.000000000000000000 ) ) ;
#76731 = CARTESIAN_POINT ( 'NONE',  ( 17.08211943468705130, 53.47041550158063217, 12.26659068614894998 ) ) ;
#76732 = CARTESIAN_POINT ( 'NONE',  ( -0.8801773607111009756, 48.06368534415484817, 1.068504757029289695E-15 ) ) ;
#76733 = AXIS2_PLACEMENT_3D ( 'NONE', #10079, #61097, #91607 ) ;
#76734 = CARTESIAN_POINT ( 'NONE',  ( 0.1532563361054100626, 30.80059781766744820, -2.638427012816831230 ) ) ;
#76735 = CARTESIAN_POINT ( 'NONE',  ( -0.8801773607110991993, 7.855352010821504471, -2.915334737309923874 ) ) ;
#76736 = CARTESIAN_POINT ( 'NONE',  ( 18.61655166652078108, 39.87718327197428891, 6.499999999999962697 ) ) ;
#76737 = CARTESIAN_POINT ( 'NONE',  ( 10.00000000000000178, 52.25893115100078745, 9.846743663894594434 ) ) ;
#76738 = AXIS2_PLACEMENT_3D ( 'NONE', #91090, #22618, #91597 ) ;
#76739 = CARTESIAN_POINT ( 'NONE',  ( 19.42250999205614193, 55.14701867748817676, 5.440088680355555262 ) ) ;
#76740 = CARTESIAN_POINT ( 'NONE',  ( 1.472469842513823179, 1.425597817667451528, 4.923371831947296329 ) ) ;
#76741 = ORIENTED_EDGE ( 'NONE', *, *, #93607, .F. ) ;
#76742 = VERTEX_POINT ( 'NONE', #74750 ) ;
#76743 = AXIS2_PLACEMENT_3D ( 'NONE', #62159, #33623, #1698 ) ;
#76744 = DIRECTION ( 'NONE',  ( -1.000000000000000000, 0.000000000000000000, 0.000000000000000000 ) ) ;
#76745 = LINE ( 'NONE', #68280, #42866 ) ;
#76746 = CARTESIAN_POINT ( 'NONE',  ( 5.076628168052703671, 6.842264484334118713, 8.527530157486179263 ) ) ;
#76747 = CARTESIAN_POINT ( 'NONE',  ( 10.00000000000000000, 62.87363466993042493, -12.81628187352647608 ) ) ;
#76749 = CARTESIAN_POINT ( 'NONE',  ( 17.20831665107776587, 44.13393115100078745, -7.208316651077762316 ) ) ;
#76748 = CARTESIAN_POINT ( 'NONE',  ( 12.91533473730993009, 11.60535201082150714, -10.88017736071109987 ) ) ;
#76750 = CARTESIAN_POINT ( 'NONE',  ( 1.780824192092386404, 14.49999999999999112, 14.89391369643520946 ) ) ;
#76751 = CARTESIAN_POINT ( 'NONE',  ( 24.16423886937410614, 64.51208216824728936, -3.795296366450302550 ) ) ;
#76752 = CARTESIAN_POINT ( 'NONE',  ( 19.84674366389459266, 58.30059781766745886, 2.638427012816836559 ) ) ;
#76753 = EDGE_CURVE ( 'NONE', #43677, #87849, #10053, .T. ) ;
#76754 = CARTESIAN_POINT ( 'NONE',  ( 18.00000000000000000, 78.80384757729336798, 3.750000000000000444 ) ) ;
#76755 = CARTESIAN_POINT ( 'NONE',  ( 4.559911319644449179, 57.23035201082150536, -9.422509992056141925 ) ) ;
#76756 = CARTESIAN_POINT ( 'NONE',  ( 12.63842701281683034, 17.46726448433411250, 9.846743663894596210 ) ) ;
#76757 = CARTESIAN_POINT ( 'NONE',  ( -3.522141228383032452, -0.8488377519105255731, 3.750000000000201172 ) ) ;
#76758 = ORIENTED_EDGE ( 'NONE', *, *, #97928, .T. ) ;
#76759 = CARTESIAN_POINT ( 'NONE',  ( 20.24186590665275531, 30.59014588040357197, -6.114288769123077394 ) ) ;
#76760 = VERTEX_POINT ( 'NONE', #57766 ) ;
#76761 = CARTESIAN_POINT ( 'NONE',  ( 19.84674366389459266, 8.717264484334116048, -2.638427012816827677 ) ) ;
#76762 = EDGE_LOOP ( 'NONE', ( #47763, #17860, #84925, #21220, #90587, #1628 ) ) ;
#76763 = CARTESIAN_POINT ( 'NONE',  ( 17.08211943468705840, 20.13708216824730357, -12.26659068614894466 ) ) ;
#76764 = CARTESIAN_POINT ( 'NONE',  ( 10.00000000000000178, 17.25893115100078745, 9.846743663894594434 ) ) ;
#76765 = CARTESIAN_POINT ( 'NONE',  ( 2.035157376598824452, 28.68868534415484106, 7.964842623401179544 ) ) ;
#76766 = CARTESIAN_POINT ( 'NONE',  ( 7.002992508388946824, -3.201784540621254098E-15, 12.84003923133022695 ) ) ;
#76767 = VERTEX_POINT ( 'NONE', #97781 ) ;
#76768 = MECHANICAL_DESIGN_GEOMETRIC_PRESENTATION_REPRESENTATION (  '', ( #8116 ), #1845 ) ;
#76769 = CARTESIAN_POINT ( 'NONE',  ( -0.8801773607110991993, 27.85535201082150181, -2.915334737309923874 ) ) ;
#76770 = ADVANCED_FACE ( 'NONE', ( #14265 ), #3532, .T. ) ;
#76771 = EDGE_CURVE ( 'NONE', #90212, #21688, #91487, .T. ) ;
#76772 = ORIENTED_EDGE ( 'NONE', *, *, #54217, .T. ) ;
#76773 = CARTESIAN_POINT ( 'NONE',  ( 20.88017736071110875, 35.77201867748816966, -2.915334737309920765 ) ) ;
#76774 = CIRCLE ( 'NONE', #68795, 0.5000000000000004441 ) ;
#76775 = CARTESIAN_POINT ( 'NONE',  ( 1.046131998950040387, 65.73810908735725889, 6.499999999999984901 ) ) ;
#76776 = VERTEX_POINT ( 'NONE', #42096 ) ;
#76777 = CARTESIAN_POINT ( 'NONE',  ( 10.00000000000000000, 12.87363466993042138, -12.81628187352647608 ) ) ;
#76778 = CARTESIAN_POINT ( 'NONE',  ( 12.63842701281683922, 14.55059781766744997, -9.846743663894590881 ) ) ;
#76779 = FILL_AREA_STYLE ('',( #30778 ) ) ;
#76780 = CARTESIAN_POINT ( 'NONE',  ( 18.72515096720569616, 10.05509018479935968, 6.500000000000001776 ) ) ;
#76781 = CARTESIAN_POINT ( 'NONE',  ( 7.361572987183169658, 14.96726448433411960, -9.846743663894592657 ) ) ;
#76782 = CARTESIAN_POINT ( 'NONE',  ( 12.91533473730992121, 29.52201867748817321, 10.88017736071110164 ) ) ;
#76783 = ORIENTED_EDGE ( 'NONE', *, *, #28711, .T. ) ;
#76784 = ORIENTED_EDGE ( 'NONE', *, *, #96522, .T. ) ;
#76785 = CARTESIAN_POINT ( 'NONE',  ( 22.81628187352647785, 61.62363466993041783, 6.195893100308588602E-16 ) ) ;
#76786 = CARTESIAN_POINT ( 'NONE',  ( 20.88017736071110164, 60.35535201082151957, 2.915334737309930979 ) ) ;
#76787 = CARTESIAN_POINT ( 'NONE',  ( -0.3289641300567998083, 23.07879003517447103, 5.963430220938281678 ) ) ;
#76788 = CARTESIAN_POINT ( 'NONE',  ( -2.816281873526473856, 64.12363466993042493, 9.499525473075851096E-16 ) ) ;
#76789 = CARTESIAN_POINT ( 'NONE',  ( 4.559911319644449179, 62.23035201082150536, -9.422509992056141925 ) ) ;
#76790 = CARTESIAN_POINT ( 'NONE',  ( 21.09922568453594849, 1.206968003263753531, 6.408140936763242479 ) ) ;
#76791 = EDGE_CURVE ( 'NONE', #44200, #92170, #96079, .T. ) ;
#76792 = CARTESIAN_POINT ( 'NONE',  ( 66.76470751278411342, 44.99999999999998579, 10.00000000000000000 ) ) ;
#76793 = CARTESIAN_POINT ( 'NONE',  ( 0.1532563361054100626, 35.80059781766745175, -2.638427012816831230 ) ) ;
#76794 = CARTESIAN_POINT ( 'NONE',  ( -2.816281873526473856, 49.12363466993042493, 9.499525473075851096E-16 ) ) ;
#76795 = CARTESIAN_POINT ( 'NONE',  ( 0.000000000000000000, 14.49999999999999822, 0.000000000000000000 ) ) ;
#76796 = CARTESIAN_POINT ( 'NONE',  ( 1.472469842513823179, 15.59226448433411960, -4.923371831947296329 ) ) ;
#76797 = CARTESIAN_POINT ( 'NONE',  ( 13.43411237798105340, 20.58196800326374643, 12.81628187352647963 ) ) ;
#76799 = CARTESIAN_POINT ( 'NONE',  ( -5.069387707482587935, -24.96207253826403871, -2.750000000000001776 ) ) ;
#76798 = CARTESIAN_POINT ( 'NONE',  ( 14.56195259121204799, 6.403569081242508591E-16, -1.374002722866695336 ) ) ;
#76800 = CARTESIAN_POINT ( 'NONE',  ( 17.96484262340118221, 41.18868534415484106, -7.964842623401177768 ) ) ;
#76801 = CARTESIAN_POINT ( 'NONE',  ( 6.565887622018943937, 0.1653013365970866511, 12.81628187352647430 ) ) ;
#76802 = CARTESIAN_POINT ( 'NONE',  ( 1.472469842513823179, 25.59226448433412315, -4.923371831947296329 ) ) ;
#76803 = CARTESIAN_POINT ( 'NONE',  ( 10.00000000000000000, 14.75893115100078568, -9.846743663894594434 ) ) ;
#76804 = CARTESIAN_POINT ( 'NONE',  ( 2.035157376598822676, 12.43868534415483751, -7.964842623401177768 ) ) ;
#76805 = CARTESIAN_POINT ( 'NONE',  ( -2.816281873526471635, 13.91530133659708746, -3.434112377981056508 ) ) ;
#76806 = CARTESIAN_POINT ( 'NONE',  ( 0.5774900079438607392, 3.480352010821504027, 5.440088680355550821 ) ) ;
#76807 = DIRECTION ( 'NONE',  ( 0.000000000000000000, 0.000000000000000000, 1.000000000000000000 ) ) ;
#76808 = CARTESIAN_POINT ( 'NONE',  ( 10.00000000000000178, 62.25893115100078745, 9.846743663894594434 ) ) ;
#76809 =( GEOMETRIC_REPRESENTATION_CONTEXT ( 3 ) GLOBAL_UNCERTAINTY_ASSIGNED_CONTEXT ( ( #91231 ) ) GLOBAL_UNIT_ASSIGNED_CONTEXT ( ( #1585, #69078, #94035 ) ) REPRESENTATION_CONTEXT ( 'NONE', 'WORKASPACE' ) );
#76810 = CARTESIAN_POINT ( 'NONE',  ( 4.323026924234770085, -6.401461444633167019, -2.500000000000000000 ) ) ;
#76811 = CARTESIAN_POINT ( 'NONE',  ( 17.96484262340118221, 24.93868534415484461, 7.964842623401181321 ) ) ;
#76812 = CARTESIAN_POINT ( 'NONE',  ( 19.84674366389459266, 48.30059781766745175, 2.638427012816836559 ) ) ;
#76813 = CARTESIAN_POINT ( 'NONE',  ( 20.88017736071110164, 20.35535201082150891, 2.915334737309930979 ) ) ;
#76814 = DIRECTION ( 'NONE',  ( 0.000000000000000000, 1.000000000000000000, 0.000000000000000000 ) ) ;
#76815 = CARTESIAN_POINT ( 'NONE',  ( 12.91533473730992121, 34.52201867748817676, 10.88017736071110164 ) ) ;
#76817 = CARTESIAN_POINT ( 'NONE',  ( -0.9940297508535884674, 15.00000000000000000, -14.21528771620250886 ) ) ;
#76816 = CARTESIAN_POINT ( 'NONE',  ( 10.00000000000000000, 65.55374883491396076, -14.16423886937410082 ) ) ;
#76818 = SURFACE_SIDE_STYLE ('',( #90333 ) ) ;
#76819 = CARTESIAN_POINT ( 'NONE',  ( 12.63842701281683034, 27.46726448433411250, 9.846743663894596210 ) ) ;
#76820 = CARTESIAN_POINT ( 'NONE',  ( 6.565887622018943937, 10.16530133659708746, 12.81628187352647430 ) ) ;
#76821 = STYLED_ITEM ( 'NONE', ( #2806 ), #33244 ) ;
#76822 = CARTESIAN_POINT ( 'NONE',  ( -5.817157072110620497, 14.49999999999999112, -13.82608706751101302 ) ) ;
#76823 = DIRECTION ( 'NONE',  ( 0.000000000000000000, 1.000000000000000000, 0.000000000000000000 ) ) ;
#76824 = ADVANCED_FACE ( 'NONE', ( #88063 ), #45572, .T. ) ;
#76825 = SURFACE_STYLE_FILL_AREA ( #861 ) ;
#76826 = CARTESIAN_POINT ( 'NONE',  ( 13.79529636645031943, 5.345415501580634832, -14.16423886937409904 ) ) ;
#76827 = AXIS2_PLACEMENT_3D ( 'NONE', #50649, #4172, #67125 ) ;
#76828 = CARTESIAN_POINT ( 'NONE',  ( 5.076628168052703671, 36.84226448433412315, 8.527530157486179263 ) ) ;
#76829 = VERTEX_POINT ( 'NONE', #83552 ) ;
#76830 = CARTESIAN_POINT ( 'NONE',  ( 17.08211943468705130, 48.47041550158063927, 12.26659068614894998 ) ) ;
#76831 = CARTESIAN_POINT ( 'NONE',  ( 7.361572987183170547, 17.05059781766745530, 9.846743663894590881 ) ) ;
#76833 = CARTESIAN_POINT ( 'NONE',  ( -13.07661834287478797, 15.00000000000000711, -6.550615570651864061 ) ) ;
#76832 = FACE_OUTER_BOUND ( 'NONE', #1407, .T. ) ;
#76834 = CARTESIAN_POINT ( 'NONE',  ( 4.559911319644449179, 42.23035201082151247, -9.422509992056141925 ) ) ;
#76835 = CARTESIAN_POINT ( 'NONE',  ( 13.43411237798105340, 55.58196800326374643, 12.81628187352647963 ) ) ;
#76836 = CARTESIAN_POINT ( 'NONE',  ( 17.96484262340118221, 21.18868534415483396, -7.964842623401177768 ) ) ;
#76837 = AXIS2_PLACEMENT_3D ( 'NONE', #53492, #44514, #29008 ) ;
#76838 = CARTESIAN_POINT ( 'NONE',  ( 0.6178305044545818747, 48.49863466993042493, -9.382169495545419124 ) ) ;
#76839 = CARTESIAN_POINT ( 'NONE',  ( 0.1532563361054082862, 61.21726448433412315, 2.638427012816831674 ) ) ;
#76840 = CARTESIAN_POINT ( 'NONE',  ( 12.63842701281683922, 4.550597817667451750, -9.846743663894590881 ) ) ;
#76841 = VERTEX_POINT ( 'NONE', #82560 ) ;
#76842 = CARTESIAN_POINT ( 'NONE',  ( -18.89999999999999147, 91.00000000000000000, 8.000000000000000000 ) ) ;
#76843 = CARTESIAN_POINT ( 'NONE',  ( 2.562013731377108972, 0.5000000000000000000, -6.499999999999999112 ) ) ;
#76844 = CARTESIAN_POINT ( 'NONE',  ( 22.26659068614895176, 59.72041550158063927, -7.082119434687042414 ) ) ;
#76845 = CARTESIAN_POINT ( 'NONE',  ( -4.164238869374099927, 17.01208216824730357, 3.795296366450308767 ) ) ;
#76846 = CARTESIAN_POINT ( 'NONE',  ( 20.88017736071110875, 20.77201867748816611, -2.915334737309920765 ) ) ;
#76847 = CARTESIAN_POINT ( 'NONE',  ( 20.88017736071110875, 35.77201867748816966, -2.915334737309920765 ) ) ;
#76848 = CARTESIAN_POINT ( 'NONE',  ( 10.09777502097884216, 14.95077488074853456, -10.75551206493379830 ) ) ;
#76849 = DIRECTION ( 'NONE',  ( -0.5948227867513427025, 0.000000000000000000, 0.8038568606172163955 ) ) ;
#76850 = CARTESIAN_POINT ( 'NONE',  ( 4.559911319644449179, 68.89701867748817676, 9.422509992056141925 ) ) ;
#76851 = CARTESIAN_POINT ( 'NONE',  ( 15.44008868035555793, 61.39701867748817676, -9.422509992056140149 ) ) ;
#76852 = CARTESIAN_POINT ( 'NONE',  ( 16.40814093676323893, 20.79030133659708923, 11.09922568453595026 ) ) ;
#76853 = CARTESIAN_POINT ( 'NONE',  ( 18.06765999051786409, 18.99127512925449679, 6.499999999999999112 ) ) ;
#76854 =( GEOMETRIC_REPRESENTATION_CONTEXT ( 3 ) GLOBAL_UNCERTAINTY_ASSIGNED_CONTEXT ( ( #54109 ) ) GLOBAL_UNIT_ASSIGNED_CONTEXT ( ( #28045, #6533, #83030 ) ) REPRESENTATION_CONTEXT ( 'NONE', 'WORKASPACE' ) );
#76855 = DIRECTION ( 'NONE',  ( 0.000000000000000000, 1.000000000000000000, 0.000000000000000000 ) ) ;
#76856 = CARTESIAN_POINT ( 'NONE',  ( 7.361572987183170547, 12.05059781766744997, 9.846743663894590881 ) ) ;
#76857 = CARTESIAN_POINT ( 'NONE',  ( 0.1532563361054100626, 35.80059781766745175, -2.638427012816831230 ) ) ;
#76858 = ADVANCED_FACE ( 'NONE', ( #15075 ), #85287, .T. ) ;
#76859 = CARTESIAN_POINT ( 'NONE',  ( 20.88017736071110519, 15.56368534415483751, 2.639326808657452039E-16 ) ) ;
#76860 = CARTESIAN_POINT ( 'NONE',  ( 3.591859063236763294, 38.29030133659708923, -11.09922568453595026 ) ) ;
#76861 = CARTESIAN_POINT ( 'NONE',  ( 19.84674366389459621, 8.508931151000785675, 7.409399052514197653E-17 ) ) ;
#76862 = CARTESIAN_POINT ( 'NONE',  ( 2.035157376598824452, 13.68868534415483751, 7.964842623401179544 ) ) ;
#76863 = CARTESIAN_POINT ( 'NONE',  ( 14.92337183194729633, 57.67559781766745886, 8.527530157486181039 ) ) ;
#76864 = CARTESIAN_POINT ( 'NONE',  ( 19.84674366389459266, 33.71726448433410894, -2.638427012816827677 ) ) ;
#76865 = CARTESIAN_POINT ( 'NONE',  ( 22.26659068614895176, 24.72041550158063572, -7.082119434687042414 ) ) ;
#76866 = CARTESIAN_POINT ( 'NONE',  ( 10.00000000000000000, 31.81368534415483751, -10.88017736071110342 ) ) ;
#76867 = CARTESIAN_POINT ( 'NONE',  ( 4.559911319644449179, 12.23035201082150536, -9.422509992056141925 ) ) ;
#76868 = CARTESIAN_POINT ( 'NONE',  ( 15.44008868035555793, 26.39701867748817321, -9.422509992056140149 ) ) ;
#76869 = CARTESIAN_POINT ( 'NONE',  ( 15.44008868035555260, 34.73035201082151247, 9.422509992056143702 ) ) ;
#76870 = ORIENTED_EDGE ( 'NONE', *, *, #27596, .F. ) ;
#76871 = EDGE_CURVE ( 'NONE', #65586, #69353, #28320, .T. ) ;
#76872 = CARTESIAN_POINT ( 'NONE',  ( 12.91533473730993009, 46.60535201082150536, -10.88017736071109987 ) ) ;
#76873 = AXIS2_PLACEMENT_3D ( 'NONE', #82853, #92323, #61818 ) ;
#76874 = ORIENTED_EDGE ( 'NONE', *, *, #38798, .F. ) ;
#76875 = CARTESIAN_POINT ( 'NONE',  ( 0.6178305044545838731, 59.74863466993041783, 9.382169495545420901 ) ) ;
#76876 = CARTESIAN_POINT ( 'NONE',  ( 19.42250999205614548, 45.98035201082150536, -5.440088680355545492 ) ) ;
#76877 = CARTESIAN_POINT ( 'NONE',  ( 0.5774900079438607392, 48.48035201082150536, 5.440088680355550821 ) ) ;
#76878 = VERTEX_POINT ( 'NONE', #67532 ) ;
#76880 = ADVANCED_FACE ( 'NONE', ( #28037 ), #73530, .F. ) ;
#76879 = CARTESIAN_POINT ( 'NONE',  ( -0.8801773607111008646, 53.27201867748816966, 2.915334737309923430 ) ) ;
#76881 = CARTESIAN_POINT ( 'NONE',  ( 6.935087012919454175, -80.58470470491536730, 4.000000000001609379 ) ) ;
#76882 = TOROIDAL_SURFACE ( 'NONE', #19432, 14.49999999999999822, 0.5000000000000000000 ) ;
#76883 = DIRECTION ( 'NONE',  ( 1.000000000000000000, 0.000000000000000000, 0.000000000000000000 ) ) ;
#76884 = CARTESIAN_POINT ( 'NONE',  ( -4.164238869374099039, 61.80374883491397497, 8.674139862899312516E-16 ) ) ;
#76885 = CARTESIAN_POINT ( 'NONE',  ( 12.91533473730993009, 61.60535201082150536, -10.88017736071109987 ) ) ;
#76886 = CARTESIAN_POINT ( 'NONE',  ( 20.88017736071110164, 55.35535201082149825, 2.915334737309930979 ) ) ;
#76887 = EDGE_CURVE ( 'NONE', #40011, #86711, #2157, .T. ) ;
#76888 = CARTESIAN_POINT ( 'NONE',  ( -14.09394518620614711, 15.00000000000000000, 3.407449058785264384 ) ) ;
#76889 = CARTESIAN_POINT ( 'NONE',  ( -14.99847009497950978, 14.49999999999999112, 0.2142307401079103502 ) ) ;
#76890 = CARTESIAN_POINT ( 'NONE',  ( 0.1532563361054083140, 31.00893115100078390, 1.131784320476157264E-15 ) ) ;
#76891 = ORIENTED_EDGE ( 'NONE', *, *, #73921, .F. ) ;
#76892 = CARTESIAN_POINT ( 'NONE',  ( 19.84674366389459266, 28.71726448433411960, -2.638427012816827677 ) ) ;
#76893 = CARTESIAN_POINT ( 'NONE',  ( -0.8801773607111009756, 38.06368534415484106, 1.068504757029289695E-15 ) ) ;
#76894 = CARTESIAN_POINT ( 'NONE',  ( 12.63842701281683034, 42.46726448433412315, 9.846743663894596210 ) ) ;
#76896 = CARTESIAN_POINT ( 'NONE',  ( 20.88017736071110164, 55.35535201082149825, 2.915334737309930979 ) ) ;
#76895 = CARTESIAN_POINT ( 'NONE',  ( 20.10239578412226891, 2.633775574782959428, -6.340343622311910288 ) ) ;
#76898 = SURFACE_STYLE_FILL_AREA ( #61398 ) ;
#76897 = CARTESIAN_POINT ( 'NONE',  ( 20.88017736071110875, 50.77201867748817676, -2.915334737309920765 ) ) ;
#76899 = CARTESIAN_POINT ( 'NONE',  ( -4.164238869374099039, 51.80374883491396787, 8.674139862899312516E-16 ) ) ;
#76900 = CIRCLE ( 'NONE', #46568, 19.99999999999999645 ) ;
#76901 = AXIS2_PLACEMENT_3D ( 'NONE', #5849, #98851, #60807 ) ;
#76902 = EDGE_CURVE ( 'NONE', #59535, #45656, #3708, .T. ) ;
#76903 = CARTESIAN_POINT ( 'NONE',  ( 3.591859063236763294, 23.29030133659708568, -11.09922568453595026 ) ) ;
#76904 = CARTESIAN_POINT ( 'NONE',  ( 0.000000000000000000, 14.49999999999999822, 0.000000000000000000 ) ) ;
#76905 = ORIENTED_EDGE ( 'NONE', *, *, #46967, .T. ) ;
#76906 = CARTESIAN_POINT ( 'NONE',  ( -1.099225684535947600, 14.54030133659708568, 6.408140936763237150 ) ) ;
#76907 = CARTESIAN_POINT ( 'NONE',  ( 17.96484262340118221, 21.18868534415483396, -7.964842623401177768 ) ) ;
#76908 = CARTESIAN_POINT ( 'NONE',  ( 12.91533473730992121, 64.52201867748817676, 10.88017736071110164 ) ) ;
#76909 = AXIS2_PLACEMENT_3D ( 'NONE', #7315, #15322, #14826 ) ;
#76911 = ORIENTED_EDGE ( 'NONE', *, *, #63010, .F. ) ;
#76910 = EDGE_CURVE ( 'NONE', #74647, #69120, #69156, .T. ) ;
#76912 = B_SPLINE_CURVE_WITH_KNOTS ( 'NONE', 3,
 ( #75613, #16103, #22629, #46590, #640, #83617 ),
 .UNSPECIFIED., .F., .F.,
 ( 4, 2, 4 ),
 ( 0.0002800026249563186903, 0.0006862078800502437095, 0.001092413135144168837 ),
 .UNSPECIFIED. ) ;
#76913 = CARTESIAN_POINT ( 'NONE',  ( 12.63842701281683922, 4.550597817667451750, -9.846743663894590881 ) ) ;
#76914 = AXIS2_PLACEMENT_3D ( 'NONE', #23092, #25063, #15099 ) ;
#76915 = CARTESIAN_POINT ( 'NONE',  ( 2.791683348922240793, 51.63393115100078745, 7.208316651077764092 ) ) ;
#76916 = CARTESIAN_POINT ( 'NONE',  ( 14.92337183194729988, 34.34226448433411605, -8.527530157486177487 ) ) ;
#76917 = DIRECTION ( 'NONE',  ( 0.000000000000000000, 1.000000000000000000, 0.000000000000000000 ) ) ;
#76918 = CARTESIAN_POINT ( 'NONE',  ( 0.1532563361054082862, 21.21726448433412315, 2.638427012816831674 ) ) ;
#76919 = CARTESIAN_POINT ( 'NONE',  ( 21.92686044187656336, 56.97997603579417358, 3.195792623639536423 ) ) ;
#76920 = PLANE ( 'NONE',  #75594 ) ;
#76922 = CARTESIAN_POINT ( 'NONE',  ( 14.99847009497944583, 15.00000000000000000, -0.2142307401080305596 ) ) ;
#76921 = CARTESIAN_POINT ( 'NONE',  ( 10.00000000000000178, 12.25893115100078568, 9.846743663894594434 ) ) ;
#76923 = DIRECTION ( 'NONE',  ( -0.000000000000000000, -0.000000000000000000, 1.000000000000000000 ) ) ;
#76925 = EDGE_LOOP ( 'NONE', ( #8418, #18468, #60262, #8177 ) ) ;
#76924 = CARTESIAN_POINT ( 'NONE',  ( 2.791683348922237240, 40.38393115100078035, -7.208316651077763204 ) ) ;
#76926 = B_SPLINE_CURVE_WITH_KNOTS ( 'NONE', 3,
 ( #63092, #26093, #56589, #9606, #64062, #47100, #9113, #24626, #33567, #86105 ),
 .UNSPECIFIED., .F., .F.,
 ( 4, 3, 3, 4 ),
 ( 2.023017827855918282E-17, 0.0006253016069560817305, 0.001250604074564927361, 0.002501455912506536129 ),
 .UNSPECIFIED. ) ;
#76927 = CARTESIAN_POINT ( 'NONE',  ( -4.000000000000000000, 36.75000000000000000, 2.750000000000000000 ) ) ;
#76928 = CARTESIAN_POINT ( 'NONE',  ( 3.591859063236763294, 18.29030133659708568, -11.09922568453595026 ) ) ;
#76929 = CARTESIAN_POINT ( 'NONE',  ( 19.42250999205614548, 55.98035201082150536, -5.440088680355545492 ) ) ;
#76930 = CARTESIAN_POINT ( 'NONE',  ( 6.204703633549690345, 32.84541550158063927, 14.16423886937410082 ) ) ;
#76931 = B_SPLINE_CURVE_WITH_KNOTS ( 'NONE', 3,
 ( #14316, #36808, #88812, #5815, #51309, #20326, #12808, #44785, #4349, #50820 ),
 .UNSPECIFIED., .F., .F.,
 ( 4, 2, 2, 2, 4 ),
 ( 3.632321844000487879E-16, 0.0002035700444593245724, 0.0004071400889182858829, 0.0008142801778362085581, 0.001628560355672053908 ),
 .UNSPECIFIED. ) ;
#76932 = DIRECTION ( 'NONE',  ( -0.7253743710122912969, 0.000000000000000000, 0.6883545756937501370 ) ) ;
#76933 = CARTESIAN_POINT ( 'NONE',  ( -4.164238869374099927, 42.01208216824728936, 3.795296366450308767 ) ) ;
#76934 = CARTESIAN_POINT ( 'NONE',  ( 22.26659068614895176, 64.72041550158064638, -7.082119434687042414 ) ) ;
#76935 = CARTESIAN_POINT ( 'NONE',  ( -2.266590686148945544, 26.38708216824730357, -7.082119434687050408 ) ) ;
#76937 = CARTESIAN_POINT ( 'NONE',  ( 19.72487221294570148, 35.71833443783938833, -6.500000000000010658 ) ) ;
#76936 = CARTESIAN_POINT ( 'NONE',  ( -2.266590686148945544, 22.22041550158063572, 7.082119434687048631 ) ) ;
#76938 = DIRECTION ( 'NONE',  ( 0.000000000000000000, -1.000000000000000000, -0.000000000000000000 ) ) ;
#76940 = CARTESIAN_POINT ( 'NONE',  ( 7.361572987183170547, 37.05059781766744464, 9.846743663894590881 ) ) ;
#76939 = LINE ( 'NONE', #39935, #56438 ) ;
#76941 = ORIENTED_EDGE ( 'NONE', *, *, #21041, .F. ) ;
#76942 = CARTESIAN_POINT ( 'NONE',  ( 17.96484262340118221, 21.18868534415483396, -7.964842623401177768 ) ) ;
#76943 = DIRECTION ( 'NONE',  ( -0.2334453638559087496, 0.000000000000000000, 0.9723699203976758909 ) ) ;
#76944 = DIRECTION ( 'NONE',  ( -1.000000000000000000, 0.000000000000000000, 0.000000000000000000 ) ) ;
#76945 = CARTESIAN_POINT ( 'NONE',  ( 20.00000000000000711, 87.39023020535609021, -4.970182471799478918 ) ) ;
#76946 = CARTESIAN_POINT ( 'NONE',  ( 17.20831665107776587, 39.13393115100079456, -7.208316651077762316 ) ) ;
#76947 = CARTESIAN_POINT ( 'NONE',  ( -2.816281873526473856, 59.33196800326374643, 3.434112377981055619 ) ) ;
#76948 = CARTESIAN_POINT ( 'NONE',  ( -14.16423886937409726, -12.98791783175269643, 3.795296366450320757 ) ) ;
#76949 = CARTESIAN_POINT ( 'NONE',  ( 10.00000000000000178, 37.25893115100078745, 9.846743663894594434 ) ) ;
#76950 = CARTESIAN_POINT ( 'NONE',  ( 2.791683348922240793, 46.63393115100077324, 7.208316651077764092 ) ) ;
#76951 = CIRCLE ( 'NONE', #67394, 14.49999999999999822 ) ;
#76952 = CARTESIAN_POINT ( 'NONE',  ( 13.79529636645030344, 43.26208216824730357, 14.16423886937410614 ) ) ;
#76953 = ORIENTED_EDGE ( 'NONE', *, *, #36104, .T. ) ;
#76954 = CARTESIAN_POINT ( 'NONE',  ( -0.3689425029237898834, 16.17874883491396076, -10.36894250292378850 ) ) ;
#76955 = CARTESIAN_POINT ( 'NONE',  ( 4.559911319644449179, 63.89701867748817676, 9.422509992056141925 ) ) ;
#76956 = DIRECTION ( 'NONE',  ( -0.5905099943842175847, -0.8070303256584298035, 0.000000000000000000 ) ) ;
#76957 = CARTESIAN_POINT ( 'NONE',  ( 7.084665262690076126, 7.022018677488170546, -10.88017736071110164 ) ) ;
#76958 = CARTESIAN_POINT ( 'NONE',  ( -2.816281873526473856, 9.331968003263753531, 3.434112377981055619 ) ) ;
#76959 = CARTESIAN_POINT ( 'NONE',  ( 8.879999999999995453, 41.24999999999999289, -6.250000000000000000 ) ) ;
#76960 = CARTESIAN_POINT ( 'NONE',  ( 19.84674366389459266, 3.717264484334118713, -2.638427012816827677 ) ) ;
#76961 = DIRECTION ( 'NONE',  ( 0.000000000000000000, 1.000000000000000000, 0.000000000000000000 ) ) ;
#76962 = CARTESIAN_POINT ( 'NONE',  ( 0.1532563361054100626, 30.80059781766745175, -2.638427012816831230 ) ) ;
#76963 = EDGE_CURVE ( 'NONE', #13116, #17551, #13249, .T. ) ;
#76964 = CARTESIAN_POINT ( 'NONE',  ( -2.266590686148945544, 61.38708216824730357, -7.082119434687050408 ) ) ;
#76965 = DIRECTION ( 'NONE',  ( 0.000000000000000000, 0.000000000000000000, -1.000000000000000000 ) ) ;
#76966 = CARTESIAN_POINT ( 'NONE',  ( 0.5774900079438607392, 23.48035201082150536, 5.440088680355550821 ) ) ;
#76967 = CARTESIAN_POINT ( 'NONE',  ( 20.88017736071110519, 25.56368534415483751, 2.639326808657452039E-16 ) ) ;
#76968 = CARTESIAN_POINT ( 'NONE',  ( 19.84674366389459266, 53.71726448433411605, -2.638427012816827677 ) ) ;
#76969 = CARTESIAN_POINT ( 'NONE',  ( 17.20831665107776587, 59.13393115100078745, -7.208316651077762316 ) ) ;
#76970 = CARTESIAN_POINT ( 'NONE',  ( 13.43411237798105340, 55.58196800326374643, 12.81628187352647963 ) ) ;
#76971 = CARTESIAN_POINT ( 'NONE',  ( 7.361572987183170547, 2.050597817667451750, 9.846743663894590881 ) ) ;
#76972 = VERTEX_POINT ( 'NONE', #97063 ) ;
#76973 = EDGE_CURVE ( 'NONE', #93626, #45054, #58532, .T. ) ;
#76974 = CARTESIAN_POINT ( 'NONE',  ( 0.5774900079438590739, 22.64701867748817321, -5.440088680355550821 ) ) ;
#76975 = CARTESIAN_POINT ( 'NONE',  ( -1.099225684535947600, 18.70696800326375353, -6.408140936763238038 ) ) ;
#76976 = CARTESIAN_POINT ( 'NONE',  ( -8.000000000000000000, 41.24999999999999289, -4.250000000000000000 ) ) ;
#76977 = AXIS2_PLACEMENT_3D ( 'NONE', #36934, #917, #67425 ) ;
#76978 = CARTESIAN_POINT ( 'NONE',  ( 5.076628168052703671, 41.84226448433411605, 8.527530157486179263 ) ) ;
#76979 = CARTESIAN_POINT ( 'NONE',  ( 20.88017736071110875, 50.77201867748817676, -2.915334737309920765 ) ) ;
#76980 = CARTESIAN_POINT ( 'NONE',  ( 21.09922568453594849, 21.20696800326375353, 6.408140936763242479 ) ) ;
#76982 = PLANE ( 'NONE',  #81550 ) ;
#76981 = CARTESIAN_POINT ( 'NONE',  ( 0.5774900079438590739, 57.64701867748817676, -5.440088680355550821 ) ) ;
#76983 = CARTESIAN_POINT ( 'NONE',  ( -0.1023957841222410819, 50.13377557478298030, 6.340343622311920058 ) ) ;
#76984 = AXIS2_PLACEMENT_3D ( 'NONE', #16072, #31550, #46559 ) ;
#76985 = CARTESIAN_POINT ( 'NONE',  ( 3.591859063236761518, 64.95696800326376774, 11.09922568453594849 ) ) ;
#76986 = ORIENTED_EDGE ( 'NONE', *, *, #56748, .F. ) ;
#76987 = DIRECTION ( 'NONE',  ( 0.000000000000000000, 0.000000000000000000, 1.000000000000000000 ) ) ;
#76988 = DIRECTION ( 'NONE',  ( -0.000000000000000000, -1.000000000000000000, -0.000000000000000000 ) ) ;
#76989 = CARTESIAN_POINT ( 'NONE',  ( 7.084665262690076126, 49.10535201082149825, 10.88017736071109987 ) ) ;
#76991 = CARTESIAN_POINT ( 'NONE',  ( 13.79529636645031943, 15.34541550158063750, -14.16423886937409904 ) ) ;
#76990 = CARTESIAN_POINT ( 'NONE',  ( 21.09922568453595559, 47.04030133659708923, -6.408140936763230044 ) ) ;
#76992 = CARTESIAN_POINT ( 'NONE',  ( 14.92337183194729988, 9.342264484334119601, -8.527530157486177487 ) ) ;
#76993 = AXIS2_PLACEMENT_3D ( 'NONE', #31009, #61505, #90037 ) ;
#76994 = CARTESIAN_POINT ( 'NONE',  ( 0.1532563361054083140, 66.00893115100079456, 1.131784320476157264E-15 ) ) ;
#76995 = CARTESIAN_POINT ( 'NONE',  ( 2.791683348922237240, 15.38393115100078212, -7.208316651077763204 ) ) ;
#76996 = FACE_OUTER_BOUND ( 'NONE', #83337, .T. ) ;
#76997 = CARTESIAN_POINT ( 'NONE',  ( 24.16423886937409904, 54.09541550158063217, 3.795296366450317205 ) ) ;
#76998 = CARTESIAN_POINT ( 'NONE',  ( 0.4195498155886434599, -2.441190589077521466E-17, -9.500000000000000000 ) ) ;
#76999 = CARTESIAN_POINT ( 'NONE',  ( 20.88017736071110164, 5.355352010821502695, 2.915334737309930979 ) ) ;
#77000 = CARTESIAN_POINT ( 'NONE',  ( -7.374934931933696092, -78.83424294380051833, -4.000000000000000888 ) ) ;
#77001 = VECTOR ( 'NONE', #8452, 1000.000000000000000 ) ;
#77002 = ORIENTED_EDGE ( 'NONE', *, *, #63590, .F. ) ;
#77003 = CARTESIAN_POINT ( 'NONE',  ( 19.42250999205614193, 10.14701867748816966, 5.440088680355555262 ) ) ;
#77005 = EDGE_CURVE ( 'NONE', #22285, #86977, #75516, .T. ) ;
#77004 = CARTESIAN_POINT ( 'NONE',  ( -0.8801773607111008646, 8.272018677488171434, 2.915334737309923430 ) ) ;
#77006 = CARTESIAN_POINT ( 'NONE',  ( 18.52753015748618282, 43.92559781766745175, -4.923371831947291888 ) ) ;
#77007 = CARTESIAN_POINT ( 'NONE',  ( -2.816281873526471635, 38.91530133659708213, -3.434112377981056508 ) ) ;
#77008 = DIRECTION ( 'NONE',  ( -0.000000000000000000, -0.000000000000000000, -1.000000000000000000 ) ) ;
#77010 = CARTESIAN_POINT ( 'NONE',  ( 2.917880565312950480, 25.97041550158063572, -12.26659068614894821 ) ) ;
#77009 = CARTESIAN_POINT ( 'NONE',  ( -10.19513985507841447, 14.63595249122789177, 11.00268709613211371 ) ) ;
#77011 = CARTESIAN_POINT ( 'NONE',  ( 7.084665262690076126, 22.02201867748817321, -10.88017736071110164 ) ) ;
#77012 = CARTESIAN_POINT ( 'NONE',  ( 4.559911319644449179, 3.897018677488171434, 9.422509992056141925 ) ) ;
#77013 = CARTESIAN_POINT ( 'NONE',  ( 7.361572987183170547, 37.05059781766744464, 9.846743663894590881 ) ) ;
#77014 = EDGE_CURVE ( 'NONE', #84056, #38312, #86767, .T. ) ;
#77015 = CARTESIAN_POINT ( 'NONE',  ( -5.845017550302832987, 15.00000000000000000, -14.89003580495041668 ) ) ;
#77016 = CARTESIAN_POINT ( 'NONE',  ( 14.92337183194729988, 19.34226448433411960, -8.527530157486177487 ) ) ;
#77017 = CARTESIAN_POINT ( 'NONE',  ( 0.1532563361054100626, 0.8005978176674514168, -2.638427012816831230 ) ) ;
#77018 = CARTESIAN_POINT ( 'NONE',  ( 9.382169495545419124, -39.00136533006958217, 9.382169495545417348 ) ) ;
#77019 = VERTEX_POINT ( 'NONE', #34846 ) ;
#77020 = PRODUCT_RELATED_PRODUCT_CATEGORY ( 'part', '', ( #5926 ) ) ;
#77021 = ORIENTED_EDGE ( 'NONE', *, *, #10215, .T. ) ;
#77022 = CARTESIAN_POINT ( 'NONE',  ( 12.63842701281683922, 54.55059781766745175, -9.846743663894590881 ) ) ;
#77024 = CARTESIAN_POINT ( 'NONE',  ( 0.5774900079438590739, 37.64701867748817676, -5.440088680355550821 ) ) ;
#77023 = CARTESIAN_POINT ( 'NONE',  ( 15.44008868035555793, 36.39701867748816966, -9.422509992056140149 ) ) ;
#77026 = CARTESIAN_POINT ( 'NONE',  ( 6.565887622018943937, 30.16530133659708568, 12.81628187352647430 ) ) ;
#77025 = CARTESIAN_POINT ( 'NONE',  ( 12.91533473730992121, 4.522018677488169658, 10.88017736071110164 ) ) ;
#77027 = CARTESIAN_POINT ( 'NONE',  ( 20.36894250292379382, 23.67874883491397142, 10.36894250292379205 ) ) ;
#77028 = ORIENTED_EDGE ( 'NONE', *, *, #72974, .F. ) ;
#77029 = VECTOR ( 'NONE', #73334, 999.9999999999998863 ) ;
#77030 = EDGE_CURVE ( 'NONE', #86977, #9285, #88336, .T. ) ;
#77031 = ADVANCED_FACE ( 'NONE', ( #49855 ), #97355, .T. ) ;
#77032 = CARTESIAN_POINT ( 'NONE',  ( 3.591859063236761518, 44.95696800326376064, 11.09922568453594849 ) ) ;
#77033 = EDGE_LOOP ( 'NONE', ( #9633, #911, #86848, #45471, #90791, #34879 ) ) ;
#77034 = CARTESIAN_POINT ( 'NONE',  ( 12.63842701281683922, 39.55059781766744464, -9.846743663894590881 ) ) ;
#77035 = CARTESIAN_POINT ( 'NONE',  ( 20.88017736071110875, 25.77201867748816966, -2.915334737309920765 ) ) ;
#77036 = ORIENTED_EDGE ( 'NONE', *, *, #77030, .T. ) ;
#77037 = CARTESIAN_POINT ( 'NONE',  ( 0.5774900079438607392, 13.48035201082150358, 5.440088680355550821 ) ) ;
#77038 = ORIENTED_EDGE ( 'NONE', *, *, #45390, .T. ) ;
#77039 = CARTESIAN_POINT ( 'NONE',  ( 20.88017736071110875, 55.77201867748816966, -2.915334737309920765 ) ) ;
#77040 = CARTESIAN_POINT ( 'NONE',  ( 7.084665262690076126, 67.02201867748817676, -10.88017736071110164 ) ) ;
#77041 = CARTESIAN_POINT ( 'NONE',  ( 19.42250999205614548, 65.98035201082151957, -5.440088680355545492 ) ) ;
#77042 = CARTESIAN_POINT ( 'NONE',  ( 17.20831665107776587, 4.133931151000785675, -7.208316651077762316 ) ) ;
#77043 = CARTESIAN_POINT ( 'NONE',  ( 4.559911319644449179, 62.23035201082150536, -9.422509992056141925 ) ) ;
#77044 = DIRECTION ( 'NONE',  ( 8.673617379884028570E-16, 1.000000000000000000, -9.540979117872446908E-15 ) ) ;
#77045 = CARTESIAN_POINT ( 'NONE',  ( 1.472469842513823179, 11.42559781766745175, 4.923371831947296329 ) ) ;
#77046 = CARTESIAN_POINT ( 'NONE',  ( 5.076628168052703671, 11.84226448433411960, 8.527530157486179263 ) ) ;
#77047 = CARTESIAN_POINT ( 'NONE',  ( 1.472469842513823179, 46.42559781766745175, 4.923371831947296329 ) ) ;
#77048 = VERTEX_POINT ( 'NONE', #95361 ) ;
#77049 = ORIENTED_EDGE ( 'NONE', *, *, #71517, .T. ) ;
#77050 = DIRECTION ( 'NONE',  ( 0.000000000000000000, 0.000000000000000000, -1.000000000000000000 ) ) ;
#77051 = AXIS2_PLACEMENT_3D ( 'NONE', #42737, #35214, #19734 ) ;
#77052 = AXIS2_PLACEMENT_3D ( 'NONE', #36980, #34986, #52467 ) ;
#77053 = AXIS2_PLACEMENT_3D ( 'NONE', #48367, #41394, #63846 ) ;
#77054 = CARTESIAN_POINT ( 'NONE',  ( 22.26659068614895176, 19.72041550158063572, -7.082119434687042414 ) ) ;
#77055 = CARTESIAN_POINT ( 'NONE',  ( 10.00000000000000178, 70.00000000000000000, 0.000000000000000000 ) ) ;
#77056 = CYLINDRICAL_SURFACE ( 'NONE', #32235, 0.5000000000000004441 ) ;
#77057 = CARTESIAN_POINT ( 'NONE',  ( 20.88017736071110164, 25.35535201082150891, 2.915334737309930979 ) ) ;
#77058 = CARTESIAN_POINT ( 'NONE',  ( 0.2751277870542876980, 48.21833443783936701, 6.499999999999984901 ) ) ;
#77059 = ORIENTED_EDGE ( 'NONE', *, *, #27965, .F. ) ;
#77061 = VECTOR ( 'NONE', #4296, 1000.000000000000000 ) ;
#77060 = CARTESIAN_POINT ( 'NONE',  ( 1.472469842513823179, 0.5922644843341181575, -4.923371831947296329 ) ) ;
#77062 =( NAMED_UNIT ( * ) SI_UNIT ( $, .STERADIAN. ) SOLID_ANGLE_UNIT ( ) );
#77063 = CARTESIAN_POINT ( 'NONE',  ( 6.565887622018943937, 35.16530133659708923, 12.81628187352647430 ) ) ;
#77064 = CARTESIAN_POINT ( 'NONE',  ( 14.92337183194729633, 17.67559781766745175, 8.527530157486181039 ) ) ;
#77065 = CARTESIAN_POINT ( 'NONE',  ( 16.40814093676323893, 20.79030133659708923, 11.09922568453595026 ) ) ;
#77066 = VECTOR ( 'NONE', #86795, 1000.000000000000114 ) ;
#77067 = DIRECTION ( 'NONE',  ( 0.000000000000000000, 1.000000000000000000, 0.000000000000000000 ) ) ;
#77068 = CARTESIAN_POINT ( 'NONE',  ( 19.84674366389459266, 3.717264484334118713, -2.638427012816827677 ) ) ;
#77069 = VERTEX_POINT ( 'NONE', #4381 ) ;
#77070 = ORIENTED_EDGE ( 'NONE', *, *, #67793, .T. ) ;
#77071 = CARTESIAN_POINT ( 'NONE',  ( -0.8801773607111009756, 28.06368534415484106, 1.068504757029289695E-15 ) ) ;
#77072 = CARTESIAN_POINT ( 'NONE',  ( 22.26659068614894466, 23.88708216824730357, 7.082119434687054849 ) ) ;
#77073 = CARTESIAN_POINT ( 'NONE',  ( 2.791683348922240793, 41.63393115100078745, 7.208316651077764092 ) ) ;
#77074 = CARTESIAN_POINT ( 'NONE',  ( 7.084665262690076126, 67.02201867748817676, -10.88017736071110164 ) ) ;
#77076 = DIRECTION ( 'NONE',  ( 0.000000000000000000, -0.000000000000000000, 1.000000000000000000 ) ) ;
#77075 = CARTESIAN_POINT ( 'NONE',  ( -2.816281873526473856, 59.12363466993042493, 9.499525473075851096E-16 ) ) ;
#77077 = CARTESIAN_POINT ( 'NONE',  ( 19.42250999205614548, 25.98035201082150891, -5.440088680355545492 ) ) ;
#77078 = DIRECTION ( 'NONE',  ( 0.08715574274765112983, 0.9961946980917461003, 0.000000000000000000 ) ) ;
#77079 = COLOUR_RGB ( '', 0.72549020, 0.75294118, 0.79215686) ;
#77080 = CARTESIAN_POINT ( 'NONE',  ( -1.099225684535947600, 4.540301336597087456, 6.408140936763237150 ) ) ;
#77081 = CARTESIAN_POINT ( 'NONE',  ( 7.361572987183170547, 47.05059781766745175, 9.846743663894590881 ) ) ;
#77082 = CARTESIAN_POINT ( 'NONE',  ( 9.422509992056141925, -4.019647989178490199, -5.440088680355554374 ) ) ;
#77083 = CARTESIAN_POINT ( 'NONE',  ( 19.38216949554541557, 47.24863466993041783, -9.382169495545420901 ) ) ;
#77084 = LINE ( 'NONE', #47577, #72330 ) ;
#77086 = LINE ( 'NONE', #92580, #16067 ) ;
#77085 = CARTESIAN_POINT ( 'NONE',  ( -0.8801773607111008646, 48.27201867748816966, 2.915334737309923430 ) ) ;
#77087 = ADVANCED_FACE ( 'NONE', ( #65840 ), #26861, .T. ) ;
#77088 = DIRECTION ( 'NONE',  ( -0.2334453638559087496, 0.000000000000000000, 0.9723699203976758909 ) ) ;
#77089 = CARTESIAN_POINT ( 'NONE',  ( 4.559911319644449179, 52.23035201082151247, -9.422509992056141925 ) ) ;
#77091 = CARTESIAN_POINT ( 'NONE',  ( 17.96484262340118221, 46.18868534415484106, -7.964842623401177768 ) ) ;
#77090 = TOROIDAL_SURFACE ( 'NONE', #26004, 14.49999999999999822, 0.5000000000000000000 ) ;
#77092 = CYLINDRICAL_SURFACE ( 'NONE', #28105, 15.00000000000000000 ) ;
#77093 = CARTESIAN_POINT ( 'NONE',  ( 7.084665262690076126, 69.10535201082151957, 10.88017736071109987 ) ) ;
#77094 = CARTESIAN_POINT ( 'NONE',  ( 14.92337183194729633, 52.67559781766745175, 8.527530157486181039 ) ) ;
#77096 = DIRECTION ( 'NONE',  ( -0.9890158633619177131, 0.000000000000000000, 0.1478094111296046342 ) ) ;
#77095 = CARTESIAN_POINT ( 'NONE',  ( 7.084665262690076126, 12.02201867748817143, -10.88017736071110164 ) ) ;
#77097 = CARTESIAN_POINT ( 'NONE',  ( -1.099225684535947600, 19.54030133659708568, 6.408140936763237150 ) ) ;
#77098 = EDGE_LOOP ( 'NONE', ( #11824, #40156, #4460, #52109 ) ) ;
#77099 = CARTESIAN_POINT ( 'NONE',  ( 10.00000000000000000, 36.81368534415484106, -10.88017736071110342 ) ) ;
#77101 = CARTESIAN_POINT ( 'NONE',  ( 20.10239578412226180, 47.63377557478296609, -6.340343622311913840 ) ) ;
#77100 = CARTESIAN_POINT ( 'NONE',  ( 22.81628187352647785, 1.415301336597087012, 3.434112377981063169 ) ) ;
#77102 = CARTESIAN_POINT ( 'NONE',  ( 4.559911319644449179, 17.23035201082150536, -9.422509992056141925 ) ) ;
#77103 = CARTESIAN_POINT ( 'NONE',  ( 19.42250999205614193, 30.14701867748817321, 5.440088680355555262 ) ) ;
#77104 = CARTESIAN_POINT ( 'NONE',  ( 17.08211943468705130, 33.47041550158063927, 12.26659068614894998 ) ) ;
#77105 = CARTESIAN_POINT ( 'NONE',  ( 19.84674366389459266, 28.30059781766745886, 2.638427012816836559 ) ) ;
#77106 = CARTESIAN_POINT ( 'NONE',  ( -0.8801773607111009756, 58.06368534415484106, 1.068504757029289695E-15 ) ) ;
#77107 = FACE_OUTER_BOUND ( 'NONE', #79767, .T. ) ;
#77108 = CARTESIAN_POINT ( 'NONE',  ( -2.266590686148945544, 2.220415501580634388, 7.082119434687048631 ) ) ;
#77109 = DIRECTION ( 'NONE',  ( -0.000000000000000000, -0.000000000000000000, 1.000000000000000000 ) ) ;
#77110 = CARTESIAN_POINT ( 'NONE',  ( 17.20831665107776587, 64.13393115100079456, -7.208316651077762316 ) ) ;
#77111 = VERTEX_POINT ( 'NONE', #81826 ) ;
#77112 = CARTESIAN_POINT ( 'NONE',  ( 20.36894250292379382, 28.67874883491396787, 10.36894250292379205 ) ) ;
#77114 = EDGE_CURVE ( 'NONE', #70392, #44443, #88355, .T. ) ;
#77113 = CARTESIAN_POINT ( 'NONE',  ( -4.164238869374099927, 32.01208216824730357, 3.795296366450308767 ) ) ;
#77115 = CARTESIAN_POINT ( 'NONE',  ( 17.20831665107776587, 2.883931151000785231, 7.208316651077764980 ) ) ;
#77116 = CARTESIAN_POINT ( 'NONE',  ( 22.81628187352648496, 6.831968003263753531, -3.434112377981050290 ) ) ;
#77117 = CARTESIAN_POINT ( 'NONE',  ( 19.84674366389459266, 63.30059781766745886, 2.638427012816836559 ) ) ;
#77118 = CARTESIAN_POINT ( 'NONE',  ( -10.79671963681641600, -44.59934526486136974, 3.999999999996397992 ) ) ;
#77120 = CARTESIAN_POINT ( 'NONE',  ( 6.565887622018943937, 25.16530133659708213, 12.81628187352647430 ) ) ;
#77119 = CARTESIAN_POINT ( 'NONE',  ( 2.035157376598824452, 63.68868534415484106, 7.964842623401179544 ) ) ;
#77121 = CARTESIAN_POINT ( 'NONE',  ( 17.08211943468705130, 33.47041550158063927, 12.26659068614894998 ) ) ;
#77122 = CARTESIAN_POINT ( 'NONE',  ( 2.035157376598822676, 32.43868534415483396, -7.964842623401177768 ) ) ;
#77123 = AXIS2_PLACEMENT_3D ( 'NONE', #44599, #29579, #68596 ) ;
#77124 = CARTESIAN_POINT ( 'NONE',  ( 15.44008868035555260, 34.73035201082151247, 9.422509992056143702 ) ) ;
#77125 = EDGE_CURVE ( 'NONE', #38057, #10110, #77192, .T. ) ;
#77126 = CARTESIAN_POINT ( 'NONE',  ( 4.838527690343520149, 14.49999999999999112, 14.19819177887736927 ) ) ;
#77127 = CARTESIAN_POINT ( 'NONE',  ( 20.88017736071110164, 50.35535201082151247, 2.915334737309930979 ) ) ;
#77128 = VECTOR ( 'NONE', #70579, 1000.000000000000000 ) ;
#77129 = CARTESIAN_POINT ( 'NONE',  ( 8.527530157486179263, -16.90773551566587685, 4.923371831947292776 ) ) ;
#77130 = VERTEX_POINT ( 'NONE', #43340 ) ;
#77131 = CARTESIAN_POINT ( 'NONE',  ( 17.39651004071838969, 54.08210964143329846, -6.500000000000027534 ) ) ;
#77132 = STYLED_ITEM ( 'NONE', ( #37346 ), #77457 ) ;
#77133 = DIRECTION ( 'NONE',  ( -0.000000000000000000, 1.000000000000000000, -0.000000000000000000 ) ) ;
#77134 = ORIENTED_EDGE ( 'NONE', *, *, #50492, .F. ) ;
#77135 = CARTESIAN_POINT ( 'NONE',  ( 22.26659068614894466, 3.887082168247300906, 7.082119434687054849 ) ) ;
#77137 = CARTESIAN_POINT ( 'NONE',  ( -4.164238869374099039, 66.80374883491396076, 8.674139862899312516E-16 ) ) ;
#77136 = CARTESIAN_POINT ( 'NONE',  ( 24.16423886937410614, 59.30374883491397497, 8.672049930838204340E-16 ) ) ;
#77139 = CARTESIAN_POINT ( 'NONE',  ( 5.076628168052703671, 56.84226448433412315, 8.527530157486179263 ) ) ;
#77138 = CARTESIAN_POINT ( 'NONE',  ( 12.63842701281683922, 39.55059781766744464, -9.846743663894590881 ) ) ;
#77140 = CARTESIAN_POINT ( 'NONE',  ( 19.89220837332778657, 49.74062864464239908, 6.478736007405907493 ) ) ;
#77141 = CARTESIAN_POINT ( 'NONE',  ( -2.816281873526471635, 8.915301336597083903, -3.434112377981056508 ) ) ;
#77142 = EDGE_LOOP ( 'NONE', ( #74569, #63476, #98534, #77021 ) ) ;
#77143 = CARTESIAN_POINT ( 'NONE',  ( 17.08211943468705840, 45.13708216824730357, -12.26659068614894466 ) ) ;
#77144 = CARTESIAN_POINT ( 'NONE',  ( 24.16423886937410614, 44.51208216824730357, -3.795296366450302550 ) ) ;
#77145 = ORIENTED_EDGE ( 'NONE', *, *, #94125, .T. ) ;
#77146 = CARTESIAN_POINT ( 'NONE',  ( 7.084665262690076126, 24.10535201082150181, 10.88017736071109987 ) ) ;
#77147 = CARTESIAN_POINT ( 'NONE',  ( 13.43411237798106583, 62.66530133659708923, -12.81628187352647252 ) ) ;
#77148 = ADVANCED_FACE ( 'NONE', ( #80855 ), #21344, .T. ) ;
#77149 = CARTESIAN_POINT ( 'NONE',  ( 7.361572987183170547, 52.05059781766745175, 9.846743663894590881 ) ) ;
#77150 = CARTESIAN_POINT ( 'NONE',  ( 7.084665262690076126, 32.02201867748816966, -10.88017736071110164 ) ) ;
#77151 = CARTESIAN_POINT ( 'NONE',  ( -3.377746357650261988, -3.629174488344649951, 2.499999999999999556 ) ) ;
#77152 = CARTESIAN_POINT ( 'NONE',  ( 1.472469842513823179, 55.59226448433412315, -4.923371831947296329 ) ) ;
#77153 = CARTESIAN_POINT ( 'NONE',  ( 6.767445849361247490, 0.5000000000000004441, -13.38662304974496564 ) ) ;
#77154 = CARTESIAN_POINT ( 'NONE',  ( 15.44008868035555793, 21.39701867748817321, -9.422509992056140149 ) ) ;
#77155 = EDGE_CURVE ( 'NONE', #86532, #17162, #19370, .T. ) ;
#77157 = EDGE_LOOP ( 'NONE', ( #90996, #7426, #70157, #779 ) ) ;
#77156 = DIRECTION ( 'NONE',  ( 0.000000000000000000, 0.000000000000000000, -1.000000000000000000 ) ) ;
#77158 = AXIS2_PLACEMENT_3D ( 'NONE', #16924, #98973, #31897 ) ;
#77159 = DIRECTION ( 'NONE',  ( -0.000000000000000000, -1.000000000000000000, -0.000000000000000000 ) ) ;
#77160 = PRESENTATION_STYLE_ASSIGNMENT (( #8668 ) ) ;
#77161 = FILL_AREA_STYLE_COLOUR ( '', #43541 ) ;
#77162 = ORIENTED_EDGE ( 'NONE', *, *, #49690, .T. ) ;
#77163 = CARTESIAN_POINT ( 'NONE',  ( 2.933660812629996339, -0.03417435944610275333, -15.72485391577589731 ) ) ;
#77164 = CARTESIAN_POINT ( 'NONE',  ( 10.00000000000000000, 29.75893115100078745, -9.846743663894594434 ) ) ;
#77165 = CARTESIAN_POINT ( 'NONE',  ( 64.56412365047462742, 13.99999999999999467, -9.500000000000000000 ) ) ;
#77166 = CARTESIAN_POINT ( 'NONE',  ( 10.00000000000000000, 47.87363466993042493, -12.81628187352647608 ) ) ;
#77167 = B_SPLINE_CURVE_WITH_KNOTS ( 'NONE', 3,
 ( #79420, #59357, #65377, #36372 ),
 .UNSPECIFIED., .F., .F.,
 ( 4, 4 ),
 ( 1.110764993427085326E-17, 0.0003904528506838490006 ),
 .UNSPECIFIED. ) ;
#77168 = DIRECTION ( 'NONE',  ( 0.1736481776669272503, -0.9848077530122086864, 0.000000000000000000 ) ) ;
#77169 = ORIENTED_EDGE ( 'NONE', *, *, #87612, .F. ) ;
#77170 = CARTESIAN_POINT ( 'NONE',  ( 0.1532563361054100626, 65.80059781766745175, -2.638427012816831230 ) ) ;
#77171 = CARTESIAN_POINT ( 'NONE',  ( -14.17193700899788134, 15.00000000000000000, -1.489530601564206247 ) ) ;
#77172 = CARTESIAN_POINT ( 'NONE',  ( 5.076628168052704559, 60.17559781766745175, -8.527530157486179263 ) ) ;
#77173 = CARTESIAN_POINT ( 'NONE',  ( 24.16423886937410614, 44.30374883491397497, 8.672049930838204340E-16 ) ) ;
#77174 = CARTESIAN_POINT ( 'NONE',  ( 18.52753015748617571, 63.09226448433412315, 4.923371831947298993 ) ) ;
#77175 = CARTESIAN_POINT ( 'NONE',  ( -11.59608414876335658, 0.2306972965111898921, -9.421724210956444523 ) ) ;
#77176 = CARTESIAN_POINT ( 'NONE',  ( 19.84674366389459266, 13.30059781766745353, 2.638427012816836559 ) ) ;
#77177 = CARTESIAN_POINT ( 'NONE',  ( 10.00000000000000000, 52.87363466993041783, -12.81628187352647608 ) ) ;
#77178 = CARTESIAN_POINT ( 'NONE',  ( 2.791683348922237240, 55.38393115100078745, -7.208316651077763204 ) ) ;
#77179 = CARTESIAN_POINT ( 'NONE',  ( 12.91533473730992121, 49.52201867748817676, 10.88017736071110164 ) ) ;
#77180 = CARTESIAN_POINT ( 'NONE',  ( 20.15039907845753575, 39.72266099184919597, 6.262539305110075283 ) ) ;
#77181 = PRESENTATION_LAYER_ASSIGNMENT (  '', '', ( #21315 ) ) ;
#77182 = CIRCLE ( 'NONE', #45215, 0.2500000000000002220 ) ;
#77183 = ORIENTED_EDGE ( 'NONE', *, *, #63876, .F. ) ;
#77184 = LINE ( 'NONE', #39208, #18617 ) ;
#77185 = CARTESIAN_POINT ( 'NONE',  ( 4.559911319644449179, 33.89701867748817676, 9.422509992056141925 ) ) ;
#77187 = CARTESIAN_POINT ( 'NONE',  ( 15.44008868035555260, 59.73035201082151247, 9.422509992056143702 ) ) ;
#77186 = CARTESIAN_POINT ( 'NONE',  ( 21.09922568453594849, 6.206968003263753531, 6.408140936763242479 ) ) ;
#77188 = LINE ( 'NONE', #8696, #85584 ) ;
#77189 = CIRCLE ( 'NONE', #18176, 15.00000000000000000 ) ;
#77190 = CARTESIAN_POINT ( 'NONE',  ( 4.023424921641736596, 15.00000000000000000, -15.48190712851506667 ) ) ;
#77191 = CARTESIAN_POINT ( 'NONE',  ( 3.469446951953614189E-15, 3.912123368507817833, 11.92686044187656513 ) ) ;
#77192 = B_SPLINE_CURVE_WITH_KNOTS ( 'NONE', 3,
 ( #19851, #73837, #13342, #96369, #27842, #13842, #89827, #96867, #50344, #89340 ),
 .UNSPECIFIED., .F., .F.,
 ( 4, 3, 3, 4 ),
 ( -5.954425897502142659E-06, 0.000000000000000000, 6.576041642147462129E-05, 0.0001360868310503591421 ),
 .UNSPECIFIED. ) ;
#77194 = CARTESIAN_POINT ( 'NONE',  ( -11.62719953690071506, 0.5000000000000004441, 9.476720473301710967 ) ) ;
#77193 = CARTESIAN_POINT ( 'NONE',  ( 17.96484262340118221, 41.18868534415484106, -7.964842623401177768 ) ) ;
#77195 = CARTESIAN_POINT ( 'NONE',  ( 5.076628168052703671, 31.84226448433412315, 8.527530157486179263 ) ) ;
#77196 = CARTESIAN_POINT ( 'NONE',  ( 7.361572987183170547, 2.050597817667451750, 9.846743663894590881 ) ) ;
#77197 = CIRCLE ( 'NONE', #3774, 14.49999999999999822 ) ;
#77198 = CARTESIAN_POINT ( 'NONE',  ( -7.082119434687058401, 30.97041550158063927, -12.26659068614894110 ) ) ;
#77199 = CARTESIAN_POINT ( 'NONE',  ( 22.81628187352647785, 11.41530133659708390, 3.434112377981063169 ) ) ;
#77200 = CARTESIAN_POINT ( 'NONE',  ( 20.88017736071110875, 10.77201867748817143, -2.915334737309920765 ) ) ;
#77201 = CARTESIAN_POINT ( 'NONE',  ( 8.879999999999991900, 27.04366094290857347, 3.000000000000000000 ) ) ;
#77202 = CARTESIAN_POINT ( 'NONE',  ( 10.00000000000000178, 18.05374883491396787, 14.16423886937410082 ) ) ;
#77203 = EDGE_CURVE ( 'NONE', #38304, #49656, #50851, .T. ) ;
#77204 = CARTESIAN_POINT ( 'NONE',  ( 6.204703633549690345, 65.76208216824731778, -14.16423886937410259 ) ) ;
#77205 = CARTESIAN_POINT ( 'NONE',  ( 2.791683348922240793, 11.63393115100078568, 7.208316651077764092 ) ) ;
#77206 = SURFACE_SIDE_STYLE ('',( #46706 ) ) ;
#77207 = VERTEX_POINT ( 'NONE', #35346 ) ;
#77208 = CARTESIAN_POINT ( 'NONE',  ( 19.84674366389459621, 28.50893115100078745, 7.409399052514197653E-17 ) ) ;
#77209 = CARTESIAN_POINT ( 'NONE',  ( -0.8801773607110991993, 27.85535201082150181, -2.915334737309923874 ) ) ;
#77210 = CARTESIAN_POINT ( 'NONE',  ( 19.84674366389459266, 58.71726448433411605, -2.638427012816827677 ) ) ;
#77212 = CARTESIAN_POINT ( 'NONE',  ( 17.39651004071841456, 49.08210964143329136, -6.500000000000001776 ) ) ;
#77211 = CARTESIAN_POINT ( 'NONE',  ( 22.26659068614895176, 14.72041550158063572, -7.082119434687042414 ) ) ;
#77213 = DIRECTION ( 'NONE',  ( 1.000000000000000000, -1.257568779154408793E-17, 0.000000000000000000 ) ) ;
#77214 = UNCERTAINTY_MEASURE_WITH_UNIT (LENGTH_MEASURE( 1.000000000000000082E-05 ), #52287, 'distance_accuracy_value', 'NONE');
#77215 = CARTESIAN_POINT ( 'NONE',  ( 5.076628168052703671, 16.84226448433411960, 8.527530157486179263 ) ) ;
#77216 = CARTESIAN_POINT ( 'NONE',  ( 22.81628187352647785, 31.41530133659709279, 3.434112377981063169 ) ) ;
#77217 = CARTESIAN_POINT ( 'NONE',  ( 14.92337183194729988, 39.34226448433412315, -8.527530157486177487 ) ) ;
#77218 = EDGE_LOOP ( 'NONE', ( #75932, #17041, #34304, #34388 ) ) ;
#77219 = CARTESIAN_POINT ( 'NONE',  ( 2.791683348922237240, 15.38393115100078212, -7.208316651077763204 ) ) ;
#77220 = CARTESIAN_POINT ( 'NONE',  ( 19.50000000000000355, 79.40087001978915282, -5.000000000000000000 ) ) ;
#77221 = FACE_OUTER_BOUND ( 'NONE', #98363, .T. ) ;
#77222 = CARTESIAN_POINT ( 'NONE',  ( 17.08211943468705840, 60.13708216824729647, -12.26659068614894466 ) ) ;
#77223 = CARTESIAN_POINT ( 'NONE',  ( 9.898881779040660689, 15.00000000000000000, 10.25059215482582786 ) ) ;
#77224 = CARTESIAN_POINT ( 'NONE',  ( 19.42250999205614548, 55.98035201082150536, -5.440088680355545492 ) ) ;
#77225 = CARTESIAN_POINT ( 'NONE',  ( 19.84674366389459266, 33.71726448433410894, -2.638427012816827677 ) ) ;
#77226 = CARTESIAN_POINT ( 'NONE',  ( 15.44008868035555260, 19.73035201082150536, 9.422509992056143702 ) ) ;
#77227 =( NAMED_UNIT ( * ) PLANE_ANGLE_UNIT ( ) SI_UNIT ( $, .RADIAN. ) );
#77228 = CARTESIAN_POINT ( 'NONE',  ( 5.076628168052704559, 55.17559781766745175, -8.527530157486179263 ) ) ;
#77229 = CARTESIAN_POINT ( 'NONE',  ( 17.96484262340118221, 44.93868534415483396, 7.964842623401181321 ) ) ;
#77230 =( NAMED_UNIT ( * ) SI_UNIT ( $, .STERADIAN. ) SOLID_ANGLE_UNIT ( ) );
#77231 = ORIENTED_EDGE ( 'NONE', *, *, #28563, .T. ) ;
#77232 = ORIENTED_EDGE ( 'NONE', *, *, #59426, .F. ) ;
#77233 = CARTESIAN_POINT ( 'NONE',  ( 19.50000000000000711, 105.0000000000000000, -5.000000000000000000 ) ) ;
#77235 = EDGE_CURVE ( 'NONE', #34058, #35670, #12840, .T. ) ;
#77234 = FILL_AREA_STYLE_COLOUR ( '', #58779 ) ;
#77236 = CARTESIAN_POINT ( 'NONE',  ( 1.472469842513823179, 46.42559781766745175, 4.923371831947296329 ) ) ;
#77237 = CARTESIAN_POINT ( 'NONE',  ( 14.92337183194729633, 17.67559781766745175, 8.527530157486181039 ) ) ;
#77238 = CARTESIAN_POINT ( 'NONE',  ( -2.816281873526473856, 59.12363466993042493, 9.499525473075851096E-16 ) ) ;
#77240 = CARTESIAN_POINT ( 'NONE',  ( 14.92337183194729633, 52.67559781766745175, 8.527530157486181039 ) ) ;
#77239 = CARTESIAN_POINT ( 'NONE',  ( 17.96484262340118221, 16.18868534415483396, -7.964842623401177768 ) ) ;
#77241 = FACE_OUTER_BOUND ( 'NONE', #2037, .T. ) ;
#77242 = CARTESIAN_POINT ( 'NONE',  ( 24.16423886937410614, 54.51208216824730357, -3.795296366450302550 ) ) ;
#77243 = CARTESIAN_POINT ( 'NONE',  ( 18.52753015748617571, 63.09226448433412315, 4.923371831947298993 ) ) ;
#77244 = DIRECTION ( 'NONE',  ( 0.000000000000000000, 1.000000000000000000, 0.000000000000000000 ) ) ;
#77245 = CARTESIAN_POINT ( 'NONE',  ( 2.035157376598824452, 48.68868534415483396, 7.964842623401179544 ) ) ;
#77246 = EDGE_CURVE ( 'NONE', #32363, #80599, #44955, .T. ) ;
#77247 = CARTESIAN_POINT ( 'NONE',  ( 10.00000000000000000, 14.75893115100078568, -9.846743663894594434 ) ) ;
#77248 = LINE ( 'NONE', #39273, #82901 ) ;
#77249 = ORIENTED_EDGE ( 'NONE', *, *, #48768, .T. ) ;
#77250 = CARTESIAN_POINT ( 'NONE',  ( 0.000000000000000000, 0.5000000000000000000, 6.000000000000000000 ) ) ;
#77251 = ORIENTED_EDGE ( 'NONE', *, *, #96753, .F. ) ;
#77252 = CARTESIAN_POINT ( 'NONE',  ( 7.361572987183170547, 12.05059781766744997, 9.846743663894590881 ) ) ;
#77253 = ORIENTED_EDGE ( 'NONE', *, *, #88394, .F. ) ;
#77254 = CARTESIAN_POINT ( 'NONE',  ( 24.16423886937409904, 14.09541550158063217, 3.795296366450317205 ) ) ;
#77255 = CARTESIAN_POINT ( 'NONE',  ( 2.791683348922240793, 16.63393115100078745, 7.208316651077764092 ) ) ;
#77256 = CARTESIAN_POINT ( 'NONE',  ( 10.00000000000000178, 39.31368534415484106, 10.88017736071110342 ) ) ;
#77257 = ORIENTED_EDGE ( 'NONE', *, *, #21078, .T. ) ;
#77258 = CARTESIAN_POINT ( 'NONE',  ( 2.035157376598824452, 28.68868534415484106, 7.964842623401179544 ) ) ;
#77259 = PRESENTATION_LAYER_ASSIGNMENT (  '', '', ( #56498 ) ) ;
#77260 = ORIENTED_EDGE ( 'NONE', *, *, #14357, .T. ) ;
#77261 = CARTESIAN_POINT ( 'NONE',  ( 2.917880565312950480, 5.970415501580634832, -12.26659068614894821 ) ) ;
#77262 = VECTOR ( 'NONE', #23613, 1000.000000000000000 ) ;
#77263 = ORIENTED_EDGE ( 'NONE', *, *, #88187, .F. ) ;
#77264 = CARTESIAN_POINT ( 'NONE',  ( -2.816281873526471635, 23.91530133659708568, -3.434112377981056508 ) ) ;
#77265 = CARTESIAN_POINT ( 'NONE',  ( 0.1532563361054083140, 16.00893115100078390, 1.131784320476157264E-15 ) ) ;
#77266 = DIRECTION ( 'NONE',  ( 0.1132032137679039180, 0.000000000000000000, 0.9935718556765877896 ) ) ;
#77267 = LINE ( 'NONE', #24784, #43164 ) ;
#77268 = CARTESIAN_POINT ( 'NONE',  ( 10.00000000000000178, 12.25893115100078568, 9.846743663894594434 ) ) ;
#77269 = CARTESIAN_POINT ( 'NONE',  ( 2.035157376598822676, 27.43868534415483396, -7.964842623401177768 ) ) ;
#77270 = EDGE_CURVE ( 'NONE', #88314, #79187, #28824, .T. ) ;
#77271 = ORIENTED_EDGE ( 'NONE', *, *, #456, .F. ) ;
#77272 = ORIENTED_EDGE ( 'NONE', *, *, #21286, .F. ) ;
#77273 = DIRECTION ( 'NONE',  ( 3.375077994860475883E-14, 0.000000000000000000, 1.000000000000000000 ) ) ;
#77274 = CARTESIAN_POINT ( 'NONE',  ( 7.084665262690076126, 57.02201867748817676, -10.88017736071110164 ) ) ;
#77275 = CARTESIAN_POINT ( 'NONE',  ( 1.274849032794116210, 8.572280503510292249, 6.499999999999738876 ) ) ;
#77276 = CARTESIAN_POINT ( 'NONE',  ( 0.6178305044545818747, 63.49863466993043204, -9.382169495545419124 ) ) ;
#77277 = CARTESIAN_POINT ( 'NONE',  ( 17.96484262340118221, 66.18868534415483396, -7.964842623401177768 ) ) ;
#77278 = CARTESIAN_POINT ( 'NONE',  ( 18.52753015748618282, 63.92559781766745886, -4.923371831947291888 ) ) ;
#77279 = CARTESIAN_POINT ( 'NONE',  ( 20.15039907845753930, 70.00000000000000000, 6.262539305110068177 ) ) ;
#77280 = ADVANCED_FACE ( 'NONE', ( #5848 ), #36339, .F. ) ;
#77281 = CARTESIAN_POINT ( 'NONE',  ( 7.361572987183170547, 27.05059781766745175, 9.846743663894590881 ) ) ;
#77282 = CARTESIAN_POINT ( 'NONE',  ( 16.40814093676323893, 55.79030133659708923, 11.09922568453595026 ) ) ;
#77283 = CARTESIAN_POINT ( 'NONE',  ( 4.395798237819382059, -0.8372147401281977430, -3.750000000000000444 ) ) ;
#77284 = CARTESIAN_POINT ( 'NONE',  ( 0.1532563361054100626, 15.80059781766745353, -2.638427012816831230 ) ) ;
#77285 =( BOUNDED_SURFACE ( )  B_SPLINE_SURFACE ( 1, 2, ( 
 ( #17059, #25059, #85547, #17554, #64490, #55028, #10043, #55543, #26029, #39562, #32532, #79018, #24567, #3530, #47037, #94998, #86041, #94509, #40544, #78532, #26505, #87012, #77533, #56038, #62528, #33023, #71044, #2567, #63520, #47540, #41039, #3046, #9541, #94024, #9050, #33500, #33989, #18036, #71539, #70052, #48515, #93032, #25546, #63030, #10528, #40045, #70545, #18521, #2070, #93528, #56522, #49012, #79518, #11019, #72003, #85049, #16563, #1575, #32024, #80988, #49494, #58473, #4515, #13479, #5987, #35482, #26996, #66474, #80503, #57494, #87989, #36480, #95504, #19501, #97003, #65977, #34980, #66973, #58975, #20491, #42025, #50489, #88986, #50978, #96503, #97492, #28479, #57002, #12488, #49996, #81473, #27977, #12976, #73973, #12000, #89474, #19989, #42989, #43471, #19017, #87503, #27486, #5499, #73471, #42503, #43959, #5000, #35973, #51474, #79999, #11503, #96004, #20989, #81965, #74460, #72490, #4023, #65479, #72986, #34485, #64980, #57979, #88486, #98489, #69437, #28958, #67469, #7960, #13985, #21984, #59953, #97990, #91937, #22468, #68462, #29945, #67966, #53941, #98984, #29446, #83455, #89962, #30436, #6465, #75950, #14977, #60449, #90940, #90444, #83947, #45956, #52458, #45447, #21478, #76444, #76930, #60937, #15473, #51978, #91446, #36972, #52945, #6969, #7476, #82962, #14478, #61429, #44951, #75455, #68951, #38456, #37476, #37973, #22971, #8440, #53438, #482, #59461, #30929, #82464, #23466, #84448, #15945, #38946, #46437, #44459, #74962, #24442, #1454, #31906, #48886, #39442, #62406, #10411, #9924, #47411, #10903, #2934, #63399, #84930, #93411, #2444, #93905, #78405, #79398, #71418, #957, #55416, #92913, #32900, #70924, #40428, #17915, #69935, #33381, #62909, #24934, #25431, #61921, #41425, #70427, #55915, #85923, #85422, #86894, #17433, #78902, #94390, #92424, #31418, #39925, #47901, #86414, #48399, #40918, #18404, #77913, #54909, #63878, #25906, #16932, #56408, #1946, #23949, #54419, #9422, #16442, #46918, #32408, #77411, #8926, #35856, #65359, #12369, #42385, #11882, #96883, #42875, #11387, #27368, #89355, #33868, #51356, #72862, #81358, #57861, #34866, #81841, #73852, #88372, #20865, #64375, #13355, #4397, #12856, #19867, #95888, #71886, #5382, #94884, #73358, #49380, #50362, #80871, #4885, #35363, #41908, #27856, #88863, #72370, #65856, #26383, #20372, #3406, #96384, #58343, #56882, #50866, #79881, #43354, #49868, #66345, #3901, #26880, #28360, #34369, #64859, #58849, #87385, #80381, #18903, #95379, #57373, #87868, #19384, #84337, #67850, #36354, #45332, #90323, #366, #91825, #22353, #13858, #53321 ),
 ( #21861, #60334, #60820, #6344, #52341, #75332, #98368, #91319, #52828, #29332, #45840, #68835, #66850, #14859, #29824, #82836, #75831, #90827, #37853, #83335, #23343, #97369, #44826, #83828, #14356, #6845, #36855, #30814, #7352, #37357, #28837, #44338, #74843, #61313, #68343, #98864, #30318, #22847, #51850, #21357, #15355, #76324, #7843, #82338, #38340, #53825, #43840, #59830, #67346, #74336, #5861, #59339, #89842, #97872, #47290, #2325, #33268, #55797, #46806, #93290, #77298, #69323, #61804, #24326, #63762, #40795, #92798, #85307, #9302, #24814, #63278, #40301, #54790, #70809, #2816, #32779, #94269, #55290, #16813, #32284, #93782, #8811, #77792, #39812, #70314, #25312, #85800, #1342, #17800, #71297, #8326, #17313, #1831, #62790, #47789, #78287, #9802, #86292, #25792, #38830, #48276, #78789, #62291, #10296, #39323, #56289, #15839, #46324, #844, #84816, #16322, #76811, #31303, #92311, #23837, #54302, #69818, #31793, #49745, #11759, #4765, #26266, #42267, #80254, #19752, #72255, #56765, #88739, #80752, #20250, #5259, #35738, #19261, #73236, #66226, #27738, #18783, #65234, #49266, #41302, #33749, #79766, #35236, #71775, #72737, #95759, #27244, #58220, #41783, #26757, #3786, #12736, #11264, #57251, #87261, #4271, #96760, #34241, #34743, #87747, #50751, #3285, #64739, #12247, #95252, #57741, #18287, #42754, #65733, #81237, #88243, #50237, #43234, #73730, #96260, #28236, #86785, #94766, #48769, #79276, #10783, #64249, #67229, #30199, #60702, #51738, #68232, #51235, #81720, #97257, #37730, #89722, #97752, #59218, #90211, #38224, #28727, #82717, #29216, #98749, #13233, #6235, #52711, #21237, #37241, #89235, #83217, #7226, #53209, #82221, #36737, #15232, #91199, #13734, #29706, #14236, #66733, #59716, #76213, #68710, #21743, #52225, #22726, #83712, #44218, #45713, #43729, #74215, #74722, #7728, #44716, #242, #58731, #75214, #6726, #67731, #98247, #20744, #14740, #60215, #45214, #5747, #75713, #36237, #90709, #22234, #62168, #3064, #732, #8690, #39205, #1223, #33518, #24201, #54182, #87025, #79534, #91706, #18052, #31676, #69691, #10543, #92674, #41053, #54668, #34010, #23225, #85186, #26046, #84696, #48529, #31186, #11034, #71552, #64014, #53696, #38708, #69207, #41556, #94526, #56536, #18537, #49028, #76693, #8214, #72020, #64507, #30690, #61680, #61198, #15725, #92197, #37074, #90057, #54876, #45548, #16900, #39891, #70394, #52553, #38063, #62876, #62372, #82563, #30040, #14079, #36579, #97593, #44559, #68555, #29054, #83057, #60548, #91041, #92876, #75056, #22078, #98084, #9387, #29542, #75554, #21580, #7070, #82062, #37572 ) ),
 .UNSPECIFIED., .F., .F., .F. ) 
 B_SPLINE_SURFACE_WITH_KNOTS ( ( 2, 2 ),
 ( 3, 2, 2, 2, 2, 2, 2, 2, 2, 2, 2, 2, 2, 2, 2, 2, 2, 2, 2, 2, 2, 2, 2, 2, 2, 2, 2, 2, 2, 2, 2, 2, 2, 2, 2, 2, 2, 2, 2, 2, 2, 2, 2, 2, 2, 2, 2, 2, 2, 2, 2, 2, 2, 2, 2, 2, 2, 2, 2, 2, 2, 2, 2, 2, 2, 2, 2, 2, 2, 2, 2, 2, 2, 2, 2, 2, 2, 2, 2, 2, 2, 2, 2, 2, 2, 2, 2, 2, 2, 2, 2, 2, 2, 2, 2, 2, 2, 2, 2, 2, 2, 2, 2, 2, 2, 2, 2, 2, 2, 2, 2, 2, 2, 2, 2, 2, 2, 2, 2, 2, 2, 2, 2, 2, 2, 2, 2, 2, 2, 2, 2, 2, 2, 2, 2, 2, 2, 2, 2, 2, 2, 2, 2, 2, 2, 2, 2, 2, 2, 2, 2, 2, 2, 2, 2, 2, 2, 2, 2, 2, 2, 2, 3 ),
 ( 0.000000000000000000, 1.000000000000000000 ),
 ( 0.000000000000000000, 0.005952380952380952051, 0.01190476190476190410, 0.01785714285714285615, 0.02380952380952380820, 0.02976190476190476025, 0.03571428571428571230, 0.04166666666666666435, 0.04761904761904761640, 0.05357142857142856845, 0.05952380952380952051, 0.06547619047619047949, 0.07142857142857142461, 0.07738095238095238360, 0.08333333333333332871, 0.08928571428571428770, 0.09523809523809523281, 0.1011904761904761918, 0.1071428571428571369, 0.1130952380952380959, 0.1190476190476190410, 0.1250000000000000000, 0.1309523809523809590, 0.1369047619047619180, 0.1428571428571428492, 0.1488095238095238082, 0.1547619047619047672, 0.1607142857142857262, 0.1666666666666666574, 0.1726190476190476164, 0.1785714285714285754, 0.1845238095238095344, 0.1904761904761904656, 0.1964285714285714246, 0.2023809523809523836, 0.2083333333333333426, 0.2142857142857142738, 0.2202380952380952328, 0.2261904761904761918, 0.2321428571428571508, 0.2380952380952380820, 0.2440476190476190410, 0.2500000000000000000, 0.2559523809523809312, 0.2619047619047619180, 0.2678571428571428492, 0.2738095238095238360, 0.2797619047619047672, 0.2857142857142856984, 0.2916666666666666852, 0.2976190476190476164, 0.3035714285714285476, 0.3095238095238095344, 0.3154761904761904656, 0.3214285714285714524, 0.3273809523809523836, 0.3333333333333333148, 0.3392857142857143016, 0.3452380952380952328, 0.3511904761904761640, 0.3571428571428571508, 0.3630952380952380820, 0.3690476190476190688, 0.3750000000000000000, 0.3809523809523809312, 0.3869047619047619180, 0.3928571428571428492, 0.3988095238095238360, 0.4047619047619047672, 0.4107142857142856984, 0.4166666666666666852, 0.4226190476190476164, 0.4285714285714285476, 0.4345238095238095344, 0.4404761904761904656, 0.4464285714285714524, 0.4523809523809523836, 0.4583333333333333148, 0.4642857142857143016, 0.4702380952380952328, 0.4761904761904761640, 0.4821428571428571508, 0.4880952380952380820, 0.4940476190476190688, 0.5000000000000000000, 0.5059523809523809312, 0.5119047619047618625, 0.5178571428571429047, 0.5238095238095238360, 0.5297619047619047672, 0.5357142857142856984, 0.5416666666666666297, 0.5476190476190476719, 0.5535714285714286031, 0.5595238095238095344, 0.5654761904761904656, 0.5714285714285713969, 0.5773809523809523281, 0.5833333333333333703, 0.5892857142857143016, 0.5952380952380952328, 0.6011904761904761640, 0.6071428571428570953, 0.6130952380952381375, 0.6190476190476190688, 0.6250000000000000000, 0.6309523809523809312, 0.6369047619047618625, 0.6428571428571429047, 0.6488095238095238360, 0.6547619047619047672, 0.6607142857142856984, 0.6666666666666666297, 0.6726190476190476719, 0.6785714285714286031, 0.6845238095238095344, 0.6904761904761904656, 0.6964285714285713969, 0.7023809523809523281, 0.7083333333333333703, 0.7142857142857143016, 0.7202380952380952328, 0.7261904761904761640, 0.7321428571428570953, 0.7380952380952381375, 0.7440476190476190688, 0.7500000000000000000, 0.7559523809523809312, 0.7619047619047618625, 0.7678571428571429047, 0.7738095238095238360, 0.7797619047619047672, 0.7857142857142856984, 0.7916666666666666297, 0.7976190476190476719, 0.8035714285714286031, 0.8095238095238095344, 0.8154761904761904656, 0.8214285714285713969, 0.8273809523809523281, 0.8333333333333333703, 0.8392857142857143016, 0.8452380952380952328, 0.8511904761904761640, 0.8571428571428570953, 0.8630952380952381375, 0.8690476190476190688, 0.8750000000000000000, 0.8809523809523809312, 0.8869047619047618625, 0.8928571428571429047, 0.8988095238095238360, 0.9047619047619047672, 0.9107142857142856984, 0.9166666666666666297, 0.9226190476190476719, 0.9285714285714286031, 0.9345238095238095344, 0.9404761904761904656, 0.9464285714285713969, 0.9523809523809523281, 0.9583333333333333703, 0.9642857142857143016 ),
 .UNSPECIFIED. ) 
 GEOMETRIC_REPRESENTATION_ITEM ( )  RATIONAL_B_SPLINE_SURFACE ( (
 ( 1.000000000000000000, 0.9659258262890683122, 1.000000000000000000, 0.9659258262890683122, 1.000000000000000000, 0.9659258262890683122, 1.000000000000000000, 0.9659258262890683122, 1.000000000000000000, 0.9659258262890683122, 1.000000000000000000, 0.9659258262890683122, 1.000000000000000000, 0.9659258262890683122, 1.000000000000000000, 0.9659258262890683122, 1.000000000000000000, 0.9659258262890683122, 1.000000000000000000, 0.9659258262890683122, 1.000000000000000000, 0.9659258262890683122, 1.000000000000000000, 0.9659258262890683122, 1.000000000000000000, 0.9659258262890683122, 1.000000000000000000, 0.9659258262890683122, 1.000000000000000000, 0.9659258262890683122, 1.000000000000000000, 0.9659258262890683122, 1.000000000000000000, 0.9659258262890683122, 1.000000000000000000, 0.9659258262890683122, 1.000000000000000000, 0.9659258262890683122, 1.000000000000000000, 0.9659258262890683122, 1.000000000000000000, 0.9659258262890683122, 1.000000000000000000, 0.9659258262890683122, 1.000000000000000000, 0.9659258262890683122, 1.000000000000000000, 0.9659258262890683122, 1.000000000000000000, 0.9659258262890683122, 1.000000000000000000, 0.9659258262890683122, 1.000000000000000000, 0.9659258262890683122, 1.000000000000000000, 0.9659258262890683122, 1.000000000000000000, 0.9659258262890683122, 1.000000000000000000, 0.9659258262890683122, 1.000000000000000000, 0.9659258262890683122, 1.000000000000000000, 0.9659258262890683122, 1.000000000000000000, 0.9659258262890683122, 1.000000000000000000, 0.9659258262890683122, 1.000000000000000000, 0.9659258262890683122, 1.000000000000000000, 0.9659258262890683122, 1.000000000000000000, 0.9659258262890683122, 1.000000000000000000, 0.9659258262890683122, 1.000000000000000000, 0.9659258262890683122, 1.000000000000000000, 0.9659258262890683122, 1.000000000000000000, 0.9659258262890683122, 1.000000000000000000, 0.9659258262890683122, 1.000000000000000000, 0.9659258262890683122, 1.000000000000000000, 0.9659258262890683122, 1.000000000000000000, 0.9659258262890683122, 1.000000000000000000, 0.9659258262890683122, 1.000000000000000000, 0.9659258262890683122, 1.000000000000000000, 0.9659258262890683122, 1.000000000000000000, 0.9659258262890683122, 1.000000000000000000, 0.9659258262890683122, 1.000000000000000000, 0.9659258262890683122, 1.000000000000000000, 0.9659258262890683122, 1.000000000000000000, 0.9659258262890683122, 1.000000000000000000, 0.9659258262890683122, 1.000000000000000000, 0.9659258262890683122, 1.000000000000000000, 0.9659258262890683122, 1.000000000000000000, 0.9659258262890683122, 1.000000000000000000, 0.9659258262890683122, 1.000000000000000000, 0.9659258262890683122, 1.000000000000000000, 0.9659258262890683122, 1.000000000000000000, 0.9659258262890683122, 1.000000000000000000, 0.9659258262890683122, 1.000000000000000000, 0.9659258262890683122, 1.000000000000000000, 0.9659258262890683122, 1.000000000000000000, 0.9659258262890683122, 1.000000000000000000, 0.9659258262890683122, 1.000000000000000000, 0.9659258262890683122, 1.000000000000000000, 0.9659258262890683122, 1.000000000000000000, 0.9659258262890683122, 1.000000000000000000, 0.9659258262890683122, 1.000000000000000000, 0.9659258262890683122, 1.000000000000000000, 0.9659258262890683122, 1.000000000000000000, 0.9659258262890683122, 1.000000000000000000, 0.9659258262890683122, 1.000000000000000000, 0.9659258262890683122, 1.000000000000000000, 0.9659258262890683122, 1.000000000000000000, 0.9659258262890683122, 1.000000000000000000, 0.9659258262890683122, 1.000000000000000000, 0.9659258262890683122, 1.000000000000000000, 0.9659258262890683122, 1.000000000000000000, 0.9659258262890683122, 1.000000000000000000, 0.9659258262890683122, 1.000000000000000000, 0.9659258262890683122, 1.000000000000000000, 0.9659258262890683122, 1.000000000000000000, 0.9659258262890683122, 1.000000000000000000, 0.9659258262890683122, 1.000000000000000000, 0.9659258262890683122, 1.000000000000000000, 0.9659258262890683122, 1.000000000000000000, 0.9659258262890683122, 1.000000000000000000, 0.9659258262890683122, 1.000000000000000000, 0.9659258262890683122, 1.000000000000000000, 0.9659258262890683122, 1.000000000000000000, 0.9659258262890683122, 1.000000000000000000, 0.9659258262890683122, 1.000000000000000000, 0.9659258262890683122, 1.000000000000000000, 0.9659258262890683122, 1.000000000000000000, 0.9659258262890683122, 1.000000000000000000, 0.9659258262890683122, 1.000000000000000000, 0.9659258262890683122, 1.000000000000000000, 0.9659258262890683122, 1.000000000000000000, 0.9659258262890683122, 1.000000000000000000, 0.9659258262890683122, 1.000000000000000000, 0.9659258262890683122, 1.000000000000000000, 0.9659258262890683122, 1.000000000000000000, 0.9659258262890683122, 1.000000000000000000, 0.9659258262890683122, 1.000000000000000000, 0.9659258262890683122, 1.000000000000000000, 0.9659258262890683122, 1.000000000000000000, 0.9659258262890683122, 1.000000000000000000, 0.9659258262890683122, 1.000000000000000000, 0.9659258262890683122, 1.000000000000000000, 0.9659258262890683122, 1.000000000000000000, 0.9659258262890683122, 1.000000000000000000, 0.9659258262890683122, 1.000000000000000000, 0.9659258262890683122, 1.000000000000000000, 0.9659258262890683122, 1.000000000000000000, 0.9659258262890683122, 1.000000000000000000, 0.9659258262890683122, 1.000000000000000000, 0.9659258262890683122, 1.000000000000000000, 0.9659258262890683122, 1.000000000000000000, 0.9659258262890683122, 1.000000000000000000, 0.9659258262890683122, 1.000000000000000000, 0.9659258262890683122, 1.000000000000000000, 0.9659258262890683122, 1.000000000000000000, 0.9659258262890683122, 1.000000000000000000, 0.9659258262890683122, 1.000000000000000000, 0.9659258262890683122, 1.000000000000000000, 0.9659258262890683122, 1.000000000000000000, 0.9659258262890683122, 1.000000000000000000, 0.9659258262890683122, 1.000000000000000000, 0.9659258262890683122, 1.000000000000000000, 0.9659258262890683122, 1.000000000000000000, 0.9659258262890683122, 1.000000000000000000, 0.9659258262890683122, 1.000000000000000000, 0.9659258262890683122, 1.000000000000000000, 0.9659258262890683122, 1.000000000000000000, 0.9659258262890683122, 1.000000000000000000, 0.9659258262890683122, 1.000000000000000000, 0.9659258262890683122, 1.000000000000000000, 0.9659258262890683122, 1.000000000000000000, 0.9659258262890683122, 1.000000000000000000, 0.9659258262890683122, 1.000000000000000000, 0.9659258262890683122, 1.000000000000000000, 0.9659258262890683122, 1.000000000000000000, 0.9659258262890683122, 1.000000000000000000, 0.9659258262890683122, 1.000000000000000000, 0.9659258262890683122, 1.000000000000000000, 0.9659258262890683122, 1.000000000000000000, 0.9659258262890683122, 1.000000000000000000, 0.9659258262890683122, 1.000000000000000000, 0.9659258262890683122, 1.000000000000000000, 0.9659258262890683122, 1.000000000000000000, 0.9659258262890683122, 1.000000000000000000, 0.9659258262890683122, 1.000000000000000000, 0.9659258262890683122, 1.000000000000000000, 0.9659258262890683122, 1.000000000000000000, 0.9659258262890683122, 1.000000000000000000, 0.9659258262890683122, 1.000000000000000000, 0.9659258262890683122, 1.000000000000000000, 0.9659258262890683122, 1.000000000000000000, 0.9659258262890683122, 1.000000000000000000, 0.9659258262890683122, 1.000000000000000000),
 ( 1.000000000000000000, 0.9659258262890683122, 1.000000000000000000, 0.9659258262890683122, 1.000000000000000000, 0.9659258262890683122, 1.000000000000000000, 0.9659258262890683122, 1.000000000000000000, 0.9659258262890683122, 1.000000000000000000, 0.9659258262890683122, 1.000000000000000000, 0.9659258262890683122, 1.000000000000000000, 0.9659258262890683122, 1.000000000000000000, 0.9659258262890683122, 1.000000000000000000, 0.9659258262890683122, 1.000000000000000000, 0.9659258262890683122, 1.000000000000000000, 0.9659258262890683122, 1.000000000000000000, 0.9659258262890683122, 1.000000000000000000, 0.9659258262890683122, 1.000000000000000000, 0.9659258262890683122, 1.000000000000000000, 0.9659258262890683122, 1.000000000000000000, 0.9659258262890683122, 1.000000000000000000, 0.9659258262890683122, 1.000000000000000000, 0.9659258262890683122, 1.000000000000000000, 0.9659258262890683122, 1.000000000000000000, 0.9659258262890683122, 1.000000000000000000, 0.9659258262890683122, 1.000000000000000000, 0.9659258262890683122, 1.000000000000000000, 0.9659258262890683122, 1.000000000000000000, 0.9659258262890683122, 1.000000000000000000, 0.9659258262890683122, 1.000000000000000000, 0.9659258262890683122, 1.000000000000000000, 0.9659258262890683122, 1.000000000000000000, 0.9659258262890683122, 1.000000000000000000, 0.9659258262890683122, 1.000000000000000000, 0.9659258262890683122, 1.000000000000000000, 0.9659258262890683122, 1.000000000000000000, 0.9659258262890683122, 1.000000000000000000, 0.9659258262890683122, 1.000000000000000000, 0.9659258262890683122, 1.000000000000000000, 0.9659258262890683122, 1.000000000000000000, 0.9659258262890683122, 1.000000000000000000, 0.9659258262890683122, 1.000000000000000000, 0.9659258262890683122, 1.000000000000000000, 0.9659258262890683122, 1.000000000000000000, 0.9659258262890683122, 1.000000000000000000, 0.9659258262890683122, 1.000000000000000000, 0.9659258262890683122, 1.000000000000000000, 0.9659258262890683122, 1.000000000000000000, 0.9659258262890683122, 1.000000000000000000, 0.9659258262890683122, 1.000000000000000000, 0.9659258262890683122, 1.000000000000000000, 0.9659258262890683122, 1.000000000000000000, 0.9659258262890683122, 1.000000000000000000, 0.9659258262890683122, 1.000000000000000000, 0.9659258262890683122, 1.000000000000000000, 0.9659258262890683122, 1.000000000000000000, 0.9659258262890683122, 1.000000000000000000, 0.9659258262890683122, 1.000000000000000000, 0.9659258262890683122, 1.000000000000000000, 0.9659258262890683122, 1.000000000000000000, 0.9659258262890683122, 1.000000000000000000, 0.9659258262890683122, 1.000000000000000000, 0.9659258262890683122, 1.000000000000000000, 0.9659258262890683122, 1.000000000000000000, 0.9659258262890683122, 1.000000000000000000, 0.9659258262890683122, 1.000000000000000000, 0.9659258262890683122, 1.000000000000000000, 0.9659258262890683122, 1.000000000000000000, 0.9659258262890683122, 1.000000000000000000, 0.9659258262890683122, 1.000000000000000000, 0.9659258262890683122, 1.000000000000000000, 0.9659258262890683122, 1.000000000000000000, 0.9659258262890683122, 1.000000000000000000, 0.9659258262890683122, 1.000000000000000000, 0.9659258262890683122, 1.000000000000000000, 0.9659258262890683122, 1.000000000000000000, 0.9659258262890683122, 1.000000000000000000, 0.9659258262890683122, 1.000000000000000000, 0.9659258262890683122, 1.000000000000000000, 0.9659258262890683122, 1.000000000000000000, 0.9659258262890683122, 1.000000000000000000, 0.9659258262890683122, 1.000000000000000000, 0.9659258262890683122, 1.000000000000000000, 0.9659258262890683122, 1.000000000000000000, 0.9659258262890683122, 1.000000000000000000, 0.9659258262890683122, 1.000000000000000000, 0.9659258262890683122, 1.000000000000000000, 0.9659258262890683122, 1.000000000000000000, 0.9659258262890683122, 1.000000000000000000, 0.9659258262890683122, 1.000000000000000000, 0.9659258262890683122, 1.000000000000000000, 0.9659258262890683122, 1.000000000000000000, 0.9659258262890683122, 1.000000000000000000, 0.9659258262890683122, 1.000000000000000000, 0.9659258262890683122, 1.000000000000000000, 0.9659258262890683122, 1.000000000000000000, 0.9659258262890683122, 1.000000000000000000, 0.9659258262890683122, 1.000000000000000000, 0.9659258262890683122, 1.000000000000000000, 0.9659258262890683122, 1.000000000000000000, 0.9659258262890683122, 1.000000000000000000, 0.9659258262890683122, 1.000000000000000000, 0.9659258262890683122, 1.000000000000000000, 0.9659258262890683122, 1.000000000000000000, 0.9659258262890683122, 1.000000000000000000, 0.9659258262890683122, 1.000000000000000000, 0.9659258262890683122, 1.000000000000000000, 0.9659258262890683122, 1.000000000000000000, 0.9659258262890683122, 1.000000000000000000, 0.9659258262890683122, 1.000000000000000000, 0.9659258262890683122, 1.000000000000000000, 0.9659258262890683122, 1.000000000000000000, 0.9659258262890683122, 1.000000000000000000, 0.9659258262890683122, 1.000000000000000000, 0.9659258262890683122, 1.000000000000000000, 0.9659258262890683122, 1.000000000000000000, 0.9659258262890683122, 1.000000000000000000, 0.9659258262890683122, 1.000000000000000000, 0.9659258262890683122, 1.000000000000000000, 0.9659258262890683122, 1.000000000000000000, 0.9659258262890683122, 1.000000000000000000, 0.9659258262890683122, 1.000000000000000000, 0.9659258262890683122, 1.000000000000000000, 0.9659258262890683122, 1.000000000000000000, 0.9659258262890683122, 1.000000000000000000, 0.9659258262890683122, 1.000000000000000000, 0.9659258262890683122, 1.000000000000000000, 0.9659258262890683122, 1.000000000000000000, 0.9659258262890683122, 1.000000000000000000, 0.9659258262890683122, 1.000000000000000000, 0.9659258262890683122, 1.000000000000000000, 0.9659258262890683122, 1.000000000000000000, 0.9659258262890683122, 1.000000000000000000, 0.9659258262890683122, 1.000000000000000000, 0.9659258262890683122, 1.000000000000000000, 0.9659258262890683122, 1.000000000000000000, 0.9659258262890683122, 1.000000000000000000, 0.9659258262890683122, 1.000000000000000000, 0.9659258262890683122, 1.000000000000000000, 0.9659258262890683122, 1.000000000000000000, 0.9659258262890683122, 1.000000000000000000, 0.9659258262890683122, 1.000000000000000000, 0.9659258262890683122, 1.000000000000000000, 0.9659258262890683122, 1.000000000000000000, 0.9659258262890683122, 1.000000000000000000, 0.9659258262890683122, 1.000000000000000000, 0.9659258262890683122, 1.000000000000000000, 0.9659258262890683122, 1.000000000000000000, 0.9659258262890683122, 1.000000000000000000, 0.9659258262890683122, 1.000000000000000000, 0.9659258262890683122, 1.000000000000000000, 0.9659258262890683122, 1.000000000000000000, 0.9659258262890683122, 1.000000000000000000, 0.9659258262890683122, 1.000000000000000000, 0.9659258262890683122, 1.000000000000000000, 0.9659258262890683122, 1.000000000000000000, 0.9659258262890683122, 1.000000000000000000, 0.9659258262890683122, 1.000000000000000000, 0.9659258262890683122, 1.000000000000000000, 0.9659258262890683122, 1.000000000000000000, 0.9659258262890683122, 1.000000000000000000, 0.9659258262890683122, 1.000000000000000000, 0.9659258262890683122, 1.000000000000000000, 0.9659258262890683122, 1.000000000000000000, 0.9659258262890683122, 1.000000000000000000, 0.9659258262890683122, 1.000000000000000000) ) ) 
 REPRESENTATION_ITEM ( '' )  SURFACE ( )  );
#77286 = CARTESIAN_POINT ( 'NONE',  ( 3.591859063236763294, 23.29030133659708568, -11.09922568453595026 ) ) ;
#77288 = DIRECTION ( 'NONE',  ( 0.000000000000000000, 1.000000000000000000, 0.000000000000000000 ) ) ;
#77287 = CARTESIAN_POINT ( 'NONE',  ( 14.76044511231851075, 0.2301501264598460050, 2.313329003772481851 ) ) ;
#77289 = CARTESIAN_POINT ( 'NONE',  ( 17.96484262340118221, 54.93868534415484106, 7.964842623401181321 ) ) ;
#77290 = CARTESIAN_POINT ( 'NONE',  ( 10.00000000000000178, 62.25893115100078745, 9.846743663894594434 ) ) ;
#77291 = CARTESIAN_POINT ( 'NONE',  ( 19.84674366389459266, 33.30059781766744464, 2.638427012816836559 ) ) ;
#77292 = CARTESIAN_POINT ( 'NONE',  ( 17.20831665107776587, 24.13393115100078035, -7.208316651077762316 ) ) ;
#77293 = CARTESIAN_POINT ( 'NONE',  ( 15.44008868035555793, 11.39701867748817143, -9.422509992056140149 ) ) ;
#77294 = CARTESIAN_POINT ( 'NONE',  ( -2.816281873526473856, 14.12363466993041961, 9.499525473075851096E-16 ) ) ;
#77295 = CARTESIAN_POINT ( 'NONE',  ( 4.559911319644449179, 2.230352010821504471, -9.422509992056141925 ) ) ;
#77296 = CARTESIAN_POINT ( 'NONE',  ( -10.34223742324294548, 89.23976162705943693, 5.715022854599767221 ) ) ;
#77297 = DIRECTION ( 'NONE',  ( 0.000000000000000000, 0.000000000000000000, 1.000000000000000000 ) ) ;
#77298 = CARTESIAN_POINT ( 'NONE',  ( 10.00000000000000178, 14.31368534415483929, 10.88017736071110342 ) ) ;
#77299 = LINE ( 'NONE', #9805, #37726 ) ;
#77301 = CARTESIAN_POINT ( 'NONE',  ( -0.8801773607111008646, 13.27201867748817321, 2.915334737309923430 ) ) ;
#77300 = CARTESIAN_POINT ( 'NONE',  ( 7.361572987183169658, 34.96726448433411605, -9.846743663894592657 ) ) ;
#77302 = CARTESIAN_POINT ( 'NONE',  ( 1.472469842513823179, 5.592264484334118713, -4.923371831947296329 ) ) ;
#77303 = CARTESIAN_POINT ( 'NONE',  ( 10.00000000000000000, 36.81368534415484106, -10.88017736071110342 ) ) ;
#77305 = CARTESIAN_POINT ( 'NONE',  ( 0.2751277870542911397, 40.30223176428831522, 6.499999999999992006 ) ) ;
#77304 = CARTESIAN_POINT ( 'NONE',  ( 6.204703633549690345, 60.76208216824730357, -14.16423886937410259 ) ) ;
#77306 = CARTESIAN_POINT ( 'NONE',  ( 0.1532563361054082862, 1.217264484334117824, 2.638427012816831674 ) ) ;
#77307 = CARTESIAN_POINT ( 'NONE',  ( 17.20831665107776587, 29.13393115100078390, -7.208316651077762316 ) ) ;
#77308 = DIRECTION ( 'NONE',  ( -1.000000000000000000, 8.673617379884036705E-17, 0.000000000000000000 ) ) ;
#77309 = CARTESIAN_POINT ( 'NONE',  ( -0.3093388210927633941, 14.49999999999999822, -14.99680997725065978 ) ) ;
#77310 = SPHERICAL_SURFACE ( 'NONE', #63493, 0.5000000000000000000 ) ;
#77311 = EDGE_CURVE ( 'NONE', #21166, #68203, #34351, .T. ) ;
#77312 = CARTESIAN_POINT ( 'NONE',  ( 24.16423886937409904, 24.09541550158063927, 3.795296366450317205 ) ) ;
#77313 = CARTESIAN_POINT ( 'NONE',  ( 19.84674366389459266, 38.30059781766745175, 2.638427012816836559 ) ) ;
#77314 = DIRECTION ( 'NONE',  ( 0.000000000000000000, -1.000000000000000000, 0.000000000000000000 ) ) ;
#77315 = TOROIDAL_SURFACE ( 'NONE', #62983, 14.49999999999999822, 0.5000000000000000000 ) ;
#77316 = CARTESIAN_POINT ( 'NONE',  ( 6.204703633549690345, 50.76208216824730357, -14.16423886937410259 ) ) ;
#77317 = EDGE_CURVE ( 'NONE', #84883, #89457, #79945, .T. ) ;
#77318 = CARTESIAN_POINT ( 'NONE',  ( 19.84674366389459266, 23.71726448433412315, -2.638427012816827677 ) ) ;
#77320 = LINE ( 'NONE', #75359, #21557 ) ;
#77319 = FILL_AREA_STYLE ('',( #83852 ) ) ;
#77321 = CARTESIAN_POINT ( 'NONE',  ( 17.96484262340118221, 39.93868534415484106, 7.964842623401181321 ) ) ;
#77322 = CARTESIAN_POINT ( 'NONE',  ( 10.00000000000000178, 55.37363466993042493, 12.81628187352647608 ) ) ;
#77323 = CARTESIAN_POINT ( 'NONE',  ( 2.035157376598822676, 17.43868534415483751, -7.964842623401177768 ) ) ;
#77325 = ORIENTED_EDGE ( 'NONE', *, *, #510, .T. ) ;
#77324 = CARTESIAN_POINT ( 'NONE',  ( -1.099225684535947600, 49.54030133659708923, 6.408140936763237150 ) ) ;
#77326 = CARTESIAN_POINT ( 'NONE',  ( 17.20831665107776587, 62.88393115100078745, 7.208316651077764980 ) ) ;
#77327 = CARTESIAN_POINT ( 'NONE',  ( 2.791683348922240793, 1.633931151000784565, 7.208316651077764092 ) ) ;
#77328 = ORIENTED_EDGE ( 'NONE', *, *, #10014, .F. ) ;
#77329 = VECTOR ( 'NONE', #90106, 1000.000000000000000 ) ;
#77330 = PLANE ( 'NONE',  #82183 ) ;
#77331 = DIRECTION ( 'NONE',  ( -1.000000000000000000, 0.000000000000000000, 0.000000000000000000 ) ) ;
#77332 = CARTESIAN_POINT ( 'NONE',  ( 24.16423886937409904, 54.09541550158063217, 3.795296366450317205 ) ) ;
#77333 = CARTESIAN_POINT ( 'NONE',  ( -4.164238869374099039, 16.80374883491396787, 8.674139862899312516E-16 ) ) ;
#77334 = CARTESIAN_POINT ( 'NONE',  ( 2.035157376598822676, 22.43868534415483396, -7.964842623401177768 ) ) ;
#77335 = CARTESIAN_POINT ( 'NONE',  ( 2.035157376598822676, 42.43868534415483396, -7.964842623401177768 ) ) ;
#77336 = DIRECTION ( 'NONE',  ( 0.000000000000000000, 0.000000000000000000, 1.000000000000000000 ) ) ;
#77337 = DIRECTION ( 'NONE',  ( -1.000000000000000000, 0.000000000000000000, 0.000000000000000000 ) ) ;
#77338 = CARTESIAN_POINT ( 'NONE',  ( 20.88017736071110164, 65.35535201082150536, 2.915334737309930979 ) ) ;
#77339 = CARTESIAN_POINT ( 'NONE',  ( 19.42250999205614548, 65.98035201082151957, -5.440088680355545492 ) ) ;
#77340 = CARTESIAN_POINT ( 'NONE',  ( 17.20831665107776587, 22.88393115100078745, 7.208316651077764980 ) ) ;
#77341 = FACE_OUTER_BOUND ( 'NONE', #81410, .T. ) ;
#77342 = FACE_OUTER_BOUND ( 'NONE', #80414, .T. ) ;
#77343 = CARTESIAN_POINT ( 'NONE',  ( 17.20831665107776587, 7.883931151000784787, 7.208316651077764980 ) ) ;
#77344 = CARTESIAN_POINT ( 'NONE',  ( 12.63842701281683922, 34.55059781766745886, -9.846743663894590881 ) ) ;
#77345 = CARTESIAN_POINT ( 'NONE',  ( 2.035157376598822676, 12.43868534415483751, -7.964842623401177768 ) ) ;
#77346 = B_SPLINE_CURVE_WITH_KNOTS ( 'NONE', 3,
 ( #23000, #6018, #74993, #37004, #29475, #59983 ),
 .UNSPECIFIED., .F., .F.,
 ( 4, 2, 4 ),
 ( 0.000000000000000000, 0.0002605067024380876522, 0.0005210134048761753045 ),
 .UNSPECIFIED. ) ;
#77348 = EDGE_CURVE ( 'NONE', #98073, #65284, #21251, .T. ) ;
#77347 = CARTESIAN_POINT ( 'NONE',  ( 22.81628187352647785, 26.62363466993042138, 6.195893100308588602E-16 ) ) ;
#77349 = CARTESIAN_POINT ( 'NONE',  ( 14.92337183194729988, 4.342264484334117824, -8.527530157486177487 ) ) ;
#77350 = DIRECTION ( 'NONE',  ( -0.2672383760782703344, -0.000000000000000000, 0.9636304532086192864 ) ) ;
#77351 = CARTESIAN_POINT ( 'NONE',  ( 19.84674366389459266, 53.71726448433411605, -2.638427012816827677 ) ) ;
#77352 = CARTESIAN_POINT ( 'NONE',  ( 1.472469842513823179, 31.42559781766745530, 4.923371831947296329 ) ) ;
#77353 = CARTESIAN_POINT ( 'NONE',  ( 13.79529636645030344, 23.26208216824730002, 14.16423886937410614 ) ) ;
#77354 = CARTESIAN_POINT ( 'NONE',  ( 10.00000000000000000, 51.81368534415484106, -10.88017736071110342 ) ) ;
#77355 = CARTESIAN_POINT ( 'NONE',  ( 7.084665262690076126, 7.022018677488169658, -10.88017736071110164 ) ) ;
#77356 = EDGE_CURVE ( 'NONE', #74440, #78790, #91811, .T. ) ;
#77357 = CARTESIAN_POINT ( 'NONE',  ( 15.44008868035555793, 51.39701867748816966, -9.422509992056140149 ) ) ;
#77358 = CARTESIAN_POINT ( 'NONE',  ( 17.96484262340118221, 36.18868534415484106, -7.964842623401177768 ) ) ;
#77359 = ORIENTED_EDGE ( 'NONE', *, *, #37974, .T. ) ;
#77360 = CARTESIAN_POINT ( 'NONE',  ( 20.88017736071110519, 40.56368534415484106, 2.639326808657452039E-16 ) ) ;
#77361 = ORIENTED_EDGE ( 'NONE', *, *, #34774, .T. ) ;
#77362 = AXIS2_PLACEMENT_3D ( 'NONE', #4329, #64792, #19803 ) ;
#77363 = CARTESIAN_POINT ( 'NONE',  ( 16.40814093676323893, 60.79030133659709634, 11.09922568453595026 ) ) ;
#77364 = CARTESIAN_POINT ( 'NONE',  ( 12.91533473730992121, 49.52201867748817676, 10.88017736071110164 ) ) ;
#77365 = ORIENTED_EDGE ( 'NONE', *, *, #67392, .T. ) ;
#77366 = CARTESIAN_POINT ( 'NONE',  ( -0.8801773607111009756, 48.06368534415484817, 1.068504757029289695E-15 ) ) ;
#77367 = CARTESIAN_POINT ( 'NONE',  ( 5.170525679121678486, -13.81869365337359845, 4.000000000000000000 ) ) ;
#77368 = CARTESIAN_POINT ( 'NONE',  ( 14.29730467489533652, 3.971653163193037558E-16, -2.416004766803220516 ) ) ;
#77369 = CARTESIAN_POINT ( 'NONE',  ( -14.15281240980442945, 15.00000000000000711, -3.688687068602892971 ) ) ;
#77370 = CARTESIAN_POINT ( 'NONE',  ( 24.16423886937410614, 59.51208216824728936, -3.795296366450302550 ) ) ;
#77371 = CARTESIAN_POINT ( 'NONE',  ( 15.44008868035555260, 59.73035201082151247, 9.422509992056143702 ) ) ;
#77372 = CARTESIAN_POINT ( 'NONE',  ( 19.72487221294571569, 25.71833443783938478, -6.499999999999989342 ) ) ;
#77373 = CARTESIAN_POINT ( 'NONE',  ( -3.836041483939801378, -2.701055130266050153, -4.000000000000000888 ) ) ;
#77374 = CARTESIAN_POINT ( 'NONE',  ( 20.88017736071110164, 10.35535201082150714, 2.915334737309930979 ) ) ;
#77375 = CARTESIAN_POINT ( 'NONE',  ( 18.52753015748617571, 33.09226448433411605, 4.923371831947298993 ) ) ;
#77376 = ORIENTED_EDGE ( 'NONE', *, *, #38207, .T. ) ;
#77377 = CARTESIAN_POINT ( 'NONE',  ( 10.00000000000000178, 32.25893115100078745, 9.846743663894594434 ) ) ;
#77378 = CARTESIAN_POINT ( 'NONE',  ( 0.5774900079438607392, 33.48035201082150536, 5.440088680355550821 ) ) ;
#77379 = CARTESIAN_POINT ( 'NONE',  ( 2.791683348922237240, 40.38393115100078035, -7.208316651077763204 ) ) ;
#77380 = CARTESIAN_POINT ( 'NONE',  ( 22.81628187352648496, 16.83196800326374998, -3.434112377981050290 ) ) ;
#77381 = CARTESIAN_POINT ( 'NONE',  ( 17.96484262340118221, 66.18868534415483396, -7.964842623401177768 ) ) ;
#77382 = CARTESIAN_POINT ( 'NONE',  ( 0.5774900079438590739, 52.64701867748817676, -5.440088680355550821 ) ) ;
#77383 = CARTESIAN_POINT ( 'NONE',  ( -4.164238869374099927, 57.01208216824731068, 3.795296366450308767 ) ) ;
#77384 = EDGE_CURVE ( 'NONE', #14921, #93129, #98850, .T. ) ;
#77385 = CARTESIAN_POINT ( 'NONE',  ( 22.81628187352648496, 26.83196800326374998, -3.434112377981050290 ) ) ;
#77386 = DIRECTION ( 'NONE',  ( -0.000000000000000000, 1.000000000000000000, 0.000000000000000000 ) ) ;
#77387 = ORIENTED_EDGE ( 'NONE', *, *, #78101, .F. ) ;
#77388 = CARTESIAN_POINT ( 'NONE',  ( 13.43411237798105340, 25.58196800326374998, 12.81628187352647963 ) ) ;
#77389 = CARTESIAN_POINT ( 'NONE',  ( 12.91533473730992121, 19.52201867748816611, 10.88017736071110164 ) ) ;
#77390 =( BOUNDED_CURVE ( )  B_SPLINE_CURVE ( 2, ( #30894, #53901, #46880, #76886, #46398, #82918, #23909, #16398, #38908 ),
 .UNSPECIFIED., .F., .F. ) 
 B_SPLINE_CURVE_WITH_KNOTS ( ( 3, 2, 2, 2, 3 ),
 ( 0.7605718029354654464, 0.7619047619047618625, 0.7678571428571429047, 0.7738095238095238360, 0.7751424827788201410 ),
 .UNSPECIFIED. ) 
 CURVE ( )  GEOMETRIC_REPRESENTATION_ITEM ( )  RATIONAL_B_SPLINE_CURVE ( ( 0.9881565478350733400, 0.9923695281211490915, 1.000000000000000000, 0.9659258262890683122, 1.000000000000000000, 0.9659258262890683122, 1.000000000000000000, 0.9923695281211497576, 0.9881565478350740062 ) ) 
 REPRESENTATION_ITEM ( '' )  );
#77391 = VECTOR ( 'NONE', #58256, 1000.000000000000000 ) ;
#77392 = ORIENTED_EDGE ( 'NONE', *, *, #6684, .F. ) ;
#77393 = CARTESIAN_POINT ( 'NONE',  ( 0.1532563361054082862, 1.217264484334117824, 2.638427012816831674 ) ) ;
#77394 = VECTOR ( 'NONE', #24813, 1000.000000000000000 ) ;
#77395 = CARTESIAN_POINT ( 'NONE',  ( 19.84674366389459621, 43.50893115100078745, 7.409399052514197653E-17 ) ) ;
#77396 = CARTESIAN_POINT ( 'NONE',  ( 7.361572987183169658, 39.96726448433411605, -9.846743663894592657 ) ) ;
#77397 = DIRECTION ( 'NONE',  ( -8.673617379884027583E-16, -1.000000000000000000, 0.000000000000000000 ) ) ;
#77398 = LINE ( 'NONE', #8427, #61806 ) ;
#77399 = CARTESIAN_POINT ( 'NONE',  ( 7.361572987183170547, 22.05059781766745530, 9.846743663894590881 ) ) ;
#77400 = CARTESIAN_POINT ( 'NONE',  ( -0.03447792253739219437, 40.15514106990689669, 6.401564815979744694 ) ) ;
#77401 = CARTESIAN_POINT ( 'NONE',  ( -18.00000000000000355, 75.73428692542562146, -2.900000000000000799 ) ) ;
#77403 = DIRECTION ( 'NONE',  ( 1.000000000000000000, 1.387778780781444413E-14, 0.000000000000000000 ) ) ;
#77402 = CARTESIAN_POINT ( 'NONE',  ( 18.52753015748618282, 8.925597817667451750, -4.923371831947291888 ) ) ;
#77404 = CARTESIAN_POINT ( 'NONE',  ( 7.007880867418010418, -58.32092081208355694, -4.000000000000000888 ) ) ;
#77406 = ORIENTED_EDGE ( 'NONE', *, *, #29792, .T. ) ;
#77405 = CARTESIAN_POINT ( 'NONE',  ( 10.00000000000000000, 49.75893115100078745, -9.846743663894594434 ) ) ;
#77407 = DIRECTION ( 'NONE',  ( 0.000000000000000000, -1.000000000000000000, -0.000000000000000000 ) ) ;
#77408 = CARTESIAN_POINT ( 'NONE',  ( -1.099225684535947600, 13.70696800326375353, -6.408140936763238038 ) ) ;
#77409 = AXIS2_PLACEMENT_3D ( 'NONE', #81746, #13262, #66758 ) ;
#77410 = CARTESIAN_POINT ( 'NONE',  ( 15.44008868035555793, 46.39701867748817676, -9.422509992056140149 ) ) ;
#77411 = CARTESIAN_POINT ( 'NONE',  ( -0.3689425029237881626, 52.42874883491396076, 10.36894250292379027 ) ) ;
#77412 = CARTESIAN_POINT ( 'NONE',  ( 12.63842701281683034, 2.467264484334118269, 9.846743663894596210 ) ) ;
#77413 = DIRECTION ( 'NONE',  ( -0.000000000000000000, -0.000000000000000000, -1.000000000000000000 ) ) ;
#77414 = CARTESIAN_POINT ( 'NONE',  ( 6.204703633549690345, 40.76208216824731778, -14.16423886937410259 ) ) ;
#77415 = CARTESIAN_POINT ( 'NONE',  ( -2.266590686148945544, 61.38708216824730357, -7.082119434687050408 ) ) ;
#77416 = CARTESIAN_POINT ( 'NONE',  ( -4.164238869374099927, 22.01208216824730357, 3.795296366450308767 ) ) ;
#77418 = CARTESIAN_POINT ( 'NONE',  ( -2.913501739333568707, 15.00000000000000000, -14.20427779279538960 ) ) ;
#77417 = CARTESIAN_POINT ( 'NONE',  ( -4.164238869374098151, 21.59541550158063217, -3.795296366450310543 ) ) ;
#77419 = CARTESIAN_POINT ( 'NONE',  ( 4.474002695404426966, -3.767820133606233579, -3.750000000000000888 ) ) ;
#77420 = EDGE_CURVE ( 'NONE', #76539, #58682, #53812, .T. ) ;
#77422 = CARTESIAN_POINT ( 'NONE',  ( 19.84674366389459266, 43.30059781766744464, 2.638427012816836559 ) ) ;
#77421 = CARTESIAN_POINT ( 'NONE',  ( 4.380000000000000782, 1.019547802438464768, 2.500000000000000000 ) ) ;
#77423 = ORIENTED_EDGE ( 'NONE', *, *, #24581, .F. ) ;
#77424 = CARTESIAN_POINT ( 'NONE',  ( 2.035157376598822676, 37.43868534415484106, -7.964842623401177768 ) ) ;
#77425 = CARTESIAN_POINT ( 'NONE',  ( -4.250000000000000000, 36.75000000000000000, 3.750000000000000000 ) ) ;
#77426 = CARTESIAN_POINT ( 'NONE',  ( -12.54342190210035213, 0.2301501149690338699, -8.116945096741464027 ) ) ;
#77427 = PRESENTATION_LAYER_ASSIGNMENT (  '', '', ( #67823 ) ) ;
#77428 = CARTESIAN_POINT ( 'NONE',  ( 14.66148682522523217, 0.2301506158824408732, -2.874551585517186147 ) ) ;
#77429 = CARTESIAN_POINT ( 'NONE',  ( 0.1532563361054082862, 46.21726448433411605, 2.638427012816831674 ) ) ;
#77430 = CARTESIAN_POINT ( 'NONE',  ( -2.816281873526473856, 54.33196800326376064, 3.434112377981055619 ) ) ;
#77431 = CARTESIAN_POINT ( 'NONE',  ( 10.36894250292379027, -11.32125116508602858, 10.36894250292378672 ) ) ;
#77432 = CARTESIAN_POINT ( 'NONE',  ( 7.361572987183170547, 47.05059781766745175, 9.846743663894590881 ) ) ;
#77433 = CARTESIAN_POINT ( 'NONE',  ( 10.00000000000000178, 47.25893115100078745, 9.846743663894594434 ) ) ;
#77434 = EDGE_CURVE ( 'NONE', #33828, #34829, #60806, .T. ) ;
#77435 = CARTESIAN_POINT ( 'NONE',  ( 24.16423886937410614, 39.30374883491396787, 8.672049930838204340E-16 ) ) ;
#77436 = ORIENTED_EDGE ( 'NONE', *, *, #14870, .F. ) ;
#77437 = CARTESIAN_POINT ( 'NONE',  ( 24.16423886937410614, 19.51208216824729647, -3.795296366450302550 ) ) ;
#77438 = EDGE_CURVE ( 'NONE', #6459, #95671, #21521, .T. ) ;
#77439 = DIRECTION ( 'NONE',  ( -0.000000000000000000, 1.000000000000000000, 0.000000000000000000 ) ) ;
#77441 = DIRECTION ( 'NONE',  ( 0.000000000000000000, 1.000000000000000000, 0.000000000000000000 ) ) ;
#77440 = DIRECTION ( 'NONE',  ( 0.000000000000000000, -0.000000000000000000, -1.000000000000000000 ) ) ;
#77442 = CARTESIAN_POINT ( 'NONE',  ( 7.084665262690076126, 4.105352010821503583, 10.88017736071109987 ) ) ;
#77443 = CARTESIAN_POINT ( 'NONE',  ( 16.40814093676324603, 7.456968003263754419, -11.09922568453594671 ) ) ;
#77444 = CARTESIAN_POINT ( 'NONE',  ( 20.88017736071110519, 65.56368534415483396, 2.639326808657452039E-16 ) ) ;
#77445 = LINE ( 'NONE', #16968, #86758 ) ;
#77446 = CARTESIAN_POINT ( 'NONE',  ( 0.1129803114748713505, 14.29427333184090720, -6.480634945678661829 ) ) ;
#77447 = DIRECTION ( 'NONE',  ( 0.000000000000000000, 1.000000000000000000, 0.000000000000000000 ) ) ;
#77448 = CARTESIAN_POINT ( 'NONE',  ( 2.917880565312948704, 62.63708216824730357, 12.26659068614894643 ) ) ;
#77449 = CARTESIAN_POINT ( 'NONE',  ( 0.1077916266722676458, 42.24062864464241329, -6.478736007405996311 ) ) ;
#77450 = CARTESIAN_POINT ( 'NONE',  ( 15.44008868035555793, 21.39701867748817321, -9.422509992056140149 ) ) ;
#77451 = CARTESIAN_POINT ( 'NONE',  ( 0.5774900079438590739, 22.64701867748817321, -5.440088680355550821 ) ) ;
#77452 = CARTESIAN_POINT ( 'NONE',  ( 2.791683348922237240, 50.38393115100078035, -7.208316651077763204 ) ) ;
#77453 = CARTESIAN_POINT ( 'NONE',  ( 19.84674366389459621, 53.50893115100078745, 7.409399052514197653E-17 ) ) ;
#77454 = CARTESIAN_POINT ( 'NONE',  ( -2.816281873526471635, 63.91530133659708923, -3.434112377981056508 ) ) ;
#77455 = CARTESIAN_POINT ( 'NONE',  ( 0.000000000000000000, 70.00000000000000000, -5.000000000000000000 ) ) ;
#77456 = VERTEX_POINT ( 'NONE', #75319 ) ;
#77457 = ADVANCED_FACE ( 'NONE', ( #22834 ), #7831, .T. ) ;
#77458 = CARTESIAN_POINT ( 'NONE',  ( 7.084665262690076126, 24.10535201082150181, 10.88017736071109987 ) ) ;
#77459 = CARTESIAN_POINT ( 'NONE',  ( 10.00000000000000178, 30.37363466993042138, 12.81628187352647608 ) ) ;
#77460 = CARTESIAN_POINT ( 'NONE',  ( -5.451370222425310885, 0.000000000000000000, -0.1427491530890833693 ) ) ;
#77461 = PRODUCT_DEFINITION_FORMATION_WITH_SPECIFIED_SOURCE ( 'ANY', '', #98603, .NOT_KNOWN. ) ;
#77462 = CARTESIAN_POINT ( 'NONE',  ( 0.1532563361054100626, 55.80059781766745175, -2.638427012816831230 ) ) ;
#77463 = CARTESIAN_POINT ( 'NONE',  ( 2.035157376598824452, 43.68868534415484106, 7.964842623401179544 ) ) ;
#77464 = CIRCLE ( 'NONE', #47127, 10.90000000000026326 ) ;
#77465 = CARTESIAN_POINT ( 'NONE',  ( 18.52753015748617571, 8.092264484334117824, 4.923371831947298993 ) ) ;
#77466 = CARTESIAN_POINT ( 'NONE',  ( -2.816281873526471635, 18.91530133659708213, -3.434112377981056508 ) ) ;
#77468 = DIRECTION ( 'NONE',  ( -0.000000000000000000, -1.000000000000000000, -0.000000000000000000 ) ) ;
#77467 = CARTESIAN_POINT ( 'NONE',  ( 20.88017736071110164, 60.35535201082151957, 2.915334737309930979 ) ) ;
#77469 = FACE_OUTER_BOUND ( 'NONE', #89330, .T. ) ;
#77470 = ORIENTED_EDGE ( 'NONE', *, *, #54063, .T. ) ;
#77471 = FACE_OUTER_BOUND ( 'NONE', #98772, .T. ) ;
#77472 = LINE ( 'NONE', #84006, #65348 ) ;
#77473 = CARTESIAN_POINT ( 'NONE',  ( -0.8801773607110991993, 52.85535201082151247, -2.915334737309923874 ) ) ;
#77474 = CARTESIAN_POINT ( 'NONE',  ( -2.816281873526473856, 49.33196800326374643, 3.434112377981055619 ) ) ;
#77475 = EDGE_CURVE ( 'NONE', #84126, #30654, #38327, .T. ) ;
#77476 = CARTESIAN_POINT ( 'NONE',  ( 17.20831665107776587, 14.13393115100078568, -7.208316651077762316 ) ) ;
#77477 = CARTESIAN_POINT ( 'NONE',  ( 7.084665262690076126, 4.105352010821503583, 10.88017736071109987 ) ) ;
#77478 = CARTESIAN_POINT ( 'NONE',  ( 1.472469842513823179, 21.42559781766745175, 4.923371831947296329 ) ) ;
#77479 = DIRECTION ( 'NONE',  ( 0.000000000000000000, 1.000000000000000000, 0.000000000000000000 ) ) ;
#77480 = CARTESIAN_POINT ( 'NONE',  ( 17.08211943468705840, 55.13708216824731068, -12.26659068614894466 ) ) ;
#77481 = ORIENTED_EDGE ( 'NONE', *, *, #97118, .F. ) ;
#77482 = CARTESIAN_POINT ( 'NONE',  ( 20.88017736071110519, 5.563685344154837509, 2.639326808657452039E-16 ) ) ;
#77483 = CARTESIAN_POINT ( 'NONE',  ( 15.44008868035555793, 11.39701867748817143, -9.422509992056140149 ) ) ;
#77484 = PLANE ( 'NONE',  #23246 ) ;
#77485 = ORIENTED_EDGE ( 'NONE', *, *, #87250, .F. ) ;
#77486 = CARTESIAN_POINT ( 'NONE',  ( 20.88017736071110875, 10.77201867748817143, -2.915334737309920765 ) ) ;
#77487 = CARTESIAN_POINT ( 'NONE',  ( 20.88017736071110519, 10.56368534415483929, 2.639326808657452039E-16 ) ) ;
#77488 = CARTESIAN_POINT ( 'NONE',  ( 1.472469842513823179, 40.59226448433411605, -4.923371831947296329 ) ) ;
#77489 = CARTESIAN_POINT ( 'NONE',  ( -2.816281873526473856, 34.12363466993042493, 9.499525473075851096E-16 ) ) ;
#77490 = CARTESIAN_POINT ( 'NONE',  ( -8.439016546559980014, 3.939291001653719071E-16, 11.79122553964967679 ) ) ;
#77492 = CARTESIAN_POINT ( 'NONE',  ( 22.26659068614895176, 24.72041550158063572, -7.082119434687042414 ) ) ;
#77491 = CARTESIAN_POINT ( 'NONE',  ( -9.402796353260978179, 14.63606911086602658, -11.68706210897773978 ) ) ;
#77493 = CARTESIAN_POINT ( 'NONE',  ( 15.44008868035555260, 19.73035201082150536, 9.422509992056143702 ) ) ;
#77494 = CARTESIAN_POINT ( 'NONE',  ( 15.44008868035555260, 4.730352010821505360, 9.422509992056143702 ) ) ;
#77495 = CARTESIAN_POINT ( 'NONE',  ( 1.472469842513823179, 36.42559781766745175, 4.923371831947296329 ) ) ;
#77496 = LINE ( 'NONE', #45532, #36454 ) ;
#77497 = CARTESIAN_POINT ( 'NONE',  ( 2.791683348922237240, 40.38393115100078035, -7.208316651077763204 ) ) ;
#77498 = DIRECTION ( 'NONE',  ( -3.552713678800500929E-14, 0.000000000000000000, 1.000000000000000000 ) ) ;
#77499 = CARTESIAN_POINT ( 'NONE',  ( -9.846743663894594434, 26.00893115100079456, 3.469446951953614189E-15 ) ) ;
#77500 = ORIENTED_EDGE ( 'NONE', *, *, #19708, .F. ) ;
#77501 = CARTESIAN_POINT ( 'NONE',  ( 12.91533473730992121, 4.522018677488169658, 10.88017736071110164 ) ) ;
#77502 = CARTESIAN_POINT ( 'NONE',  ( 0.5774900079438607392, 63.48035201082149825, 5.440088680355550821 ) ) ;
#77503 = CARTESIAN_POINT ( 'NONE',  ( 15.44008868035555793, 31.39701867748817676, -9.422509992056140149 ) ) ;
#77505 = CARTESIAN_POINT ( 'NONE',  ( 6.565887622018943937, 25.16530133659708213, 12.81628187352647430 ) ) ;
#77504 = CARTESIAN_POINT ( 'NONE',  ( 20.88017736071110875, 10.77201867748817143, -2.915334737309920765 ) ) ;
#77506 = CARTESIAN_POINT ( 'NONE',  ( 20.36894250292379738, 19.92874883491396787, -10.36894250292379027 ) ) ;
#77507 = PRESENTATION_LAYER_ASSIGNMENT (  '', '', ( #21640 ) ) ;
#77508 = CIRCLE ( 'NONE', #24862, 2.999999999999999556 ) ;
#77509 = CARTESIAN_POINT ( 'NONE',  ( -2.816281873526473856, 44.33196800326375353, 3.434112377981055619 ) ) ;
#77510 = ORIENTED_EDGE ( 'NONE', *, *, #56253, .F. ) ;
#77511 = CARTESIAN_POINT ( 'NONE',  ( 12.63842701281683922, 54.55059781766745175, -9.846743663894590881 ) ) ;
#77512 = CARTESIAN_POINT ( 'NONE',  ( 7.084665262690076126, 14.10535201082150358, 10.88017736071109987 ) ) ;
#77513 = ORIENTED_EDGE ( 'NONE', *, *, #8268, .F. ) ;
#77514 = CARTESIAN_POINT ( 'NONE',  ( -0.8801773607111009756, 18.06368534415484106, 1.068504757029289695E-15 ) ) ;
#77515 = ORIENTED_EDGE ( 'NONE', *, *, #65000, .T. ) ;
#77516 = CARTESIAN_POINT ( 'NONE',  ( 15.44008868035555260, 64.73035201082151957, 9.422509992056143702 ) ) ;
#77517 = CARTESIAN_POINT ( 'NONE',  ( 2.035157376598824452, 68.68868534415484817, 7.964842623401179544 ) ) ;
#77518 = ADVANCED_FACE ( 'NONE', ( #52327 ), #19677, .T. ) ;
#77519 = CARTESIAN_POINT ( 'NONE',  ( 17.20831665107776587, 9.133931151000787452, -7.208316651077762316 ) ) ;
#77520 = CARTESIAN_POINT ( 'NONE',  ( 20.88017736071110875, 65.77201867748817676, -2.915334737309920765 ) ) ;
#77521 = DIRECTION ( 'NONE',  ( -0.2334453638558956767, 0.000000000000000000, -0.9723699203976788885 ) ) ;
#77522 = ADVANCED_FACE ( 'NONE', ( #29813 ), #78776, .T. ) ;
#77523 = CARTESIAN_POINT ( 'NONE',  ( -46.61145641952149532, 101.4776089914260950, 8.252540973952291026 ) ) ;
#77524 = TOROIDAL_SURFACE ( 'NONE', #67984, 14.49999999999999822, 0.5000000000000000000 ) ;
#77526 = ORIENTED_EDGE ( 'NONE', *, *, #72291, .F. ) ;
#77525 = CARTESIAN_POINT ( 'NONE',  ( 2.791683348922240793, 6.633931151000785675, 7.208316651077764092 ) ) ;
#77527 = VECTOR ( 'NONE', #76932, 1000.000000000000000 ) ;
#77528 = CARTESIAN_POINT ( 'NONE',  ( 18.52753015748617571, 43.09226448433412315, 4.923371831947298993 ) ) ;
#77529 = VERTEX_POINT ( 'NONE', #92783 ) ;
#77530 = ORIENTED_EDGE ( 'NONE', *, *, #94607, .F. ) ;
#77531 = CARTESIAN_POINT ( 'NONE',  ( 1.499999999999999112, 23.03999999999999915, 1.836970198721028701E-16 ) ) ;
#77532 = VECTOR ( 'NONE', #72730, 1000.000000000000000 ) ;
#77533 = CARTESIAN_POINT ( 'NONE',  ( 17.08211943468705840, 5.137082168247300906, -12.26659068614894466 ) ) ;
#77534 = CARTESIAN_POINT ( 'NONE',  ( 10.00000000000000178, 60.37363466993041783, 12.81628187352647608 ) ) ;
#77535 = PRESENTATION_STYLE_ASSIGNMENT (( #87014 ) ) ;
#77536 = CARTESIAN_POINT ( 'NONE',  ( 13.79529636645030344, 13.26208216824729824, 14.16423886937410614 ) ) ;
#77537 = FILL_AREA_STYLE_COLOUR ( '', #74604 ) ;
#77539 = CARTESIAN_POINT ( 'NONE',  ( 4.559911319644449179, 58.89701867748817676, 9.422509992056141925 ) ) ;
#77538 = DIRECTION ( 'NONE',  ( 0.2503800040544389427, 0.000000000000000000, 0.9681476403781082984 ) ) ;
#77540 = CARTESIAN_POINT ( 'NONE',  ( 4.559911319644449179, 22.23035201082150536, -9.422509992056141925 ) ) ;
#77541 = CARTESIAN_POINT ( 'NONE',  ( 1.959929470562281395, 65.51528370094808906, -5.767676674365853629 ) ) ;
#77542 = ORIENTED_EDGE ( 'NONE', *, *, #14315, .F. ) ;
#77543 = CARTESIAN_POINT ( 'NONE',  ( 0.1532563361054082862, 6.217264484334118713, 2.638427012816831674 ) ) ;
#77544 = CARTESIAN_POINT ( 'NONE',  ( 19.84674366389459266, 3.300597817667451750, 2.638427012816836559 ) ) ;
#77545 = CARTESIAN_POINT ( 'NONE',  ( 13.43411237798106583, 27.66530133659708568, -12.81628187352647252 ) ) ;
#77546 = CARTESIAN_POINT ( 'NONE',  ( 19.84674366389459266, 23.30059781766745530, 2.638427012816836559 ) ) ;
#77547 = CARTESIAN_POINT ( 'NONE',  ( -4.880290883660354240, 0.000000000000000000, 2.433223276543825975 ) ) ;
#77548 = CARTESIAN_POINT ( 'NONE',  ( 13.43411237798105340, 10.58196800326375353, 12.81628187352647963 ) ) ;
#77549 = CARTESIAN_POINT ( 'NONE',  ( 0.3093388210927633941, 14.49999999999999822, 14.99680997725065978 ) ) ;
#77550 = EDGE_CURVE ( 'NONE', #25872, #15638, #91559, .T. ) ;
#77551 = AXIS2_PLACEMENT_3D ( 'NONE', #44727, #76225, #37252 ) ;
#77552 = CARTESIAN_POINT ( 'NONE',  ( 0.1532563361054082862, 11.21726448433411605, 2.638427012816831674 ) ) ;
#77553 = ORIENTED_EDGE ( 'NONE', *, *, #26104, .F. ) ;
#77554 = ORIENTED_EDGE ( 'NONE', *, *, #27201, .F. ) ;
#77555 = ADVANCED_FACE ( 'NONE', ( #64238 ), #1330, .F. ) ;
#77556 = CARTESIAN_POINT ( 'NONE',  ( 7.084665262690076126, 42.02201867748816966, -10.88017736071110164 ) ) ;
#77557 = CARTESIAN_POINT ( 'NONE',  ( 24.16423886937410614, 29.30374883491396787, 8.672049930838204340E-16 ) ) ;
#77558 = CARTESIAN_POINT ( 'NONE',  ( 7.361572987183170547, 37.05059781766744464, 9.846743663894590881 ) ) ;
#77559 = CARTESIAN_POINT ( 'NONE',  ( 18.52753015748617571, 3.092264484334118269, 4.923371831947298993 ) ) ;
#77561 = CARTESIAN_POINT ( 'NONE',  ( 32.56412365047463453, 14.00000000000001066, 10.00000000000000000 ) ) ;
#77560 = CARTESIAN_POINT ( 'NONE',  ( 3.591859063236761518, 49.95696800326375353, 11.09922568453594849 ) ) ;
#77562 = CARTESIAN_POINT ( 'NONE',  ( 7.084665262690076126, 32.02201867748816966, -10.88017736071110164 ) ) ;
#77563 = FILL_AREA_STYLE_COLOUR ( '', #58186 ) ;
#77564 = CARTESIAN_POINT ( 'NONE',  ( 0.6178305044545838731, 19.74863466993042138, 9.382169495545420901 ) ) ;
#77565 = CARTESIAN_POINT ( 'NONE',  ( -2.816281873526473856, 4.331968003263754419, 3.434112377981055619 ) ) ;
#77566 = CARTESIAN_POINT ( 'NONE',  ( 14.92337183194729633, 42.67559781766745886, 8.527530157486181039 ) ) ;
#77567 = CARTESIAN_POINT ( 'NONE',  ( 3.469446951953614189E-15, 4.313685344154848167, 10.88017736071110342 ) ) ;
#77568 = CARTESIAN_POINT ( 'NONE',  ( -2.816281873526473856, 54.33196800326376064, 3.434112377981055619 ) ) ;
#77569 = B_SPLINE_CURVE_WITH_KNOTS ( 'NONE', 3,
 ( #84926, #92909, #953, #75946, #29941, #61918 ),
 .UNSPECIFIED., .F., .F.,
 ( 4, 2, 4 ),
 ( 0.0002800039672440411773, 0.0006862092354666055397, 0.001092414503689169902 ),
 .UNSPECIFIED. ) ;
#77571 = CARTESIAN_POINT ( 'NONE',  ( 14.49440716394873263, 4.853942851202206293E-16, 0.4026921475167233311 ) ) ;
#77570 = CARTESIAN_POINT ( 'NONE',  ( 17.96484262340118221, 56.18868534415484817, -7.964842623401177768 ) ) ;
#77572 = VECTOR ( 'NONE', #4277, 1000.000000000000000 ) ;
#77573 = DIRECTION ( 'NONE',  ( 0.000000000000000000, 0.000000000000000000, 1.000000000000000000 ) ) ;
#77574 = DIRECTION ( 'NONE',  ( 0.000000000000000000, -0.000000000000000000, -1.000000000000000000 ) ) ;
#77575 = CARTESIAN_POINT ( 'NONE',  ( 2.035157376598824452, 53.68868534415484817, 7.964842623401179544 ) ) ;
#77576 = CARTESIAN_POINT ( 'NONE',  ( 20.88017736071110164, 60.35535201082151957, 2.915334737309930979 ) ) ;
#77577 = CARTESIAN_POINT ( 'NONE',  ( 26.00000000000000355, 35.99999999999997158, 10.00000000000000000 ) ) ;
#77578 = FACE_OUTER_BOUND ( 'NONE', #28575, .T. ) ;
#77579 = CARTESIAN_POINT ( 'NONE',  ( 2.035157376598822676, 7.438685344154837509, -7.964842623401177768 ) ) ;
#77580 = CARTESIAN_POINT ( 'NONE',  ( 17.20831665107776587, 47.88393115100078745, 7.208316651077764980 ) ) ;
#77582 = CARTESIAN_POINT ( 'NONE',  ( 18.04007052943773104, 23.01528370094808551, 5.767676674365834977 ) ) ;
#77581 = CARTESIAN_POINT ( 'NONE',  ( 20.88017736071110875, 20.77201867748816611, -2.915334737309920765 ) ) ;
#77583 = CARTESIAN_POINT ( 'NONE',  ( -2.816281873526473856, 19.12363466993042138, 9.499525473075851096E-16 ) ) ;
#77584 = VERTEX_POINT ( 'NONE', #94256 ) ;
#77585 = CARTESIAN_POINT ( 'NONE',  ( 20.88017736071110519, 35.56368534415484106, 2.639326808657452039E-16 ) ) ;
#77587 = DIRECTION ( 'NONE',  ( 3.469446951953615372E-15, 1.000000000000000000, 0.000000000000000000 ) ) ;
#77586 = CARTESIAN_POINT ( 'NONE',  ( 22.81628187352647785, 6.415301336597088344, 3.434112377981063169 ) ) ;
#77588 = EDGE_CURVE ( 'NONE', #4683, #30551, #89517, .T. ) ;
#77589 = CARTESIAN_POINT ( 'NONE',  ( 17.96484262340118221, 14.93868534415483751, 7.964842623401181321 ) ) ;
#77590 = CARTESIAN_POINT ( 'NONE',  ( 20.88017736071110519, 40.56368534415484106, 2.639326808657452039E-16 ) ) ;
#77591 = CARTESIAN_POINT ( 'NONE',  ( -4.164238869374099039, 56.80374883491397497, 8.674139862899312516E-16 ) ) ;
#77592 = CARTESIAN_POINT ( 'NONE',  ( 1.472469842513823179, 21.42559781766745175, 4.923371831947296329 ) ) ;
#77593 = CARTESIAN_POINT ( 'NONE',  ( 17.96484262340118221, 66.18868534415483396, -7.964842623401177768 ) ) ;
#77594 = CARTESIAN_POINT ( 'NONE',  ( 0.7375392941517084910, 14.63606910179106535, 14.98185688723475195 ) ) ;
#77595 = CARTESIAN_POINT ( 'NONE',  ( 10.00000000000000178, 23.05374883491397142, 14.16423886937410082 ) ) ;
#77596 = AXIS2_PLACEMENT_3D ( 'NONE', #75398, #53387, #36425 ) ;
#77597 = CARTESIAN_POINT ( 'NONE',  ( -46.94000000000000483, 103.1204114943229939, 5.953233499612015756 ) ) ;
#77598 = CARTESIAN_POINT ( 'NONE',  ( 14.04391541078765471, 3.833537969851530006E-16, -3.608107528142839637 ) ) ;
#77599 = STYLED_ITEM ( 'NONE', ( #13681 ), #17407 ) ;
#77600 = ORIENTED_EDGE ( 'NONE', *, *, #23549, .T. ) ;
#77601 = EDGE_LOOP ( 'NONE', ( #24586, #1028, #68901, #47668 ) ) ;
#77602 = CARTESIAN_POINT ( 'NONE',  ( 20.36894250292379738, 39.92874883491396787, -10.36894250292379027 ) ) ;
#77603 = CARTESIAN_POINT ( 'NONE',  ( 13.79529636645030344, 38.26208216824729647, 14.16423886937410614 ) ) ;
#77604 = CARTESIAN_POINT ( 'NONE',  ( 0.5774900079438590739, 67.64701867748817676, -5.440088680355550821 ) ) ;
#77605 = CARTESIAN_POINT ( 'NONE',  ( 21.09922568453594849, 11.20696800326375531, 6.408140936763242479 ) ) ;
#77606 = CARTESIAN_POINT ( 'NONE',  ( 14.92337183194729988, 59.34226448433412315, -8.527530157486177487 ) ) ;
#77607 = PLANE ( 'NONE',  #40310 ) ;
#77609 = CARTESIAN_POINT ( 'NONE',  ( 10.00000000000000000, 17.87363466993041783, -12.81628187352647608 ) ) ;
#77608 = CARTESIAN_POINT ( 'NONE',  ( 7.084665262690076126, 59.10535201082150536, 10.88017736071109987 ) ) ;
#77610 = CARTESIAN_POINT ( 'NONE',  ( 10.00000000000000000, 35.55374883491396787, -14.16423886937410082 ) ) ;
#77611 = CARTESIAN_POINT ( 'NONE',  ( 0.5774900079438590739, 27.64701867748817676, -5.440088680355550821 ) ) ;
#77612 = VECTOR ( 'NONE', #90185, 1000.000000000000114 ) ;
#77613 = CARTESIAN_POINT ( 'NONE',  ( 20.88017736071110519, 35.56368534415484106, 2.639326808657452039E-16 ) ) ;
#77614 = CARTESIAN_POINT ( 'NONE',  ( 6.880000000000009663, 40.99999999999999289, -4.250000000000000000 ) ) ;
#77615 = CARTESIAN_POINT ( 'NONE',  ( -9.846743663894596210, -14.19940218233255003, -2.638427012816824124 ) ) ;
#77616 = ORIENTED_EDGE ( 'NONE', *, *, #81167, .T. ) ;
#77617 = CARTESIAN_POINT ( 'NONE',  ( -0.2838433074297238012, 13.12729635533385597, -9.500000000000000000 ) ) ;
#77618 = LINE ( 'NONE', #93613, #55724 ) ;
#77619 = ORIENTED_EDGE ( 'NONE', *, *, #43911, .F. ) ;
#77621 = CARTESIAN_POINT ( 'NONE',  ( 20.88017736071110164, 10.35535201082150714, 2.915334737309930979 ) ) ;
#77620 = CARTESIAN_POINT ( 'NONE',  ( 13.79529636645030344, 63.26208216824730357, 14.16423886937410614 ) ) ;
#77623 = CARTESIAN_POINT ( 'NONE',  ( 12.63842701281683034, 57.46726448433411605, 9.846743663894596210 ) ) ;
#77622 = CARTESIAN_POINT ( 'NONE',  ( 2.791683348922240793, 41.63393115100078745, 7.208316651077764092 ) ) ;
#77624 = CARTESIAN_POINT ( 'NONE',  ( 9.879999999999990123, 20.99999999999999645, 0.000000000000000000 ) ) ;
#77625 = CARTESIAN_POINT ( 'NONE',  ( -9.519554572443036378, 15.00000000000000178, 11.10344954678173757 ) ) ;
#77626 = CARTESIAN_POINT ( 'NONE',  ( 10.00000000000000000, 2.873634669930420049, -12.81628187352647608 ) ) ;
#77627 = ORIENTED_EDGE ( 'NONE', *, *, #4039, .F. ) ;
#77628 = CARTESIAN_POINT ( 'NONE',  ( -4.164238869374099039, 46.80374883491397497, 8.674139862899312516E-16 ) ) ;
#77629 = ORIENTED_EDGE ( 'NONE', *, *, #41733, .F. ) ;
#77630 = CARTESIAN_POINT ( 'NONE',  ( -2.266590686148945544, 47.22041550158063927, 7.082119434687048631 ) ) ;
#77631 = ORIENTED_EDGE ( 'NONE', *, *, #50019, .F. ) ;
#77632 = CARTESIAN_POINT ( 'NONE',  ( 4.559911319644449179, 23.89701867748817321, 9.422509992056141925 ) ) ;
#77633 = DIRECTION ( 'NONE',  ( 0.000000000000000000, 0.000000000000000000, 1.000000000000000000 ) ) ;
#77634 = CARTESIAN_POINT ( 'NONE',  ( -0.8801773607111008646, 43.27201867748817676, 2.915334737309923430 ) ) ;
#77635 = CARTESIAN_POINT ( 'NONE',  ( 1.472469842513823179, 51.42559781766745886, 4.923371831947296329 ) ) ;
#77636 = CARTESIAN_POINT ( 'NONE',  ( 7.084665262690076126, 34.10535201082151247, 10.88017736071109987 ) ) ;
#77637 = CARTESIAN_POINT ( 'NONE',  ( 14.73513795193453468, 14.95077488074853456, -0.7223639599946776180 ) ) ;
#77638 = CARTESIAN_POINT ( 'NONE',  ( 2.035157376598824452, 63.68868534415484106, 7.964842623401179544 ) ) ;
#77639 = CARTESIAN_POINT ( 'NONE',  ( 10.00000000000000178, 29.31368534415483751, 10.88017736071110342 ) ) ;
#77640 = B_SPLINE_CURVE_WITH_KNOTS ( 'NONE', 3,
 ( #2689, #33140, #63635, #10654, #71653, #57123 ),
 .UNSPECIFIED., .F., .F.,
 ( 4, 2, 4 ),
 ( 0.0002800553958269957748, 0.0006862611673083382664, 0.001092466938789680812 ),
 .UNSPECIFIED. ) ;
#77641 = AXIS2_PLACEMENT_3D ( 'NONE', #97776, #755, #98771 ) ;
#77642 = EDGE_CURVE ( 'NONE', #800, #11760, #9655, .T. ) ;
#77643 = B_SPLINE_CURVE_WITH_KNOTS ( 'NONE', 3,
 ( #38195, #16666, #61167, #1680, #84663, #94982 ),
 .UNSPECIFIED., .F., .F.,
 ( 4, 2, 4 ),
 ( 3.409110551494649399E-05, 0.0004400426677367928600, 0.0008459942299586392395 ),
 .UNSPECIFIED. ) ;
#77645 = ORIENTED_EDGE ( 'NONE', *, *, #50461, .F. ) ;
#77644 = PLANE ( 'NONE',  #92034 ) ;
#77646 = CARTESIAN_POINT ( 'NONE',  ( 19.84674366389459266, 3.300597817667451750, 2.638427012816836559 ) ) ;
#77647 = FACE_OUTER_BOUND ( 'NONE', #59934, .T. ) ;
#77648 = ORIENTED_EDGE ( 'NONE', *, *, #42020, .T. ) ;
#77649 = DIRECTION ( 'NONE',  ( 0.000000000000000000, 1.000000000000000000, -0.000000000000000000 ) ) ;
#77650 = CARTESIAN_POINT ( 'NONE',  ( 7.361572987183169658, 29.96726448433411960, -9.846743663894592657 ) ) ;
#77651 = CARTESIAN_POINT ( 'NONE',  ( 0.3998276802503074046, -0.03417435944610275333, 15.99117050944548879 ) ) ;
#77652 = AXIS2_PLACEMENT_3D ( 'NONE', #87855, #42862, #19373 ) ;
#77653 =( LENGTH_UNIT ( ) NAMED_UNIT ( * ) SI_UNIT ( .MILLI., .METRE. ) );
#77654 = DIRECTION ( 'NONE',  ( -1.000000000000000000, 0.000000000000000000, 0.000000000000000000 ) ) ;
#77655 = ORIENTED_EDGE ( 'NONE', *, *, #49221, .T. ) ;
#77656 = CARTESIAN_POINT ( 'NONE',  ( 14.26328062697243837, 0.04962887699556053911, -3.770429249334784849 ) ) ;
#77657 = CARTESIAN_POINT ( 'NONE',  ( 7.771322705631417804, 3.835866486557528145E-16, 12.24159072199922704 ) ) ;
#77658 = CARTESIAN_POINT ( 'NONE',  ( 7.361572987183170547, 52.05059781766745175, 9.846743663894590881 ) ) ;
#77659 = CARTESIAN_POINT ( 'NONE',  ( 20.36894250292379382, 48.67874883491396076, 10.36894250292379205 ) ) ;
#77660 = CARTESIAN_POINT ( 'NONE',  ( 19.84674366389459266, 53.71726448433411605, -2.638427012816827677 ) ) ;
#77661 = ORIENTED_EDGE ( 'NONE', *, *, #39973, .F. ) ;
#77662 = CARTESIAN_POINT ( 'NONE',  ( 8.880000000000000782, 1.019547802438458550, 4.000000000000000000 ) ) ;
#77663 = CARTESIAN_POINT ( 'NONE',  ( 19.84674366389459266, 23.30059781766745530, 2.638427012816836559 ) ) ;
#77665 = PRESENTATION_LAYER_ASSIGNMENT (  '', '', ( #42561 ) ) ;
#77664 = CARTESIAN_POINT ( 'NONE',  ( 21.09922568453594849, 51.20696800326375353, 6.408140936763242479 ) ) ;
#77666 = CARTESIAN_POINT ( 'NONE',  ( 2.791683348922240793, 56.63393115100078035, 7.208316651077764092 ) ) ;
#77667 = CARTESIAN_POINT ( 'NONE',  ( 0.5774900079438590739, 52.64701867748817676, -5.440088680355550821 ) ) ;
#77668 = AXIS2_PLACEMENT_3D ( 'NONE', #91718, #75227, #8226 ) ;
#77669 = CARTESIAN_POINT ( 'NONE',  ( -3.195792623639463592, 8.703790035174481687, 11.92686044187660421 ) ) ;
#77670 = PRESENTATION_LAYER_ASSIGNMENT (  '', '', ( #31353 ) ) ;
#77671 = ADVANCED_FACE ( 'NONE', ( #18773 ), #56278, .T. ) ;
#77672 = VERTEX_POINT ( 'NONE', #70796 ) ;
#77673 = ADVANCED_FACE ( 'NONE', ( #2313 ), #55279, .F. ) ;
#77674 = CARTESIAN_POINT ( 'NONE',  ( 17.08211943468705840, 55.13708216824731068, -12.26659068614894466 ) ) ;
#77675 = CARTESIAN_POINT ( 'NONE',  ( 11.60808467749492934, 57.07844016847288060, 0.000000000000000000 ) ) ;
#77676 = CARTESIAN_POINT ( 'NONE',  ( 10.00000000000000178, 24.31368534415484106, 10.88017736071110342 ) ) ;
#77678 = CARTESIAN_POINT ( 'NONE',  ( 0.5774900079438607392, 53.48035201082151247, 5.440088680355550821 ) ) ;
#77677 = CARTESIAN_POINT ( 'NONE',  ( -1.099225684535947600, 13.70696800326375353, -6.408140936763238038 ) ) ;
#77679 = CARTESIAN_POINT ( 'NONE',  ( 20.88017736071110164, 65.35535201082151957, 2.915334737309930979 ) ) ;
#77680 =( LENGTH_UNIT ( ) NAMED_UNIT ( * ) SI_UNIT ( .MILLI., .METRE. ) );
#77681 = DIRECTION ( 'NONE',  ( 1.101341240428155162E-13, 0.000000000000000000, 1.000000000000000000 ) ) ;
#77683 = CARTESIAN_POINT ( 'NONE',  ( 8.630000000000000782, 1.019547802438458550, -4.000000000000000000 ) ) ;
#77682 = CARTESIAN_POINT ( 'NONE',  ( 7.084665262690076126, 59.10535201082150536, 10.88017736071109987 ) ) ;
#77684 = CARTESIAN_POINT ( 'NONE',  ( 1.472469842513823179, 41.42559781766745886, 4.923371831947296329 ) ) ;
#77685 = CARTESIAN_POINT ( 'NONE',  ( -14.16423886937410082, 31.80374883491396432, 4.336808689942017736E-15 ) ) ;
#77686 = CARTESIAN_POINT ( 'NONE',  ( 0.6178305044545838731, 4.748634669930420493, 9.382169495545420901 ) ) ;
#77687 = CARTESIAN_POINT ( 'NONE',  ( 20.88017736071110164, 10.35535201082150714, 2.915334737309930979 ) ) ;
#77688 =( LENGTH_UNIT ( ) NAMED_UNIT ( * ) SI_UNIT ( .MILLI., .METRE. ) );
#77689 = CARTESIAN_POINT ( 'NONE',  ( -4.164238869374099927, 42.01208216824728936, 3.795296366450308767 ) ) ;
#77690 = VECTOR ( 'NONE', #81946, 1000.000000000000000 ) ;
#77691 = CARTESIAN_POINT ( 'NONE',  ( 17.08211943468705130, 63.47041550158063927, 12.26659068614894998 ) ) ;
#77692 = CARTESIAN_POINT ( 'NONE',  ( 12.63842701281683034, 32.46726448433412315, 9.846743663894596210 ) ) ;
#77693 = AXIS2_PLACEMENT_3D ( 'NONE', #61421, #91931, #23458 ) ;
#77694 = CARTESIAN_POINT ( 'NONE',  ( 7.361572987183170547, 12.05059781766744997, 9.846743663894590881 ) ) ;
#77695 = CARTESIAN_POINT ( 'NONE',  ( -0.8801773607111008646, 8.272018677488171434, 2.915334737309923430 ) ) ;
#77696 = ORIENTED_EDGE ( 'NONE', *, *, #95205, .T. ) ;
#77697 = CARTESIAN_POINT ( 'NONE',  ( 1.472469842513823179, 35.59226448433412315, -4.923371831947296329 ) ) ;
#77698 = AXIS2_PLACEMENT_3D ( 'NONE', #76080, #84578, #85066 ) ;
#77699 = CARTESIAN_POINT ( 'NONE',  ( 2.035157376598824452, 23.68868534415484461, 7.964842623401179544 ) ) ;
#77700 = CARTESIAN_POINT ( 'NONE',  ( 10.00000000000000000, -2.126365330069579951, -12.81628187352647608 ) ) ;
#77702 = DIRECTION ( 'NONE',  ( 0.000000000000000000, 1.000000000000000000, 0.000000000000000000 ) ) ;
#77701 = CARTESIAN_POINT ( 'NONE',  ( -2.266590686148945544, 27.22041550158063572, 7.082119434687048631 ) ) ;
#77703 = DIRECTION ( 'NONE',  ( 0.5224985647159496871, 0.000000000000000000, 0.8526401643540917341 ) ) ;
#77704 = CARTESIAN_POINT ( 'NONE',  ( 5.076628168052704559, 10.17559781766745175, -8.527530157486179263 ) ) ;
#77705 = CARTESIAN_POINT ( 'NONE',  ( 6.565887622018943937, 53.08196800326374643, -12.81628187352647608 ) ) ;
#77706 = CARTESIAN_POINT ( 'NONE',  ( 2.791683348922240793, 56.63393115100078035, 7.208316651077764092 ) ) ;
#77707 = ORIENTED_EDGE ( 'NONE', *, *, #80326, .T. ) ;
#77708 = CARTESIAN_POINT ( 'NONE',  ( 18.52753015748618282, 18.92559781766745175, -4.923371831947291888 ) ) ;
#77709 = DIRECTION ( 'NONE',  ( 0.000000000000000000, -1.000000000000000000, 0.000000000000000000 ) ) ;
#77710 = CARTESIAN_POINT ( 'NONE',  ( 32.56412365047463453, 26.99999999999998224, 9.500000000000000000 ) ) ;
#77711 = CARTESIAN_POINT ( 'NONE',  ( 2.035157376598824452, 3.688685344154837953, 7.964842623401179544 ) ) ;
#77712 = CARTESIAN_POINT ( 'NONE',  ( 2.035157376598822676, 52.43868534415483396, -7.964842623401177768 ) ) ;
#77713 = CARTESIAN_POINT ( 'NONE',  ( 20.36894250292379382, 3.678748834913967869, 10.36894250292379205 ) ) ;
#77714 = CARTESIAN_POINT ( 'NONE',  ( 17.96484262340118221, 59.93868534415484106, 7.964842623401181321 ) ) ;
#77715 = CARTESIAN_POINT ( 'NONE',  ( 17.20831665107776587, 37.88393115100078745, 7.208316651077764980 ) ) ;
#77716 = CARTESIAN_POINT ( 'NONE',  ( 19.42250999205614548, 20.98035201082150891, -5.440088680355545492 ) ) ;
#77717 = SURFACE_STYLE_FILL_AREA ( #69740 ) ;
#77718 = CARTESIAN_POINT ( 'NONE',  ( 18.52753015748618282, 58.92559781766745886, -4.923371831947291888 ) ) ;
#77719 = VECTOR ( 'NONE', #42972, 1000.000000000000000 ) ;
#77720 = EDGE_CURVE ( 'NONE', #98695, #62655, #31061, .T. ) ;
#77721 = FACE_BOUND ( 'NONE', #26011, .T. ) ;
#77722 =( GEOMETRIC_REPRESENTATION_CONTEXT ( 3 ) GLOBAL_UNCERTAINTY_ASSIGNED_CONTEXT ( ( #29124 ) ) GLOBAL_UNIT_ASSIGNED_CONTEXT ( ( #59871, #27401, #20410 ) ) REPRESENTATION_CONTEXT ( 'NONE', 'WORKASPACE' ) );
#77723 = ORIENTED_EDGE ( 'NONE', *, *, #73953, .F. ) ;
#77724 = ORIENTED_EDGE ( 'NONE', *, *, #77960, .F. ) ;
#77725 = DIRECTION ( 'NONE',  ( -0.06975647374412534407, -0.9975640502598241977, 0.000000000000000000 ) ) ;
#77726 = CARTESIAN_POINT ( 'NONE',  ( 12.63842701281683034, 42.46726448433412315, 9.846743663894596210 ) ) ;
#77727 = CARTESIAN_POINT ( 'NONE',  ( 19.84674366389459621, 23.50893115100078390, 7.409399052514197653E-17 ) ) ;
#77728 = CARTESIAN_POINT ( 'NONE',  ( 0.6178305044545818747, 53.49863466993041072, -9.382169495545419124 ) ) ;
#77730 = CARTESIAN_POINT ( 'NONE',  ( 5.076628168052704559, 45.17559781766745175, -8.527530157486179263 ) ) ;
#77729 = CARTESIAN_POINT ( 'NONE',  ( 15.44008868035555793, 21.39701867748817321, -9.422509992056140149 ) ) ;
#77731 = CARTESIAN_POINT ( 'NONE',  ( -3.897244926436033374, 3.994152527635309729E-16, -13.96644127841335958 ) ) ;
#77732 = CARTESIAN_POINT ( 'NONE',  ( 6.204703633549690345, 35.76208216824729647, -14.16423886937410259 ) ) ;
#77733 = AXIS2_PLACEMENT_3D ( 'NONE', #76669, #8187, #61651 ) ;
#77734 = CARTESIAN_POINT ( 'NONE',  ( -0.3689425029237881626, 52.42874883491396076, 10.36894250292379027 ) ) ;
#77735 = DIRECTION ( 'NONE',  ( 0.000000000000000000, 1.000000000000000000, 0.000000000000000000 ) ) ;
#77736 = CARTESIAN_POINT ( 'NONE',  ( -11.94720539484397115, 14.76930270348885088, -8.972309510150314082 ) ) ;
#77737 = CARTESIAN_POINT ( 'NONE',  ( 4.559911319644449179, 52.23035201082151247, -9.422509992056141925 ) ) ;
#77738 = CARTESIAN_POINT ( 'NONE',  ( 19.84674366389459266, 13.71726448433411782, -2.638427012816827677 ) ) ;
#77739 = CYLINDRICAL_SURFACE ( 'NONE', #27001, 0.1000000000000001166 ) ;
#77740 = VERTEX_POINT ( 'NONE', #20236 ) ;
#77741 = CARTESIAN_POINT ( 'NONE',  ( 21.92686044187656691, 29.95379003517447458, 3.195792623639537755 ) ) ;
#77742 = ORIENTED_EDGE ( 'NONE', *, *, #89863, .T. ) ;
#77743 = CARTESIAN_POINT ( 'NONE',  ( 18.52753015748618282, 8.925597817667451750, -4.923371831947291888 ) ) ;
#77744 = ORIENTED_EDGE ( 'NONE', *, *, #11642, .F. ) ;
#77745 = CARTESIAN_POINT ( 'NONE',  ( -2.266590686148945544, 17.22041550158063572, 7.082119434687048631 ) ) ;
#77746 = CARTESIAN_POINT ( 'NONE',  ( 1.472469842513823179, 21.42559781766745175, 4.923371831947296329 ) ) ;
#77747 = CARTESIAN_POINT ( 'NONE',  ( 20.88017736071110164, 45.35535201082149115, 2.915334737309930979 ) ) ;
#77748 = CARTESIAN_POINT ( 'NONE',  ( -46.44000000000001194, 100.8660254037844339, -9.500000000000000000 ) ) ;
#77749 = ORIENTED_EDGE ( 'NONE', *, *, #45376, .T. ) ;
#77750 = CARTESIAN_POINT ( 'NONE',  ( 19.42250999205614193, 40.14701867748817676, 5.440088680355555262 ) ) ;
#77751 = CARTESIAN_POINT ( 'NONE',  ( -0.1049300847420728683, 2.216974130838790469, -6.336235997365750272 ) ) ;
#77752 = ORIENTED_EDGE ( 'NONE', *, *, #68363, .T. ) ;
#77753 = CARTESIAN_POINT ( 'NONE',  ( 19.42250999205614193, 45.14701867748817676, 5.440088680355555262 ) ) ;
#77754 = CARTESIAN_POINT ( 'NONE',  ( -0.3689425029237898834, 1.178748834913967869, -10.36894250292378850 ) ) ;
#77755 = ORIENTED_EDGE ( 'NONE', *, *, #49226, .T. ) ;
#77756 = CARTESIAN_POINT ( 'NONE',  ( -1.099225684535947600, 24.54030133659708923, 6.408140936763237150 ) ) ;
#77757 = SURFACE_STYLE_FILL_AREA ( #69783 ) ;
#77758 = CARTESIAN_POINT ( 'NONE',  ( 18.52753015748618282, 8.925597817667451750, -4.923371831947291888 ) ) ;
#77759 = CARTESIAN_POINT ( 'NONE',  ( 0.9940297508536876103, 15.00000000000000000, 14.21528771620250353 ) ) ;
#77760 = CARTESIAN_POINT ( 'NONE',  ( 0.1532563361054082862, 16.21726448433411960, 2.638427012816831674 ) ) ;
#77761 = CARTESIAN_POINT ( 'NONE',  ( 2.035157376598822676, 37.43868534415484106, -7.964842623401177768 ) ) ;
#77762 = AXIS2_PLACEMENT_3D ( 'NONE', #41926, #17932, #48905 ) ;
#77763 = EDGE_CURVE ( 'NONE', #86159, #43937, #49733, .T. ) ;
#77764 = VECTOR ( 'NONE', #63998, 1000.000000000000000 ) ;
#77765 = AXIS2_PLACEMENT_3D ( 'NONE', #22150, #30120, #44134 ) ;
#77766 = VERTEX_POINT ( 'NONE', #50740 ) ;
#77767 = CARTESIAN_POINT ( 'NONE',  ( -2.816281873526473856, 64.33196800326376774, 3.434112377981055619 ) ) ;
#77768 = CARTESIAN_POINT ( 'NONE',  ( 7.084665262690076126, 54.10535201082151247, 10.88017736071109987 ) ) ;
#77769 = DIRECTION ( 'NONE',  ( 0.000000000000000000, 0.000000000000000000, -1.000000000000000000 ) ) ;
#77770 = SURFACE_STYLE_FILL_AREA ( #94245 ) ;
#77771 = CARTESIAN_POINT ( 'NONE',  ( 10.00000000000000178, 64.31368534415483396, 10.88017736071110342 ) ) ;
#77772 = CARTESIAN_POINT ( 'NONE',  ( 22.81628187352648496, 11.83196800326375531, -3.434112377981050290 ) ) ;
#77773 = DIRECTION ( 'NONE',  ( 0.000000000000000000, 0.000000000000000000, 1.000000000000000000 ) ) ;
#77774 = CARTESIAN_POINT ( 'NONE',  ( 12.63842701281683922, 29.55059781766745175, -9.846743663894590881 ) ) ;
#77775 = CARTESIAN_POINT ( 'NONE',  ( 22.81628187352647785, 61.41530133659709634, 3.434112377981063169 ) ) ;
#77776 = CARTESIAN_POINT ( 'NONE',  ( 20.36894250292379382, 13.67874883491396965, 10.36894250292379205 ) ) ;
#77777 = CARTESIAN_POINT ( 'NONE',  ( 10.00000000000000000, 19.75893115100078390, -9.846743663894594434 ) ) ;
#77778 = CARTESIAN_POINT ( 'NONE',  ( 21.09922568453594849, 16.20696800326375353, 6.408140936763242479 ) ) ;
#77779 = ADVANCED_FACE ( 'NONE', ( #12234 ), #72242, .T. ) ;
#77781 = CLOSED_SHELL ( 'NONE', ( #98824, #5806, #53984, #3619, #68830, #50856, #16760, #50009, #30764, #68443, #26127, #47403, #94843, #85675, #59803, #95150, #12876, #77838, #86498, #21933, #59355, #16265, #14578, #2442 ) ) ;
#77780 = FACE_OUTER_BOUND ( 'NONE', #72468, .T. ) ;
#77782 = CARTESIAN_POINT ( 'NONE',  ( -0.8801773607111009756, 53.06368534415484106, 1.068504757029289695E-15 ) ) ;
#77783 = CARTESIAN_POINT ( 'NONE',  ( 18.52753015748618282, 58.92559781766745886, -4.923371831947291888 ) ) ;
#77784 = CARTESIAN_POINT ( 'NONE',  ( -0.1503990784575277573, 33.10158574516643171, 6.262539305110076171 ) ) ;
#77785 = CARTESIAN_POINT ( 'NONE',  ( 10.00000000000000178, 27.25893115100078390, 9.846743663894594434 ) ) ;
#77786 = CARTESIAN_POINT ( 'NONE',  ( 10.00000000000000178, 9.313685344154839285, 10.88017736071110342 ) ) ;
#77787 = CARTESIAN_POINT ( 'NONE',  ( 16.40814093676324603, 22.45696800326375353, -11.09922568453594671 ) ) ;
#77788 = CARTESIAN_POINT ( 'NONE',  ( 18.52753015748617571, 28.09226448433411960, 4.923371831947298993 ) ) ;
#77789 =( NAMED_UNIT ( * ) PLANE_ANGLE_UNIT ( ) SI_UNIT ( $, .RADIAN. ) );
#77790 = FACE_OUTER_BOUND ( 'NONE', #7060, .T. ) ;
#77791 = EDGE_CURVE ( 'NONE', #65924, #7321, #77197, .T. ) ;
#77792 = CARTESIAN_POINT ( 'NONE',  ( 4.559911319644449179, 18.89701867748817321, 9.422509992056141925 ) ) ;
#77793 = ADVANCED_FACE ( 'NONE', ( #87737 ), #57239, .F. ) ;
#77795 = CARTESIAN_POINT ( 'NONE',  ( 4.559911319644449179, 12.23035201082150714, -9.422509992056141925 ) ) ;
#77794 = CARTESIAN_POINT ( 'NONE',  ( 19.84674366389459266, 48.30059781766745175, 2.638427012816836559 ) ) ;
#77796 = CARTESIAN_POINT ( 'NONE',  ( -5.810202895580550475, 14.95077488074853456, 13.56051778013760689 ) ) ;
#77797 = CARTESIAN_POINT ( 'NONE',  ( -0.8801773607111008646, 33.27201867748817676, 2.915334737309923430 ) ) ;
#77798 = CARTESIAN_POINT ( 'NONE',  ( 7.084665262690076126, 14.10535201082150358, 10.88017736071109987 ) ) ;
#77799 = CARTESIAN_POINT ( 'NONE',  ( 2.791683348922237240, 20.38393115100078745, -7.208316651077763204 ) ) ;
#77800 = CARTESIAN_POINT ( 'NONE',  ( 19.84674366389459266, 38.71726448433412315, -2.638427012816827677 ) ) ;
#77801 = LINE ( 'NONE', #9314, #84878 ) ;
#77802 = CARTESIAN_POINT ( 'NONE',  ( 12.63842701281683922, 64.55059781766745175, -9.846743663894590881 ) ) ;
#77803 =( NAMED_UNIT ( * ) SI_UNIT ( $, .STERADIAN. ) SOLID_ANGLE_UNIT ( ) );
#77804 = CARTESIAN_POINT ( 'NONE',  ( -7.778994393791476725, -1.060811710739452796, -4.000000000000000000 ) ) ;
#77805 = CARTESIAN_POINT ( 'NONE',  ( 6.204703633549690345, 27.84541550158063217, 14.16423886937410082 ) ) ;
#77806 = CARTESIAN_POINT ( 'NONE',  ( 19.84674366389459266, 33.71726448433410894, -2.638427012816827677 ) ) ;
#77807 = DIRECTION ( 'NONE',  ( -0.000000000000000000, 1.000000000000000000, -0.000000000000000000 ) ) ;
#77808 = ORIENTED_EDGE ( 'NONE', *, *, #92002, .T. ) ;
#77809 = CARTESIAN_POINT ( 'NONE',  ( 17.08211943468705130, 53.47041550158063217, 12.26659068614894998 ) ) ;
#77810 = CARTESIAN_POINT ( 'NONE',  ( 17.20831665107776587, 19.13393115100078035, -7.208316651077762316 ) ) ;
#77812 = CARTESIAN_POINT ( 'NONE',  ( -7.750355510519348456, 84.07179676972448590, -4.000000000000000000 ) ) ;
#77811 = DIRECTION ( 'NONE',  ( 0.8788171126619646056, 0.000000000000000000, 0.4771587602596096267 ) ) ;
#77813 = CARTESIAN_POINT ( 'NONE',  ( 12.91533473730992121, 49.52201867748817676, 10.88017736071110164 ) ) ;
#77814 = CARTESIAN_POINT ( 'NONE',  ( 3.384800920124074075, 14.76930270348881180, 14.55270344038010322 ) ) ;
#77815 = ORIENTED_EDGE ( 'NONE', *, *, #90094, .F. ) ;
#77816 = CARTESIAN_POINT ( 'NONE',  ( 15.44008868035555260, 14.73035201082150536, 9.422509992056143702 ) ) ;
#77817 = CARTESIAN_POINT ( 'NONE',  ( 3.591859063236763294, 53.29030133659708923, -11.09922568453595026 ) ) ;
#77818 = CARTESIAN_POINT ( 'NONE',  ( 3.591859063236763294, 13.29030133659708746, -11.09922568453595026 ) ) ;
#77819 = CARTESIAN_POINT ( 'NONE',  ( 17.20831665107776587, 12.88393115100078390, 7.208316651077764980 ) ) ;
#77820 = EDGE_LOOP ( 'NONE', ( #82646, #1672, #86393, #37562 ) ) ;
#77821 = DIRECTION ( 'NONE',  ( -0.000000000000000000, -1.000000000000000000, -0.000000000000000000 ) ) ;
#77822 = CARTESIAN_POINT ( 'NONE',  ( -0.03447792253739259682, 20.15514106990689669, 6.401564815979746470 ) ) ;
#77823 = CARTESIAN_POINT ( 'NONE',  ( 17.08211943468705130, 48.47041550158063927, 12.26659068614894998 ) ) ;
#77824 = CARTESIAN_POINT ( 'NONE',  ( -2.266590686148945544, 16.38708216824730357, -7.082119434687050408 ) ) ;
#77825 = CARTESIAN_POINT ( 'NONE',  ( 19.42250999205614548, 20.98035201082150891, -5.440088680355545492 ) ) ;
#77826 = VECTOR ( 'NONE', #16056, 999.9999999999998863 ) ;
#77827 = CARTESIAN_POINT ( 'NONE',  ( 17.96484262340118221, 34.93868534415482685, 7.964842623401181321 ) ) ;
#77828 = CARTESIAN_POINT ( 'NONE',  ( 13.82192141328809676, 4.465570197798056962E-16, 4.382292601468775750 ) ) ;
#77829 = EDGE_CURVE ( 'NONE', #52174, #26555, #79755, .T. ) ;
#77830 = CYLINDRICAL_SURFACE ( 'NONE', #81549, 2.000000000000001776 ) ;
#77831 = CARTESIAN_POINT ( 'NONE',  ( 0.5774900079438607392, 63.48035201082149825, 5.440088680355550821 ) ) ;
#77832 = CARTESIAN_POINT ( 'NONE',  ( 7.361572987183169658, 19.96726448433411960, -9.846743663894592657 ) ) ;
#77833 = CARTESIAN_POINT ( 'NONE',  ( -19.89999999999999858, 0.000000000000000000, 8.000000000000000000 ) ) ;
#77834 = CYLINDRICAL_SURFACE ( 'NONE', #21233, 0.2500000000000002220 ) ;
#77835 = CARTESIAN_POINT ( 'NONE',  ( 7.361572987183169658, 9.967264484334119601, -9.846743663894592657 ) ) ;
#77836 = CARTESIAN_POINT ( 'NONE',  ( 7.361572987183169658, 39.96726448433411605, -9.846743663894592657 ) ) ;
#77837 = CIRCLE ( 'NONE', #37958, 0.2500000000000002220 ) ;
#77838 = ADVANCED_FACE ( 'NONE', ( #64726 ), #11253, .T. ) ;
#77839 = CARTESIAN_POINT ( 'NONE',  ( 12.91533473730993009, 16.60535201082150891, -10.88017736071109987 ) ) ;
#77840 = VECTOR ( 'NONE', #22712, 1000.000000000000000 ) ;
#77841 =( GEOMETRIC_REPRESENTATION_CONTEXT ( 3 ) GLOBAL_UNCERTAINTY_ASSIGNED_CONTEXT ( ( #31230 ) ) GLOBAL_UNIT_ASSIGNED_CONTEXT ( ( #91765, #38283, #309 ) ) REPRESENTATION_CONTEXT ( 'NONE', 'WORKASPACE' ) );
#77842 = CARTESIAN_POINT ( 'NONE',  ( 3.591859063236763294, 28.29030133659708568, -11.09922568453595026 ) ) ;
#77843 = CARTESIAN_POINT ( 'NONE',  ( 7.084665262690076126, 49.10535201082149825, 10.88017736071109987 ) ) ;
#77845 = CARTESIAN_POINT ( 'NONE',  ( 2.791683348922240793, 11.63393115100078568, 7.208316651077764092 ) ) ;
#77844 = CARTESIAN_POINT ( 'NONE',  ( -4.164238869374099039, 51.80374883491396787, 8.674139862899312516E-16 ) ) ;
#77846 = CARTESIAN_POINT ( 'NONE',  ( -7.750000000000000000, 41.24999999999999289, -4.250000000000000000 ) ) ;
#77847 = CARTESIAN_POINT ( 'NONE',  ( 19.84674366389459266, 48.30059781766745175, 2.638427012816836559 ) ) ;
#77849 = CARTESIAN_POINT ( 'NONE',  ( 6.204703633549690345, 7.845415501580634832, 14.16423886937410082 ) ) ;
#77848 = CARTESIAN_POINT ( 'NONE',  ( 7.361572987183169658, 29.96726448433411960, -9.846743663894592657 ) ) ;
#77850 = CARTESIAN_POINT ( 'NONE',  ( 22.26659068614894466, 23.88708216824730357, 7.082119434687054849 ) ) ;
#77851 = CARTESIAN_POINT ( 'NONE',  ( 10.00000000000000178, 44.31368534415484106, 10.88017736071110342 ) ) ;
#77852 = CARTESIAN_POINT ( 'NONE',  ( 7.084665262690076126, 14.10535201082150358, 10.88017736071109987 ) ) ;
#77853 = EDGE_CURVE ( 'NONE', #31539, #97319, #89712, .T. ) ;
#77854 = CARTESIAN_POINT ( 'NONE',  ( 7.084665262690076126, 39.10535201082150536, 10.88017736071109987 ) ) ;
#77855 = CARTESIAN_POINT ( 'NONE',  ( 7.084665262690076126, 29.10535201082150181, 10.88017736071109987 ) ) ;
#77856 = VERTEX_POINT ( 'NONE', #41771 ) ;
#77857 = CARTESIAN_POINT ( 'NONE',  ( -1.099225684535947600, 34.54030133659708923, 6.408140936763237150 ) ) ;
#77858 = CARTESIAN_POINT ( 'NONE',  ( 15.44008868035555260, 39.73035201082150536, 9.422509992056143702 ) ) ;
#77859 = VERTEX_POINT ( 'NONE', #72726 ) ;
#77860 = CARTESIAN_POINT ( 'NONE',  ( 6.565887622018943937, 63.08196800326376064, -12.81628187352647608 ) ) ;
#77861 = CARTESIAN_POINT ( 'NONE',  ( 20.88017736071110875, 45.77201867748816966, -2.915334737309920765 ) ) ;
#77862 = ORIENTED_EDGE ( 'NONE', *, *, #35008, .T. ) ;
#77863 = CARTESIAN_POINT ( 'NONE',  ( 12.91533473730992121, 54.52201867748816255, 10.88017736071110164 ) ) ;
#77864 = DIRECTION ( 'NONE',  ( -0.8320502943378437211, 0.5547001962252290364, 0.000000000000000000 ) ) ;
#77865 = DIRECTION ( 'NONE',  ( 0.6246950475544237324, 0.7808688094430306093, 0.000000000000000000 ) ) ;
#77866 = PLANE ( 'NONE',  #74813 ) ;
#77867 = CARTESIAN_POINT ( 'NONE',  ( 22.26659068614894466, 63.88708216824730357, 7.082119434687054849 ) ) ;
#77868 = CARTESIAN_POINT ( 'NONE',  ( 2.791683348922237240, 0.3839311510007847872, -7.208316651077763204 ) ) ;
#77869 = CARTESIAN_POINT ( 'NONE',  ( 2.917880565312950480, 0.9704155015806342766, -12.26659068614894821 ) ) ;
#77870 = CARTESIAN_POINT ( 'NONE',  ( -7.232415441807423129, -88.12698951299773853, -4.000000000000000000 ) ) ;
#77871 = CARTESIAN_POINT ( 'NONE',  ( 15.44008868035555260, 14.73035201082150536, 9.422509992056143702 ) ) ;
#77872 = CARTESIAN_POINT ( 'NONE',  ( 2.791683348922240793, 51.63393115100078745, 7.208316651077764092 ) ) ;
#77873 = ORIENTED_EDGE ( 'NONE', *, *, #85796, .T. ) ;
#77874 = CARTESIAN_POINT ( 'NONE',  ( 1.472469842513823179, 50.59226448433411605, -4.923371831947296329 ) ) ;
#77875 = AXIS2_PLACEMENT_3D ( 'NONE', #14737, #45213, #75711 ) ;
#77876 = CARTESIAN_POINT ( 'NONE',  ( -0.8801773607111008646, 33.27201867748817676, 2.915334737309923430 ) ) ;
#77877 = CARTESIAN_POINT ( 'NONE',  ( 1.472469842513823179, 40.59226448433411605, -4.923371831947296329 ) ) ;
#77879 = CARTESIAN_POINT ( 'NONE',  ( 20.88017736071110164, 65.35535201082150536, 2.915334737309930979 ) ) ;
#77878 = CARTESIAN_POINT ( 'NONE',  ( -15.94000000000001371, 93.50000000000000000, -10.09898361729590199 ) ) ;
#77880 = CARTESIAN_POINT ( 'NONE',  ( 0.5774900079438590739, 47.64701867748817676, -5.440088680355550821 ) ) ;
#77881 = CARTESIAN_POINT ( 'NONE',  ( 24.16423886937409904, 64.09541550158064638, 3.795296366450317205 ) ) ;
#77882 = EDGE_CURVE ( 'NONE', #10063, #29181, #22773, .T. ) ;
#77883 = AXIS2_PLACEMENT_3D ( 'NONE', #66553, #97569, #45526 ) ;
#77884 = CARTESIAN_POINT ( 'NONE',  ( 21.09922568453594849, 26.20696800326375353, 6.408140936763242479 ) ) ;
#77885 = CARTESIAN_POINT ( 'NONE',  ( 0.1532563361054083140, 51.00893115100078745, 1.131784320476157264E-15 ) ) ;
#77886 = EDGE_CURVE ( 'NONE', #12702, #83059, #34229, .T. ) ;
#77887 = VERTEX_POINT ( 'NONE', #51226 ) ;
#77888 = CARTESIAN_POINT ( 'NONE',  ( 6.565887622018943937, 30.16530133659708568, 12.81628187352647430 ) ) ;
#77889 = CARTESIAN_POINT ( 'NONE',  ( 15.44008868035555260, 24.73035201082150891, 9.422509992056143702 ) ) ;
#77890 = ORIENTED_EDGE ( 'NONE', *, *, #56253, .T. ) ;
#77891 = VECTOR ( 'NONE', #74163, 1000.000000000000000 ) ;
#77892 = CARTESIAN_POINT ( 'NONE',  ( 4.559911319644449179, 67.23035201082150536, -9.422509992056141925 ) ) ;
#77893 = CARTESIAN_POINT ( 'NONE',  ( 18.52753015748618282, 53.92559781766745175, -4.923371831947291888 ) ) ;
#77894 = EDGE_CURVE ( 'NONE', #26787, #18967, #59640, .T. ) ;
#77896 = CARTESIAN_POINT ( 'NONE',  ( 1.472469842513823179, 41.42559781766745886, 4.923371831947296329 ) ) ;
#77895 = CARTESIAN_POINT ( 'NONE',  ( 12.63842701281683034, 12.46726448433411782, 9.846743663894596210 ) ) ;
#77897 = CARTESIAN_POINT ( 'NONE',  ( -10.77730536144846596, -98.63085534186639336, 3.750000000000000000 ) ) ;
#77898 = DIRECTION ( 'NONE',  ( 0.000000000000000000, 0.000000000000000000, 1.000000000000000000 ) ) ;
#77899 = CARTESIAN_POINT ( 'NONE',  ( 14.92337183194729988, 24.34226448433411960, -8.527530157486177487 ) ) ;
#77900 = CARTESIAN_POINT ( 'NONE',  ( -42.94000000000001194, 92.50000000000000000, 9.500000000000000000 ) ) ;
#77901 = DIRECTION ( 'NONE',  ( 1.000000000000000000, 1.483861936729427615E-16, 0.000000000000000000 ) ) ;
#77904 = DIRECTION ( 'NONE',  ( 0.000000000000000000, 0.000000000000000000, 1.000000000000000000 ) ) ;
#77903 = VECTOR ( 'NONE', #90471, 999.9999999999998863 ) ;
#77902 = CARTESIAN_POINT ( 'NONE',  ( 0.1532563361054083140, 26.00893115100078745, 1.131784320476157264E-15 ) ) ;
#77905 = DIRECTION ( 'NONE',  ( 1.000000000000000000, 0.000000000000000000, 0.000000000000000000 ) ) ;
#77907 = ORIENTED_EDGE ( 'NONE', *, *, #3089, .F. ) ;
#77906 = CARTESIAN_POINT ( 'NONE',  ( 19.84674366389459266, 48.30059781766745175, 2.638427012816836559 ) ) ;
#77908 = AXIS2_PLACEMENT_3D ( 'NONE', #58170, #95191, #20189 ) ;
#77909 = LINE ( 'NONE', #9419, #23043 ) ;
#77910 = CARTESIAN_POINT ( 'NONE',  ( 22.81628187352647785, 31.41530133659709279, 3.434112377981063169 ) ) ;
#77911 = ADVANCED_FACE ( 'NONE', ( #65722 ), #96248, .T. ) ;
#77912 = CARTESIAN_POINT ( 'NONE',  ( -3.750000000000000888, 1.019547802438465212, -4.000000000000000000 ) ) ;
#77913 = CARTESIAN_POINT ( 'NONE',  ( 22.26659068614895176, 49.72041550158063927, -7.082119434687042414 ) ) ;
#77914 = CARTESIAN_POINT ( 'NONE',  ( 1.472469842513823179, 15.59226448433411960, -4.923371831947296329 ) ) ;
#77915 = B_SPLINE_CURVE_WITH_KNOTS ( 'NONE', 3,
 ( #60678, #37702, #89699, #82198, #36716, #90188 ),
 .UNSPECIFIED., .F., .F.,
 ( 4, 2, 4 ),
 ( 8.777993292121407760E-20, 0.0004057005074147807607, 0.0008114010148295614129 ),
 .UNSPECIFIED. ) ;
#77916 = CARTESIAN_POINT ( 'NONE',  ( 19.72487221294571569, 45.71833443783938122, -6.499999999999989342 ) ) ;
#77917 = CARTESIAN_POINT ( 'NONE',  ( -14.16722289976688565, 0.5000000000000004441, 4.928467845925418089 ) ) ;
#77918 = EDGE_CURVE ( 'NONE', #54753, #13947, #35728, .T. ) ;
#77919 = CARTESIAN_POINT ( 'NONE',  ( 13.79529636645030344, 43.26208216824730357, 14.16423886937410614 ) ) ;
#77920 = CARTESIAN_POINT ( 'NONE',  ( 10.00000000000000000, 64.75893115100078035, -9.846743663894594434 ) ) ;
#77921 = CARTESIAN_POINT ( 'NONE',  ( 2.917880565312950480, 60.97041550158063927, -12.26659068614894821 ) ) ;
#77922 = CARTESIAN_POINT ( 'NONE',  ( 2.917880565312948704, 22.63708216824730002, 12.26659068614894643 ) ) ;
#77923 = CARTESIAN_POINT ( 'NONE',  ( -2.266590686148945544, 21.38708216824730357, -7.082119434687050408 ) ) ;
#77924 = LINE ( 'NONE', #17443, #61137 ) ;
#77926 = CARTESIAN_POINT ( 'NONE',  ( 14.92337183194729988, 59.34226448433412315, -8.527530157486177487 ) ) ;
#77925 = CARTESIAN_POINT ( 'NONE',  ( 4.669733657693289963, -13.81599790096684899, 2.500000000000000000 ) ) ;
#77927 = EDGE_LOOP ( 'NONE', ( #7793, #91633, #1530, #4611 ) ) ;
#77928 = CARTESIAN_POINT ( 'NONE',  ( 0.5774900079438607392, 38.48035201082150536, 5.440088680355550821 ) ) ;
#77929 = DIRECTION ( 'NONE',  ( 0.000000000000000000, 0.000000000000000000, 1.000000000000000000 ) ) ;
#77930 = CARTESIAN_POINT ( 'NONE',  ( 19.59355889808634643, 95.39896427371951404, -5.130931023488903620 ) ) ;
#77931 = CARTESIAN_POINT ( 'NONE',  ( 19.84674366389459266, 38.71726448433412315, -2.638427012816827677 ) ) ;
#77932 = CARTESIAN_POINT ( 'NONE',  ( 3.591859063236763294, 53.29030133659708923, -11.09922568453595026 ) ) ;
#77933 = CARTESIAN_POINT ( 'NONE',  ( -3.795296366450322534, -4.237917831752698206, -14.16423886937409904 ) ) ;
#77934 = CARTESIAN_POINT ( 'NONE',  ( 14.92337183194729988, 39.34226448433412315, -8.527530157486177487 ) ) ;
#77935 = CARTESIAN_POINT ( 'NONE',  ( -3.750000000000000000, 36.75000000000000000, 3.750000000000000000 ) ) ;
#77936 = B_SPLINE_CURVE_WITH_KNOTS ( 'NONE', 3,
 ( #85431, #34377, #95387, #47422, #93420, #1954, #78415, #66355 ),
 .UNSPECIFIED., .F., .F.,
 ( 4, 2, 2, 4 ),
 ( 0.000000000000000000, 0.002747544437249704527, 0.004121316655874556791, 0.005495088874499409054 ),
 .UNSPECIFIED. ) ;
#77937 = ORIENTED_EDGE ( 'NONE', *, *, #39969, .T. ) ;
#77938 = B_SPLINE_CURVE_WITH_KNOTS ( 'NONE', 3,
 ( #15881, #54832, #68388, #91868, #8853, #83872 ),
 .UNSPECIFIED., .F., .F.,
 ( 4, 2, 4 ),
 ( 0.0002800808511900510487, 0.0006862868719403119808, 0.001092492892690572750 ),
 .UNSPECIFIED. ) ;
#77939 = CARTESIAN_POINT ( 'NONE',  ( -2.266590686148945544, 12.22041550158063394, 7.082119434687048631 ) ) ;
#77940 = CARTESIAN_POINT ( 'NONE',  ( 19.72487221294570858, 70.00000000000000000, 6.500000000000000888 ) ) ;
#77942 = CARTESIAN_POINT ( 'NONE',  ( -8.813102413619921194, 15.00000000000000000, -13.34940531570976496 ) ) ;
#77941 = CARTESIAN_POINT ( 'NONE',  ( -3.750000000000000000, 37.25000000000000000, -4.000000000000000000 ) ) ;
#77943 = CARTESIAN_POINT ( 'NONE',  ( 15.44008868035555793, 6.397018677488171434, -9.422509992056140149 ) ) ;
#77944 = CARTESIAN_POINT ( 'NONE',  ( 22.81628187352647785, 6.415301336597088344, 3.434112377981063169 ) ) ;
#77945 = CARTESIAN_POINT ( 'NONE',  ( 21.92686044187657046, 2.396642702460841434, -3.195792623639524432 ) ) ;
#77946 = CARTESIAN_POINT ( 'NONE',  ( 20.88017736071110875, 65.77201867748817676, -2.915334737309920765 ) ) ;
#77947 = SURFACE_SIDE_STYLE ('',( #991 ) ) ;
#77948 = CARTESIAN_POINT ( 'NONE',  ( -46.94000000000126960, 101.3832071409885884, -8.175121524388728744 ) ) ;
#77949 = CARTESIAN_POINT ( 'NONE',  ( 2.897438467171757030E-16, 23.03999999999999915, 0.000000000000000000 ) ) ;
#77950 = CARTESIAN_POINT ( 'NONE',  ( 22.26659068614894466, 58.88708216824729647, 7.082119434687054849 ) ) ;
#77951 = DIRECTION ( 'NONE',  ( -0.000000000000000000, 1.000000000000000000, 0.000000000000000000 ) ) ;
#77952 = CARTESIAN_POINT ( 'NONE',  ( 2.035157376598822676, 32.43868534415483396, -7.964842623401177768 ) ) ;
#77953 = CARTESIAN_POINT ( 'NONE',  ( -0.8801773607111009756, 38.06368534415484106, 1.068504757029289695E-15 ) ) ;
#77954 = CARTESIAN_POINT ( 'NONE',  ( -2.816281873526473856, 4.123634669930420493, 9.499525473075851096E-16 ) ) ;
#77955 = CARTESIAN_POINT ( 'NONE',  ( 14.92337183194729633, 47.67559781766745175, 8.527530157486181039 ) ) ;
#77956 = CARTESIAN_POINT ( 'NONE',  ( -2.816281873526471635, 58.91530133659707502, -3.434112377981056508 ) ) ;
#77957 = FILL_AREA_STYLE ('',( #85966 ) ) ;
#77958 = ORIENTED_EDGE ( 'NONE', *, *, #13039, .F. ) ;
#77959 = CARTESIAN_POINT ( 'NONE',  ( 15.44008868035555793, 36.39701867748816966, -9.422509992056140149 ) ) ;
#77960 = EDGE_CURVE ( 'NONE', #63027, #54853, #35341, .T. ) ;
#77961 = CARTESIAN_POINT ( 'NONE',  ( 13.43411237798106583, 32.66530133659708213, -12.81628187352647252 ) ) ;
#77962 = CARTESIAN_POINT ( 'NONE',  ( -0.1503990784575328643, 55.12777174578612716, 6.262539305110068177 ) ) ;
#77963 =( GEOMETRIC_REPRESENTATION_CONTEXT ( 3 ) GLOBAL_UNCERTAINTY_ASSIGNED_CONTEXT ( ( #47202 ) ) GLOBAL_UNIT_ASSIGNED_CONTEXT ( ( #78487, #23042, #84027 ) ) REPRESENTATION_CONTEXT ( 'NONE', 'WORKASPACE' ) );
#77964 = CARTESIAN_POINT ( 'NONE',  ( 10.00000000000000178, 57.25893115100078745, 9.846743663894594434 ) ) ;
#77965 = CARTESIAN_POINT ( 'NONE',  ( 4.559911319644449179, 53.89701867748817676, 9.422509992056141925 ) ) ;
#77966 = CARTESIAN_POINT ( 'NONE',  ( 21.09922568453594849, 41.20696800326375353, 6.408140936763242479 ) ) ;
#77968 = DIRECTION ( 'NONE',  ( -0.8073289077886854903, 0.5901017155107486367, 0.000000000000000000 ) ) ;
#77967 = CARTESIAN_POINT ( 'NONE',  ( 12.91533473730993009, 61.60535201082150536, -10.88017736071109987 ) ) ;
#77969 = DIRECTION ( 'NONE',  ( -0.000000000000000000, -1.000000000000000000, -0.000000000000000000 ) ) ;
#77970 = CARTESIAN_POINT ( 'NONE',  ( 0.6178305044545838731, 59.74863466993041783, 9.382169495545420901 ) ) ;
#77971 = VERTEX_POINT ( 'NONE', #13722 ) ;
#77972 = SURFACE_SIDE_STYLE ('',( #93469 ) ) ;
#77973 = FACE_OUTER_BOUND ( 'NONE', #8625, .T. ) ;
#77974 = CARTESIAN_POINT ( 'NONE',  ( 20.88017736071110164, 10.35535201082150714, 2.915334737309930979 ) ) ;
#77976 = CARTESIAN_POINT ( 'NONE',  ( -4.164238869374099927, 12.01208216824730357, 3.795296366450308767 ) ) ;
#77975 = CARTESIAN_POINT ( 'NONE',  ( -2.816281873526471635, 48.91530133659708213, -3.434112377981056508 ) ) ;
#77977 = CARTESIAN_POINT ( 'NONE',  ( 7.361572987183169658, 19.96726448433411960, -9.846743663894592657 ) ) ;
#77978 = CARTESIAN_POINT ( 'NONE',  ( 2.035157376598824452, 8.688685344154839285, 7.964842623401179544 ) ) ;
#77979 = CARTESIAN_POINT ( 'NONE',  ( 12.63842701281683922, 14.55059781766744997, -9.846743663894590881 ) ) ;
#77980 = CARTESIAN_POINT ( 'NONE',  ( 6.204703633549690345, 55.76208216824730357, -14.16423886937410259 ) ) ;
#77981 = VERTEX_POINT ( 'NONE', #29695 ) ;
#77982 = CARTESIAN_POINT ( 'NONE',  ( -46.44000000000001194, 99.99999999999998579, 9.000000000000000000 ) ) ;
#77983 = AXIS2_PLACEMENT_3D ( 'NONE', #15461, #45942, #76432 ) ;
#77984 = CARTESIAN_POINT ( 'NONE',  ( 2.035157376598822676, 22.43868534415483396, -7.964842623401177768 ) ) ;
#77985 = CARTESIAN_POINT ( 'NONE',  ( 19.88701968852524615, 46.79427333184086280, 6.480634945678618308 ) ) ;
#77986 = CIRCLE ( 'NONE', #50860, 14.49999999999999822 ) ;
#77987 = ORIENTED_EDGE ( 'NONE', *, *, #63911, .F. ) ;
#77988 = ORIENTED_EDGE ( 'NONE', *, *, #47583, .T. ) ;
#77989 = CARTESIAN_POINT ( 'NONE',  ( 4.559911319644449179, 2.230352010821504916, -9.422509992056141925 ) ) ;
#77990 = CARTESIAN_POINT ( 'NONE',  ( 0.5774900079438590739, 12.64701867748817321, -5.440088680355550821 ) ) ;
#77991 = CARTESIAN_POINT ( 'NONE',  ( 7.361572987183170547, 47.05059781766745175, 9.846743663894590881 ) ) ;
#77992 = CARTESIAN_POINT ( 'NONE',  ( 6.565887622018943937, 55.16530133659709634, 12.81628187352647430 ) ) ;
#77993 = DIRECTION ( 'NONE',  ( 0.000000000000000000, 0.000000000000000000, -1.000000000000000000 ) ) ;
#77995 = CARTESIAN_POINT ( 'NONE',  ( -4.164238869374099039, 21.80374883491396787, 8.674139862899312516E-16 ) ) ;
#77994 = CARTESIAN_POINT ( 'NONE',  ( 19.84674366389459621, 63.50893115100078745, 7.409399052514197653E-17 ) ) ;
#77996 = CARTESIAN_POINT ( 'NONE',  ( 10.00000000000000178, 29.31368534415483751, 10.88017736071110342 ) ) ;
#77997 = CARTESIAN_POINT ( 'NONE',  ( 2.035157376598822676, 7.438685344154837509, -7.964842623401177768 ) ) ;
#77998 = CARTESIAN_POINT ( 'NONE',  ( 5.076628168052703671, 51.84226448433412315, 8.527530157486179263 ) ) ;
#77999 = CARTESIAN_POINT ( 'NONE',  ( 18.61655166652076687, 44.87718327197428181, 6.499999999999981348 ) ) ;
#78000 = CARTESIAN_POINT ( 'NONE',  ( 14.92337183194729633, 42.67559781766745886, 8.527530157486181039 ) ) ;
#78001 = FACE_OUTER_BOUND ( 'NONE', #70949, .T. ) ;
#78002 = CARTESIAN_POINT ( 'NONE',  ( 19.84674366389459621, 8.508931151000785675, 7.409399052514197653E-17 ) ) ;
#78003 = CARTESIAN_POINT ( 'NONE',  ( 4.923371831947295441, 29.34226448433413381, -8.527530157486179263 ) ) ;
#78004 = ORIENTED_EDGE ( 'NONE', *, *, #32334, .T. ) ;
#78005 =( NAMED_UNIT ( * ) PLANE_ANGLE_UNIT ( ) SI_UNIT ( $, .RADIAN. ) );
#78006 = CARTESIAN_POINT ( 'NONE',  ( 2.035157376598824452, 68.68868534415484817, 7.964842623401179544 ) ) ;
#78007 = CARTESIAN_POINT ( 'NONE',  ( 6.565887622018943937, 3.081968003263753531, -12.81628187352647608 ) ) ;
#78008 = CARTESIAN_POINT ( 'NONE',  ( 15.44008868035555793, 41.39701867748817676, -9.422509992056140149 ) ) ;
#78010 = CARTESIAN_POINT ( 'NONE',  ( 22.81628187352647785, 41.41530133659708923, 3.434112377981063169 ) ) ;
#78009 = CARTESIAN_POINT ( 'NONE',  ( 7.084665262690076126, 12.02201867748817143, -10.88017736071110164 ) ) ;
#78011 = CARTESIAN_POINT ( 'NONE',  ( 10.00000000000000178, 23.05374883491397142, 14.16423886937410082 ) ) ;
#78012 = ADVANCED_FACE ( 'NONE', ( #723 ), #6227, .F. ) ;
#78013 = ORIENTED_EDGE ( 'NONE', *, *, #21116, .F. ) ;
#78014 = EDGE_CURVE ( 'NONE', #11622, #89199, #14452, .T. ) ;
#78015 = CARTESIAN_POINT ( 'NONE',  ( 16.40814093676324603, 42.45696800326375353, -11.09922568453594671 ) ) ;
#78016 = EDGE_CURVE ( 'NONE', #45903, #42131, #52826, .T. ) ;
#78017 = ORIENTED_EDGE ( 'NONE', *, *, #46213, .F. ) ;
#78018 =( BOUNDED_CURVE ( )  B_SPLINE_CURVE ( 2, ( #74097, #75593, #89609, #6602, #90093, #75095, #21120, #67107, #45587 ),
 .UNSPECIFIED., .F., .T. ) 
 B_SPLINE_CURVE_WITH_KNOTS ( ( 3, 2, 2, 2, 3 ),
 ( 0.3667998787605536437, 0.3690476190476190688, 0.3750000000000000000, 0.3809523809523809312, 0.3832001212394454126 ),
 .UNSPECIFIED. ) 
 CURVE ( )  GEOMETRIC_REPRESENTATION_ITEM ( )  RATIONAL_B_SPLINE_CURVE ( ( 0.9839835555609424134, 0.9871328979762475919, 1.000000000000000000, 0.9659258262890683122, 1.000000000000000000, 0.9659258262890683122, 1.000000000000000000, 0.9871328979762530320, 0.9839835555609450779 ) ) 
 REPRESENTATION_ITEM ( '' )  );
#78019 = CARTESIAN_POINT ( 'NONE',  ( 17.20831665107776587, 52.88393115100078035, 7.208316651077764980 ) ) ;
#78020 = CARTESIAN_POINT ( 'NONE',  ( 7.084665262690076126, 22.02201867748817321, -10.88017736071110164 ) ) ;
#78021 = ORIENTED_EDGE ( 'NONE', *, *, #70002, .T. ) ;
#78022 = CARTESIAN_POINT ( 'NONE',  ( 10.00000000000000178, 29.31368534415483751, 10.88017736071110342 ) ) ;
#78023 = ORIENTED_EDGE ( 'NONE', *, *, #96478, .T. ) ;
#78024 = CARTESIAN_POINT ( 'NONE',  ( 2.791683348922237240, 10.38393115100078390, -7.208316651077763204 ) ) ;
#78025 = FACE_OUTER_BOUND ( 'NONE', #26639, .T. ) ;
#78026 = FACE_OUTER_BOUND ( 'NONE', #29087, .T. ) ;
#78027 = VECTOR ( 'NONE', #57166, 1000.000000000000000 ) ;
#78028 = CARTESIAN_POINT ( 'NONE',  ( 1.472469842513823179, 11.42559781766745175, 4.923371831947296329 ) ) ;
#78029 = CARTESIAN_POINT ( 'NONE',  ( 4.559911319644449179, 67.23035201082150536, -9.422509992056141925 ) ) ;
#78030 = CARTESIAN_POINT ( 'NONE',  ( -13.34343830728408697, 15.00000000000000000, 6.852200678592504701 ) ) ;
#78031 = CARTESIAN_POINT ( 'NONE',  ( 0.8952175423694819223, 38.52576239577081907, 5.990408912944316100 ) ) ;
#78032 = CARTESIAN_POINT ( 'NONE',  ( -0.8801773607111008646, 63.27201867748817676, 2.915334737309923430 ) ) ;
#78034 = ORIENTED_EDGE ( 'NONE', *, *, #26323, .F. ) ;
#78033 = CARTESIAN_POINT ( 'NONE',  ( 12.63842701281683922, 4.550597817667451750, -9.846743663894590881 ) ) ;
#78035 = CARTESIAN_POINT ( 'NONE',  ( 0.1532563361054083140, 61.00893115100078745, 1.131784320476157264E-15 ) ) ;
#78036 = ORIENTED_EDGE ( 'NONE', *, *, #23390, .T. ) ;
#78037 = ORIENTED_EDGE ( 'NONE', *, *, #23510, .F. ) ;
#78038 = CARTESIAN_POINT ( 'NONE',  ( -11.96291822454885612, 15.00000000000000000, 8.193813980848972278 ) ) ;
#78039 =( NAMED_UNIT ( * ) SI_UNIT ( $, .STERADIAN. ) SOLID_ANGLE_UNIT ( ) );
#78040 = CARTESIAN_POINT ( 'NONE',  ( 19.38216949554541557, 57.24863466993042493, -9.382169495545420901 ) ) ;
#78041 = EDGE_CURVE ( 'NONE', #16571, #15515, #95884, .T. ) ;
#78042 = CARTESIAN_POINT ( 'NONE',  ( -4.164238869374099039, 21.80374883491396787, 8.674139862899312516E-16 ) ) ;
#78043 = SURFACE_STYLE_USAGE ( .BOTH. , #24572 ) ;
#78045 = CARTESIAN_POINT ( 'NONE',  ( 12.91533473730992121, 59.52201867748816966, 10.88017736071110164 ) ) ;
#78044 = CARTESIAN_POINT ( 'NONE',  ( -4.698669664746476293, 0.000000000000000000, -2.767727949825321332 ) ) ;
#78046 = CARTESIAN_POINT ( 'NONE',  ( -0.8801773607111008646, 18.27201867748817321, 2.915334737309923430 ) ) ;
#78047 = ORIENTED_EDGE ( 'NONE', *, *, #87137, .F. ) ;
#78048 = CARTESIAN_POINT ( 'NONE',  ( 0.1532563361054083140, 6.008931151000784787, 1.131784320476157264E-15 ) ) ;
#78049 = CARTESIAN_POINT ( 'NONE',  ( 10.00000000000000178, 7.258931151000785675, 9.846743663894594434 ) ) ;
#78050 = CARTESIAN_POINT ( 'NONE',  ( -2.816281873526473856, 29.33196800326376064, 3.434112377981055619 ) ) ;
#78051 = CARTESIAN_POINT ( 'NONE',  ( 18.52753015748617571, 43.09226448433412315, 4.923371831947298993 ) ) ;
#78052 =( GEOMETRIC_REPRESENTATION_CONTEXT ( 3 ) GLOBAL_UNCERTAINTY_ASSIGNED_CONTEXT ( ( #88295 ) ) GLOBAL_UNIT_ASSIGNED_CONTEXT ( ( #32216, #23772, #24741 ) ) REPRESENTATION_CONTEXT ( 'NONE', 'WORKASPACE' ) );
#78053 = LINE ( 'NONE', #91585, #26597 ) ;
#78054 = CARTESIAN_POINT ( 'NONE',  ( 0.6178305044545838731, 14.74863466993041783, 9.382169495545420901 ) ) ;
#78055 = AXIS2_PLACEMENT_3D ( 'NONE', #58935, #89435, #97951 ) ;
#78056 = CARTESIAN_POINT ( 'NONE',  ( -8.900000000000002132, 75.76920769491746910, -2.900000000000000355 ) ) ;
#78057 = CARTESIAN_POINT ( 'NONE',  ( 7.361572987183170547, 27.05059781766745175, 9.846743663894590881 ) ) ;
#78058 = CARTESIAN_POINT ( 'NONE',  ( 17.20831665107776587, 9.133931151000787452, -7.208316651077762316 ) ) ;
#78059 = ORIENTED_EDGE ( 'NONE', *, *, #57257, .F. ) ;
#78060 = ORIENTED_EDGE ( 'NONE', *, *, #56567, .T. ) ;
#78061 = CARTESIAN_POINT ( 'NONE',  ( 15.44008868035555260, 39.73035201082150536, 9.422509992056143702 ) ) ;
#78062 = CARTESIAN_POINT ( 'NONE',  ( -0.3689425029237881626, 37.42874883491396787, 10.36894250292379027 ) ) ;
#78063 = CARTESIAN_POINT ( 'NONE',  ( 5.076628168052704559, 40.17559781766745175, -8.527530157486179263 ) ) ;
#78064 = CARTESIAN_POINT ( 'NONE',  ( 10.00000000000000000, 14.75893115100078568, -9.846743663894594434 ) ) ;
#78066 = CARTESIAN_POINT ( 'NONE',  ( -6.445967608602039434, -48.01283281809150338, -2.750000000000000444 ) ) ;
#78065 = CARTESIAN_POINT ( 'NONE',  ( 19.38216949554541202, 55.99863466993041072, 9.382169495545424454 ) ) ;
#78067 = CARTESIAN_POINT ( 'NONE',  ( -0.8801773607111009756, 33.06368534415484106, 1.068504757029289695E-15 ) ) ;
#78068 = FACE_OUTER_BOUND ( 'NONE', #81510, .T. ) ;
#78069 = CARTESIAN_POINT ( 'NONE',  ( 3.591859063236763294, 28.29030133659708568, -11.09922568453595026 ) ) ;
#78070 = CARTESIAN_POINT ( 'NONE',  ( 12.63842701281683922, 44.55059781766745175, -9.846743663894590881 ) ) ;
#78071 = CARTESIAN_POINT ( 'NONE',  ( -7.964842623401179544, 7.438685344154837509, -7.964842623401174215 ) ) ;
#78072 = CARTESIAN_POINT ( 'NONE',  ( 22.81628187352647785, 46.41530133659708213, 3.434112377981063169 ) ) ;
#78073 = CARTESIAN_POINT ( 'NONE',  ( 4.838527690343618737, 14.49999999999999822, -14.19819177887726624 ) ) ;
#78075 = DIRECTION ( 'NONE',  ( 0.000000000000000000, 1.000000000000000000, 0.000000000000000000 ) ) ;
#78074 = CARTESIAN_POINT ( 'NONE',  ( 7.084665262690076126, 54.10535201082151247, 10.88017736071109987 ) ) ;
#78076 = COLOUR_RGB ( '', 0.66274510, 0.83137255, 0.94901961) ;
#78077 = CARTESIAN_POINT ( 'NONE',  ( -10.77984007285762047, -96.52126437879435628, 3.999999999999999112 ) ) ;
#78078 = DIRECTION ( 'NONE',  ( 0.9588197348681964938, 0.000000000000000000, -0.2840153447039108214 ) ) ;
#78079 = CARTESIAN_POINT ( 'NONE',  ( 19.42250999205614548, 55.98035201082150536, -5.440088680355545492 ) ) ;
#78080 = CARTESIAN_POINT ( 'NONE',  ( 2.035157376598822676, 62.43868534415483396, -7.964842623401177768 ) ) ;
#78081 = CYLINDRICAL_SURFACE ( 'NONE', #74432, 0.5000000000000004441 ) ;
#78082 = LINE ( 'NONE', #25589, #26868 ) ;
#78083 = CARTESIAN_POINT ( 'NONE',  ( 4.559911319644449179, 12.23035201082150714, -9.422509992056141925 ) ) ;
#78084 = CARTESIAN_POINT ( 'NONE',  ( 14.92337183194729988, 64.34226448433412315, -8.527530157486177487 ) ) ;
#78086 = CARTESIAN_POINT ( 'NONE',  ( 5.129999999999994564, 43.00000000000000711, -6.500000000000000888 ) ) ;
#78085 = CARTESIAN_POINT ( 'NONE',  ( 17.96484262340118221, 21.18868534415483396, -7.964842623401177768 ) ) ;
#78087 = FILL_AREA_STYLE_COLOUR ( '', #43296 ) ;
#78088 = CARTESIAN_POINT ( 'NONE',  ( 19.38216949554541202, 25.99863466993042138, 9.382169495545424454 ) ) ;
#78089 = ORIENTED_EDGE ( 'NONE', *, *, #6450, .F. ) ;
#78090 = CARTESIAN_POINT ( 'NONE',  ( 19.42250999205614193, 50.14701867748817676, 5.440088680355555262 ) ) ;
#78091 = CARTESIAN_POINT ( 'NONE',  ( 19.84674366389459266, 43.30059781766744464, 2.638427012816836559 ) ) ;
#78093 = CARTESIAN_POINT ( 'NONE',  ( 20.15039907845753575, 47.62777174578613426, -6.262539305110073506 ) ) ;
#78092 = CARTESIAN_POINT ( 'NONE',  ( -2.816281873526473856, 4.331968003263754419, 3.434112377981055619 ) ) ;
#78094 = CARTESIAN_POINT ( 'NONE',  ( 19.42250999205614548, 10.98035201082150358, -5.440088680355545492 ) ) ;
#78095 = CARTESIAN_POINT ( 'NONE',  ( 20.88017736071110519, 45.56368534415484106, 2.639326808657452039E-16 ) ) ;
#78096 = CARTESIAN_POINT ( 'NONE',  ( 13.79529636645031943, 55.34541550158062506, -14.16423886937409904 ) ) ;
#78097 = CARTESIAN_POINT ( 'NONE',  ( 17.20831665107776587, 44.13393115100078745, -7.208316651077762316 ) ) ;
#78098 = VECTOR ( 'NONE', #84734, 1000.000000000000000 ) ;
#78099 = CARTESIAN_POINT ( 'NONE',  ( 20.88017736071110875, 65.77201867748817676, -2.915334737309920765 ) ) ;
#78100 = CARTESIAN_POINT ( 'NONE',  ( 20.36894250292379382, 18.67874883491397142, 10.36894250292379205 ) ) ;
#78101 = EDGE_CURVE ( 'NONE', #83910, #11101, #67187, .T. ) ;
#78102 = UNCERTAINTY_MEASURE_WITH_UNIT (LENGTH_MEASURE( 1.000000000000000082E-05 ), #88765, 'distance_accuracy_value', 'NONE');
#78103 = LINE ( 'NONE', #34057, #15326 ) ;
#78104 = ORIENTED_EDGE ( 'NONE', *, *, #35000, .F. ) ;
#78105 = CARTESIAN_POINT ( 'NONE',  ( -4.164238869374098151, 31.59541550158063927, -3.795296366450310543 ) ) ;
#78106 = CARTESIAN_POINT ( 'NONE',  ( -4.164238869374098151, 41.59541550158061796, -3.795296366450310543 ) ) ;
#78107 = CARTESIAN_POINT ( 'NONE',  ( 2.791683348922237240, 5.383931151000785675, -7.208316651077763204 ) ) ;
#78108 = CARTESIAN_POINT ( 'NONE',  ( 13.43411237798105340, 20.58196800326374643, 12.81628187352647963 ) ) ;
#78109 = CARTESIAN_POINT ( 'NONE',  ( 12.63842701281683034, 57.46726448433411605, 9.846743663894596210 ) ) ;
#78110 = CARTESIAN_POINT ( 'NONE',  ( 3.420591144908545100, 0.5000000000000004441, -14.60477854057955938 ) ) ;
#78112 = CARTESIAN_POINT ( 'NONE',  ( -1.099225684535947600, 38.70696800326375353, -6.408140936763238038 ) ) ;
#78111 = CARTESIAN_POINT ( 'NONE',  ( 7.084665262690076126, 62.02201867748816966, -10.88017736071110164 ) ) ;
#78113 = CARTESIAN_POINT ( 'NONE',  ( 13.79529636645031943, 25.34541550158063572, -14.16423886937409904 ) ) ;
#78114 = CARTESIAN_POINT ( 'NONE',  ( 7.084665262690076126, 27.02201867748817676, -10.88017736071110164 ) ) ;
#78115 = CARTESIAN_POINT ( 'NONE',  ( 3.640395162852214650, 89.00000000000000000, 12.00000000000000000 ) ) ;
#78116 = CARTESIAN_POINT ( 'NONE',  ( 7.361572987183170547, 2.050597817667451750, 9.846743663894590881 ) ) ;
#78117 = AXIS2_PLACEMENT_3D ( 'NONE', #49758, #89787, #21303 ) ;
#78118 = CARTESIAN_POINT ( 'NONE',  ( 9.846743663894590881, -11.69940218233254114, 2.638427012816828565 ) ) ;
#78119 = ORIENTED_EDGE ( 'NONE', *, *, #16476, .T. ) ;
#78120 = DIRECTION ( 'NONE',  ( -0.9636304532086248376, 0.000000000000000000, 0.2672383760782501838 ) ) ;
#78122 = ADVANCED_FACE ( 'NONE', ( #45207 ), #74716, .F. ) ;
#78121 = CARTESIAN_POINT ( 'NONE',  ( 46.27857419604806211, 63.24738473459895260, -8.000000000000000000 ) ) ;
#78123 = ORIENTED_EDGE ( 'NONE', *, *, #77014, .F. ) ;
#78124 = CARTESIAN_POINT ( 'NONE',  ( 2.917880565312948704, 7.637082168247301794, 12.26659068614894643 ) ) ;
#78126 = CARTESIAN_POINT ( 'NONE',  ( 12.91533473730992121, 9.522018677488171434, 10.88017736071110164 ) ) ;
#78125 = CARTESIAN_POINT ( 'NONE',  ( -4.164238869374099927, 67.01208216824728936, 3.795296366450308767 ) ) ;
#78128 = CARTESIAN_POINT ( 'NONE',  ( -2.816281873526473856, 9.123634669930421381, 9.499525473075851096E-16 ) ) ;
#78127 = CARTESIAN_POINT ( 'NONE',  ( 5.076628168052703671, 41.84226448433411605, 8.527530157486179263 ) ) ;
#78129 = CARTESIAN_POINT ( 'NONE',  ( 0.000000000000000000, 14.49999999999999822, 0.000000000000000000 ) ) ;
#78130 = PRESENTATION_LAYER_ASSIGNMENT (  '', '', ( #14254 ) ) ;
#78131 = EDGE_CURVE ( 'NONE', #70674, #88822, #91192, .T. ) ;
#78132 = CARTESIAN_POINT ( 'NONE',  ( 0.6178305044545838731, 4.748634669930420493, 9.382169495545420901 ) ) ;
#78133 = ADVANCED_FACE ( 'NONE', ( #90699 ), #83705, .F. ) ;
#78134 = ORIENTED_EDGE ( 'NONE', *, *, #71148, .F. ) ;
#78135 = CARTESIAN_POINT ( 'NONE',  ( 10.00000000000000178, 48.05374883491396787, 14.16423886937410082 ) ) ;
#78136 = ORIENTED_EDGE ( 'NONE', *, *, #29682, .T. ) ;
#78137 = CARTESIAN_POINT ( 'NONE',  ( 6.204703633549690345, 62.84541550158063927, 14.16423886937410082 ) ) ;
#78138 = VERTEX_POINT ( 'NONE', #82709 ) ;
#78139 = CARTESIAN_POINT ( 'NONE',  ( 20.88017736071110164, 20.35535201082150891, 2.915334737309930979 ) ) ;
#78140 = CARTESIAN_POINT ( 'NONE',  ( 10.00000000000000000, 41.81368534415484106, -10.88017736071110342 ) ) ;
#78141 = CARTESIAN_POINT ( 'NONE',  ( 19.84674366389459621, 58.50893115100078745, 7.409399052514197653E-17 ) ) ;
#78142 = CARTESIAN_POINT ( 'NONE',  ( 19.42250999205614548, 40.98035201082150536, -5.440088680355545492 ) ) ;
#78143 = CARTESIAN_POINT ( 'NONE',  ( 15.44008868035555793, 66.39701867748817676, -9.422509992056140149 ) ) ;
#78144 = CARTESIAN_POINT ( 'NONE',  ( -0.8801773607111008646, 23.27201867748817676, 2.915334737309923430 ) ) ;
#78145 = VECTOR ( 'NONE', #32215, 999.9999999999998863 ) ;
#78146 = DIRECTION ( 'NONE',  ( 0.000000000000000000, 1.000000000000000000, 0.000000000000000000 ) ) ;
#78148 = ADVANCED_FACE ( 'NONE', ( #52704 ), #14227, .T. ) ;
#78147 = CARTESIAN_POINT ( 'NONE',  ( 0.1532563361054082862, 6.217264484334118713, 2.638427012816831674 ) ) ;
#78149 = CARTESIAN_POINT ( 'NONE',  ( -3.500000000000000444, 0.09224605989676173956, 2.750000000000000000 ) ) ;
#78150 = ORIENTED_EDGE ( 'NONE', *, *, #57339, .F. ) ;
#78151 = FILL_AREA_STYLE ('',( #23702 ) ) ;
#78152 = CARTESIAN_POINT ( 'NONE',  ( 0.1532563361054082862, 41.21726448433411605, 2.638427012816831674 ) ) ;
#78153 = CARTESIAN_POINT ( 'NONE',  ( -14.71525861348285957, 0.5000000000000004441, -2.908807992686776700 ) ) ;
#78154 = DIRECTION ( 'NONE',  ( 0.000000000000000000, -1.000000000000000000, 0.000000000000000000 ) ) ;
#78155 = EDGE_CURVE ( 'NONE', #55638, #1168, #37717, .T. ) ;
#78156 = DIRECTION ( 'NONE',  ( -0.000000000000000000, -1.000000000000000000, -0.000000000000000000 ) ) ;
#78157 = CARTESIAN_POINT ( 'NONE',  ( 0.000000000000000000, 35.00000000000000000, 0.000000000000000000 ) ) ;
#78158 = DIRECTION ( 'NONE',  ( 1.000000000000000000, 0.000000000000000000, 0.000000000000000000 ) ) ;
#78159 = CARTESIAN_POINT ( 'NONE',  ( 10.00000000000000000, 54.75893115100078745, -9.846743663894594434 ) ) ;
#78160 = CARTESIAN_POINT ( 'NONE',  ( 22.26659068614895176, 44.72041550158063927, -7.082119434687042414 ) ) ;
#78161 = CARTESIAN_POINT ( 'NONE',  ( 0.1532563361054100626, 65.80059781766745175, -2.638427012816831230 ) ) ;
#78162 = ORIENTED_EDGE ( 'NONE', *, *, #64, .F. ) ;
#78163 = DIRECTION ( 'NONE',  ( -0.000000000000000000, 1.000000000000000000, -0.000000000000000000 ) ) ;
#78164 = CARTESIAN_POINT ( 'NONE',  ( 2.791683348922240793, 21.63393115100078745, 7.208316651077764092 ) ) ;
#78165 = CARTESIAN_POINT ( 'NONE',  ( -2.816281873526473856, 54.33196800326376064, 3.434112377981055619 ) ) ;
#78166 = VECTOR ( 'NONE', #94796, 1000.000000000000000 ) ;
#78167 = CARTESIAN_POINT ( 'NONE',  ( 10.00000000000000000, 64.75893115100078035, -9.846743663894594434 ) ) ;
#78168 = CARTESIAN_POINT ( 'NONE',  ( 10.00000000000000000, 61.81368534415484106, -10.88017736071110342 ) ) ;
#78169 = CARTESIAN_POINT ( 'NONE',  ( 4.469999999999999751, 36.75000000000000000, -4.000000000000000000 ) ) ;
#78170 = ORIENTED_EDGE ( 'NONE', *, *, #43319, .T. ) ;
#78171 = CARTESIAN_POINT ( 'NONE',  ( -0.3689425029237881626, 67.42874883491396076, 10.36894250292379027 ) ) ;
#78172 = DIRECTION ( 'NONE',  ( 0.000000000000000000, 0.000000000000000000, 1.000000000000000000 ) ) ;
#78173 = CARTESIAN_POINT ( 'NONE',  ( 7.084665262690076126, 24.10535201082150181, 10.88017736071109987 ) ) ;
#78175 = CARTESIAN_POINT ( 'NONE',  ( 4.559911319644449179, 53.89701867748817676, 9.422509992056141925 ) ) ;
#78174 = CARTESIAN_POINT ( 'NONE',  ( 16.40814093676324603, 7.456968003263754419, -11.09922568453594671 ) ) ;
#78176 = CARTESIAN_POINT ( 'NONE',  ( -8.564643372776711061, 0.3639308585234187210, 12.31449893000738527 ) ) ;
#78177 = FILL_AREA_STYLE ('',( #47175 ) ) ;
#78178 = CARTESIAN_POINT ( 'NONE',  ( 11.34661744925197624, 54.08985607419764818, 0.000000000000000000 ) ) ;
#78179 = CARTESIAN_POINT ( 'NONE',  ( 10.00000000000000178, 52.25893115100078745, 9.846743663894594434 ) ) ;
#78180 = CARTESIAN_POINT ( 'NONE',  ( 10.00000000000000000, 4.758931151000784787, -9.846743663894594434 ) ) ;
#78181 = CARTESIAN_POINT ( 'NONE',  ( -7.964842623401172439, -36.31131465584515894, 7.964842623401183097 ) ) ;
#78182 = CARTESIAN_POINT ( 'NONE',  ( 13.43411237798105340, 5.581968003263753531, 12.81628187352647963 ) ) ;
#78184 = CARTESIAN_POINT ( 'NONE',  ( -0.1503990784575328643, 69.92552686551195507, -6.262539305110068177 ) ) ;
#78183 = CARTESIAN_POINT ( 'NONE',  ( -0.8801773607110991993, 17.85535201082150536, -2.915334737309923874 ) ) ;
#78185 = CARTESIAN_POINT ( 'NONE',  ( -4.164238869374098151, 41.59541550158061796, -3.795296366450310543 ) ) ;
#78186 = CARTESIAN_POINT ( 'NONE',  ( -4.164238869374098151, 36.59541550158063217, -3.795296366450310543 ) ) ;
#78187 = CARTESIAN_POINT ( 'NONE',  ( 4.559911319644449179, 3.897018677488171434, 9.422509992056141925 ) ) ;
#78188 = CARTESIAN_POINT ( 'NONE',  ( 1.472469842513823179, 35.59226448433412315, -4.923371831947296329 ) ) ;
#78189 = CARTESIAN_POINT ( 'NONE',  ( 5.076628168052704559, 20.17559781766745175, -8.527530157486179263 ) ) ;
#78190 = CARTESIAN_POINT ( 'NONE',  ( 17.96484262340118221, 19.93868534415484106, 7.964842623401181321 ) ) ;
#78191 = ORIENTED_EDGE ( 'NONE', *, *, #8687, .F. ) ;
#78192 = CARTESIAN_POINT ( 'NONE',  ( 17.20831665107776587, 39.13393115100079456, -7.208316651077762316 ) ) ;
#78193 = CARTESIAN_POINT ( 'NONE',  ( 10.00000000000000000, 41.81368534415484106, -10.88017736071110342 ) ) ;
#78194 = CARTESIAN_POINT ( 'NONE',  ( 17.20831665107776587, 57.88393115100078745, 7.208316651077764980 ) ) ;
#78196 = LINE ( 'NONE', #17714, #7281 ) ;
#78195 = CARTESIAN_POINT ( 'NONE',  ( -2.266590686148945544, 16.38708216824730357, -7.082119434687050408 ) ) ;
#78197 = LINE ( 'NONE', #9710, #88641 ) ;
#78198 = UNCERTAINTY_MEASURE_WITH_UNIT (LENGTH_MEASURE( 1.000000000000000082E-05 ), #36411, 'distance_accuracy_value', 'NONE');
#78199 = CARTESIAN_POINT ( 'NONE',  ( 7.361572987183169658, 14.96726448433411960, -9.846743663894592657 ) ) ;
#78200 = CARTESIAN_POINT ( 'NONE',  ( 22.81628187352647785, 51.41530133659708923, 3.434112377981063169 ) ) ;
#78201 = CARTESIAN_POINT ( 'NONE',  ( 7.361572987183169658, 49.96726448433410894, -9.846743663894592657 ) ) ;
#78202 = VERTEX_POINT ( 'NONE', #23215 ) ;
#78203 = FACE_OUTER_BOUND ( 'NONE', #81495, .T. ) ;
#78204 = CARTESIAN_POINT ( 'NONE',  ( 4.879999999999991900, 76.07179676972444327, -6.250000000000000000 ) ) ;
#78205 = CARTESIAN_POINT ( 'NONE',  ( 7.084665262690076126, 7.022018677488170546, -10.88017736071110164 ) ) ;
#78206 = CARTESIAN_POINT ( 'NONE',  ( 4.559911319644449179, 53.89701867748817676, 9.422509992056141925 ) ) ;
#78207 = CARTESIAN_POINT ( 'NONE',  ( 2.917880565312950480, 5.970415501580634832, -12.26659068614894821 ) ) ;
#78208 = CARTESIAN_POINT ( 'NONE',  ( 2.791683348922237240, 0.3839311510007847872, -7.208316651077763204 ) ) ;
#78209 = CARTESIAN_POINT ( 'NONE',  ( 7.361572987183169658, 44.96726448433412315, -9.846743663894592657 ) ) ;
#78210 = CARTESIAN_POINT ( 'NONE',  ( 12.91533473730992121, 19.52201867748816611, 10.88017736071110164 ) ) ;
#78211 = DIRECTION ( 'NONE',  ( 0.000000000000000000, 0.000000000000000000, 1.000000000000000000 ) ) ;
#78212 = CARTESIAN_POINT ( 'NONE',  ( 17.20831665107776587, 64.13393115100079456, -7.208316651077762316 ) ) ;
#78213 = EDGE_CURVE ( 'NONE', #77529, #97117, #90755, .T. ) ;
#78214 = CARTESIAN_POINT ( 'NONE',  ( 18.52753015748617571, 3.092264484334118269, 4.923371831947298993 ) ) ;
#78215 = UNCERTAINTY_MEASURE_WITH_UNIT (LENGTH_MEASURE( 1.000000000000000082E-05 ), #91181, 'distance_accuracy_value', 'NONE');
#78216 = CARTESIAN_POINT ( 'NONE',  ( 9.997910040112596874, 15.00000000000000000, -10.50199004140715253 ) ) ;
#78217 = ORIENTED_EDGE ( 'NONE', *, *, #46303, .F. ) ;
#78218 = EDGE_LOOP ( 'NONE', ( #44693, #32744, #61609, #36162 ) ) ;
#78219 = CARTESIAN_POINT ( 'NONE',  ( -1.915564264621232748, 15.00000000000000000, -14.37291249357993372 ) ) ;
#78220 = LINE ( 'NONE', #67903, #63851 ) ;
#78221 = CARTESIAN_POINT ( 'NONE',  ( -0.3689425029237898834, 1.178748834913967869, -10.36894250292378850 ) ) ;
#78222 = CARTESIAN_POINT ( 'NONE',  ( 10.00000000000000000, 40.55374883491397497, -14.16423886937410082 ) ) ;
#78223 = CARTESIAN_POINT ( 'NONE',  ( 0.1532563361054100626, 45.80059781766745886, -2.638427012816831230 ) ) ;
#78224 = CARTESIAN_POINT ( 'NONE',  ( 2.791683348922240793, 26.63393115100078745, 7.208316651077764092 ) ) ;
#78226 = CARTESIAN_POINT ( 'NONE',  ( 5.076628168052703671, 61.84226448433412315, 8.527530157486179263 ) ) ;
#78225 = CARTESIAN_POINT ( 'NONE',  ( 20.88017736071110164, 25.35535201082150891, 2.915334737309930979 ) ) ;
#78227 = DIRECTION ( 'NONE',  ( 0.000000000000000000, 1.000000000000000000, 0.000000000000000000 ) ) ;
#78228 = CARTESIAN_POINT ( 'NONE',  ( 10.00000000000000000, 60.55374883491397497, -14.16423886937410082 ) ) ;
#78229 = CARTESIAN_POINT ( 'NONE',  ( -8.000000000000000000, 0.000000000000000000, 3.750000000000000000 ) ) ;
#78230 = DIRECTION ( 'NONE',  ( -0.000000000000000000, 1.000000000000000000, 0.000000000000000000 ) ) ;
#78231 = CARTESIAN_POINT ( 'NONE',  ( -0.8801773607111008646, 68.27201867748817676, 2.915334737309923430 ) ) ;
#78232 = CARTESIAN_POINT ( 'NONE',  ( 19.84674366389459266, 13.30059781766745353, 2.638427012816836559 ) ) ;
#78233 = CARTESIAN_POINT ( 'NONE',  ( -7.080143328648152767, -69.54337233422636189, 3.750000000000000444 ) ) ;
#78234 = EDGE_LOOP ( 'NONE', ( #67280, #64927, #93993, #13089 ) ) ;
#78235 = CARTESIAN_POINT ( 'NONE',  ( 20.32896413005680358, 29.74545670184113888, 5.963430220938287007 ) ) ;
#78236 = VERTEX_POINT ( 'NONE', #68702 ) ;
#78237 = CARTESIAN_POINT ( 'NONE',  ( 17.20831665107776587, 29.13393115100078390, -7.208316651077762316 ) ) ;
#78238 = ORIENTED_EDGE ( 'NONE', *, *, #21581, .F. ) ;
#78239 = CARTESIAN_POINT ( 'NONE',  ( 13.79529636645031943, 30.34541550158063927, -14.16423886937409904 ) ) ;
#78240 = CARTESIAN_POINT ( 'NONE',  ( 19.84674366389459621, 23.50893115100078390, 7.409399052514197653E-17 ) ) ;
#78241 = CARTESIAN_POINT ( 'NONE',  ( 4.559911319644449179, 47.23035201082150536, -9.422509992056141925 ) ) ;
#78242 = DIRECTION ( 'NONE',  ( 0.000000000000000000, 0.000000000000000000, 1.000000000000000000 ) ) ;
#78243 = EDGE_LOOP ( 'NONE', ( #63517, #20595, #86506, #55626 ) ) ;
#78244 = CARTESIAN_POINT ( 'NONE',  ( 15.44008868035555260, 34.73035201082151247, 9.422509992056143702 ) ) ;
#78245 = EDGE_CURVE ( 'NONE', #3849, #85778, #234, .T. ) ;
#78246 = CARTESIAN_POINT ( 'NONE',  ( 12.60589901313217354, 14.63595249122788999, 8.129656208642140669 ) ) ;
#78247 = CARTESIAN_POINT ( 'NONE',  ( -6.408140936763232709, -5.043031996736238476, 11.09922568453595026 ) ) ;
#78248 = EDGE_CURVE ( 'NONE', #16062, #60724, #9659, .T. ) ;
#78249 = VERTEX_POINT ( 'NONE', #76684 ) ;
#78250 = CARTESIAN_POINT ( 'NONE',  ( 22.26659068614895176, 4.720415501580633943, -7.082119434687042414 ) ) ;
#78251 = VERTEX_POINT ( 'NONE', #69198 ) ;
#78252 = VERTEX_POINT ( 'NONE', #62656 ) ;
#78253 = ORIENTED_EDGE ( 'NONE', *, *, #66277, .F. ) ;
#78254 = CARTESIAN_POINT ( 'NONE',  ( 6.565887622018943937, 30.16530133659708568, 12.81628187352647430 ) ) ;
#78255 = CARTESIAN_POINT ( 'NONE',  ( 6.204703633549690345, 0.7620821682473009062, -14.16423886937410259 ) ) ;
#78256 = CARTESIAN_POINT ( 'NONE',  ( 18.52753015748618282, 3.925597817667451306, -4.923371831947291888 ) ) ;
#78257 = PRODUCT_RELATED_PRODUCT_CATEGORY ( 'part', '', ( #98572 ) ) ;
#78258 = CARTESIAN_POINT ( 'NONE',  ( 22.81628187352647785, 46.41530133659708213, 3.434112377981063169 ) ) ;
#78259 = DIRECTION ( 'NONE',  ( -0.000000000000000000, -0.000000000000000000, 1.000000000000000000 ) ) ;
#78260 = CARTESIAN_POINT ( 'NONE',  ( 17.20831665107776587, 32.88393115100078745, 7.208316651077764980 ) ) ;
#78261 = AXIS2_PLACEMENT_3D ( 'NONE', #93209, #25240, #46729 ) ;
#78262 = ORIENTED_EDGE ( 'NONE', *, *, #63333, .F. ) ;
#78263 = CARTESIAN_POINT ( 'NONE',  ( 20.24186590665278018, 65.59014588040358262, -6.114288769123040090 ) ) ;
#78264 = CARTESIAN_POINT ( 'NONE',  ( 0.5774900079438590739, 62.64701867748817676, -5.440088680355550821 ) ) ;
#78265 = FACE_OUTER_BOUND ( 'NONE', #9330, .T. ) ;
#78266 = ADVANCED_FACE ( 'NONE', ( #31669 ), #70403, .F. ) ;
#78267 = CARTESIAN_POINT ( 'NONE',  ( 14.92337183194729988, 9.342264484334119601, -8.527530157486177487 ) ) ;
#78268 = DIRECTION ( 'NONE',  ( 0.000000000000000000, 1.000000000000000000, 0.000000000000000000 ) ) ;
#78269 = VECTOR ( 'NONE', #22888, 1000.000000000000114 ) ;
#78270 = CARTESIAN_POINT ( 'NONE',  ( 5.076628168052703671, 36.84226448433412315, 8.527530157486179263 ) ) ;
#78271 = CARTESIAN_POINT ( 'NONE',  ( 20.88017736071110875, 35.77201867748816966, -2.915334737309920321 ) ) ;
#78272 = CARTESIAN_POINT ( 'NONE',  ( -4.164238869374098151, 1.595415501580634388, -3.795296366450310543 ) ) ;
#78273 = CARTESIAN_POINT ( 'NONE',  ( 19.84674366389459266, 18.30059781766745175, 2.638427012816836559 ) ) ;
#78274 = CARTESIAN_POINT ( 'NONE',  ( 19.38216949554541557, 17.24863466993041783, -9.382169495545420901 ) ) ;
#78276 = CARTESIAN_POINT ( 'NONE',  ( -7.037762029935627162, -86.26090954799332167, -2.749999999999999556 ) ) ;
#78275 = CARTESIAN_POINT ( 'NONE',  ( 34.56412365047464874, 11.99999999999999645, 10.00000000000000000 ) ) ;
#78277 = CARTESIAN_POINT ( 'NONE',  ( 7.084665262690076126, 47.02201867748818387, -10.88017736071110164 ) ) ;
#78278 = AXIS2_PLACEMENT_3D ( 'NONE', #19849, #50341, #88352 ) ;
#78279 = CARTESIAN_POINT ( 'NONE',  ( 12.63842701281683922, 59.55059781766744464, -9.846743663894590881 ) ) ;
#78280 = LINE ( 'NONE', #86778, #21601 ) ;
#78281 = CARTESIAN_POINT ( 'NONE',  ( 14.92337183194729633, 22.67559781766745175, 8.527530157486181039 ) ) ;
#78282 = CARTESIAN_POINT ( 'NONE',  ( 19.42250999205614193, 20.14701867748817321, 5.440088680355555262 ) ) ;
#78283 = CARTESIAN_POINT ( 'NONE',  ( 22.81628187352647785, 11.62363466993042138, 6.195893100308588602E-16 ) ) ;
#78284 = CARTESIAN_POINT ( 'NONE',  ( 1.472469842513823179, 21.42559781766745175, 4.923371831947296329 ) ) ;
#78285 = SURFACE_STYLE_USAGE ( .BOTH. , #31791 ) ;
#78286 = CARTESIAN_POINT ( 'NONE',  ( 0.000000000000000000, 40.74999999999999289, 4.000000000000000000 ) ) ;
#78287 = CARTESIAN_POINT ( 'NONE',  ( 12.91533473730993009, 21.60535201082150536, -10.88017736071109987 ) ) ;
#78288 = CARTESIAN_POINT ( 'NONE',  ( 20.88017736071110164, 60.35535201082151957, 2.915334737309930979 ) ) ;
#78289 = DIRECTION ( 'NONE',  ( 0.000000000000000000, 1.000000000000000000, 0.000000000000000000 ) ) ;
#78291 = CARTESIAN_POINT ( 'NONE',  ( 4.559911319644449179, 13.89701867748817321, 9.422509992056141925 ) ) ;
#78290 = CARTESIAN_POINT ( 'NONE',  ( 0.1532563361054082862, 46.21726448433411605, 2.638427012816831674 ) ) ;
#78292 = CARTESIAN_POINT ( 'NONE',  ( 6.829574850505127692, -88.00372650098204019, -2.750000000000000444 ) ) ;
#78293 = CARTESIAN_POINT ( 'NONE',  ( 15.44008868035555260, 49.73035201082150536, 9.422509992056143702 ) ) ;
#78294 = CARTESIAN_POINT ( 'NONE',  ( -0.8801773607111008646, 8.272018677488171434, 2.915334737309923430 ) ) ;
#78295 = CARTESIAN_POINT ( 'NONE',  ( 17.20831665107776587, 9.133931151000787452, -7.208316651077762316 ) ) ;
#78296 = TOROIDAL_SURFACE ( 'NONE', #47963, 6.499999999999995559, 0.5000000000000000000 ) ;
#78297 = CARTESIAN_POINT ( 'NONE',  ( 17.20831665107776587, 39.13393115100079456, -7.208316651077762316 ) ) ;
#78298 = CARTESIAN_POINT ( 'NONE',  ( 0.000000000000000000, 0.5000000000000004441, 0.000000000000000000 ) ) ;
#78299 = CARTESIAN_POINT ( 'NONE',  ( 1.274849032794294290, 58.57228050351032778, 6.499999999999979572 ) ) ;
#78300 = CARTESIAN_POINT ( 'NONE',  ( 0.1532563361054100626, 65.80059781766745175, -2.638427012816831230 ) ) ;
#78301 = FACE_OUTER_BOUND ( 'NONE', #61042, .T. ) ;
#78302 = CARTESIAN_POINT ( 'NONE',  ( 13.79529636645030344, 18.26208216824730002, 14.16423886937410614 ) ) ;
#78303 = CARTESIAN_POINT ( 'NONE',  ( 12.63842701281683034, 42.46726448433412315, 9.846743663894596210 ) ) ;
#78305 = LINE ( 'NONE', #32796, #41711 ) ;
#78304 =( GEOMETRIC_REPRESENTATION_CONTEXT ( 3 ) GLOBAL_UNCERTAINTY_ASSIGNED_CONTEXT ( ( #88274 ) ) GLOBAL_UNIT_ASSIGNED_CONTEXT ( ( #41169, #78663, #84685 ) ) REPRESENTATION_CONTEXT ( 'NONE', 'WORKASPACE' ) );
#78306 = CARTESIAN_POINT ( 'NONE',  ( 20.88017736071110519, 5.563685344154838397, 2.639326808657452039E-16 ) ) ;
#78307 = CARTESIAN_POINT ( 'NONE',  ( 19.84674366389459621, 18.50893115100078745, 7.409399052514197653E-17 ) ) ;
#78309 = DIRECTION ( 'NONE',  ( 0.000000000000000000, 0.000000000000000000, 1.000000000000000000 ) ) ;
#78308 = CARTESIAN_POINT ( 'NONE',  ( -6.728956594450893114, 15.00000000000000888, 12.98689685418136186 ) ) ;
#78310 = CARTESIAN_POINT ( 'NONE',  ( 15.44008868035555793, 51.39701867748816966, -9.422509992056140149 ) ) ;
#78311 = CARTESIAN_POINT ( 'NONE',  ( -8.549892366338680105, 0.2306972965111899199, -12.25305656628366791 ) ) ;
#78312 = CARTESIAN_POINT ( 'NONE',  ( 7.084665262690076126, 19.10535201082150181, 10.88017736071109987 ) ) ;
#78313 = CARTESIAN_POINT ( 'NONE',  ( -1.099225684535947600, 48.70696800326375353, -6.408140936763238038 ) ) ;
#78314 = CARTESIAN_POINT ( 'NONE',  ( 3.591859063236761518, 9.956968003263753531, 11.09922568453594849 ) ) ;
#78315 = CARTESIAN_POINT ( 'NONE',  ( 7.361572987183170547, 17.05059781766745530, 9.846743663894590881 ) ) ;
#78316 = ORIENTED_EDGE ( 'NONE', *, *, #25547, .T. ) ;
#78317 = CARTESIAN_POINT ( 'NONE',  ( -14.24131928502210975, 15.00000000000000000, -0.4973178280107823923 ) ) ;
#78318 = CARTESIAN_POINT ( 'NONE',  ( 2.826948239413922703, 14.76930270348881002, -14.67127868811025948 ) ) ;
#78319 = CARTESIAN_POINT ( 'NONE',  ( 6.204703633549690345, 50.76208216824730357, -14.16423886937410259 ) ) ;
#78320 = CARTESIAN_POINT ( 'NONE',  ( 17.08211943468705130, 23.47041550158063572, 12.26659068614894998 ) ) ;
#78321 = CARTESIAN_POINT ( 'NONE',  ( 20.88017736071110519, 15.56368534415483751, 2.639326808657452039E-16 ) ) ;
#78322 = CARTESIAN_POINT ( 'NONE',  ( 4.559911319644449179, 52.23035201082151247, -9.422509992056141925 ) ) ;
#78323 = CYLINDRICAL_SURFACE ( 'NONE', #87829, 0.2500000000000002220 ) ;
#78324 = DIRECTION ( 'NONE',  ( 0.000000000000000000, 0.000000000000000000, 1.000000000000000000 ) ) ;
#78325 = CARTESIAN_POINT ( 'NONE',  ( 4.559911319644449179, 62.23035201082150536, -9.422509992056141925 ) ) ;
#78326 = SURFACE_STYLE_FILL_AREA ( #3322 ) ;
#78327 = CARTESIAN_POINT ( 'NONE',  ( 17.20831665107776587, 14.13393115100078568, -7.208316651077762316 ) ) ;
#78328 = FILL_AREA_STYLE ('',( #69367 ) ) ;
#78329 = CARTESIAN_POINT ( 'NONE',  ( 5.076628168052704559, 30.17559781766745175, -8.527530157486179263 ) ) ;
#78330 = CARTESIAN_POINT ( 'NONE',  ( 5.076628168052704559, 45.17559781766745175, -8.527530157486179263 ) ) ;
#78331 = EDGE_CURVE ( 'NONE', #36181, #2342, #16741, .T. ) ;
#78332 = CARTESIAN_POINT ( 'NONE',  ( 2.035157376598824452, 18.68868534415484106, 7.964842623401179544 ) ) ;
#78333 = UNCERTAINTY_MEASURE_WITH_UNIT (LENGTH_MEASURE( 1.000000000000000082E-05 ), #14258, 'distance_accuracy_value', 'NONE');
#78334 = CIRCLE ( 'NONE', #89544, 14.49999999999999822 ) ;
#78335 = CARTESIAN_POINT ( 'NONE',  ( 16.40814093676324603, 32.45696800326375353, -11.09922568453594671 ) ) ;
#78336 = CARTESIAN_POINT ( 'NONE',  ( 20.88017736071110875, 50.77201867748817676, -2.915334737309920765 ) ) ;
#78337 = CARTESIAN_POINT ( 'NONE',  ( 18.52753015748618282, 28.92559781766745175, -4.923371831947291888 ) ) ;
#78339 = CARTESIAN_POINT ( 'NONE',  ( 0.1532563361054083140, 6.008931151000784787, 1.131784320476157264E-15 ) ) ;
#78338 = CARTESIAN_POINT ( 'NONE',  ( 24.16423886937410614, 44.30374883491397497, 8.672049930838204340E-16 ) ) ;
#78340 = DIRECTION ( 'NONE',  ( 0.000000000000000000, 1.000000000000000000, 0.000000000000000000 ) ) ;
#78341 = CARTESIAN_POINT ( 'NONE',  ( 1.472469842513823179, 50.59226448433411605, -4.923371831947296329 ) ) ;
#78343 = CARTESIAN_POINT ( 'NONE',  ( 10.00000000000000178, 13.05374883491396787, 14.16423886937410082 ) ) ;
#78342 = CARTESIAN_POINT ( 'NONE',  ( 14.92337183194729633, 27.67559781766745530, 8.527530157486181039 ) ) ;
#78344 = CARTESIAN_POINT ( 'NONE',  ( 13.79529636645030344, 13.26208216824729824, 14.16423886937410614 ) ) ;
#78345 = CARTESIAN_POINT ( 'NONE',  ( 7.361572987183170547, 32.05059781766745175, 9.846743663894590881 ) ) ;
#78346 = CIRCLE ( 'NONE', #79908, 1.500000000000001332 ) ;
#78347 = CARTESIAN_POINT ( 'NONE',  ( 17.96484262340118221, 51.18868534415483396, -7.964842623401177768 ) ) ;
#78348 = CARTESIAN_POINT ( 'NONE',  ( 19.42250999205614548, 15.98035201082150714, -5.440088680355545492 ) ) ;
#78349 = CARTESIAN_POINT ( 'NONE',  ( 0.5774900079438607392, 48.48035201082150536, 5.440088680355550821 ) ) ;
#78350 = CARTESIAN_POINT ( 'NONE',  ( -0.8801773607110991993, 27.85535201082150181, -2.915334737309923874 ) ) ;
#78351 = VERTEX_POINT ( 'NONE', #94142 ) ;
#78352 = CARTESIAN_POINT ( 'NONE',  ( 0.6178305044545818747, 33.49863466993042493, -9.382169495545419124 ) ) ;
#78353 = VECTOR ( 'NONE', #68669, 1000.000000000000000 ) ;
#78354 = CARTESIAN_POINT ( 'NONE',  ( 15.44008868035555260, 34.73035201082151247, 9.422509992056143702 ) ) ;
#78355 = ORIENTED_EDGE ( 'NONE', *, *, #90876, .T. ) ;
#78356 = CARTESIAN_POINT ( 'NONE',  ( -2.816281873526471635, 53.91530133659709634, -3.434112377981056508 ) ) ;
#78357 = CARTESIAN_POINT ( 'NONE',  ( 19.42250999205614193, 60.14701867748817676, 5.440088680355555262 ) ) ;
#78358 = ORIENTED_EDGE ( 'NONE', *, *, #37415, .F. ) ;
#78359 = CARTESIAN_POINT ( 'NONE',  ( -0.8801773607111008646, 48.27201867748816966, 2.915334737309923430 ) ) ;
#78360 = CARTESIAN_POINT ( 'NONE',  ( 0.5774900079438590739, 7.647018677488171434, -5.440088680355550821 ) ) ;
#78361 = ADVANCED_FACE ( 'NONE', ( #32154 ), #17676, .T. ) ;
#78362 = CARTESIAN_POINT ( 'NONE',  ( 19.84674366389459266, 8.717264484334116048, -2.638427012816827677 ) ) ;
#78363 = DIRECTION ( 'NONE',  ( -0.000000000000000000, 0.000000000000000000, 1.000000000000000000 ) ) ;
#78364 = CARTESIAN_POINT ( 'NONE',  ( 6.204703633549690345, 57.84541550158063927, 14.16423886937410082 ) ) ;
#78365 = CARTESIAN_POINT ( 'NONE',  ( 19.84674366389459266, 8.300597817667451750, 2.638427012816836559 ) ) ;
#78366 = CARTESIAN_POINT ( 'NONE',  ( 6.204703633549690345, 10.76208216824729824, -14.16423886937410259 ) ) ;
#78367 = CARTESIAN_POINT ( 'NONE',  ( 19.84674366389459266, 3.717264484334118713, -2.638427012816827677 ) ) ;
#78368 = CARTESIAN_POINT ( 'NONE',  ( 19.42250999205614193, 15.14701867748817143, 5.440088680355555262 ) ) ;
#78369 = CARTESIAN_POINT ( 'NONE',  ( 7.361572987183169658, 44.96726448433412315, -9.846743663894592657 ) ) ;
#78370 = ORIENTED_EDGE ( 'NONE', *, *, #97546, .F. ) ;
#78371 = CARTESIAN_POINT ( 'NONE',  ( 1.472469842513823179, 51.42559781766745886, 4.923371831947296329 ) ) ;
#78372 = CARTESIAN_POINT ( 'NONE',  ( 32.06412365047463453, 26.99999999999997868, 10.00000000000000000 ) ) ;
#78373 = CARTESIAN_POINT ( 'NONE',  ( 20.88017736071110519, 45.56368534415484106, 2.639326808657452039E-16 ) ) ;
#78374 = CARTESIAN_POINT ( 'NONE',  ( 5.076628168052703671, 56.84226448433412315, 8.527530157486179263 ) ) ;
#78375 = CARTESIAN_POINT ( 'NONE',  ( 19.42250999205614548, 65.98035201082151957, -5.440088680355545492 ) ) ;
#78376 = CARTESIAN_POINT ( 'NONE',  ( 7.084665262690076126, 42.02201867748816966, -10.88017736071110164 ) ) ;
#78377 = CARTESIAN_POINT ( 'NONE',  ( 0.5774900079438607392, 3.480352010821504916, 5.440088680355550821 ) ) ;
#78378 = AXIS2_PLACEMENT_3D ( 'NONE', #75853, #98885, #5882 ) ;
#78379 = COLOUR_RGB ( '', 0.09019608, 0.27058824, 0.51372549) ;
#78380 = CARTESIAN_POINT ( 'NONE',  ( 16.40814093676323893, 45.79030133659708923, 11.09922568453595026 ) ) ;
#78381 = CYLINDRICAL_SURFACE ( 'NONE', #86599, 15.00000000000000000 ) ;
#78382 = EDGE_LOOP ( 'NONE', ( #692, #94506, #41144, #85872 ) ) ;
#78383 = CARTESIAN_POINT ( 'NONE',  ( 22.81628187352647785, 26.41530133659708923, 3.434112377981063169 ) ) ;
#78384 = CARTESIAN_POINT ( 'NONE',  ( 20.88017736071110875, 20.77201867748816611, -2.915334737309920765 ) ) ;
#78385 = ORIENTED_EDGE ( 'NONE', *, *, #80080, .F. ) ;
#78386 = EDGE_CURVE ( 'NONE', #28832, #60175, #93653, .T. ) ;
#78387 = CARTESIAN_POINT ( 'NONE',  ( 15.44008868035555793, 66.39701867748817676, -9.422509992056140149 ) ) ;
#78388 = CARTESIAN_POINT ( 'NONE',  ( 10.00000000000000000, 54.75893115100078745, -9.846743663894594434 ) ) ;
#78390 = CARTESIAN_POINT ( 'NONE',  ( 10.00000000000000000, 39.75893115100078745, -9.846743663894594434 ) ) ;
#78389 = CARTESIAN_POINT ( 'NONE',  ( 19.84674366389459621, 18.50893115100078745, 7.409399052514197653E-17 ) ) ;
#78391 = CARTESIAN_POINT ( 'NONE',  ( 10.58171042697176567, 14.76984967302771246, -10.54749450092402441 ) ) ;
#78392 = CARTESIAN_POINT ( 'NONE',  ( 14.92337183194729988, 29.34226448433411960, -8.527530157486177487 ) ) ;
#78393 = CARTESIAN_POINT ( 'NONE',  ( -14.37564666802071578, 15.00000000000000888, -2.692451322017866744 ) ) ;
#78394 = CARTESIAN_POINT ( 'NONE',  ( -12.60874940350935169, 15.00000000000000000, -7.160268045227203615 ) ) ;
#78395 = EDGE_CURVE ( 'NONE', #3044, #71011, #32657, .T. ) ;
#78397 = CARTESIAN_POINT ( 'NONE',  ( 0.9082943533636174127, 4.777657996272472852E-16, 14.47152380945585648 ) ) ;
#78396 = CARTESIAN_POINT ( 'NONE',  ( 18.52753015748617571, 23.09226448433411960, 4.923371831947298993 ) ) ;
#78398 = CARTESIAN_POINT ( 'NONE',  ( 8.880000000000000782, 1.116573172248542834E-15, 4.000000000000000000 ) ) ;
#78400 = ORIENTED_EDGE ( 'NONE', *, *, #35618, .T. ) ;
#78399 = CARTESIAN_POINT ( 'NONE',  ( 18.52753015748617571, 43.09226448433412315, 4.923371831947298993 ) ) ;
#78401 = MECHANICAL_DESIGN_GEOMETRIC_PRESENTATION_REPRESENTATION (  '', ( #40153 ), #91175 ) ;
#78402 = CARTESIAN_POINT ( 'NONE',  ( 13.78891971893208890, 14.63595249122791131, -5.904717858191532720 ) ) ;
#78403 = CARTESIAN_POINT ( 'NONE',  ( 22.81628187352647785, 31.62363466993042138, 6.195893100308588602E-16 ) ) ;
#78404 = CARTESIAN_POINT ( 'NONE',  ( -0.1491070598754174470, 61.94583914210339515, -4.500000000000001776 ) ) ;
#78405 = CARTESIAN_POINT ( 'NONE',  ( 6.204703633549690345, 42.84541550158063217, 14.16423886937410082 ) ) ;
#78406 = CARTESIAN_POINT ( 'NONE',  ( 19.84674366389459266, 18.71726448433411960, -2.638427012816827677 ) ) ;
#78408 = CARTESIAN_POINT ( 'NONE',  ( 2.791683348922237240, 5.383931151000785675, -7.208316651077763204 ) ) ;
#78407 = CIRCLE ( 'NONE', #14563, 9.900000000000002132 ) ;
#78409 = CARTESIAN_POINT ( 'NONE',  ( 20.00000000000000711, 95.40264689493518802, 4.636598378017573907 ) ) ;
#78410 = CARTESIAN_POINT ( 'NONE',  ( 17.08211943468705840, 45.13708216824730357, -12.26659068614894466 ) ) ;
#78411 = CARTESIAN_POINT ( 'NONE',  ( 19.84674366389459266, 63.30059781766745886, 2.638427012816836559 ) ) ;
#78412 = CARTESIAN_POINT ( 'NONE',  ( 12.91533473730993009, 11.60535201082150714, -10.88017736071109987 ) ) ;
#78413 = CARTESIAN_POINT ( 'NONE',  ( -2.266590686148945544, 22.22041550158063572, 7.082119434687048631 ) ) ;
#78415 = CARTESIAN_POINT ( 'NONE',  ( -46.02077283339401248, 104.3984410555176510, -5.346056167492045041 ) ) ;
#78414 = CARTESIAN_POINT ( 'NONE',  ( -4.164238869374098151, 41.59541550158061796, -3.795296366450310543 ) ) ;
#78416 = CARTESIAN_POINT ( 'NONE',  ( -2.393480905992977803, 14.49999999999999112, -14.80781041047760382 ) ) ;
#78418 = CARTESIAN_POINT ( 'NONE',  ( 10.00000000000000178, 52.25893115100078745, 9.846743663894594434 ) ) ;
#78417 = CARTESIAN_POINT ( 'NONE',  ( 4.441081520556267925, -2.684960557654440638, 2.500000000000000000 ) ) ;
#78419 = EDGE_LOOP ( 'NONE', ( #85524, #95128, #82567, #23226 ) ) ;
#78420 = CARTESIAN_POINT ( 'NONE',  ( 19.42250999205614548, 30.98035201082150536, -5.440088680355545492 ) ) ;
#78421 = CARTESIAN_POINT ( 'NONE',  ( 3.836325488036179454, 0.3639308251242922565, -14.50112432709426180 ) ) ;
#78422 = CARTESIAN_POINT ( 'NONE',  ( 20.00000000000000711, 95.39111596591838804, -4.637569774571024261 ) ) ;
#78423 = CARTESIAN_POINT ( 'NONE',  ( 19.84674366389459266, 43.30059781766744464, 2.638427012816836559 ) ) ;
#78424 = CARTESIAN_POINT ( 'NONE',  ( 17.59846011966563850, 33.99402920976536535, -9.945641156544795081 ) ) ;
#78425 = CARTESIAN_POINT ( 'NONE',  ( -14.16423886937410437, -13.40458449841936606, -3.795296366450299885 ) ) ;
#78426 = CARTESIAN_POINT ( 'NONE',  ( 2.791683348922240793, 46.63393115100077324, 7.208316651077764092 ) ) ;
#78427 = CARTESIAN_POINT ( 'NONE',  ( 5.076628168052703671, 66.84226448433412315, 8.527530157486179263 ) ) ;
#78428 = ORIENTED_EDGE ( 'NONE', *, *, #42477, .T. ) ;
#78429 = CARTESIAN_POINT ( 'NONE',  ( -4.164238869374099039, 11.80374883491396965, 8.674139862899312516E-16 ) ) ;
#78430 = B_SPLINE_CURVE_WITH_KNOTS ( 'NONE', 3,
 ( #37982, #30446, #60947, #89488 ),
 .UNSPECIFIED., .F., .F.,
 ( 4, 4 ),
 ( 6.206335383118182794E-17, 0.002562518741975522863 ),
 .UNSPECIFIED. ) ;
#78431 = DIRECTION ( 'NONE',  ( -0.000000000000000000, -1.000000000000000000, -0.000000000000000000 ) ) ;
#78433 = FACE_OUTER_BOUND ( 'NONE', #38186, .T. ) ;
#78432 = CARTESIAN_POINT ( 'NONE',  ( -6.030006457149878152, -39.79017371238850842, -2.750000000000000000 ) ) ;
#78434 = CARTESIAN_POINT ( 'NONE',  ( 2.917880565312948704, 67.63708216824730357, 12.26659068614894643 ) ) ;
#78435 = CARTESIAN_POINT ( 'NONE',  ( 10.00000000000000178, 30.37363466993042138, 12.81628187352647608 ) ) ;
#78436 = CARTESIAN_POINT ( 'NONE',  ( -6.732636091893175134, -88.11213685669365248, -2.750000000000000000 ) ) ;
#78437 = CARTESIAN_POINT ( 'NONE',  ( 14.92337183194729633, 2.675597817667451750, 8.527530157486181039 ) ) ;
#78438 = B_SPLINE_CURVE_WITH_KNOTS ( 'NONE', 3,
 ( #16465, #55447, #46945, #85949, #8952, #39469 ),
 .UNSPECIFIED., .F., .F.,
 ( 4, 2, 4 ),
 ( 0.000000000000000000, 0.0002605067024380860801, 0.0005210134048761721603 ),
 .UNSPECIFIED. ) ;
#78439 = CARTESIAN_POINT ( 'NONE',  ( -1.926860441876564023, 9.688309369127509285, 1.004413902775740781E-15 ) ) ;
#78440 = CARTESIAN_POINT ( 'NONE',  ( 15.44008868035555260, 4.730352010821505360, 9.422509992056143702 ) ) ;
#78441 = FACE_OUTER_BOUND ( 'NONE', #90537, .T. ) ;
#78442 = CARTESIAN_POINT ( 'NONE',  ( 19.72487221294570858, 70.00000000000000000, 6.500000000000000888 ) ) ;
#78443 = CARTESIAN_POINT ( 'NONE',  ( 17.96484262340118221, 21.18868534415483396, -7.964842623401177768 ) ) ;
#78444 = CARTESIAN_POINT ( 'NONE',  ( 19.42250999205614548, 35.98035201082151247, -5.440088680355545492 ) ) ;
#78445 = CARTESIAN_POINT ( 'NONE',  ( 10.00000000000000000, -2.126365330069579951, -12.81628187352647608 ) ) ;
#78446 = CARTESIAN_POINT ( 'NONE',  ( 0.1532563361054083140, 51.00893115100078745, 1.131784320476157264E-15 ) ) ;
#78447 = CARTESIAN_POINT ( 'NONE',  ( -43.79232545471665361, 106.6932607868292706, -5.013557994010066743 ) ) ;
#78448 = CARTESIAN_POINT ( 'NONE',  ( 19.84674366389459621, 8.508931151000785675, 7.409399052514197653E-17 ) ) ;
#78449 = EDGE_LOOP ( 'NONE', ( #24238, #73652, #93899, #45020, #16013, #12210 ) ) ;
#78450 = TOROIDAL_SURFACE ( 'NONE', #35331, 14.49999999999999822, 0.5000000000000000000 ) ;
#78451 = CARTESIAN_POINT ( 'NONE',  ( 12.91533473730993009, 31.60535201082150891, -10.88017736071109987 ) ) ;
#78452 = EDGE_CURVE ( 'NONE', #80099, #76621, #46412, .T. ) ;
#78453 = CARTESIAN_POINT ( 'NONE',  ( -2.816281873526473856, 34.12363466993042493, 9.499525473075851096E-16 ) ) ;
#78454 = DIRECTION ( 'NONE',  ( 0.000000000000000000, 1.000000000000000000, 0.000000000000000000 ) ) ;
#78455 = UNCERTAINTY_MEASURE_WITH_UNIT (LENGTH_MEASURE( 1.000000000000000082E-05 ), #74105, 'distance_accuracy_value', 'NONE');
#78456 = STYLED_ITEM ( 'NONE', ( #42305 ), #80504 ) ;
#78457 = CARTESIAN_POINT ( 'NONE',  ( 6.565887622018943937, -1.918031996736246692, -12.81628187352647608 ) ) ;
#78458 = EDGE_CURVE ( 'NONE', #93612, #63139, #11945, .T. ) ;
#78459 = CARTESIAN_POINT ( 'NONE',  ( 2.035157376598822676, 52.43868534415483396, -7.964842623401177768 ) ) ;
#78460 = CARTESIAN_POINT ( 'NONE',  ( 2.791683348922240793, 16.63393115100078745, 7.208316651077764092 ) ) ;
#78461 = CARTESIAN_POINT ( 'NONE',  ( 13.43411237798106583, 32.66530133659708213, -12.81628187352647252 ) ) ;
#78463 = SURFACE_STYLE_FILL_AREA ( #47953 ) ;
#78462 = CARTESIAN_POINT ( 'NONE',  ( 0.5774900079438607392, 68.48035201082150536, 5.440088680355550821 ) ) ;
#78464 = CARTESIAN_POINT ( 'NONE',  ( 19.50000000000000711, 80.28026998469363207, 5.000000000000000000 ) ) ;
#78465 = ORIENTED_EDGE ( 'NONE', *, *, #84241, .T. ) ;
#78466 = DIRECTION ( 'NONE',  ( 0.000000000000000000, 1.000000000000000000, 0.000000000000000000 ) ) ;
#78467 = DIRECTION ( 'NONE',  ( -0.8141155183563146824, 0.000000000000000000, -0.5807029557109462115 ) ) ;
#78468 = CARTESIAN_POINT ( 'NONE',  ( -0.8801773607111009756, 8.063685344154837509, 1.068504757029289695E-15 ) ) ;
#78470 = CARTESIAN_POINT ( 'NONE',  ( 20.36894250292379382, 18.67874883491397142, 10.36894250292379205 ) ) ;
#78469 = CARTESIAN_POINT ( 'NONE',  ( 19.38216949554541557, 52.24863466993041072, -9.382169495545420901 ) ) ;
#78471 = CARTESIAN_POINT ( 'NONE',  ( 10.00000000000000178, 17.25893115100078745, 9.846743663894594434 ) ) ;
#78472 =( NAMED_UNIT ( * ) SI_UNIT ( $, .STERADIAN. ) SOLID_ANGLE_UNIT ( ) );
#78473 = CARTESIAN_POINT ( 'NONE',  ( 14.92337183194729988, 19.34226448433411960, -8.527530157486177487 ) ) ;
#78474 = CARTESIAN_POINT ( 'NONE',  ( 24.16423886937410614, 54.51208216824730357, -3.795296366450302550 ) ) ;
#78475 = EDGE_LOOP ( 'NONE', ( #78524, #48157, #55123, #24065 ) ) ;
#78476 =( GEOMETRIC_REPRESENTATION_CONTEXT ( 3 ) GLOBAL_UNCERTAINTY_ASSIGNED_CONTEXT ( ( #26427 ) ) GLOBAL_UNIT_ASSIGNED_CONTEXT ( ( #64001, #18524, #48022 ) ) REPRESENTATION_CONTEXT ( 'NONE', 'WORKASPACE' ) );
#78477 = CARTESIAN_POINT ( 'NONE',  ( 7.084665262690076126, 4.105352010821503583, 10.88017736071109987 ) ) ;
#78478 = CARTESIAN_POINT ( 'NONE',  ( 2.035157376598824452, 18.68868534415484106, 7.964842623401179544 ) ) ;
#78479 = CARTESIAN_POINT ( 'NONE',  ( 1.932340009482155896, 31.49127512925447547, -6.500000000000005329 ) ) ;
#78480 = EDGE_LOOP ( 'NONE', ( #72768, #64962, #21305, #88995 ) ) ;
#78481 = EDGE_LOOP ( 'NONE', ( #7922, #3353, #7151, #51302, #61287, #20611 ) ) ;
#78482 = CARTESIAN_POINT ( 'NONE',  ( 19.42250999205614548, 15.98035201082150714, -5.440088680355545492 ) ) ;
#78483 = CARTESIAN_POINT ( 'NONE',  ( 10.00000000000000178, 9.313685344154839285, 10.88017736071110342 ) ) ;
#78484 = CARTESIAN_POINT ( 'NONE',  ( 14.92337183194729633, 52.67559781766745175, 8.527530157486181039 ) ) ;
#78485 = EDGE_CURVE ( 'NONE', #72511, #59916, #47158, .T. ) ;
#78486 = CARTESIAN_POINT ( 'NONE',  ( 10.00000000000000178, 55.37363466993042493, 12.81628187352647608 ) ) ;
#78487 =( LENGTH_UNIT ( ) NAMED_UNIT ( * ) SI_UNIT ( .MILLI., .METRE. ) );
#78489 = CARTESIAN_POINT ( 'NONE',  ( 24.16423886937410614, 14.30374883491396787, 8.672049930838204340E-16 ) ) ;
#78488 = SURFACE_SIDE_STYLE ('',( #50306 ) ) ;
#78490 = CARTESIAN_POINT ( 'NONE',  ( 17.96484262340118221, 24.93868534415484461, 7.964842623401181321 ) ) ;
#78491 = CARTESIAN_POINT ( 'NONE',  ( 20.88017736071110164, 15.35535201082150358, 2.915334737309930979 ) ) ;
#78492 = CARTESIAN_POINT ( 'NONE',  ( 7.361572987183170547, 57.05059781766744464, 9.846743663894590881 ) ) ;
#78493 = CARTESIAN_POINT ( 'NONE',  ( -8.108527105141890345, -3.139510826252087661, -3.750000000000000888 ) ) ;
#78494 = CARTESIAN_POINT ( 'NONE',  ( 18.52753015748617571, 38.09226448433412315, 4.923371831947298993 ) ) ;
#78495 = EDGE_CURVE ( 'NONE', #94488, #2423, #44164, .T. ) ;
#78496 = FACE_OUTER_BOUND ( 'NONE', #31149, .T. ) ;
#78497 = CARTESIAN_POINT ( 'NONE',  ( 18.52753015748618282, 8.925597817667451750, -4.923371831947291888 ) ) ;
#78498 = CARTESIAN_POINT ( 'NONE',  ( -9.846743663894596210, 30.80059781766745530, -2.638427012816824124 ) ) ;
#78499 = ORIENTED_EDGE ( 'NONE', *, *, #64028, .T. ) ;
#78500 =( GEOMETRIC_REPRESENTATION_CONTEXT ( 3 ) GLOBAL_UNCERTAINTY_ASSIGNED_CONTEXT ( ( #31111 ) ) GLOBAL_UNIT_ASSIGNED_CONTEXT ( ( #85113, #55091, #41603 ) ) REPRESENTATION_CONTEXT ( 'NONE', 'WORKASPACE' ) );
#78501 = CARTESIAN_POINT ( 'NONE',  ( -1.761054936948033278, 12.86682408883346440, 10.00000000000000000 ) ) ;
#78502 = CARTESIAN_POINT ( 'NONE',  ( 10.00000000000000178, 17.25893115100078745, 9.846743663894594434 ) ) ;
#78503 = CARTESIAN_POINT ( 'NONE',  ( -2.816281873526473856, -0.6680319967362464695, 3.434112377981055619 ) ) ;
#78504 = CARTESIAN_POINT ( 'NONE',  ( 4.559911319644449179, 43.89701867748816966, 9.422509992056141925 ) ) ;
#78506 = CARTESIAN_POINT ( 'NONE',  ( 0.6178305044545818747, 48.49863466993042493, -9.382169495545419124 ) ) ;
#78505 = CARTESIAN_POINT ( 'NONE',  ( -0.8801773607111009756, 3.063685344154837509, 1.068504757029289695E-15 ) ) ;
#78507 = CARTESIAN_POINT ( 'NONE',  ( 10.00000000000000178, 13.05374883491396787, 14.16423886937410082 ) ) ;
#78508 = CARTESIAN_POINT ( 'NONE',  ( 0.6178305044545838731, 59.74863466993041783, 9.382169495545420901 ) ) ;
#78509 = ORIENTED_EDGE ( 'NONE', *, *, #44284, .T. ) ;
#78510 = CARTESIAN_POINT ( 'NONE',  ( 18.52753015748617571, 58.09226448433411605, 4.923371831947298993 ) ) ;
#78511 = CARTESIAN_POINT ( 'NONE',  ( 0.5774900079438607392, 23.48035201082150536, 5.440088680355550821 ) ) ;
#78512 = VERTEX_POINT ( 'NONE', #40666 ) ;
#78513 = CARTESIAN_POINT ( 'NONE',  ( -0.8801773607110991993, 67.85535201082151957, -2.915334737309923874 ) ) ;
#78514 = DIRECTION ( 'NONE',  ( 0.000000000000000000, 0.000000000000000000, 1.000000000000000000 ) ) ;
#78515 = LINE ( 'NONE', #9529, #65978 ) ;
#78516 = CARTESIAN_POINT ( 'NONE',  ( 14.92337183194729988, 4.342264484334117824, -8.527530157486177487 ) ) ;
#78517 = CARTESIAN_POINT ( 'NONE',  ( 2.035157376598822676, 67.43868534415484817, -7.964842623401177768 ) ) ;
#78518 = SURFACE_STYLE_FILL_AREA ( #47029 ) ;
#78519 = EDGE_CURVE ( 'NONE', #4697, #97173, #77640, .T. ) ;
#78521 = DIRECTION ( 'NONE',  ( 0.000000000000000000, 0.000000000000000000, 1.000000000000000000 ) ) ;
#78520 = CARTESIAN_POINT ( 'NONE',  ( 17.96484262340118221, 56.18868534415484817, -7.964842623401177768 ) ) ;
#78522 = CARTESIAN_POINT ( 'NONE',  ( -0.8801773607110991993, 67.85535201082151957, -2.915334737309923874 ) ) ;
#78524 = ORIENTED_EDGE ( 'NONE', *, *, #73462, .F. ) ;
#78523 = CARTESIAN_POINT ( 'NONE',  ( 10.00000000000000000, -0.2410688489992152128, -9.846743663894594434 ) ) ;
#78525 = B_SPLINE_CURVE_WITH_KNOTS ( 'NONE', 3,
 ( #93229, #70256, #70753, #46748, #32723, #39270 ),
 .UNSPECIFIED., .F., .F.,
 ( 4, 2, 4 ),
 ( 0.0002800138956558747335, 0.0006862192609921059219, 0.001092424626328337110 ),
 .UNSPECIFIED. ) ;
#78526 = VECTOR ( 'NONE', #49398, 1000.000000000000000 ) ;
#78527 = CARTESIAN_POINT ( 'NONE',  ( -0.1298530154764001854, 80.39370036920264795, -5.000000000000000000 ) ) ;
#78528 = CARTESIAN_POINT ( 'NONE',  ( 12.63842701281683922, 49.55059781766744464, -9.846743663894590881 ) ) ;
#78529 = VERTEX_POINT ( 'NONE', #87621 ) ;
#78530 = VERTEX_POINT ( 'NONE', #13105 ) ;
#78531 = DIRECTION ( 'NONE',  ( -0.000000000000000000, -1.000000000000000000, -0.000000000000000000 ) ) ;
#78532 = CARTESIAN_POINT ( 'NONE',  ( 24.16423886937410614, 4.512082168247300906, -3.795296366450302550 ) ) ;
#78533 = CARTESIAN_POINT ( 'NONE',  ( 21.09922568453594849, 61.20696800326376064, 6.408140936763242479 ) ) ;
#78534 = CARTESIAN_POINT ( 'NONE',  ( 10.00000000000000178, 3.053748834913967425, 14.16423886937410082 ) ) ;
#78535 = EDGE_CURVE ( 'NONE', #8981, #62748, #40061, .T. ) ;
#78536 = CARTESIAN_POINT ( 'NONE',  ( 2.917880565312948704, 22.63708216824730002, 12.26659068614894643 ) ) ;
#78537 = CARTESIAN_POINT ( 'NONE',  ( 0.000000000000000000, 0.5000000000000004441, 0.000000000000000000 ) ) ;
#78538 = FACE_OUTER_BOUND ( 'NONE', #34195, .T. ) ;
#78539 = CARTESIAN_POINT ( 'NONE',  ( 19.42250999205614193, 25.14701867748817321, 5.440088680355555262 ) ) ;
#78540 = FILL_AREA_STYLE ('',( #79526 ) ) ;
#78541 = ORIENTED_EDGE ( 'NONE', *, *, #89636, .F. ) ;
#78542 = CARTESIAN_POINT ( 'NONE',  ( 19.84674366389459621, 3.508931151000785231, 7.409399052514197653E-17 ) ) ;
#78543 = CARTESIAN_POINT ( 'NONE',  ( 12.63842701281683034, 22.46726448433411605, 9.846743663894596210 ) ) ;
#78544 = CARTESIAN_POINT ( 'NONE',  ( 3.591859063236763294, 38.29030133659708923, -11.09922568453595026 ) ) ;
#78545 = CARTESIAN_POINT ( 'NONE',  ( 18.52753015748618282, 33.92559781766745886, -4.923371831947291888 ) ) ;
#78546 = CARTESIAN_POINT ( 'NONE',  ( 11.75209714983975395, 0.04922511925147050188, -8.918201205062004533 ) ) ;
#78547 = CARTESIAN_POINT ( 'NONE',  ( -1.099225684535947600, 33.70696800326375353, -6.408140936763238038 ) ) ;
#78548 = CARTESIAN_POINT ( 'NONE',  ( 19.80777595082616216, 40.68878173731739878, -6.499999999999961808 ) ) ;
#78549 = CIRCLE ( 'NONE', #35429, 14.49999999999999822 ) ;
#78550 = CARTESIAN_POINT ( 'NONE',  ( 0.1532563361054082862, 21.21726448433412315, 2.638427012816831674 ) ) ;
#78551 = CARTESIAN_POINT ( 'NONE',  ( 2.917880565312948704, 12.63708216824730179, 12.26659068614894643 ) ) ;
#78552 = VERTEX_POINT ( 'NONE', #27116 ) ;
#78553 = CARTESIAN_POINT ( 'NONE',  ( 2.035157376598824452, 33.68868534415484106, 7.964842623401179544 ) ) ;
#78554 = CARTESIAN_POINT ( 'NONE',  ( 17.08211943468705840, 35.13708216824730357, -12.26659068614894466 ) ) ;
#78555 = CARTESIAN_POINT ( 'NONE',  ( 12.63842701281683922, 54.55059781766745175, -9.846743663894590881 ) ) ;
#78556 = EDGE_CURVE ( 'NONE', #86906, #58402, #47976, .T. ) ;
#78557 = CARTESIAN_POINT ( 'NONE',  ( 7.361572987183169658, 9.967264484334119601, -9.846743663894592657 ) ) ;
#78558 = AXIS2_PLACEMENT_3D ( 'NONE', #5939, #12931, #67419 ) ;
#78560 = CARTESIAN_POINT ( 'NONE',  ( 18.00000000000001776, 4.625929269271493211E-15, 8.000000000000000000 ) ) ;
#78559 = CARTESIAN_POINT ( 'NONE',  ( 19.38216949554541557, 57.24863466993042493, -9.382169495545420901 ) ) ;
#78561 = CARTESIAN_POINT ( 'NONE',  ( 2.035157376598822676, 27.43868534415483396, -7.964842623401177768 ) ) ;
#78562 = CARTESIAN_POINT ( 'NONE',  ( -1.099225684535947600, 19.54030133659708568, 6.408140936763237150 ) ) ;
#78563 = CARTESIAN_POINT ( 'NONE',  ( 6.565887622018943937, 20.16530133659708213, 12.81628187352647430 ) ) ;
#78564 = CARTESIAN_POINT ( 'NONE',  ( 1.472469842513823179, 46.42559781766745175, 4.923371831947296329 ) ) ;
#78565 = CARTESIAN_POINT ( 'NONE',  ( -7.964842623401179544, -2.561314655845163823, -7.964842623401174215 ) ) ;
#78566 = CARTESIAN_POINT ( 'NONE',  ( 19.38216949554541202, 50.99863466993042493, 9.382169495545424454 ) ) ;
#78567 = SURFACE_SIDE_STYLE ('',( #25095 ) ) ;
#78568 = VECTOR ( 'NONE', #96622, 1000.000000000000000 ) ;
#78570 = CYLINDRICAL_SURFACE ( 'NONE', #76733, 0.5000000000000004441 ) ;
#78569 = CARTESIAN_POINT ( 'NONE',  ( 20.88017736071110164, 55.35535201082149825, 2.915334737309930979 ) ) ;
#78571 = CARTESIAN_POINT ( 'NONE',  ( -11.37646734096567336, -81.99481244925677004, 4.000000000000000000 ) ) ;
#78572 = EDGE_CURVE ( 'NONE', #54617, #2021, #81594, .T. ) ;
#78573 = CARTESIAN_POINT ( 'NONE',  ( 0.2751277870542980231, 14.36607318730130878, -6.500000000000002665 ) ) ;
#78574 = CARTESIAN_POINT ( 'NONE',  ( 12.91533473730993009, 51.60535201082149825, -10.88017736071109987 ) ) ;
#78575 = CARTESIAN_POINT ( 'NONE',  ( 0.5774900079438590739, 52.64701867748817676, -5.440088680355550821 ) ) ;
#78576 = CARTESIAN_POINT ( 'NONE',  ( 0.2751277870542967463, 70.00000000000000000, -6.500000000000000888 ) ) ;
#78577 = CARTESIAN_POINT ( 'NONE',  ( -46.48928645636213730, 103.2957187381727238, -6.397878122524045530 ) ) ;
#78578 = EDGE_CURVE ( 'NONE', #58660, #53014, #65602, .T. ) ;
#78579 = CARTESIAN_POINT ( 'NONE',  ( 20.88017736071110875, 10.77201867748817143, -2.915334737309920765 ) ) ;
#78580 = CARTESIAN_POINT ( 'NONE',  ( 0.1532563361054083140, 66.00893115100079456, 1.131784320476157264E-15 ) ) ;
#78581 = CARTESIAN_POINT ( 'NONE',  ( 12.91533473730993009, 21.60535201082150536, -10.88017736071109987 ) ) ;
#78582 = DIRECTION ( 'NONE',  ( 0.6246950475544238435, 0.7808688094430307203, 0.000000000000000000 ) ) ;
#78583 = CARTESIAN_POINT ( 'NONE',  ( 19.38216949554541557, 27.24863466993041783, -9.382169495545420901 ) ) ;
#78584 = EDGE_LOOP ( 'NONE', ( #23925, #48394, #98610, #53683 ) ) ;
#78585 = CARTESIAN_POINT ( 'NONE',  ( 15.44008868035555793, 46.39701867748817676, -9.422509992056140149 ) ) ;
#78586 = CARTESIAN_POINT ( 'NONE',  ( 2.791683348922240793, 41.63393115100078745, 7.208316651077764092 ) ) ;
#78588 = FACE_OUTER_BOUND ( 'NONE', #98817, .T. ) ;
#78587 = CARTESIAN_POINT ( 'NONE',  ( 0.6178305044545818747, 8.498634669930421381, -9.382169495545419124 ) ) ;
#78589 = CARTESIAN_POINT ( 'NONE',  ( 20.88017736071110519, 30.56368534415484106, 2.639326808657452039E-16 ) ) ;
#78590 = CARTESIAN_POINT ( 'NONE',  ( -0.8801773607111008646, 38.27201867748816255, 2.915334737309923430 ) ) ;
#78591 = CARTESIAN_POINT ( 'NONE',  ( 24.16423886937409904, 49.09541550158063217, 3.795296366450317205 ) ) ;
#78592 = CARTESIAN_POINT ( 'NONE',  ( 18.52753015748617571, 38.09226448433412315, 4.923371831947298993 ) ) ;
#78593 = CARTESIAN_POINT ( 'NONE',  ( -0.8801773607111009756, 63.06368534415484106, 1.068504757029289695E-15 ) ) ;
#78594 = DIRECTION ( 'NONE',  ( 0.000000000000000000, 0.000000000000000000, 1.000000000000000000 ) ) ;
#78595 = CARTESIAN_POINT ( 'NONE',  ( 2.917880565312948704, 12.63708216824730179, 12.26659068614894643 ) ) ;
#78596 = DIRECTION ( 'NONE',  ( 0.000000000000000000, 0.000000000000000000, 1.000000000000000000 ) ) ;
#78597 = DIRECTION ( 'NONE',  ( 0.000000000000000000, -1.000000000000000000, 0.000000000000000000 ) ) ;
#78598 = EDGE_LOOP ( 'NONE', ( #30200, #26670, #11677, #2048 ) ) ;
#78599 = ORIENTED_EDGE ( 'NONE', *, *, #78604, .F. ) ;
#78600 = TOROIDAL_SURFACE ( 'NONE', #6725, 14.49999999999999822, 0.5000000000000000000 ) ;
#78601 = CARTESIAN_POINT ( 'NONE',  ( -4.164238869374099927, 52.01208216824729647, 3.795296366450308767 ) ) ;
#78602 = CARTESIAN_POINT ( 'NONE',  ( 17.08211943468705840, 35.13708216824730357, -12.26659068614894466 ) ) ;
#78603 = CARTESIAN_POINT ( 'NONE',  ( 0.1532563361054100626, 20.80059781766744464, -2.638427012816831230 ) ) ;
#78604 = EDGE_CURVE ( 'NONE', #12737, #28504, #94639, .T. ) ;
#78605 = CARTESIAN_POINT ( 'NONE',  ( -2.816281873526473856, 19.33196800326375708, 3.434112377981055619 ) ) ;
#78606 = CARTESIAN_POINT ( 'NONE',  ( 0.1532563361054100626, 55.80059781766745175, -2.638427012816831230 ) ) ;
#78607 = LINE ( 'NONE', #72079, #59423 ) ;
#78609 = CARTESIAN_POINT ( 'NONE',  ( 21.09922568453594849, 26.20696800326375353, 6.408140936763242479 ) ) ;
#78608 = CARTESIAN_POINT ( 'NONE',  ( 17.96484262340118221, 56.18868534415484817, -7.964842623401177768 ) ) ;
#78610 = CARTESIAN_POINT ( 'NONE',  ( 22.26659068614894466, 33.88708216824730357, 7.082119434687054849 ) ) ;
#78611 = CARTESIAN_POINT ( 'NONE',  ( 19.42250999205614193, 30.14701867748817321, 5.440088680355555262 ) ) ;
#78612 = B_SPLINE_CURVE_WITH_KNOTS ( 'NONE', 3,
 ( #29621, #37649, #89648, #43653 ),
 .UNSPECIFIED., .F., .F.,
 ( 4, 4 ),
 ( 0.000000000000000000, 0.002657014572711344572 ),
 .UNSPECIFIED. ) ;
#78613 = CARTESIAN_POINT ( 'NONE',  ( 12.21238578216011916, 1.931235119739804773E-16, -8.049595036947129856 ) ) ;
#78614 = EDGE_CURVE ( 'NONE', #42957, #81191, #96130, .T. ) ;
#78615 = B_SPLINE_CURVE_WITH_KNOTS ( 'NONE', 3,
 ( #35392, #75864, #39354, #53858 ),
 .UNSPECIFIED., .F., .F.,
 ( 4, 4 ),
 ( 2.168404344971008868E-18, 0.001060528352562004799 ),
 .UNSPECIFIED. ) ;
#78616 = CARTESIAN_POINT ( 'NONE',  ( 2.638427012816829897, -10.44940218233254470, -9.846743663894592657 ) ) ;
#78617 = CARTESIAN_POINT ( 'NONE',  ( 0.1532563361054083140, 6.008931151000784787, 1.131784320476157264E-15 ) ) ;
#78618 = ORIENTED_EDGE ( 'NONE', *, *, #86122, .F. ) ;
#78619 = CARTESIAN_POINT ( 'NONE',  ( 9.898881779040660689, -0.03417435944610275333, 10.25059215482582786 ) ) ;
#78620 = CARTESIAN_POINT ( 'NONE',  ( 0.000000000000000000, 15.00000000000000000, 0.000000000000000000 ) ) ;
#78621 = EDGE_LOOP ( 'NONE', ( #55202, #5204, #46899, #46521, #32003, #22563 ) ) ;
#78622 = CARTESIAN_POINT ( 'NONE',  ( 6.204703633549690345, 5.762082168247301794, -14.16423886937410259 ) ) ;
#78624 = CARTESIAN_POINT ( 'NONE',  ( 17.96484262340118221, 9.938685344154839285, 7.964842623401181321 ) ) ;
#78623 = CARTESIAN_POINT ( 'NONE',  ( 12.91533473730993009, 6.605352010821504471, -10.88017736071109987 ) ) ;
#78626 = CARTESIAN_POINT ( 'NONE',  ( 10.00000000000000178, 0.3736346699304200492, 12.81628187352647608 ) ) ;
#78625 = CARTESIAN_POINT ( 'NONE',  ( 2.791683348922237240, 30.38393115100078390, -7.208316651077763204 ) ) ;
#78627 = FILL_AREA_STYLE_COLOUR ( '', #88575 ) ;
#78628 = DIRECTION ( 'NONE',  ( -0.000000000000000000, -0.000000000000000000, 1.000000000000000000 ) ) ;
#78629 = AXIS2_PLACEMENT_3D ( 'NONE', #48743, #79249, #10762 ) ;
#78630 = B_SPLINE_CURVE_WITH_KNOTS ( 'NONE', 3,
 ( #98062, #14057, #46033, #8034 ),
 .UNSPECIFIED., .F., .F.,
 ( 4, 4 ),
 ( 1.758547849261791993E-16, 0.002392975128318475080 ),
 .UNSPECIFIED. ) ;
#78631 = CARTESIAN_POINT ( 'NONE',  ( 3.591859063236761518, 19.95696800326375353, 11.09922568453594849 ) ) ;
#78632 = CARTESIAN_POINT ( 'NONE',  ( -9.382169495545422677, 28.49863466993042849, -9.382169495545417348 ) ) ;
#78633 = ORIENTED_EDGE ( 'NONE', *, *, #17873, .F. ) ;
#78634 = VECTOR ( 'NONE', #70790, 1000.000000000000227 ) ;
#78635 = VECTOR ( 'NONE', #64608, 1000.000000000000000 ) ;
#78636 = CARTESIAN_POINT ( 'NONE',  ( -4.164238869374099927, 52.01208216824729647, 3.795296366450308767 ) ) ;
#78637 = ORIENTED_EDGE ( 'NONE', *, *, #15246, .F. ) ;
#78638 = CARTESIAN_POINT ( 'NONE',  ( -2.266590686148945544, 52.22041550158064638, 7.082119434687048631 ) ) ;
#78639 = ORIENTED_EDGE ( 'NONE', *, *, #56268, .F. ) ;
#78640 = CARTESIAN_POINT ( 'NONE',  ( 15.44008868035555260, 29.73035201082150891, 9.422509992056143702 ) ) ;
#78641 = CARTESIAN_POINT ( 'NONE',  ( 20.88017736071110519, 35.56368534415484106, 2.639326808657452039E-16 ) ) ;
#78642 = CARTESIAN_POINT ( 'NONE',  ( 4.559911319644449179, 33.89701867748817676, 9.422509992056141925 ) ) ;
#78643 = CIRCLE ( 'NONE', #38677, 15.00000000000000000 ) ;
#78644 = CARTESIAN_POINT ( 'NONE',  ( 0.5774900079438590739, 62.64701867748817676, -5.440088680355550821 ) ) ;
#78645 = CARTESIAN_POINT ( 'NONE',  ( 0.5774900079438607392, 28.48035201082150891, 5.440088680355550821 ) ) ;
#78646 = VECTOR ( 'NONE', #71705, 1000.000000000000114 ) ;
#78648 = ORIENTED_EDGE ( 'NONE', *, *, #64680, .F. ) ;
#78647 = CARTESIAN_POINT ( 'NONE',  ( 32.06412365047463453, 14.00000000000001421, -10.00000000000000000 ) ) ;
#78649 = CARTESIAN_POINT ( 'NONE',  ( 2.791683348922237240, 20.38393115100078745, -7.208316651077763204 ) ) ;
#78650 = CARTESIAN_POINT ( 'NONE',  ( -5.068142462294323636, -24.94450071860671514, 2.499999999999194422 ) ) ;
#78651 = ORIENTED_EDGE ( 'NONE', *, *, #30810, .T. ) ;
#78652 = CARTESIAN_POINT ( 'NONE',  ( 0.000000000000000000, -97.00000000000000000, 3.750000000000000000 ) ) ;
#78653 = CARTESIAN_POINT ( 'NONE',  ( 12.63842701281683922, 49.55059781766744464, -9.846743663894590881 ) ) ;
#78654 = LINE ( 'NONE', #79630, #43638 ) ;
#78655 = COLOUR_RGB ( '', 0.09019608, 0.27058824, 0.51372549) ;
#78656 = CARTESIAN_POINT ( 'NONE',  ( -3.530007528296587704, -1.230351260576522110, 3.750000000000000444 ) ) ;
#78657 = CARTESIAN_POINT ( 'NONE',  ( 18.18329248733315140, 22.60290668512023871, 6.499999999999997335 ) ) ;
#78658 = CARTESIAN_POINT ( 'NONE',  ( 1.274849032794294290, 53.57228050351032067, 6.499999999999979572 ) ) ;
#78659 = CARTESIAN_POINT ( 'NONE',  ( 17.20831665107776587, 47.88393115100078745, 7.208316651077764980 ) ) ;
#78660 = CARTESIAN_POINT ( 'NONE',  ( -2.266590686148945544, 47.22041550158063927, 7.082119434687048631 ) ) ;
#78661 = CARTESIAN_POINT ( 'NONE',  ( -10.44000000000001194, 92.00000000000000000, 9.500000000000000000 ) ) ;
#78662 = ORIENTED_EDGE ( 'NONE', *, *, #81204, .T. ) ;
#78663 =( NAMED_UNIT ( * ) PLANE_ANGLE_UNIT ( ) SI_UNIT ( $, .RADIAN. ) );
#78664 = CARTESIAN_POINT ( 'NONE',  ( 17.20831665107776587, 17.88393115100078745, 7.208316651077764980 ) ) ;
#78665 = CARTESIAN_POINT ( 'NONE',  ( 0.6178305044545818747, 63.49863466993043204, -9.382169495545419124 ) ) ;
#78666 = CARTESIAN_POINT ( 'NONE',  ( 17.20831665107776587, 57.88393115100078745, 7.208316651077764980 ) ) ;
#78667 = CARTESIAN_POINT ( 'NONE',  ( 20.88017736071110164, 65.35535201082150536, 2.915334737309930979 ) ) ;
#78668 = CARTESIAN_POINT ( 'NONE',  ( 14.92337183194729988, 44.34226448433412315, -8.527530157486177487 ) ) ;
#78669 = DIRECTION ( 'NONE',  ( -0.000000000000000000, -1.000000000000000000, -0.000000000000000000 ) ) ;
#78670 = AXIS2_PLACEMENT_3D ( 'NONE', #69911, #30415, #60424 ) ;
#78671 = ORIENTED_EDGE ( 'NONE', *, *, #22411, .T. ) ;
#78672 = CARTESIAN_POINT ( 'NONE',  ( 24.16423886937410614, 64.30374883491396076, 8.672049930838204340E-16 ) ) ;
#78673 = DIRECTION ( 'NONE',  ( 0.000000000000000000, 1.000000000000000000, 0.000000000000000000 ) ) ;
#78674 = CARTESIAN_POINT ( 'NONE',  ( 4.559911319644449179, 48.89701867748817676, 9.422509992056141925 ) ) ;
#78676 = DIRECTION ( 'NONE',  ( -0.9426414910921805390, 0.000000000000000000, 0.3338068592337649076 ) ) ;
#78675 = CARTESIAN_POINT ( 'NONE',  ( 16.40814093676324603, 17.45696800326375353, -11.09922568453594671 ) ) ;
#78677 = CARTESIAN_POINT ( 'NONE',  ( 19.10478245763058780, 66.02576239577082617, -5.990408912944208630 ) ) ;
#78678 = CARTESIAN_POINT ( 'NONE',  ( -14.61046065509105496, 15.00000000000000533, -0.6655452423544750973 ) ) ;
#78679 = CARTESIAN_POINT ( 'NONE',  ( 0.2751277870542909176, 30.30223176428831167, 6.499999999999992006 ) ) ;
#78680 = CARTESIAN_POINT ( 'NONE',  ( 14.92337183194729988, 49.34226448433411605, -8.527530157486177487 ) ) ;
#78681 = CARTESIAN_POINT ( 'NONE',  ( -10.88017736071110164, -37.14464798917849464, -2.915334737309917212 ) ) ;
#78682 = CARTESIAN_POINT ( 'NONE',  ( 13.43411237798106583, 12.66530133659708746, -12.81628187352647252 ) ) ;
#78683 = EDGE_CURVE ( 'NONE', #66913, #47405, #56643, .T. ) ;
#78685 = CARTESIAN_POINT ( 'NONE',  ( 1.711636803080581304, 66.84492782695771496, -6.500000000000075495 ) ) ;
#78684 = CARTESIAN_POINT ( 'NONE',  ( 20.88017736071110519, 10.56368534415483929, 2.639326808657452039E-16 ) ) ;
#78686 = CARTESIAN_POINT ( 'NONE',  ( -4.164238869374099927, 32.01208216824730357, 3.795296366450308767 ) ) ;
#78687 = CARTESIAN_POINT ( 'NONE',  ( 10.00000000000000000, 30.55374883491397142, -14.16423886937410082 ) ) ;
#78688 = CARTESIAN_POINT ( 'NONE',  ( 24.16423886937410614, 64.51208216824728936, -3.795296366450302550 ) ) ;
#78689 = VECTOR ( 'NONE', #87911, 1000.000000000000000 ) ;
#78690 = CARTESIAN_POINT ( 'NONE',  ( 21.09922568453595559, 42.04030133659708213, -6.408140936763230044 ) ) ;
#78691 = CARTESIAN_POINT ( 'NONE',  ( 20.88017736071110164, 15.35535201082150358, 2.915334737309930979 ) ) ;
#78692 = ADVANCED_FACE ( 'NONE', ( #27611 ), #26626, .F. ) ;
#78693 = ORIENTED_EDGE ( 'NONE', *, *, #81843, .F. ) ;
#78694 = CARTESIAN_POINT ( 'NONE',  ( 10.00000000000000000, 39.75893115100078745, -9.846743663894594434 ) ) ;
#78695 = CARTESIAN_POINT ( 'NONE',  ( 15.44008868035555793, 41.39701867748817676, -9.422509992056140149 ) ) ;
#78696 = CARTESIAN_POINT ( 'NONE',  ( 0.1532563361054082862, 66.21726448433413736, 2.638427012816831674 ) ) ;
#78698 = LINE ( 'NONE', #94178, #19962 ) ;
#78697 = CARTESIAN_POINT ( 'NONE',  ( 24.16423886937409904, 24.09541550158063927, 3.795296366450317205 ) ) ;
#78699 = DIRECTION ( 'NONE',  ( 1.483861936729427615E-16, -1.000000000000000000, 0.000000000000000000 ) ) ;
#78700 = ADVANCED_FACE ( 'NONE', ( #12609 ), #58097, .T. ) ;
#78701 = CIRCLE ( 'NONE', #35581, 0.2500000000000002220 ) ;
#78702 = CARTESIAN_POINT ( 'NONE',  ( 2.791683348922237240, 20.38393115100078745, -7.208316651077763204 ) ) ;
#78703 = CARTESIAN_POINT ( 'NONE',  ( -1.099225684535947600, 48.70696800326375353, -6.408140936763238038 ) ) ;
#78704 = CARTESIAN_POINT ( 'NONE',  ( 10.00000000000000178, 57.25893115100078745, 9.846743663894594434 ) ) ;
#78705 = ORIENTED_EDGE ( 'NONE', *, *, #23183, .T. ) ;
#78706 = PRESENTATION_LAYER_ASSIGNMENT (  '', '', ( #73832 ) ) ;
#78707 = CARTESIAN_POINT ( 'NONE',  ( 8.991946320824435901, -4.139779132958989472, -4.000000000000000000 ) ) ;
#78708 = CARTESIAN_POINT ( 'NONE',  ( 13.79529636645031943, 65.34541550158063217, -14.16423886937409904 ) ) ;
#78709 = CARTESIAN_POINT ( 'NONE',  ( 22.26659068614895176, 14.72041550158063572, -7.082119434687042414 ) ) ;
#78710 = CARTESIAN_POINT ( 'NONE',  ( 17.96484262340118221, 64.93868534415483396, 7.964842623401181321 ) ) ;
#78711 = CARTESIAN_POINT ( 'NONE',  ( 1.472469842513823179, 50.59226448433411605, -4.923371831947296329 ) ) ;
#78712 = CARTESIAN_POINT ( 'NONE',  ( 12.91533473730993009, 16.60535201082150891, -10.88017736071109987 ) ) ;
#78713 = COLOUR_RGB ( '', 0.40784314, 0.44705882, 0.49803922) ;
#78714 = CARTESIAN_POINT ( 'NONE',  ( 2.791683348922240793, 66.63393115100079456, 7.208316651077764092 ) ) ;
#78715 = DIRECTION ( 'NONE',  ( 0.000000000000000000, 1.000000000000000000, 0.000000000000000000 ) ) ;
#78716 =( NAMED_UNIT ( * ) SI_UNIT ( $, .STERADIAN. ) SOLID_ANGLE_UNIT ( ) );
#78717 = EDGE_LOOP ( 'NONE', ( #8028, #66097, #10228, #49213 ) ) ;
#78718 = ORIENTED_EDGE ( 'NONE', *, *, #39326, .F. ) ;
#78719 = CARTESIAN_POINT ( 'NONE',  ( -25.69000000000001194, 93.50000000000000000, -9.500000000000000000 ) ) ;
#78720 = CYLINDRICAL_SURFACE ( 'NONE', #83006, 0.2500000000000002220 ) ;
#78721 = CARTESIAN_POINT ( 'NONE',  ( 6.204703633549690345, 37.84541550158063927, 14.16423886937410082 ) ) ;
#78722 = CARTESIAN_POINT ( 'NONE',  ( 0.1532563361054083140, 56.00893115100078745, 1.131784320476157264E-15 ) ) ;
#78723 = CARTESIAN_POINT ( 'NONE',  ( 1.472469842513823179, 25.59226448433412315, -4.923371831947296329 ) ) ;
#78724 = CARTESIAN_POINT ( 'NONE',  ( 18.95785429995052240, 52.24216108172004880, 6.499999999999943157 ) ) ;
#78726 = CARTESIAN_POINT ( 'NONE',  ( 19.84674366389459621, 63.50893115100078745, 7.409399052514197653E-17 ) ) ;
#78725 = CARTESIAN_POINT ( 'NONE',  ( -0.8801773607110991993, 17.85535201082150536, -2.915334737309923874 ) ) ;
#78727 = DIRECTION ( 'NONE',  ( 0.000000000000000000, 0.000000000000000000, 1.000000000000000000 ) ) ;
#78728 = CARTESIAN_POINT ( 'NONE',  ( 24.16423886937410614, 39.51208216824731068, -3.795296366450302550 ) ) ;
#78729 = CARTESIAN_POINT ( 'NONE',  ( 7.084665262690076126, 4.105352010821503583, 10.88017736071109987 ) ) ;
#78730 = FACE_OUTER_BOUND ( 'NONE', #1077, .T. ) ;
#78731 = DIRECTION ( 'NONE',  ( 0.000000000000000000, 1.000000000000000000, 0.000000000000000000 ) ) ;
#78732 = CARTESIAN_POINT ( 'NONE',  ( 10.00000000000000178, 69.31368534415484817, 10.88017736071110342 ) ) ;
#78733 = ADVANCED_FACE ( 'NONE', ( #87128 ), #18649, .T. ) ;
#78734 = CARTESIAN_POINT ( 'NONE',  ( 12.63842701281683034, 12.46726448433411782, 9.846743663894596210 ) ) ;
#78735 = AXIS2_PLACEMENT_3D ( 'NONE', #33338, #33819, #17868 ) ;
#78736 = DIRECTION ( 'NONE',  ( -0.08715574274765114371, -0.9961946980917462113, 0.000000000000000000 ) ) ;
#78737 = ORIENTED_EDGE ( 'NONE', *, *, #93027, .T. ) ;
#78738 = CARTESIAN_POINT ( 'NONE',  ( -14.47650479471825946, 14.63595249122789177, 3.928206833721921587 ) ) ;
#78739 = ORIENTED_EDGE ( 'NONE', *, *, #64, .T. ) ;
#78740 = CARTESIAN_POINT ( 'NONE',  ( 1.472469842513823179, 25.59226448433412315, -4.923371831947296329 ) ) ;
#78741 = EDGE_LOOP ( 'NONE', ( #5663, #78998, #38632, #86877 ) ) ;
#78742 = CARTESIAN_POINT ( 'NONE',  ( -4.164238869374098151, 26.59541550158063217, -3.795296366450310543 ) ) ;
#78743 = CARTESIAN_POINT ( 'NONE',  ( 5.076628168052704559, 40.17559781766745175, -8.527530157486179263 ) ) ;
#78744 = CARTESIAN_POINT ( 'NONE',  ( -0.8801773607111008646, 43.27201867748817676, 2.915334737309923430 ) ) ;
#78745 = AXIS2_PLACEMENT_3D ( 'NONE', #93940, #3931, #33413 ) ;
#78746 = SURFACE_SIDE_STYLE ('',( #47248 ) ) ;
#78748 = EDGE_CURVE ( 'NONE', #57201, #90159, #3299, .T. ) ;
#78747 = ORIENTED_EDGE ( 'NONE', *, *, #35325, .T. ) ;
#78749 = CARTESIAN_POINT ( 'NONE',  ( 10.00000000000000000, 41.81368534415484106, -10.88017736071110342 ) ) ;
#78750 = CIRCLE ( 'NONE', #8436, 7.000000000000002665 ) ;
#78751 = CARTESIAN_POINT ( 'NONE',  ( 0.1916775849787280273, 2.258688159020693753, -6.500000000000000888 ) ) ;
#78752 = CARTESIAN_POINT ( 'NONE',  ( -11.09922568453595382, -1.293031996736242251, -6.408140936763226492 ) ) ;
#78753 = ORIENTED_EDGE ( 'NONE', *, *, #46962, .F. ) ;
#78754 = ORIENTED_EDGE ( 'NONE', *, *, #10646, .F. ) ;
#78755 = ORIENTED_EDGE ( 'NONE', *, *, #43268, .F. ) ;
#78756 = CARTESIAN_POINT ( 'NONE',  ( 21.09922568453594849, 26.20696800326375353, 6.408140936763242479 ) ) ;
#78757 = LINE ( 'NONE', #70775, #79723 ) ;
#78758 = CARTESIAN_POINT ( 'NONE',  ( 2.791683348922237240, 20.38393115100078745, -7.208316651077763204 ) ) ;
#78759 = SURFACE_STYLE_FILL_AREA ( #64220 ) ;
#78760 = DIRECTION ( 'NONE',  ( 1.000000000000000000, 0.000000000000000000, 0.000000000000000000 ) ) ;
#78761 = CARTESIAN_POINT ( 'NONE',  ( 14.92337183194729988, 29.34226448433411960, -8.527530157486177487 ) ) ;
#78762 = CARTESIAN_POINT ( 'NONE',  ( 19.42250999205614548, 55.98035201082150536, -5.440088680355545492 ) ) ;
#78763 = LINE ( 'NONE', #10272, #94529 ) ;
#78764 = DIRECTION ( 'NONE',  ( 1.483861936729427615E-16, -1.000000000000000000, -0.000000000000000000 ) ) ;
#78765 = CARTESIAN_POINT ( 'NONE',  ( 13.43411237798106583, 62.66530133659708923, -12.81628187352647252 ) ) ;
#78766 = CARTESIAN_POINT ( 'NONE',  ( 0.1532563361054100626, 10.80059781766745175, -2.638427012816831230 ) ) ;
#78767 = AXIS2_PLACEMENT_3D ( 'NONE', #40031, #17540, #48007 ) ;
#78768 = CARTESIAN_POINT ( 'NONE',  ( 0.6178305044545818747, 13.49863466993041783, -9.382169495545419124 ) ) ;
#78770 = CARTESIAN_POINT ( 'NONE',  ( 20.30776406404415724, 0.000000000000000000, -5.999999999999999112 ) ) ;
#78769 = AXIS2_PLACEMENT_3D ( 'NONE', #11540, #88522, #73509 ) ;
#78771 = ADVANCED_FACE ( 'NONE', ( #11630 ), #95118, .T. ) ;
#78772 = CARTESIAN_POINT ( 'NONE',  ( 19.84674366389459266, 48.30059781766745175, 2.638427012816836559 ) ) ;
#78773 = DIRECTION ( 'NONE',  ( -0.000000000000000000, -0.000000000000000000, -1.000000000000000000 ) ) ;
#78774 = CARTESIAN_POINT ( 'NONE',  ( 17.08211943468705130, 8.470415501580635720, 12.26659068614894998 ) ) ;
#78775 = CARTESIAN_POINT ( 'NONE',  ( 0.1532563361054082862, 21.21726448433412315, 2.638427012816831674 ) ) ;
#78776 = TOROIDAL_SURFACE ( 'NONE', #35662, 14.49999999999999822, 0.5000000000000000000 ) ;
#78777 = CARTESIAN_POINT ( 'NONE',  ( 19.38216949554541557, 37.24863466993041783, -9.382169495545420901 ) ) ;
#78778 = CARTESIAN_POINT ( 'NONE',  ( -0.8801773607111009756, 23.27201867748817676, 2.915334737309923874 ) ) ;
#78779 = CARTESIAN_POINT ( 'NONE',  ( -0.8801773607110991993, 42.85535201082150536, -2.915334737309923874 ) ) ;
#78780 = CARTESIAN_POINT ( 'NONE',  ( 13.43411237798106583, 2.665301336597086568, -12.81628187352647252 ) ) ;
#78781 = LINE ( 'NONE', #11752, #31143 ) ;
#78782 = EDGE_CURVE ( 'NONE', #66580, #10785, #51196, .T. ) ;
#78783 = CARTESIAN_POINT ( 'NONE',  ( 18.52753015748617571, 18.09226448433411960, 4.923371831947298993 ) ) ;
#78784 = CARTESIAN_POINT ( 'NONE',  ( 0.5774900079438590739, 32.64701867748816966, -5.440088680355550821 ) ) ;
#78785 = CARTESIAN_POINT ( 'NONE',  ( 13.43411237798105340, 35.58196800326375353, 12.81628187352647963 ) ) ;
#78786 = CARTESIAN_POINT ( 'NONE',  ( 14.92337183194729633, 22.67559781766745175, 8.527530157486181039 ) ) ;
#78787 =( BOUNDED_SURFACE ( )  B_SPLINE_SURFACE ( 3, 2, ( 
 ( #60952, #60467, #7491 ),
 ( #92926, #90956, #22488 ),
 ( #52961, #37987, #68478 ),
 ( #53954, #91461, #22987 ),
 ( #76460, #38474, #498 ),
 ( #84944, #46452, #76945 ),
 ( #8455, #69948, #972 ),
 ( #31433, #61936, #31921 ),
 ( #92437, #23961, #46935 ),
 ( #39458, #1468, #87401 ),
 ( #17450, #33396, #62926 ),
 ( #9938, #17931, #78422 ),
 ( #40442, #32425, #26396 ),
 ( #47916, #18420, #70441 ) ),
 .UNSPECIFIED., .F., .F., .F. ) 
 B_SPLINE_SURFACE_WITH_KNOTS ( ( 4, 2, 2, 2, 2, 2, 4 ),
 ( 3, 3 ),
 ( 0.000000000000000000, 0.004797171936611956643, 0.007195757904917934530, 0.009594343873223913285, 0.01199292984152989031, 0.01439151580983586906, 0.01918868774644782657 ),
 ( 0.000000000000000000, 1.000000000000000000 ),
 .UNSPECIFIED. ) 
 GEOMETRIC_REPRESENTATION_ITEM ( )  RATIONAL_B_SPLINE_SURFACE ( (
 ( 1.000000000000000000, 0.7071067811865475727, 1.000000000000000000),
 ( 1.000000000000000000, 0.7404680669573554530, 1.000000000000000000),
 ( 1.000000000000000000, 0.7699744256204830162, 1.000000000000000000),
 ( 1.000000000000000000, 0.8013264333401337591, 1.000000000000000000),
 ( 1.000000000000000000, 0.8096066803150596680, 1.000000000000000000),
 ( 1.000000000000000000, 0.8208168491805714062, 1.000000000000000000),
 ( 1.000000000000000000, 0.8237352673350482046, 1.000000000000000000),
 ( 1.000000000000000000, 0.8237872525054150685, 1.000000000000000000),
 ( 1.000000000000000000, 0.8209201555335595701, 1.000000000000000000),
 ( 1.000000000000000000, 0.8097813946840403121, 1.000000000000000000),
 ( 1.000000000000000000, 0.8015207097676279036, 1.000000000000000000),
 ( 1.000000000000000000, 0.7701797223629573974, 1.000000000000000000),
 ( 1.000000000000000000, 0.7406378784107900959, 1.000000000000000000),
 ( 1.000000000000000000, 0.7071067811865475727, 1.000000000000000000) ) ) 
 REPRESENTATION_ITEM ( '' )  SURFACE ( )  );
#78788 = CARTESIAN_POINT ( 'NONE',  ( -8.669785729375572458, 87.01784090252159842, 4.324025984537457568 ) ) ;
#78789 = CARTESIAN_POINT ( 'NONE',  ( -0.8801773607110991993, 22.85535201082150181, -2.915334737309923874 ) ) ;
#78790 = VERTEX_POINT ( 'NONE', #51107 ) ;
#78791 = CARTESIAN_POINT ( 'NONE',  ( 2.035157376598822676, 67.43868534415484817, -7.964842623401177768 ) ) ;
#78792 = CARTESIAN_POINT ( 'NONE',  ( -0.8801773607111008646, 8.272018677488171434, 2.915334737309923430 ) ) ;
#78794 = CARTESIAN_POINT ( 'NONE',  ( 12.91533473730993009, 16.60535201082150891, -10.88017736071109987 ) ) ;
#78793 = CARTESIAN_POINT ( 'NONE',  ( 2.791683348922240793, 41.63393115100078745, 7.208316651077764092 ) ) ;
#78795 = CARTESIAN_POINT ( 'NONE',  ( -5.806645064956620139, 15.00000000000000888, 13.42464971016990205 ) ) ;
#78796 = CARTESIAN_POINT ( 'NONE',  ( 17.96484262340118221, 39.93868534415484106, 7.964842623401181321 ) ) ;
#78797 = CARTESIAN_POINT ( 'NONE',  ( 2.035157376598822676, 7.438685344154837509, -7.964842623401177768 ) ) ;
#78798 = CARTESIAN_POINT ( 'NONE',  ( 12.63842701281683922, 34.55059781766745886, -9.846743663894590881 ) ) ;
#78799 = CARTESIAN_POINT ( 'NONE',  ( 17.99999999999999645, 78.20646178170991902, -3.828774214053709990 ) ) ;
#78800 = FACE_OUTER_BOUND ( 'NONE', #10405, .T. ) ;
#78801 = CARTESIAN_POINT ( 'NONE',  ( -2.266590686148945544, 26.38708216824730357, -7.082119434687050408 ) ) ;
#78802 = EDGE_CURVE ( 'NONE', #15653, #44561, #97540, .T. ) ;
#78803 = PLANE ( 'NONE',  #9793 ) ;
#78804 = EDGE_LOOP ( 'NONE', ( #62117, #98925, #17664, #47134 ) ) ;
#78805 = CARTESIAN_POINT ( 'NONE',  ( 20.88017736071110164, 5.355352010821503583, 2.915334737309930979 ) ) ;
#78806 = CARTESIAN_POINT ( 'NONE',  ( 18.52753015748617571, 28.09226448433411960, 4.923371831947298993 ) ) ;
#78808 = FILL_AREA_STYLE_COLOUR ( '', #58197 ) ;
#78807 = CARTESIAN_POINT ( 'NONE',  ( -10.19513985507840736, 15.00000000000000000, 11.00268709613209950 ) ) ;
#78809 = CARTESIAN_POINT ( 'NONE',  ( 19.42250999205614548, 45.98035201082150536, -5.440088680355545492 ) ) ;
#78810 = CARTESIAN_POINT ( 'NONE',  ( 22.81628187352647785, 61.62363466993041783, 6.195893100308588602E-16 ) ) ;
#78811 = EDGE_CURVE ( 'NONE', #31048, #64121, #58514, .T. ) ;
#78812 = CARTESIAN_POINT ( 'NONE',  ( 2.035157376598824452, 33.68868534415484106, 7.964842623401179544 ) ) ;
#78813 = CARTESIAN_POINT ( 'NONE',  ( 0.000000000000000000, 0.5000000000000004441, 0.000000000000000000 ) ) ;
#78814 = CARTESIAN_POINT ( 'NONE',  ( 16.40814093676323893, 15.79030133659708746, 11.09922568453595026 ) ) ;
#78815 = CARTESIAN_POINT ( 'NONE',  ( 5.076628168052703671, 16.84226448433411960, 8.527530157486179263 ) ) ;
#78816 = ORIENTED_EDGE ( 'NONE', *, *, #11409, .T. ) ;
#78817 = FILL_AREA_STYLE ('',( #19296 ) ) ;
#78818 = DIRECTION ( 'NONE',  ( 0.6225146366376078655, 0.000000000000000000, 0.7826081568524232424 ) ) ;
#78819 = CARTESIAN_POINT ( 'NONE',  ( 10.00000000000000178, 58.05374883491397497, 14.16423886937410082 ) ) ;
#78820 = CARTESIAN_POINT ( 'NONE',  ( -0.3689425029237881626, 27.42874883491397142, 10.36894250292379027 ) ) ;
#78821 = CARTESIAN_POINT ( 'NONE',  ( 4.559911319644449179, 18.89701867748817321, 9.422509992056141925 ) ) ;
#78822 = CARTESIAN_POINT ( 'NONE',  ( 7.084665262690076126, 47.02201867748818387, -10.88017736071110164 ) ) ;
#78823 = FACE_OUTER_BOUND ( 'NONE', #36062, .T. ) ;
#78824 = CARTESIAN_POINT ( 'NONE',  ( 8.630000000000002558, -0.01510857754941254301, -4.000000000000000000 ) ) ;
#78825 = CARTESIAN_POINT ( 'NONE',  ( 2.791683348922240793, 16.63393115100078745, 7.208316651077764092 ) ) ;
#78826 = CARTESIAN_POINT ( 'NONE',  ( -14.62617646268090432, 0.3640475087720987935, 3.327906561566782884 ) ) ;
#78827 = CARTESIAN_POINT ( 'NONE',  ( 2.791683348922240793, 16.63393115100078745, 7.208316651077764092 ) ) ;
#78828 = FILL_AREA_STYLE_COLOUR ( '', #98613 ) ;
#78829 = CARTESIAN_POINT ( 'NONE',  ( 0.000000000000000000, 15.00000000000000000, 0.000000000000000000 ) ) ;
#78830 = CARTESIAN_POINT ( 'NONE',  ( 14.92337183194729988, 24.34226448433411960, -8.527530157486177487 ) ) ;
#78831 = CARTESIAN_POINT ( 'NONE',  ( 10.00000000000000178, 52.25893115100078745, 9.846743663894594434 ) ) ;
#78832 = CARTESIAN_POINT ( 'NONE',  ( 19.38216949554541557, 37.24863466993041783, -9.382169495545420901 ) ) ;
#78833 = CARTESIAN_POINT ( 'NONE',  ( -0.8801773607110991993, 57.85535201082149825, -2.915334737309923874 ) ) ;
#78834 = CARTESIAN_POINT ( 'NONE',  ( 14.92337183194729988, 29.34226448433411960, -8.527530157486177487 ) ) ;
#78836 = CARTESIAN_POINT ( 'NONE',  ( 19.84674366389459621, 18.50893115100078745, 7.409399052514197653E-17 ) ) ;
#78835 = CARTESIAN_POINT ( 'NONE',  ( -0.3689425029237881626, 42.42874883491396787, 10.36894250292379027 ) ) ;
#78837 = FACE_OUTER_BOUND ( 'NONE', #34582, .T. ) ;
#78838 = CARTESIAN_POINT ( 'NONE',  ( 2.791683348922240793, 46.63393115100077324, 7.208316651077764092 ) ) ;
#78840 = CARTESIAN_POINT ( 'NONE',  ( 24.16423886937410614, 4.303748834913967869, 8.672049930838204340E-16 ) ) ;
#78839 = CARTESIAN_POINT ( 'NONE',  ( 5.076628168052703671, 36.84226448433412315, 8.527530157486179263 ) ) ;
#78841 = CARTESIAN_POINT ( 'NONE',  ( -0.3689425029237898834, 16.17874883491396076, -10.36894250292378850 ) ) ;
#78842 = CARTESIAN_POINT ( 'NONE',  ( 14.92337183194729988, 24.34226448433411960, -8.527530157486177487 ) ) ;
#78843 = CARTESIAN_POINT ( 'NONE',  ( 7.084665262690076126, 42.02201867748816966, -10.88017736071110164 ) ) ;
#78844 = CARTESIAN_POINT ( 'NONE',  ( 17.96484262340118221, 19.93868534415484106, 7.964842623401181321 ) ) ;
#78845 = VECTOR ( 'NONE', #27423, 1000.000000000000000 ) ;
#78846 = EDGE_CURVE ( 'NONE', #28832, #74162, #55799, .T. ) ;
#78847 = CARTESIAN_POINT ( 'NONE',  ( 19.42250999205614193, 45.14701867748817676, 5.440088680355555262 ) ) ;
#78848 = CARTESIAN_POINT ( 'NONE',  ( 10.00000000000000000, 26.81368534415484106, -10.88017736071110342 ) ) ;
#78849 = EDGE_LOOP ( 'NONE', ( #50859, #75174, #18236, #6162 ) ) ;
#78850 = CARTESIAN_POINT ( 'NONE',  ( -0.8801773607111008646, 53.27201867748816966, 2.915334737309923430 ) ) ;
#78851 = ORIENTED_EDGE ( 'NONE', *, *, #23514, .F. ) ;
#78852 = CARTESIAN_POINT ( 'NONE',  ( 1.780824192092403058, 15.00000000000000000, 14.89391369643514729 ) ) ;
#78853 = CARTESIAN_POINT ( 'NONE',  ( 15.44008868035555260, 64.73035201082151957, 9.422509992056143702 ) ) ;
#78854 = ORIENTED_EDGE ( 'NONE', *, *, #94864, .F. ) ;
#78855 = CARTESIAN_POINT ( 'NONE',  ( 17.96484262340118221, 61.18868534415482685, -7.964842623401177768 ) ) ;
#78856 = FILL_AREA_STYLE ('',( #70384 ) ) ;
#78857 = FACE_OUTER_BOUND ( 'NONE', #22514, .T. ) ;
#78858 = DIRECTION ( 'NONE',  ( -0.000000000000000000, 1.000000000000000000, 0.000000000000000000 ) ) ;
#78859 = CARTESIAN_POINT ( 'NONE',  ( 13.79529636645031943, 55.34541550158062506, -14.16423886937409904 ) ) ;
#78860 = CARTESIAN_POINT ( 'NONE',  ( 2.791683348922237240, 5.383931151000785675, -7.208316651077763204 ) ) ;
#78861 = CARTESIAN_POINT ( 'NONE',  ( 22.26659068614895176, 4.720415501580633943, -7.082119434687042414 ) ) ;
#78862 =( BOUNDED_CURVE ( )  B_SPLINE_CURVE ( 2, ( #31431, #496, #30945, #10795, #53450, #68964, #63769, #33278, #79775 ),
 .UNSPECIFIED., .F., .T. ) 
 B_SPLINE_CURVE_WITH_KNOTS ( ( 3, 2, 2, 2, 3 ),
 ( 0.1901409369402313476, 0.1904761904761904656, 0.1964285714285713969, 0.2023809523809524391, 0.2027162059169115571 ),
 .UNSPECIFIED. ) 
 CURVE ( )  GEOMETRIC_REPRESENTATION_ITEM ( )  RATIONAL_B_SPLINE_CURVE ( ( 0.9963778908391762723, 0.9980808541467921513, 1.000000000000000000, 0.9659258262890682012, 1.000000000000000000, 0.9659258262890682012, 1.000000000000000000, 0.9980808541467921513, 0.9963778908391762723 ) ) 
 REPRESENTATION_ITEM ( '' )  );
#78863 = CARTESIAN_POINT ( 'NONE',  ( 1.472469842513823179, 5.592264484334118713, -4.923371831947296329 ) ) ;
#78864 = CARTESIAN_POINT ( 'NONE',  ( 12.91533473730993009, 6.605352010821504471, -10.88017736071109987 ) ) ;
#78865 = CARTESIAN_POINT ( 'NONE',  ( 17.20831665107776587, 47.88393115100078745, 7.208316651077764980 ) ) ;
#78866 = ORIENTED_EDGE ( 'NONE', *, *, #54063, .F. ) ;
#78867 = CARTESIAN_POINT ( 'NONE',  ( 0.1532563361054100626, 45.80059781766745886, -2.638427012816831230 ) ) ;
#78868 = VERTEX_POINT ( 'NONE', #30071 ) ;
#78869 = DIRECTION ( 'NONE',  ( 0.000000000000000000, 0.000000000000000000, 1.000000000000000000 ) ) ;
#78870 = CARTESIAN_POINT ( 'NONE',  ( -0.8801773607111009756, 48.06368534415484817, 1.068504757029289695E-15 ) ) ;
#78871 = CARTESIAN_POINT ( 'NONE',  ( 2.791683348922240793, 51.63393115100078745, 7.208316651077764092 ) ) ;
#78873 = CYLINDRICAL_SURFACE ( 'NONE', #46314, 15.00000000000000000 ) ;
#78872 =( NAMED_UNIT ( * ) PLANE_ANGLE_UNIT ( ) SI_UNIT ( $, .RADIAN. ) );
#78874 = CARTESIAN_POINT ( 'NONE',  ( 12.91533473730992121, 59.52201867748816966, 10.88017736071110164 ) ) ;
#78875 = CARTESIAN_POINT ( 'NONE',  ( 20.88017736071110164, 5.355352010821503583, 2.915334737309930979 ) ) ;
#78876 = CARTESIAN_POINT ( 'NONE',  ( 0.6178305044545818747, 38.49863466993042493, -9.382169495545419124 ) ) ;
#78877 = CARTESIAN_POINT ( 'NONE',  ( 0.000000000000000000, 0.5000000000000004441, 0.000000000000000000 ) ) ;
#78878 = ORIENTED_EDGE ( 'NONE', *, *, #73538, .F. ) ;
#78879 = CARTESIAN_POINT ( 'NONE',  ( 13.43411237798106583, 27.66530133659708568, -12.81628187352647252 ) ) ;
#78880 = CARTESIAN_POINT ( 'NONE',  ( 7.084665262690076126, 32.02201867748816966, -10.88017736071110164 ) ) ;
#78881 = ORIENTED_EDGE ( 'NONE', *, *, #35665, .T. ) ;
#78882 = CARTESIAN_POINT ( 'NONE',  ( 1.472469842513823179, 10.59226448433411782, -4.923371831947296329 ) ) ;
#78883 = CARTESIAN_POINT ( 'NONE',  ( 14.92337183194729633, 62.67559781766745886, 8.527530157486181039 ) ) ;
#78885 = CARTESIAN_POINT ( 'NONE',  ( 1.472469842513823179, 55.59226448433412315, -4.923371831947296329 ) ) ;
#78884 = CARTESIAN_POINT ( 'NONE',  ( 19.84674366389459266, 18.71726448433411960, -2.638427012816827677 ) ) ;
#78886 = CARTESIAN_POINT ( 'NONE',  ( -8.899009838862365740, -15.58694756607049570, 3.749999999999999112 ) ) ;
#78887 = CARTESIAN_POINT ( 'NONE',  ( 0.000000000000000000, 0.5000000000000004441, 0.000000000000000000 ) ) ;
#78888 = CARTESIAN_POINT ( 'NONE',  ( 0.1532563361054082862, 41.21726448433411605, 2.638427012816831674 ) ) ;
#78889 = CARTESIAN_POINT ( 'NONE',  ( -14.66148682522520019, 14.76984938411755088, -2.874551585517384211 ) ) ;
#78890 = CARTESIAN_POINT ( 'NONE',  ( 1.046131998950050379, 60.73810908735726599, 6.499999999999992006 ) ) ;
#78891 = EDGE_CURVE ( 'NONE', #53272, #21472, #75172, .T. ) ;
#78893 = CARTESIAN_POINT ( 'NONE',  ( 2.791683348922237240, 0.3839311510007847872, -7.208316651077763204 ) ) ;
#78892 = CARTESIAN_POINT ( 'NONE',  ( 5.076628168052704559, 30.17559781766745175, -8.527530157486179263 ) ) ;
#78894 = CARTESIAN_POINT ( 'NONE',  ( 3.115783986955464435, 4.832823856176936692E-16, 14.16128137375399731 ) ) ;
#78896 = ORIENTED_EDGE ( 'NONE', *, *, #64209, .F. ) ;
#78895 = CARTESIAN_POINT ( 'NONE',  ( 10.00000000000000000, 59.75893115100078745, -9.846743663894594434 ) ) ;
#78897 = CYLINDRICAL_SURFACE ( 'NONE', #50197, 0.2500000000000002220 ) ;
#78898 = CARTESIAN_POINT ( 'NONE',  ( -2.816281873526473856, 19.33196800326375708, 3.434112377981055619 ) ) ;
#78899 = CARTESIAN_POINT ( 'NONE',  ( 5.076628168052704559, 50.17559781766745886, -8.527530157486179263 ) ) ;
#78900 = AXIS2_PLACEMENT_3D ( 'NONE', #6163, #75143, #67662 ) ;
#78901 = CARTESIAN_POINT ( 'NONE',  ( 12.80781515976310203, 15.00000000000000000, 6.246788841744411513 ) ) ;
#78902 = CARTESIAN_POINT ( 'NONE',  ( 2.917880565312948704, 47.63708216824730357, 12.26659068614894643 ) ) ;
#78903 = CARTESIAN_POINT ( 'NONE',  ( 0.1532563361054082862, 16.21726448433411960, 2.638427012816831674 ) ) ;
#78904 = EDGE_LOOP ( 'NONE', ( #30527, #8651, #37202, #45950 ) ) ;
#78905 = CARTESIAN_POINT ( 'NONE',  ( -12.98685442714204008, 4.660809545892429844E-16, 6.449155920600864178 ) ) ;
#78906 = CIRCLE ( 'NONE', #61348, 15.00000000000000000 ) ;
#78907 = CARTESIAN_POINT ( 'NONE',  ( 13.79529636645030344, 48.26208216824728936, 14.16423886937410614 ) ) ;
#78908 = CARTESIAN_POINT ( 'NONE',  ( 1.472469842513823179, 61.42559781766745175, 4.923371831947296329 ) ) ;
#78909 = CARTESIAN_POINT ( 'NONE',  ( 15.44008868035555793, 6.397018677488171434, -9.422509992056140149 ) ) ;
#78910 = CARTESIAN_POINT ( 'NONE',  ( -2.266590686148945544, 27.22041550158063572, 7.082119434687048631 ) ) ;
#78911 = CARTESIAN_POINT ( 'NONE',  ( 17.08211943468705130, 43.47041550158063927, 12.26659068614894998 ) ) ;
#78912 = DIRECTION ( 'NONE',  ( 0.000000000000000000, 1.000000000000000000, 0.000000000000000000 ) ) ;
#78914 = CARTESIAN_POINT ( 'NONE',  ( 17.20831665107776587, 52.88393115100078035, 7.208316651077764980 ) ) ;
#78913 = DIRECTION ( 'NONE',  ( 0.000000000000000000, -1.000000000000000000, -0.000000000000000000 ) ) ;
#78915 = CARTESIAN_POINT ( 'NONE',  ( 10.00000000000000000, 36.81368534415484106, -10.88017736071110342 ) ) ;
#78916 = CARTESIAN_POINT ( 'NONE',  ( 10.76493118081690881, 15.00000000000000888, -9.902252441915713632 ) ) ;
#78917 = CARTESIAN_POINT ( 'NONE',  ( 10.35044781186116936, -32.03405546004147908, 3.750000000000000000 ) ) ;
#78918 = CARTESIAN_POINT ( 'NONE',  ( 10.00000000000000178, 37.25893115100078745, 9.846743663894594434 ) ) ;
#78919 = CARTESIAN_POINT ( 'NONE',  ( 6.565887622018943937, 63.08196800326376064, -12.81628187352647608 ) ) ;
#78920 = CARTESIAN_POINT ( 'NONE',  ( -5.204170427930421283E-15, 10.55374883491398030, -14.16423886937410082 ) ) ;
#78921 = CARTESIAN_POINT ( 'NONE',  ( 7.361572987183170547, 62.05059781766745886, 9.846743663894590881 ) ) ;
#78922 = CARTESIAN_POINT ( 'NONE',  ( 2.791683348922240793, 61.63393115100079456, 7.208316651077764092 ) ) ;
#78923 = ADVANCED_FACE ( 'NONE', ( #29572 ), #15104, .F. ) ;
#78924 = EDGE_LOOP ( 'NONE', ( #21371, #84763, #43074, #30421 ) ) ;
#78925 = CARTESIAN_POINT ( 'NONE',  ( 6.204703633549690345, 32.84541550158063927, 14.16423886937410082 ) ) ;
#78926 = CARTESIAN_POINT ( 'NONE',  ( -12.58781651029194393, 15.00000000000000533, -7.446837378630896787 ) ) ;
#78928 = DIRECTION ( 'NONE',  ( -1.000000000000000000, 0.000000000000000000, 0.000000000000000000 ) ) ;
#78927 = CARTESIAN_POINT ( 'NONE',  ( -3.500000000000000444, 1.019547802438453887, -2.750000000000000000 ) ) ;
#78929 = CARTESIAN_POINT ( 'NONE',  ( 19.42250999205614193, 5.147018677488171434, 5.440088680355555262 ) ) ;
#78930 = CARTESIAN_POINT ( 'NONE',  ( 3.591859063236763294, 18.29030133659708568, -11.09922568453595026 ) ) ;
#78931 = EDGE_CURVE ( 'NONE', #34672, #1705, #60697, .T. ) ;
#78932 = CARTESIAN_POINT ( 'NONE',  ( 0.1532563361054100626, 10.80059781766745175, -2.638427012816831230 ) ) ;
#78933 = CARTESIAN_POINT ( 'NONE',  ( 4.645844135293939914, -0.8374644621422210333, -4.000000000000000000 ) ) ;
#78934 = CARTESIAN_POINT ( 'NONE',  ( 20.25388882277826141, 0.000000000000000000, -6.092555545977055509 ) ) ;
#78935 = CARTESIAN_POINT ( 'NONE',  ( -0.03932841506541493587, 43.12161441960501662, 6.397827110479010315 ) ) ;
#78936 = CARTESIAN_POINT ( 'NONE',  ( 10.00000000000000000, 11.81368534415483751, -10.88017736071110342 ) ) ;
#78937 = DIRECTION ( 'NONE',  ( -1.000000000000000000, 0.000000000000000000, 0.000000000000000000 ) ) ;
#78938 = CARTESIAN_POINT ( 'NONE',  ( 19.42250999205614193, 35.14701867748816966, 5.440088680355555262 ) ) ;
#78939 = CARTESIAN_POINT ( 'NONE',  ( -0.8801773607111009756, 43.06368534415484106, 1.068504757029289695E-15 ) ) ;
#78940 = CARTESIAN_POINT ( 'NONE',  ( 10.00000000000000178, 67.25893115100079456, 9.846743663894594434 ) ) ;
#78941 = CARTESIAN_POINT ( 'NONE',  ( -45.35639774302337912, 104.5887517005673004, -5.643674680800299548 ) ) ;
#78942 = CARTESIAN_POINT ( 'NONE',  ( 12.63842701281683034, 12.46726448433411782, 9.846743663894596210 ) ) ;
#78943 = ORIENTED_EDGE ( 'NONE', *, *, #45890, .F. ) ;
#78944 = CIRCLE ( 'NONE', #26260, 0.2500000000000002220 ) ;
#78945 = CARTESIAN_POINT ( 'NONE',  ( 17.96484262340118221, 36.18868534415484106, -7.964842623401177768 ) ) ;
#78946 = CARTESIAN_POINT ( 'NONE',  ( 16.40814093676323893, 35.79030133659708923, 11.09922568453595026 ) ) ;
#78947 = CARTESIAN_POINT ( 'NONE',  ( 19.72487221294571569, 34.78217586085237656, 6.499999999999993783 ) ) ;
#78948 = CARTESIAN_POINT ( 'NONE',  ( 1.472469842513823179, 61.42559781766745175, 4.923371831947296329 ) ) ;
#78949 = CARTESIAN_POINT ( 'NONE',  ( 12.91533473730992121, 64.52201867748817676, 10.88017736071110164 ) ) ;
#78950 = CARTESIAN_POINT ( 'NONE',  ( 18.52753015748618282, 13.92559781766745175, -4.923371831947291888 ) ) ;
#78951 = CARTESIAN_POINT ( 'NONE',  ( 22.81628187352647785, 36.62363466993041783, 6.195893100308588602E-16 ) ) ;
#78953 = DIRECTION ( 'NONE',  ( 0.000000000000000000, 0.000000000000000000, 1.000000000000000000 ) ) ;
#78952 = CARTESIAN_POINT ( 'NONE',  ( 12.91533473730992121, 64.52201867748817676, 10.88017736071110164 ) ) ;
#78954 = CARTESIAN_POINT ( 'NONE',  ( 3.591859063236761518, 59.95696800326375353, 11.09922568453594849 ) ) ;
#78955 = ORIENTED_EDGE ( 'NONE', *, *, #14144, .F. ) ;
#78956 = CARTESIAN_POINT ( 'NONE',  ( 2.781662917646512463E-16, 22.11937003968011695, 0.000000000000000000 ) ) ;
#78957 = CARTESIAN_POINT ( 'NONE',  ( 20.88017736071110875, 10.77201867748817143, -2.915334737309920765 ) ) ;
#78958 = CARTESIAN_POINT ( 'NONE',  ( 13.43411237798106583, 57.66530133659708923, -12.81628187352647252 ) ) ;
#78959 = CARTESIAN_POINT ( 'NONE',  ( 2.791683348922240793, 21.63393115100078745, 7.208316651077764092 ) ) ;
#78960 = CARTESIAN_POINT ( 'NONE',  ( 14.92337183194729633, 22.67559781766745175, 8.527530157486181039 ) ) ;
#78961 = CARTESIAN_POINT ( 'NONE',  ( 6.204703633549690345, 57.84541550158063927, 14.16423886937410082 ) ) ;
#78962 = ORIENTED_EDGE ( 'NONE', *, *, #95741, .T. ) ;
#78963 = CARTESIAN_POINT ( 'NONE',  ( 0.5774900079438607392, 13.48035201082150358, 5.440088680355550821 ) ) ;
#78964 = ADVANCED_FACE ( 'NONE', ( #59092 ), #53567, .T. ) ;
#78965 = CARTESIAN_POINT ( 'NONE',  ( 0.5774900079438607392, 18.48035201082150536, 5.440088680355550821 ) ) ;
#78966 = B_SPLINE_CURVE_WITH_KNOTS ( 'NONE', 3,
 ( #91528, #1033, #16522, #9002, #2026, #92011 ),
 .UNSPECIFIED., .F., .F.,
 ( 4, 2, 4 ),
 ( 0.000000000000000000, 0.0002565770811490979868, 0.0005131541622981959736 ),
 .UNSPECIFIED. ) ;
#78967 = CARTESIAN_POINT ( 'NONE',  ( 2.377183314879972809, 30.78593319516822291, -6.499999999999988454 ) ) ;
#78968 = ORIENTED_EDGE ( 'NONE', *, *, #64451, .T. ) ;
#78969 = ORIENTED_EDGE ( 'NONE', *, *, #3989, .F. ) ;
#78970 = CARTESIAN_POINT ( 'NONE',  ( 19.42250999205614548, 20.98035201082150891, -5.440088680355545492 ) ) ;
#78971 = CARTESIAN_POINT ( 'NONE',  ( 12.63842701281683922, 54.55059781766745175, -9.846743663894590881 ) ) ;
#78972 = CARTESIAN_POINT ( 'NONE',  ( 22.81628187352647785, 46.62363466993041783, 6.195893100308588602E-16 ) ) ;
#78973 = DIRECTION ( 'NONE',  ( -1.000000000000000000, 0.000000000000000000, 0.000000000000000000 ) ) ;
#78975 = CARTESIAN_POINT ( 'NONE',  ( 24.16423886937410614, 24.30374883491396787, 8.672049930838204340E-16 ) ) ;
#78974 = COLOUR_RGB ( '', 0.08235294, 0.09019608, 0.10196078) ;
#78976 = CARTESIAN_POINT ( 'NONE',  ( 7.084665262690076126, 34.10535201082151247, 10.88017736071109987 ) ) ;
#78977 = CARTESIAN_POINT ( 'NONE',  ( 10.00000000000000000, 16.81368534415483751, -10.88017736071110342 ) ) ;
#78978 = CARTESIAN_POINT ( 'NONE',  ( 0.1532563361054083140, 51.00893115100078745, 1.131784320476157264E-15 ) ) ;
#78979 = STYLED_ITEM ( 'NONE', ( #49401 ), #90548 ) ;
#78980 = DIRECTION ( 'NONE',  ( 1.000000000000000000, -0.000000000000000000, -0.000000000000000000 ) ) ;
#78981 = CARTESIAN_POINT ( 'NONE',  ( 0.1532563361054082862, 31.21726448433412315, 2.638427012816831674 ) ) ;
#78982 = AXIS2_PLACEMENT_3D ( 'NONE', #75490, #38489, #68493 ) ;
#78983 = DIRECTION ( 'NONE',  ( -0.000000000000000000, 1.000000000000000000, 0.000000000000000000 ) ) ;
#78984 = CARTESIAN_POINT ( 'NONE',  ( 18.52753015748617571, 13.09226448433411960, 4.923371831947298993 ) ) ;
#78985 = CARTESIAN_POINT ( 'NONE',  ( 6.408140936763236262, -37.54303199673623936, -11.09922568453595026 ) ) ;
#78986 = ORIENTED_EDGE ( 'NONE', *, *, #77317, .F. ) ;
#78987 = LINE ( 'NONE', #40515, #98929 ) ;
#78988 = CARTESIAN_POINT ( 'NONE',  ( 14.92337183194729988, 14.34226448433411782, -8.527530157486177487 ) ) ;
#78989 = CARTESIAN_POINT ( 'NONE',  ( 7.361572987183170547, 67.05059781766746596, 9.846743663894590881 ) ) ;
#78991 = CARTESIAN_POINT ( 'NONE',  ( 0.5774900079438607392, 48.48035201082150536, 5.440088680355550821 ) ) ;
#78990 = CARTESIAN_POINT ( 'NONE',  ( 0.5774900079438590739, 47.64701867748817676, -5.440088680355550821 ) ) ;
#78993 = CARTESIAN_POINT ( 'NONE',  ( -2.816281873526473856, 49.33196800326374643, 3.434112377981055619 ) ) ;
#78992 = CARTESIAN_POINT ( 'NONE',  ( 15.44008868035555260, 14.73035201082150536, 9.422509992056143702 ) ) ;
#78994 = CARTESIAN_POINT ( 'NONE',  ( 24.16423886937410614, 29.51208216824729647, -3.795296366450302550 ) ) ;
#78995 = CARTESIAN_POINT ( 'NONE',  ( 20.24186590665277663, 11.76028685723174227, 6.114288769123037426 ) ) ;
#78996 = AXIS2_PLACEMENT_3D ( 'NONE', #9828, #71800, #64275 ) ;
#78997 = CARTESIAN_POINT ( 'NONE',  ( 6.565887622018943937, 58.08196800326376064, -12.81628187352647608 ) ) ;
#78998 = ORIENTED_EDGE ( 'NONE', *, *, #43116, .F. ) ;
#78999 = CARTESIAN_POINT ( 'NONE',  ( 18.52753015748617571, 63.09226448433412315, 4.923371831947298993 ) ) ;
#79000 = CARTESIAN_POINT ( 'NONE',  ( 0.5774900079438607392, 38.48035201082150536, 5.440088680355550821 ) ) ;
#79001 = ORIENTED_EDGE ( 'NONE', *, *, #43710, .F. ) ;
#79002 = CARTESIAN_POINT ( 'NONE',  ( 5.076628168052704559, 0.1755978176674514724, -8.527530157486179263 ) ) ;
#79003 = CARTESIAN_POINT ( 'NONE',  ( 3.469446951953614189E-15, 5.938309369127516391, 11.92686044187656513 ) ) ;
#79004 = B_SPLINE_CURVE_WITH_KNOTS ( 'NONE', 3,
 ( #29477, #37507, #44495, #60969 ),
 .UNSPECIFIED., .F., .F.,
 ( 4, 4 ),
 ( 2.478060227011367871E-17, 0.002392975128318431711 ),
 .UNSPECIFIED. ) ;
#79005 = CARTESIAN_POINT ( 'NONE',  ( 2.791683348922240793, 11.63393115100078568, 7.208316651077764092 ) ) ;
#79006 = CARTESIAN_POINT ( 'NONE',  ( 2.035157376598824452, 63.68868534415484106, 7.964842623401179544 ) ) ;
#79007 = CARTESIAN_POINT ( 'NONE',  ( -5.999999999999994671, 43.00000000000000000, -6.500000000000000888 ) ) ;
#79008 = ADVANCED_FACE ( 'NONE', ( #83587 ), #22103, .F. ) ;
#79009 = CARTESIAN_POINT ( 'NONE',  ( 15.44008868035555260, 54.73035201082150536, 9.422509992056143702 ) ) ;
#79010 = CARTESIAN_POINT ( 'NONE',  ( 17.96484262340118221, 66.18868534415483396, -7.964842623401177768 ) ) ;
#79012 = ORIENTED_EDGE ( 'NONE', *, *, #37290, .T. ) ;
#79011 = CARTESIAN_POINT ( 'NONE',  ( 19.84674366389459266, 8.300597817667451750, 2.638427012816836559 ) ) ;
#79013 = CARTESIAN_POINT ( 'NONE',  ( -0.2838433074297238012, 13.12729635533385597, 9.500000000000000000 ) ) ;
#79014 = CARTESIAN_POINT ( 'NONE',  ( 17.20831665107776587, 49.13393115100078745, -7.208316651077762316 ) ) ;
#79015 = ORIENTED_EDGE ( 'NONE', *, *, #9608, .T. ) ;
#79016 = ORIENTED_EDGE ( 'NONE', *, *, #35822, .T. ) ;
#79017 = CYLINDRICAL_SURFACE ( 'NONE', #85777, 15.00000000000000000 ) ;
#79018 = CARTESIAN_POINT ( 'NONE',  ( 6.204703633549690345, 2.845415501580634388, 14.16423886937410082 ) ) ;
#79019 = CARTESIAN_POINT ( 'NONE',  ( 3.591859063236761518, 64.95696800326376774, 11.09922568453594849 ) ) ;
#79020 = CARTESIAN_POINT ( 'NONE',  ( 13.79529636645031943, 5.345415501580634832, -14.16423886937409904 ) ) ;
#79021 = CARTESIAN_POINT ( 'NONE',  ( 22.26659068614894466, 33.88708216824730357, 7.082119434687054849 ) ) ;
#79022 = DIRECTION ( 'NONE',  ( -0.000000000000000000, -1.000000000000000000, -0.000000000000000000 ) ) ;
#79023 = CARTESIAN_POINT ( 'NONE',  ( 12.91533473730993009, 16.60535201082150891, -10.88017736071109987 ) ) ;
#79024 = ORIENTED_EDGE ( 'NONE', *, *, #1773, .T. ) ;
#79025 = CARTESIAN_POINT ( 'NONE',  ( 2.791683348922240793, 11.63393115100078568, 7.208316651077764092 ) ) ;
#79026 = AXIS2_PLACEMENT_3D ( 'NONE', #61955, #17947, #84961 ) ;
#79027 = CARTESIAN_POINT ( 'NONE',  ( 10.00000000000000178, 17.25893115100078745, 9.846743663894594434 ) ) ;
#79028 = CARTESIAN_POINT ( 'NONE',  ( 13.43411237798105340, 40.58196800326375353, 12.81628187352647963 ) ) ;
#79029 = CARTESIAN_POINT ( 'NONE',  ( 0.1532563361054083140, 41.00893115100078745, 1.131784320476157264E-15 ) ) ;
#79030 = CARTESIAN_POINT ( 'NONE',  ( 0.2751277870542893633, 25.30223176428832232, 6.499999999999988454 ) ) ;
#79031 = CARTESIAN_POINT ( 'NONE',  ( -1.099225684535947600, 28.70696800326375353, -6.408140936763238038 ) ) ;
#79032 = CARTESIAN_POINT ( 'NONE',  ( 10.36894250292378850, -35.07125116508602503, -10.36894250292379027 ) ) ;
#79033 = CARTESIAN_POINT ( 'NONE',  ( 7.361572987183170547, 22.05059781766745530, 9.846743663894590881 ) ) ;
#79034 = CARTESIAN_POINT ( 'NONE',  ( 22.26659068614894466, 13.88708216824730179, 7.082119434687054849 ) ) ;
#79035 = EDGE_CURVE ( 'NONE', #39649, #12953, #12932, .T. ) ;
#79036 = B_SPLINE_CURVE_WITH_KNOTS ( 'NONE', 3,
 ( #69356, #68379, #45363, #877, #60857, #14893 ),
 .UNSPECIFIED., .F., .F.,
 ( 4, 2, 4 ),
 ( 0.0002800154274912493714, 0.0006862208078174524429, 0.001092426188143655677 ),
 .UNSPECIFIED. ) ;
#79037 = CARTESIAN_POINT ( 'NONE',  ( -0.8801773607111008646, 33.27201867748817676, 2.915334737309923430 ) ) ;
#79038 = CARTESIAN_POINT ( 'NONE',  ( 22.26659068614895176, 29.72041550158063572, -7.082119434687042414 ) ) ;
#79039 = CARTESIAN_POINT ( 'NONE',  ( 7.361572987183170547, 52.05059781766745175, 9.846743663894590881 ) ) ;
#79040 = CARTESIAN_POINT ( 'NONE',  ( 2.791683348922237240, 10.38393115100078390, -7.208316651077763204 ) ) ;
#79042 = CARTESIAN_POINT ( 'NONE',  ( 11.22915323889580463, 15.00000000000000000, -8.773176023390609757 ) ) ;
#79041 = CARTESIAN_POINT ( 'NONE',  ( 0.6178305044545838731, 59.74863466993041783, 9.382169495545420901 ) ) ;
#79043 = CARTESIAN_POINT ( 'NONE',  ( 7.084665262690076126, 29.10535201082150181, 10.88017736071109987 ) ) ;
#79044 = EDGE_CURVE ( 'NONE', #46560, #83062, #68587, .T. ) ;
#79045 = DIRECTION ( 'NONE',  ( 0.000000000000000000, 0.000000000000000000, 1.000000000000000000 ) ) ;
#79046 = CARTESIAN_POINT ( 'NONE',  ( 21.09922568453594849, 26.20696800326375353, 6.408140936763242479 ) ) ;
#79047 = CARTESIAN_POINT ( 'NONE',  ( 1.472469842513823179, 41.42559781766745886, 4.923371831947296329 ) ) ;
#79048 = CARTESIAN_POINT ( 'NONE',  ( 2.915334737309921209, 6.605352010821504471, -10.88017736071110164 ) ) ;
#79049 =( BOUNDED_CURVE ( )  B_SPLINE_CURVE ( 2, ( #96610, #78263, #71269, #20096, #55771, #35085, #24790, #73579, #5102 ),
 .UNSPECIFIED., .F., .F. ) 
 B_SPLINE_CURVE_WITH_KNOTS ( ( 3, 2, 2, 2, 3 ),
 ( 0.04728379408308854698, 0.04761904761904767192, 0.05357142857142860315, 0.05952380952380953438, 0.05985906305976865238 ),
 .UNSPECIFIED. ) 
 CURVE ( )  GEOMETRIC_REPRESENTATION_ITEM ( )  RATIONAL_B_SPLINE_CURVE ( ( 0.9963778908391762723, 0.9980808541467921513, 1.000000000000000000, 0.9659258262890682012, 1.000000000000000000, 0.9659258262890682012, 1.000000000000000000, 0.9980808541467921513, 0.9963778908391762723 ) ) 
 REPRESENTATION_ITEM ( '' )  );
#79050 = FACE_OUTER_BOUND ( 'NONE', #72001, .T. ) ;
#79052 = CARTESIAN_POINT ( 'NONE',  ( -10.95083791870221823, -94.44918831364067557, -4.000000000000000888 ) ) ;
#79051 = CARTESIAN_POINT ( 'NONE',  ( 13.99999999999999822, 11.00000000000000000, -6.500000000000000888 ) ) ;
#79053 = CARTESIAN_POINT ( 'NONE',  ( -11.33435148536054271, -69.53340079814059038, 4.000000000000000000 ) ) ;
#79054 = CYLINDRICAL_SURFACE ( 'NONE', #65544, 15.00000000000000000 ) ;
#79055 = CARTESIAN_POINT ( 'NONE',  ( 20.88017736071110519, 60.56368534415484106, 2.639326808657452039E-16 ) ) ;
#79056 = CARTESIAN_POINT ( 'NONE',  ( 15.44008868035555793, 56.39701867748817676, -9.422509992056140149 ) ) ;
#79057 = CARTESIAN_POINT ( 'NONE',  ( 8.209432707284900488, 14.63606883728627217, -12.55409154915488656 ) ) ;
#79058 = AXIS2_PLACEMENT_3D ( 'NONE', #67758, #274, #90239 ) ;
#79059 = CARTESIAN_POINT ( 'NONE',  ( 0.2751277870542910842, 52.28217586085238366, -6.499999999999992006 ) ) ;
#79060 = CARTESIAN_POINT ( 'NONE',  ( 7.084665262690076126, 12.02201867748817321, -10.88017736071110164 ) ) ;
#79061 = CARTESIAN_POINT ( 'NONE',  ( 12.63842701281683034, 62.46726448433410894, 9.846743663894596210 ) ) ;
#79063 = CARTESIAN_POINT ( 'NONE',  ( 18.18329248733321535, 37.60290668512019607, 6.500000000000005329 ) ) ;
#79062 = CARTESIAN_POINT ( 'NONE',  ( 2.035157376598824452, 18.68868534415484106, 7.964842623401179544 ) ) ;
#79064 = CARTESIAN_POINT ( 'NONE',  ( 11.10000000000000142, 98.49999999999998579, 8.000000000000000000 ) ) ;
#79065 = CARTESIAN_POINT ( 'NONE',  ( 21.09922568453594849, 31.20696800326375353, 6.408140936763242479 ) ) ;
#79066 = EDGE_LOOP ( 'NONE', ( #45284, #19680, #56944, #35334 ) ) ;
#79067 = CARTESIAN_POINT ( 'NONE',  ( 20.88017736071110519, 55.56368534415484817, 2.639326808657452039E-16 ) ) ;
#79068 = CARTESIAN_POINT ( 'NONE',  ( 12.63842701281683922, 34.55059781766745886, -9.846743663894590881 ) ) ;
#79070 = PRESENTATION_STYLE_ASSIGNMENT (( #34047 ) ) ;
#79069 = CARTESIAN_POINT ( 'NONE',  ( -1.099225684535947600, 19.54030133659708568, 6.408140936763237150 ) ) ;
#79071 = CARTESIAN_POINT ( 'NONE',  ( -0.8801773607110991993, 27.85535201082150181, -2.915334737309923874 ) ) ;
#79072 = CARTESIAN_POINT ( 'NONE',  ( 0.5774900079438590739, 42.64701867748816966, -5.440088680355550821 ) ) ;
#79073 = CARTESIAN_POINT ( 'NONE',  ( -4.164238869374099927, 52.01208216824729647, 3.795296366450308767 ) ) ;
#79074 = CARTESIAN_POINT ( 'NONE',  ( 2.791683348922240793, 41.63393115100078745, 7.208316651077764092 ) ) ;
#79075 = CARTESIAN_POINT ( 'NONE',  ( 15.44008868035555260, 54.73035201082150536, 9.422509992056143702 ) ) ;
#79076 = CARTESIAN_POINT ( 'NONE',  ( 10.00000000000000178, 49.31368534415484106, 10.88017736071110342 ) ) ;
#79077 = CARTESIAN_POINT ( 'NONE',  ( 13.07734668325342575, 15.00000000000000888, -6.551438809692913701 ) ) ;
#79078 = CARTESIAN_POINT ( 'NONE',  ( 13.79529636645031943, 15.34541550158063750, -14.16423886937409904 ) ) ;
#79079 = CIRCLE ( 'NONE', #32751, 1.750000000000000666 ) ;
#79080 = EDGE_CURVE ( 'NONE', #16145, #71011, #83384, .T. ) ;
#79081 = CARTESIAN_POINT ( 'NONE',  ( 10.83696084481538691, -98.17058944465519232, -3.750000000000000000 ) ) ;
#79082 = CARTESIAN_POINT ( 'NONE',  ( 2.791683348922240793, 66.63393115100079456, 7.208316651077764092 ) ) ;
#79083 = ORIENTED_EDGE ( 'NONE', *, *, #42578, .T. ) ;
#79084 = VERTEX_POINT ( 'NONE', #46079 ) ;
#79085 = CARTESIAN_POINT ( 'NONE',  ( 22.26659068614895176, 44.72041550158063927, -7.082119434687042414 ) ) ;
#79086 = CARTESIAN_POINT ( 'NONE',  ( -4.164238869374098151, 31.59541550158063927, -3.795296366450310543 ) ) ;
#79087 = CARTESIAN_POINT ( 'NONE',  ( 2.791683348922240793, 21.63393115100078745, 7.208316651077764092 ) ) ;
#79089 = CARTESIAN_POINT ( 'NONE',  ( 21.09922568453595559, 12.04030133659708746, -6.408140936763230044 ) ) ;
#79088 = AXIS2_PLACEMENT_3D ( 'NONE', #1251, #91735, #7758 ) ;
#79090 = DIRECTION ( 'NONE',  ( -0.000000000000000000, -0.000000000000000000, -1.000000000000000000 ) ) ;
#79091 = DIRECTION ( 'NONE',  ( 0.000000000000000000, 1.000000000000000000, 0.000000000000000000 ) ) ;
#79093 = CARTESIAN_POINT ( 'NONE',  ( 19.38216949554541202, 30.99863466993042138, 9.382169495545424454 ) ) ;
#79092 = CARTESIAN_POINT ( 'NONE',  ( 12.91533473730992121, 4.522018677488169658, 10.88017736071110164 ) ) ;
#79094 = CARTESIAN_POINT ( 'NONE',  ( 20.36894250292379382, 43.67874883491397497, 10.36894250292379205 ) ) ;
#79095 = CARTESIAN_POINT ( 'NONE',  ( -4.850097797903872632, 14.95037102666378281, -13.93319274794287921 ) ) ;
#79096 = CARTESIAN_POINT ( 'NONE',  ( 5.076628168052704559, 0.1755978176674514724, -8.527530157486179263 ) ) ;
#79097 = EDGE_CURVE ( 'NONE', #54543, #43815, #83239, .T. ) ;
#79098 = CARTESIAN_POINT ( 'NONE',  ( -8.527530157486182816, -14.40773551566587685, -4.923371831947288335 ) ) ;
#79099 = CARTESIAN_POINT ( 'NONE',  ( 2.791683348922240793, 6.633931151000785675, 7.208316651077764092 ) ) ;
#79100 = ORIENTED_EDGE ( 'NONE', *, *, #2450, .F. ) ;
#79101 =( NAMED_UNIT ( * ) PLANE_ANGLE_UNIT ( ) SI_UNIT ( $, .RADIAN. ) );
#79102 = CARTESIAN_POINT ( 'NONE',  ( 12.63842701281683034, 17.46726448433411250, 9.846743663894596210 ) ) ;
#79103 = FILL_AREA_STYLE ('',( #24642 ) ) ;
#79104 = VERTEX_POINT ( 'NONE', #52098 ) ;
#79105 = CARTESIAN_POINT ( 'NONE',  ( 13.79529636645030344, 8.262082168247300018, 14.16423886937410614 ) ) ;
#79107 = CARTESIAN_POINT ( 'NONE',  ( 0.5774900079438607392, 13.48035201082150358, 5.440088680355550821 ) ) ;
#79106 = CARTESIAN_POINT ( 'NONE',  ( 2.035157376598822676, 2.438685344154838397, -7.964842623401177768 ) ) ;
#79109 = CARTESIAN_POINT ( 'NONE',  ( 16.40814093676323893, 5.790301336597087456, 11.09922568453595026 ) ) ;
#79108 = CARTESIAN_POINT ( 'NONE',  ( 14.92337183194729988, 34.34226448433411605, -8.527530157486177487 ) ) ;
#79110 = DIRECTION ( 'NONE',  ( 0.9981347984218662539, 0.000000000000000000, 0.06104853953487057033 ) ) ;
#79111 = CARTESIAN_POINT ( 'NONE',  ( -9.399392868737892925, 15.00000000000000000, 11.04089732309468097 ) ) ;
#79113 = CARTESIAN_POINT ( 'NONE',  ( -1.099225684535947600, 13.70696800326375353, -6.408140936763238038 ) ) ;
#79112 = CIRCLE ( 'NONE', #36001, 15.00000000000000000 ) ;
#79114 = CARTESIAN_POINT ( 'NONE',  ( -12.81628187352647963, 28.91530133659709989, -3.434112377981046293 ) ) ;
#79115 = ORIENTED_EDGE ( 'NONE', *, *, #48984, .T. ) ;
#79116 = CARTESIAN_POINT ( 'NONE',  ( 10.00000000000000178, 43.05374883491397497, 14.16423886937410082 ) ) ;
#79117 = ORIENTED_EDGE ( 'NONE', *, *, #94809, .F. ) ;
#79118 = CARTESIAN_POINT ( 'NONE',  ( 17.08211943468705840, 55.13708216824731068, -12.26659068614894466 ) ) ;
#79119 = ORIENTED_EDGE ( 'NONE', *, *, #78213, .F. ) ;
#79120 = CARTESIAN_POINT ( 'NONE',  ( 15.44008868035555793, 31.39701867748817676, -9.422509992056140149 ) ) ;
#79121 = CARTESIAN_POINT ( 'NONE',  ( 0.5774900079438607392, 38.48035201082150536, 5.440088680355550821 ) ) ;
#79122 = CARTESIAN_POINT ( 'NONE',  ( 15.44008868035555260, 59.73035201082151247, 9.422509992056143702 ) ) ;
#79123 = CARTESIAN_POINT ( 'NONE',  ( 12.91533473730993009, 31.60535201082150891, -10.88017736071109987 ) ) ;
#79124 = EDGE_CURVE ( 'NONE', #8560, #765, #59452, .T. ) ;
#79125 = CARTESIAN_POINT ( 'NONE',  ( 0.1089645850228809637, 33.16234555792569694, 6.479102184480781013 ) ) ;
#79126 = AXIS2_PLACEMENT_3D ( 'NONE', #26166, #69703, #16212 ) ;
#79127 = CARTESIAN_POINT ( 'NONE',  ( 5.076628168052703671, 21.84226448433411960, 8.527530157486179263 ) ) ;
#79128 = CARTESIAN_POINT ( 'NONE',  ( -4.259797194937135600, -13.81744876718661885, 2.500000000000001776 ) ) ;
#79129 = ORIENTED_EDGE ( 'NONE', *, *, #84120, .F. ) ;
#79130 = CARTESIAN_POINT ( 'NONE',  ( 11.18123354744523468, -92.99280210685034831, 3.750000000000000000 ) ) ;
#79131 = CARTESIAN_POINT ( 'NONE',  ( 17.20831665107776587, 47.88393115100078745, 7.208316651077764980 ) ) ;
#79132 = ADVANCED_FACE ( 'NONE', ( #74594 ), #2380, .T. ) ;
#79133 = DIRECTION ( 'NONE',  ( -1.049065152435176504E-16, 1.000000000000000000, 0.000000000000000000 ) ) ;
#79134 = CARTESIAN_POINT ( 'NONE',  ( 16.40814093676324603, 47.45696800326375353, -11.09922568453594671 ) ) ;
#79135 = CARTESIAN_POINT ( 'NONE',  ( -6.757332319902496387, -55.97232334539076959, 3.750000000000000444 ) ) ;
#79136 = ORIENTED_EDGE ( 'NONE', *, *, #89747, .F. ) ;
#79137 = CARTESIAN_POINT ( 'NONE',  ( 17.39651004071842166, 22.93575266056828355, 6.499999999999998224 ) ) ;
#79138 = CARTESIAN_POINT ( 'NONE',  ( 15.00000000000000178, 73.00000000000000000, 6.250000000000000000 ) ) ;
#79139 = DIRECTION ( 'NONE',  ( 0.000000000000000000, 1.000000000000000000, 0.000000000000000000 ) ) ;
#79140 = CARTESIAN_POINT ( 'NONE',  ( 24.16423886937410614, 44.51208216824730357, -3.795296366450302550 ) ) ;
#79141 = DIRECTION ( 'NONE',  ( 0.000000000000000000, 1.000000000000000000, 0.000000000000000000 ) ) ;
#79142 = VERTEX_POINT ( 'NONE', #11534 ) ;
#79143 = CARTESIAN_POINT ( 'NONE',  ( 19.84674366389459621, 28.50893115100078745, 7.409399052514197653E-17 ) ) ;
#79144 = CARTESIAN_POINT ( 'NONE',  ( 3.591859063236761518, 59.95696800326375353, 11.09922568453594849 ) ) ;
#79145 = TOROIDAL_SURFACE ( 'NONE', #64784, 14.49999999999999822, 0.5000000000000000000 ) ;
#79146 = CARTESIAN_POINT ( 'NONE',  ( 19.84674366389459266, 58.30059781766745886, 2.638427012816836559 ) ) ;
#79147 = CARTESIAN_POINT ( 'NONE',  ( 19.84674366389459621, 3.508931151000785231, 7.409399052514197653E-17 ) ) ;
#79148 = LINE ( 'NONE', #87133, #96835 ) ;
#79149 = CARTESIAN_POINT ( 'NONE',  ( 14.92337183194729633, 62.67559781766745886, 8.527530157486181039 ) ) ;
#79150 = VECTOR ( 'NONE', #61858, 1000.000000000000000 ) ;
#79151 = VERTEX_POINT ( 'NONE', #3562 ) ;
#79152 = CARTESIAN_POINT ( 'NONE',  ( 2.917880565312948704, 67.63708216824730357, 12.26659068614894643 ) ) ;
#79153 = PLANE ( 'NONE',  #74481 ) ;
#79154 = CARTESIAN_POINT ( 'NONE',  ( 2.035157376598822676, 47.43868534415484817, -7.964842623401177768 ) ) ;
#79156 = CARTESIAN_POINT ( 'NONE',  ( -0.8801773607110991993, 67.85535201082151957, -2.915334737309923874 ) ) ;
#79155 = CARTESIAN_POINT ( 'NONE',  ( 6.565887622018943937, 15.16530133659708568, 12.81628187352647430 ) ) ;
#79157 = CARTESIAN_POINT ( 'NONE',  ( -0.3289641300568009741, 62.24545670184114243, -5.963430220938281678 ) ) ;
#79158 = ADVANCED_FACE ( 'NONE', ( #42054 ), #95534, .T. ) ;
#79159 = CARTESIAN_POINT ( 'NONE',  ( -14.97687855664613465, 14.49999999999999112, -0.8325315005902816923 ) ) ;
#79160 = DIRECTION ( 'NONE',  ( -0.06104853953487057033, -0.000000000000000000, 0.9981347984218662539 ) ) ;
#79161 = CARTESIAN_POINT ( 'NONE',  ( 12.63842701281683034, 57.46726448433411605, 9.846743663894596210 ) ) ;
#79162 = CARTESIAN_POINT ( 'NONE',  ( -22.44000000000001194, 93.50000000000000000, 9.500000000000000000 ) ) ;
#79163 = CARTESIAN_POINT ( 'NONE',  ( 12.26659068614894821, 28.88708216824731423, 7.082119434687044190 ) ) ;
#79164 = CARTESIAN_POINT ( 'NONE',  ( -1.099225684535947600, 13.70696800326375353, -6.408140936763238038 ) ) ;
#79166 = CARTESIAN_POINT ( 'NONE',  ( -8.000000000000000000, 80.99999999999994316, 1.249999999999987121 ) ) ;
#79165 = CARTESIAN_POINT ( 'NONE',  ( 20.88017736071110519, 20.56368534415484106, 2.639326808657452039E-16 ) ) ;
#79167 = CARTESIAN_POINT ( 'NONE',  ( 9.879999999999990123, 20.99999999999999645, 0.000000000000000000 ) ) ;
#79168 = CARTESIAN_POINT ( 'NONE',  ( -0.3689425029237898834, 31.17874883491396787, -10.36894250292378850 ) ) ;
#79169 = CARTESIAN_POINT ( 'NONE',  ( -4.164238869374099927, 27.01208216824730357, 3.795296366450308767 ) ) ;
#79170 = CARTESIAN_POINT ( 'NONE',  ( 13.79529636645030344, 63.26208216824730357, 14.16423886937410614 ) ) ;
#79171 = CARTESIAN_POINT ( 'NONE',  ( 14.92337183194729988, 49.34226448433411605, -8.527530157486177487 ) ) ;
#79172 = CARTESIAN_POINT ( 'NONE',  ( 19.38216949554541202, 30.99863466993042138, 9.382169495545424454 ) ) ;
#79173 = CARTESIAN_POINT ( 'NONE',  ( 7.084665262690076126, 14.10535201082150358, 10.88017736071109987 ) ) ;
#79174 = CIRCLE ( 'NONE', #36071, 14.49999999999999822 ) ;
#79175 = ORIENTED_EDGE ( 'NONE', *, *, #75848, .F. ) ;
#79176 = CARTESIAN_POINT ( 'NONE',  ( 12.63842701281683034, 37.46726448433411605, 9.846743663894596210 ) ) ;
#79177 = B_SPLINE_CURVE_WITH_KNOTS ( 'NONE', 3,
 ( #63081, #2126, #32586, #24616, #77101, #78093 ),
 .UNSPECIFIED., .F., .F.,
 ( 4, 2, 4 ),
 ( 0.000000000000000000, 0.0002701661927229306740, 0.0005403323854458613480 ),
 .UNSPECIFIED. ) ;
#79178 = CARTESIAN_POINT ( 'NONE',  ( 12.91533473730992121, 44.52201867748816966, 10.88017736071110164 ) ) ;
#79179 = CARTESIAN_POINT ( 'NONE',  ( 19.38216949554541557, 12.24863466993041961, -9.382169495545420901 ) ) ;
#79181 = CARTESIAN_POINT ( 'NONE',  ( 1.472469842513823179, 61.42559781766745175, 4.923371831947296329 ) ) ;
#79180 = CARTESIAN_POINT ( 'NONE',  ( -4.164238869374099039, 16.80374883491396787, 8.674139862899312516E-16 ) ) ;
#79182 = CARTESIAN_POINT ( 'NONE',  ( 5.419894505350487002, 0.5000000000000004441, 13.98659156302462314 ) ) ;
#79183 = PRESENTATION_LAYER_ASSIGNMENT (  '', '', ( #85624 ) ) ;
#79184 = CARTESIAN_POINT ( 'NONE',  ( 0.1532563361054082862, 21.21726448433412315, 2.638427012816831674 ) ) ;
#79185 = CARTESIAN_POINT ( 'NONE',  ( 6.565887622018943937, 55.16530133659709634, 12.81628187352647430 ) ) ;
#79186 = CARTESIAN_POINT ( 'NONE',  ( 7.361572987183169658, 59.96726448433410894, -9.846743663894592657 ) ) ;
#79187 = VERTEX_POINT ( 'NONE', #50028 ) ;
#79188 = DIRECTION ( 'NONE',  ( 0.9426414910921782075, 0.000000000000000000, -0.3338068592337712914 ) ) ;
#79189 =( LENGTH_UNIT ( ) NAMED_UNIT ( * ) SI_UNIT ( .MILLI., .METRE. ) );
#79190 = CARTESIAN_POINT ( 'NONE',  ( 10.00000000000000000, 65.55374883491396076, -14.16423886937410082 ) ) ;
#79191 = B_SPLINE_CURVE_WITH_KNOTS ( 'NONE', 3,
 ( #68577, #92059, #8564, #6585 ),
 .UNSPECIFIED., .F., .F.,
 ( 4, 4 ),
 ( 0.000000000000000000, 0.0003153491572467357934 ),
 .UNSPECIFIED. ) ;
#79192 = CARTESIAN_POINT ( 'NONE',  ( -0.3689425029237898834, 11.17874883491396787, -10.36894250292378850 ) ) ;
#79193 = CARTESIAN_POINT ( 'NONE',  ( -0.8801773607111009756, 68.06368534415484817, 1.068504757029289695E-15 ) ) ;
#79194 = CARTESIAN_POINT ( 'NONE',  ( 5.076628168052703671, 51.84226448433412315, 8.527530157486179263 ) ) ;
#79195 = CARTESIAN_POINT ( 'NONE',  ( 12.91533473730993009, 26.60535201082150536, -10.88017736071109987 ) ) ;
#79196 = DIRECTION ( 'NONE',  ( 0.000000000000000000, 1.000000000000000000, 0.000000000000000000 ) ) ;
#79197 = DIRECTION ( 'NONE',  ( 0.000000000000000000, 0.000000000000000000, 1.000000000000000000 ) ) ;
#79198 = ADVANCED_FACE ( 'NONE', ( #36006 ), #41567, .F. ) ;
#79199 = VERTEX_POINT ( 'NONE', #89014 ) ;
#79200 = DIRECTION ( 'NONE',  ( 0.9636304532086191754, 0.000000000000000000, 0.2672383760782702788 ) ) ;
#79201 = ORIENTED_EDGE ( 'NONE', *, *, #89523, .F. ) ;
#79202 = ORIENTED_EDGE ( 'NONE', *, *, #53096, .F. ) ;
#79203 = CARTESIAN_POINT ( 'NONE',  ( 13.40508947812163143, 3.998652394537887614E-16, 5.527528931046191474 ) ) ;
#79204 = CARTESIAN_POINT ( 'NONE',  ( 6.204703633549690345, 2.845415501580634388, 14.16423886937410082 ) ) ;
#79205 = FACE_OUTER_BOUND ( 'NONE', #41713, .T. ) ;
#79206 = CARTESIAN_POINT ( 'NONE',  ( 10.00000000000000178, 38.05374883491396787, 14.16423886937410082 ) ) ;
#79207 = CARTESIAN_POINT ( 'NONE',  ( 19.84674366389459266, 53.71726448433411605, -2.638427012816827677 ) ) ;
#79208 = CARTESIAN_POINT ( 'NONE',  ( 12.63842701281683922, 34.55059781766745886, -9.846743663894590881 ) ) ;
#79210 = CARTESIAN_POINT ( 'NONE',  ( 0.1532563361054100626, 55.80059781766745175, -2.638427012816831230 ) ) ;
#79209 = CARTESIAN_POINT ( 'NONE',  ( 7.084665262690076126, 19.10535201082150181, 10.88017736071109987 ) ) ;
#79211 = CARTESIAN_POINT ( 'NONE',  ( -0.3689425029237898834, 1.178748834913967869, -10.36894250292378850 ) ) ;
#79212 = CARTESIAN_POINT ( 'NONE',  ( 6.204703633549690345, 42.84541550158063217, 14.16423886937410082 ) ) ;
#79213 = CARTESIAN_POINT ( 'NONE',  ( 0.5774900079438607392, 8.480352010821505360, 5.440088680355550821 ) ) ;
#79214 = DIRECTION ( 'NONE',  ( -0.9981347984218665870, 0.000000000000000000, -0.06104853953486361756 ) ) ;
#79215 = DIRECTION ( 'NONE',  ( -0.000000000000000000, -0.000000000000000000, 1.000000000000000000 ) ) ;
#79216 = CARTESIAN_POINT ( 'NONE',  ( 7.084665262690076126, 59.10535201082150536, 10.88017736071109987 ) ) ;
#79217 = CARTESIAN_POINT ( 'NONE',  ( 18.52753015748617571, 28.09226448433411960, 4.923371831947298993 ) ) ;
#79218 = CARTESIAN_POINT ( 'NONE',  ( 13.48255862861920562, 15.00000000000000000, 5.335786055104250636 ) ) ;
#79219 = ORIENTED_EDGE ( 'NONE', *, *, #64077, .T. ) ;
#79220 = B_SPLINE_CURVE_WITH_KNOTS ( 'NONE', 3,
 ( #56396, #78393, #26865, #78889, #18392, #32394 ),
 .UNSPECIFIED., .F., .F.,
 ( 4, 2, 4 ),
 ( 0.0002800421825936724816, 0.0006862478247299561669, 0.001092453466866239852 ),
 .UNSPECIFIED. ) ;
#79221 = DIRECTION ( 'NONE',  ( 0.8949343616020292158, 0.000000000000000000, -0.4461978131098006672 ) ) ;
#79222 = ORIENTED_EDGE ( 'NONE', *, *, #33355, .F. ) ;
#79223 = CARTESIAN_POINT ( 'NONE',  ( 12.63842701281683922, 19.55059781766745175, -9.846743663894590881 ) ) ;
#79224 = VERTEX_POINT ( 'NONE', #87041 ) ;
#79225 = CARTESIAN_POINT ( 'NONE',  ( -2.266590686148945544, 26.38708216824730357, -7.082119434687050408 ) ) ;
#79227 = CARTESIAN_POINT ( 'NONE',  ( 1.472469842513823179, 36.42559781766745175, 4.923371831947296329 ) ) ;
#79226 = CIRCLE ( 'NONE', #61647, 1.500000000000001332 ) ;
#79228 = CARTESIAN_POINT ( 'NONE',  ( 17.96484262340118221, 49.93868534415484106, 7.964842623401181321 ) ) ;
#79229 = CARTESIAN_POINT ( 'NONE',  ( 0.000000000000000000, 0.000000000000000000, -6.500000000000000888 ) ) ;
#79230 = CARTESIAN_POINT ( 'NONE',  ( 19.42250999205614548, 35.98035201082151247, -5.440088680355545492 ) ) ;
#79231 = CARTESIAN_POINT ( 'NONE',  ( 14.93875075227008864, 0.2301502577613178946, 0.2365588874160677868 ) ) ;
#79232 = CARTESIAN_POINT ( 'NONE',  ( 3.434112377981060948, -9.418031996736241140, 12.81628187352647430 ) ) ;
#79233 = EDGE_LOOP ( 'NONE', ( #49929, #15309, #47032, #11839 ) ) ;
#79234 = CARTESIAN_POINT ( 'NONE',  ( 20.88017736071110164, 45.35535201082149115, 2.915334737309930979 ) ) ;
#79235 = CARTESIAN_POINT ( 'NONE',  ( -4.164238869374099927, 2.012082168247300906, 3.795296366450308767 ) ) ;
#79236 = ORIENTED_EDGE ( 'NONE', *, *, #36474, .T. ) ;
#79237 = ORIENTED_EDGE ( 'NONE', *, *, #10500, .F. ) ;
#79238 = CARTESIAN_POINT ( 'NONE',  ( 3.591859063236763294, 33.29030133659708213, -11.09922568453595026 ) ) ;
#79239 = FILL_AREA_STYLE_COLOUR ( '', #36618 ) ;
#79240 = CARTESIAN_POINT ( 'NONE',  ( 12.63842701281683922, 29.55059781766745175, -9.846743663894590881 ) ) ;
#79241 = CARTESIAN_POINT ( 'NONE',  ( 0.5774900079438590739, 2.647018677488170990, -5.440088680355550821 ) ) ;
#79242 = CARTESIAN_POINT ( 'NONE',  ( 22.81628187352648496, 46.83196800326376064, -3.434112377981050290 ) ) ;
#79243 = CARTESIAN_POINT ( 'NONE',  ( 0.000000000000000000, 15.00000000000000000, 0.000000000000000000 ) ) ;
#79244 = CARTESIAN_POINT ( 'NONE',  ( 19.84674366389459266, 23.30059781766745530, 2.638427012816836559 ) ) ;
#79245 = AXIS2_PLACEMENT_3D ( 'NONE', #76706, #67744, #84230 ) ;
#79247 = VECTOR ( 'NONE', #49220, 999.9999999999998863 ) ;
#79246 = CARTESIAN_POINT ( 'NONE',  ( 20.88017736071110519, 60.56368534415484106, 2.639326808657452039E-16 ) ) ;
#79248 = EDGE_CURVE ( 'NONE', #83600, #92022, #65470, .T. ) ;
#79249 = DIRECTION ( 'NONE',  ( 0.000000000000000000, 1.000000000000000000, 0.000000000000000000 ) ) ;
#79250 = CARTESIAN_POINT ( 'NONE',  ( 4.494156999534633989, 0.000000000000000000, -3.088748530746214360 ) ) ;
#79251 = EDGE_CURVE ( 'NONE', #25266, #62023, #50519, .T. ) ;
#79252 = COLOUR_RGB ( '', 0.08235294, 0.09019608, 0.10196078) ;
#79253 = CARTESIAN_POINT ( 'NONE',  ( 0.1077916266722445948, 17.24062864464239198, -6.478736007405951902 ) ) ;
#79254 = CARTESIAN_POINT ( 'NONE',  ( 2.791683348922237240, 5.383931151000785675, -7.208316651077763204 ) ) ;
#79255 = EDGE_CURVE ( 'NONE', #23745, #15318, #35006, .T. ) ;
#79256 = CARTESIAN_POINT ( 'NONE',  ( 0.6178305044545838731, 9.748634669930416052, 9.382169495545420901 ) ) ;
#79257 = CARTESIAN_POINT ( 'NONE',  ( 2.603489959281614308, 41.58210964143329846, 6.500000000000031086 ) ) ;
#79258 = CARTESIAN_POINT ( 'NONE',  ( 0.1532563361054082862, 46.21726448433411605, 2.638427012816831674 ) ) ;
#79259 = DIRECTION ( 'NONE',  ( -0.000000000000000000, -1.000000000000000000, -0.000000000000000000 ) ) ;
#79260 = CARTESIAN_POINT ( 'NONE',  ( -2.266590686148945544, 6.387082168247300906, -7.082119434687050408 ) ) ;
#79261 = CARTESIAN_POINT ( 'NONE',  ( 12.63842701281683034, 32.46726448433412315, 9.846743663894596210 ) ) ;
#79262 = CARTESIAN_POINT ( 'NONE',  ( 22.81628187352647785, 26.62363466993042138, 6.195893100308588602E-16 ) ) ;
#79264 = DIRECTION ( 'NONE',  ( 0.000000000000000000, 0.000000000000000000, -1.000000000000000000 ) ) ;
#79263 = CARTESIAN_POINT ( 'NONE',  ( 14.82269085861170943, 0.3639308522293639436, 2.299529454047053445 ) ) ;
#79265 = CARTESIAN_POINT ( 'NONE',  ( 12.91533473730992121, 44.52201867748816966, 10.88017736071110164 ) ) ;
#79266 = CARTESIAN_POINT ( 'NONE',  ( 6.565887622018943937, 13.08196800326374998, -12.81628187352647608 ) ) ;
#79267 = CARTESIAN_POINT ( 'NONE',  ( 2.603489959281588995, 40.43575266056827644, -6.500000000000003553 ) ) ;
#79268 = CARTESIAN_POINT ( 'NONE',  ( 19.84674366389459621, 18.50893115100078745, 7.409399052514197653E-17 ) ) ;
#79269 = CARTESIAN_POINT ( 'NONE',  ( 17.96484262340118221, 21.18868534415483396, -7.964842623401177768 ) ) ;
#79270 = CARTESIAN_POINT ( 'NONE',  ( 3.591859063236763294, 28.29030133659708568, -11.09922568453595026 ) ) ;
#79271 = VECTOR ( 'NONE', #29429, 1000.000000000000114 ) ;
#79272 = CARTESIAN_POINT ( 'NONE',  ( 7.361572987183170547, 27.05059781766745175, 9.846743663894590881 ) ) ;
#79273 =( GEOMETRIC_REPRESENTATION_CONTEXT ( 3 ) GLOBAL_UNCERTAINTY_ASSIGNED_CONTEXT ( ( #81162 ) ) GLOBAL_UNIT_ASSIGNED_CONTEXT ( ( #4389, #12847, #28351 ) ) REPRESENTATION_CONTEXT ( 'NONE', 'WORKASPACE' ) );
#79274 = CARTESIAN_POINT ( 'NONE',  ( -10.06059601896260247, 88.97539449291203084, 5.490105317800513696 ) ) ;
#79275 = AXIS2_PLACEMENT_3D ( 'NONE', #87627, #94644, #33147 ) ;
#79276 = CARTESIAN_POINT ( 'NONE',  ( 7.084665262690076126, 39.10535201082150536, 10.88017736071109987 ) ) ;
#79277 = CARTESIAN_POINT ( 'NONE',  ( 20.88017736071110519, 65.56368534415483396, 2.639326808657452039E-16 ) ) ;
#79278 = FILL_AREA_STYLE_COLOUR ( '', #63248 ) ;
#79280 = CARTESIAN_POINT ( 'NONE',  ( 20.88017736071110164, 30.35535201082151247, 2.915334737309930979 ) ) ;
#79279 = CARTESIAN_POINT ( 'NONE',  ( 7.361572987183170547, 37.05059781766744464, 9.846743663894590881 ) ) ;
#79281 = SURFACE_SIDE_STYLE ('',( #48775 ) ) ;
#79282 = EDGE_CURVE ( 'NONE', #74987, #25279, #61939, .T. ) ;
#79283 = CARTESIAN_POINT ( 'NONE',  ( 7.084665262690076126, 42.02201867748816966, -10.88017736071110164 ) ) ;
#79285 = SURFACE_STYLE_USAGE ( .BOTH. , #85810 ) ;
#79284 = CARTESIAN_POINT ( 'NONE',  ( 0.5774900079438590739, 12.64701867748817321, -5.440088680355550821 ) ) ;
#79286 = CARTESIAN_POINT ( 'NONE',  ( -1.899999999999997247, 98.49999999999998579, 8.000000000000000000 ) ) ;
#79287 = CARTESIAN_POINT ( 'NONE',  ( 7.361572987183169658, 34.96726448433411605, -9.846743663894592657 ) ) ;
#79289 = CARTESIAN_POINT ( 'NONE',  ( 2.603489959281590771, 46.58210964143328425, 6.500000000000003553 ) ) ;
#79288 = CARTESIAN_POINT ( 'NONE',  ( -0.3689425029237898834, 46.17874883491397497, -10.36894250292378850 ) ) ;
#79290 = CIRCLE ( 'NONE', #96872, 2.000000000000000888 ) ;
#79291 = CARTESIAN_POINT ( 'NONE',  ( 1.932340009482151011, 6.491275129254484355, -6.500000000000002665 ) ) ;
#79292 = DIRECTION ( 'NONE',  ( 0.000000000000000000, 1.000000000000000000, 0.000000000000000000 ) ) ;
#79293 = CARTESIAN_POINT ( 'NONE',  ( -4.164238869374099927, 27.01208216824730357, 3.795296366450308767 ) ) ;
#79294 = COLOUR_RGB ( '', 0.31764706, 0.68627451, 0.89019608) ;
#79295 = CARTESIAN_POINT ( 'NONE',  ( -5.810051007611032325, -36.09132727650185757, 2.750000000000000000 ) ) ;
#79296 = ORIENTED_EDGE ( 'NONE', *, *, #21596, .T. ) ;
#79297 = CARTESIAN_POINT ( 'NONE',  ( 20.36894250292379382, 63.67874883491396787, 10.36894250292379205 ) ) ;
#79298 = CARTESIAN_POINT ( 'NONE',  ( 0.1532563361054100626, 35.80059781766745175, -2.638427012816831230 ) ) ;
#79300 = CARTESIAN_POINT ( 'NONE',  ( -8.224651678658434051, 85.81254401277075772, -3.937446577531860559 ) ) ;
#79299 = DIRECTION ( 'NONE',  ( 0.000000000000000000, 0.000000000000000000, 1.000000000000000000 ) ) ;
#79301 = CARTESIAN_POINT ( 'NONE',  ( 12.91533473730993009, 61.60535201082150536, -10.88017736071109987 ) ) ;
#79302 = CARTESIAN_POINT ( 'NONE',  ( 21.09922568453595559, 62.04030133659709634, -6.408140936763230044 ) ) ;
#79303 = CIRCLE ( 'NONE', #58594, 2.000000000000001776 ) ;
#79304 = CARTESIAN_POINT ( 'NONE',  ( 10.00000000000000000, 31.81368534415483751, -10.88017736071110342 ) ) ;
#79305 = CARTESIAN_POINT ( 'NONE',  ( 19.38216949554541557, 62.24863466993041072, -9.382169495545420901 ) ) ;
#79306 = CARTESIAN_POINT ( 'NONE',  ( 13.43411237798106583, 12.66530133659708746, -12.81628187352647252 ) ) ;
#79307 = CARTESIAN_POINT ( 'NONE',  ( 18.52753015748617571, 18.09226448433411960, 4.923371831947298993 ) ) ;
#79308 = EDGE_LOOP ( 'NONE', ( #52758, #39513, #58446, #92161 ) ) ;
#79309 = DIRECTION ( 'NONE',  ( 0.000000000000000000, 0.000000000000000000, 1.000000000000000000 ) ) ;
#79310 = DIRECTION ( 'NONE',  ( 0.000000000000000000, 1.000000000000000000, 0.000000000000000000 ) ) ;
#79311 = CARTESIAN_POINT ( 'NONE',  ( 7.084665262690076126, 7.022018677488170546, -10.88017736071110164 ) ) ;
#79312 = CARTESIAN_POINT ( 'NONE',  ( 2.917880565312950480, 25.97041550158063572, -12.26659068614894821 ) ) ;
#79313 = CARTESIAN_POINT ( 'NONE',  ( -0.8801773607110991993, 37.85535201082151247, -2.915334737309923874 ) ) ;
#79314 = CARTESIAN_POINT ( 'NONE',  ( 2.035157376598824452, 48.68868534415483396, 7.964842623401179544 ) ) ;
#79315 = CARTESIAN_POINT ( 'NONE',  ( -7.640917710488839276, 0.04922511925147159823, -12.61992379908765649 ) ) ;
#79316 = CARTESIAN_POINT ( 'NONE',  ( 14.92337183194729988, 4.342264484334117824, -8.527530157486177487 ) ) ;
#79317 = CARTESIAN_POINT ( 'NONE',  ( -14.62617646268089899, 0.5000000000000004441, 3.327906561566782440 ) ) ;
#79318 = CARTESIAN_POINT ( 'NONE',  ( 19.84674366389459621, 23.50893115100078390, 7.409399052514197653E-17 ) ) ;
#79319 = CARTESIAN_POINT ( 'NONE',  ( 0.000000000000000000, 14.49999999999999822, 0.000000000000000000 ) ) ;
#79320 = CARTESIAN_POINT ( 'NONE',  ( 14.92337183194729988, 29.34226448433411960, -8.527530157486177487 ) ) ;
#79321 = CARTESIAN_POINT ( 'NONE',  ( 12.63842701281683034, 47.46726448433412315, 9.846743663894596210 ) ) ;
#79322 = CIRCLE ( 'NONE', #76106, 7.000000000000006217 ) ;
#79323 = CARTESIAN_POINT ( 'NONE',  ( 12.91533473730992121, 24.52201867748816966, 10.88017736071110164 ) ) ;
#79324 = UNCERTAINTY_MEASURE_WITH_UNIT (LENGTH_MEASURE( 1.000000000000000082E-05 ), #79597, 'distance_accuracy_value', 'NONE');
#79325 = CARTESIAN_POINT ( 'NONE',  ( -1.099225684535947600, 39.54030133659708923, 6.408140936763237150 ) ) ;
#79326 = CARTESIAN_POINT ( 'NONE',  ( 10.00000000000000178, 49.31368534415484106, 10.88017736071110342 ) ) ;
#79327 = CARTESIAN_POINT ( 'NONE',  ( 7.361572987183170547, 27.05059781766745175, 9.846743663894590881 ) ) ;
#79329 = CARTESIAN_POINT ( 'NONE',  ( 0.1532563361054082862, 16.21726448433411960, 2.638427012816831674 ) ) ;
#79328 = CARTESIAN_POINT ( 'NONE',  ( -4.164238869374099039, 41.80374883491397497, 8.674139862899312516E-16 ) ) ;
#79330 = CARTESIAN_POINT ( 'NONE',  ( 0.1916775849787265562, 47.25868815902069997, -6.499999999999990230 ) ) ;
#79331 = CIRCLE ( 'NONE', #76187, 15.00000000000000000 ) ;
#79332 = CYLINDRICAL_SURFACE ( 'NONE', #55038, 15.00000000000000000 ) ;
#79333 = CARTESIAN_POINT ( 'NONE',  ( -2.266590686148945544, 11.38708216824730179, -7.082119434687050408 ) ) ;
#79334 = CARTESIAN_POINT ( 'NONE',  ( 10.00000000000000000, 25.55374883491396787, -14.16423886937410082 ) ) ;
#79335 = CARTESIAN_POINT ( 'NONE',  ( 12.63842701281683922, 29.55059781766745175, -9.846743663894590881 ) ) ;
#79336 = CARTESIAN_POINT ( 'NONE',  ( 4.559911319644449179, 27.23035201082150536, -9.422509992056141925 ) ) ;
#79337 = CARTESIAN_POINT ( 'NONE',  ( 20.88017736071110164, 40.35535201082150536, 2.915334737309930979 ) ) ;
#79338 = CARTESIAN_POINT ( 'NONE',  ( 15.44008868035555260, 49.73035201082150536, 9.422509992056143702 ) ) ;
#79339 = ORIENTED_EDGE ( 'NONE', *, *, #29437, .T. ) ;
#79340 = STYLED_ITEM ( 'NONE', ( #34255 ), #32075 ) ;
#79341 = CARTESIAN_POINT ( 'NONE',  ( 4.559911319644449179, 53.89701867748817676, 9.422509992056141925 ) ) ;
#79342 = ORIENTED_EDGE ( 'NONE', *, *, #54750, .T. ) ;
#79343 = EDGE_CURVE ( 'NONE', #13314, #79733, #47607, .T. ) ;
#79344 = LINE ( 'NONE', #3350, #69710 ) ;
#79345 = AXIS2_PLACEMENT_3D ( 'NONE', #32916, #93921, #40441 ) ;
#79346 = CARTESIAN_POINT ( 'NONE',  ( 4.559911319644449179, 68.89701867748817676, 9.422509992056141925 ) ) ;
#79347 = ORIENTED_EDGE ( 'NONE', *, *, #14935, .F. ) ;
#79348 = AXIS2_PLACEMENT_3D ( 'NONE', #25124, #63577, #18585 ) ;
#79349 = CARTESIAN_POINT ( 'NONE',  ( 17.96484262340118221, 66.18868534415483396, -7.964842623401177768 ) ) ;
#79350 =( NAMED_UNIT ( * ) PLANE_ANGLE_UNIT ( ) SI_UNIT ( $, .RADIAN. ) );
#79351 = LINE ( 'NONE', #63353, #62731 ) ;
#79352 = DIRECTION ( 'NONE',  ( 0.000000000000000000, -1.000000000000000000, 0.000000000000000000 ) ) ;
#79353 = CARTESIAN_POINT ( 'NONE',  ( 2.035157376598822676, 12.43868534415483751, -7.964842623401177768 ) ) ;
#79354 = CARTESIAN_POINT ( 'NONE',  ( 1.472469842513823179, 16.42559781766745175, 4.923371831947296329 ) ) ;
#79355 = CARTESIAN_POINT ( 'NONE',  ( 17.08211943468705840, 5.137082168247300906, -12.26659068614894466 ) ) ;
#79356 = CARTESIAN_POINT ( 'NONE',  ( 2.791683348922240793, 6.633931151000785675, 7.208316651077764092 ) ) ;
#79357 = CARTESIAN_POINT ( 'NONE',  ( 20.88017736071110875, 5.772018677488170546, -2.915334737309920765 ) ) ;
#79358 = CARTESIAN_POINT ( 'NONE',  ( 14.92337183194729988, 49.34226448433411605, -8.527530157486177487 ) ) ;
#79359 = EDGE_LOOP ( 'NONE', ( #90732, #36819, #52986, #6054, #34840 ) ) ;
#79360 = CARTESIAN_POINT ( 'NONE',  ( 19.84674366389459266, 43.71726448433410894, -2.638427012816827677 ) ) ;
#79361 = ORIENTED_EDGE ( 'NONE', *, *, #492, .F. ) ;
#79362 = CARTESIAN_POINT ( 'NONE',  ( 4.559911319644449179, 52.23035201082151247, -9.422509992056141925 ) ) ;
#79363 = CARTESIAN_POINT ( 'NONE',  ( 17.20831665107776587, 49.13393115100078745, -7.208316651077762316 ) ) ;
#79364 = CARTESIAN_POINT ( 'NONE',  ( 0.6178305044545818747, 28.49863466993041783, -9.382169495545419124 ) ) ;
#79366 = DIRECTION ( 'NONE',  ( 0.000000000000000000, 1.000000000000000000, 0.000000000000000000 ) ) ;
#79365 = CARTESIAN_POINT ( 'NONE',  ( 2.562013731377108972, 0.5000000000000000000, -6.499999999999999112 ) ) ;
#79367 = CARTESIAN_POINT ( 'NONE',  ( 19.42250999205614193, 65.14701867748817676, 5.440088680355555262 ) ) ;
#79368 = CARTESIAN_POINT ( 'NONE',  ( 17.96484262340118221, 11.18868534415484106, -7.964842623401177768 ) ) ;
#79369 = AXIS2_PLACEMENT_3D ( 'NONE', #9954, #19416, #71922 ) ;
#79370 = EDGE_CURVE ( 'NONE', #52255, #72967, #70286, .T. ) ;
#79371 = CARTESIAN_POINT ( 'NONE',  ( 16.40814093676323893, 35.79030133659708923, 11.09922568453595026 ) ) ;
#79372 = CARTESIAN_POINT ( 'NONE',  ( 0.000000000000000000, 15.00000000000000000, 0.000000000000000000 ) ) ;
#79373 = ORIENTED_EDGE ( 'NONE', *, *, #1622, .F. ) ;
#79374 = CARTESIAN_POINT ( 'NONE',  ( 0.6178305044545838731, 24.74863466993042493, 9.382169495545420901 ) ) ;
#79375 = CARTESIAN_POINT ( 'NONE',  ( 4.559911319644449179, 38.89701867748817676, 9.422509992056141925 ) ) ;
#79376 = EDGE_CURVE ( 'NONE', #73812, #22448, #14137, .T. ) ;
#79377 = MECHANICAL_DESIGN_GEOMETRIC_PRESENTATION_REPRESENTATION (  '', ( #65001 ), #57023 ) ;
#79378 = ORIENTED_EDGE ( 'NONE', *, *, #28407, .F. ) ;
#79379 = CARTESIAN_POINT ( 'NONE',  ( 6.565887622018943937, -1.918031996736246692, -12.81628187352647608 ) ) ;
#79381 = CARTESIAN_POINT ( 'NONE',  ( 10.00000000000000178, 57.25893115100078745, 9.846743663894594434 ) ) ;
#79380 = CARTESIAN_POINT ( 'NONE',  ( 5.076628168052703671, 16.84226448433411960, 8.527530157486179263 ) ) ;
#79382 = CARTESIAN_POINT ( 'NONE',  ( -8.000000000000000000, 1.019547802438458550, 3.750000000000000000 ) ) ;
#79383 = CARTESIAN_POINT ( 'NONE',  ( 18.52753015748618282, 38.92559781766745175, -4.923371831947291888 ) ) ;
#79384 = CARTESIAN_POINT ( 'NONE',  ( 14.35840480524199947, 0.5000000000000004441, -4.340070442838851683 ) ) ;
#79385 = CARTESIAN_POINT ( 'NONE',  ( -13.07964015051215156, 14.76930270348881180, -7.222261988160926016 ) ) ;
#79387 = DIRECTION ( 'NONE',  ( 0.000000000000000000, 0.000000000000000000, 1.000000000000000000 ) ) ;
#79386 = CARTESIAN_POINT ( 'NONE',  ( 18.52753015748618282, 33.92559781766745886, -4.923371831947291888 ) ) ;
#79388 = DIRECTION ( 'NONE',  ( 0.000000000000000000, 0.000000000000000000, 1.000000000000000000 ) ) ;
#79390 = ORIENTED_EDGE ( 'NONE', *, *, #84787, .T. ) ;
#79389 = CARTESIAN_POINT ( 'NONE',  ( 0.1532563361054082862, 61.21726448433412315, 2.638427012816831674 ) ) ;
#79391 = VECTOR ( 'NONE', #21779, 1000.000000000000000 ) ;
#79392 = DIRECTION ( 'NONE',  ( 0.000000000000000000, 0.000000000000000000, -1.000000000000000000 ) ) ;
#79393 = CARTESIAN_POINT ( 'NONE',  ( -2.816281873526471635, 23.91530133659708568, -3.434112377981056508 ) ) ;
#79394 = CARTESIAN_POINT ( 'NONE',  ( 0.1532563361054083140, 51.00893115100078745, 1.131784320476157264E-15 ) ) ;
#79395 = ADVANCED_FACE ( 'NONE', ( #28510 ), #30466, .F. ) ;
#79396 = CARTESIAN_POINT ( 'NONE',  ( -13.75543905097471153, 14.95037102630581316, 5.333404663735480611 ) ) ;
#79397 = STYLED_ITEM ( 'NONE', ( #62042 ), #89831 ) ;
#79398 = CARTESIAN_POINT ( 'NONE',  ( 10.00000000000000178, 43.05374883491397497, 14.16423886937410082 ) ) ;
#79399 = CARTESIAN_POINT ( 'NONE',  ( 14.92337183194729988, 19.34226448433411960, -8.527530157486177487 ) ) ;
#79400 = ORIENTED_EDGE ( 'NONE', *, *, #13576, .F. ) ;
#79401 = CARTESIAN_POINT ( 'NONE',  ( 20.00000000000000711, 82.60888403408161196, 4.637569774571720593 ) ) ;
#79402 = CARTESIAN_POINT ( 'NONE',  ( 13.79529636645031943, 60.34541550158063927, -14.16423886937409904 ) ) ;
#79403 = CARTESIAN_POINT ( 'NONE',  ( 18.52753015748617571, 63.09226448433412315, 4.923371831947298993 ) ) ;
#79404 = EDGE_CURVE ( 'NONE', #23594, #91180, #54468, .T. ) ;
#79405 = EDGE_CURVE ( 'NONE', #2722, #21313, #52974, .T. ) ;
#79406 = CARTESIAN_POINT ( 'NONE',  ( 20.88017736071110875, 10.77201867748817143, -2.915334737309920765 ) ) ;
#79408 = AXIS2_PLACEMENT_3D ( 'NONE', #61540, #77044, #17543 ) ;
#79407 = CARTESIAN_POINT ( 'NONE',  ( 10.00000000000000000, 40.55374883491397497, -14.16423886937410082 ) ) ;
#79410 = CARTESIAN_POINT ( 'NONE',  ( 56.78206182523731371, 28.99999999999999645, 0.000000000000000000 ) ) ;
#79409 = CARTESIAN_POINT ( 'NONE',  ( 10.00000000000000178, 38.05374883491396787, 14.16423886937410082 ) ) ;
#79411 = CARTESIAN_POINT ( 'NONE',  ( 2.962741594152983993, -0.03417435944610275333, 13.93860331045674883 ) ) ;
#79413 = CARTESIAN_POINT ( 'NONE',  ( 10.00000000000000000, 59.75893115100078745, -9.846743663894594434 ) ) ;
#79412 = CARTESIAN_POINT ( 'NONE',  ( 6.685134130355901760, -80.57704203043711289, 2.500000000000000888 ) ) ;
#79414 = AXIS2_PLACEMENT_3D ( 'NONE', #63500, #65454, #41514 ) ;
#79415 = ORIENTED_EDGE ( 'NONE', *, *, #44484, .T. ) ;
#79416 = CARTESIAN_POINT ( 'NONE',  ( 4.559911319644449179, 42.23035201082151247, -9.422509992056141925 ) ) ;
#79417 = CARTESIAN_POINT ( 'NONE',  ( 10.70613742633256926, 15.00000000000000000, -9.778988772285213571 ) ) ;
#79418 = CARTESIAN_POINT ( 'NONE',  ( 11.20713776170701870, -56.83174664233160911, 3.750000000000000444 ) ) ;
#79420 = CARTESIAN_POINT ( 'NONE',  ( -46.82017113615791004, 100.6079546444643569, -9.324761308090124601 ) ) ;
#79419 = CIRCLE ( 'NONE', #55519, 0.2499999999999997224 ) ;
#79421 = CARTESIAN_POINT ( 'NONE',  ( -3.795296366450322534, 0.7620821682473031267, -14.16423886937409904 ) ) ;
#79422 = VECTOR ( 'NONE', #16007, 1000.000000000000000 ) ;
#79423 = CARTESIAN_POINT ( 'NONE',  ( 10.00000000000000178, 62.25893115100078745, 9.846743663894594434 ) ) ;
#79424 = CARTESIAN_POINT ( 'NONE',  ( -15.67879934938584263, 15.00000000000000000, 3.170591017105712339 ) ) ;
#79425 = VERTEX_POINT ( 'NONE', #14012 ) ;
#79426 = CARTESIAN_POINT ( 'NONE',  ( 17.08211943468705130, 33.47041550158063927, 12.26659068614894998 ) ) ;
#79427 = CARTESIAN_POINT ( 'NONE',  ( 14.35840480524199947, 15.00000000000000000, -4.340070442838851683 ) ) ;
#79428 =( NAMED_UNIT ( * ) SI_UNIT ( $, .STERADIAN. ) SOLID_ANGLE_UNIT ( ) );
#79429 = CARTESIAN_POINT ( 'NONE',  ( 20.88017736071110875, 15.77201867748817143, -2.915334737309920765 ) ) ;
#79430 = CARTESIAN_POINT ( 'NONE',  ( 13.43411237798106583, 27.66530133659708568, -12.81628187352647252 ) ) ;
#79431 = CARTESIAN_POINT ( 'NONE',  ( -0.1503990784575328643, 40.12777174578613426, 6.262539305110068177 ) ) ;
#79432 = CARTESIAN_POINT ( 'NONE',  ( 18.52753015748617571, 18.09226448433411960, 4.923371831947298993 ) ) ;
#79433 = CARTESIAN_POINT ( 'NONE',  ( 4.920853330076631060, -13.83152733636334020, -4.000000000001609379 ) ) ;
#79434 = DIRECTION ( 'NONE',  ( -0.000000000000000000, -1.000000000000000000, -0.000000000000000000 ) ) ;
#79435 = CARTESIAN_POINT ( 'NONE',  ( 20.88017736071110164, 10.35535201082150714, 2.915334737309930979 ) ) ;
#79436 = CARTESIAN_POINT ( 'NONE',  ( 14.99999999999998046, 70.25000000000000000, 6.500000000000000888 ) ) ;
#79437 = CARTESIAN_POINT ( 'NONE',  ( -0.8801773607111009756, 38.06368534415484106, 1.068504757029289695E-15 ) ) ;
#79438 = CARTESIAN_POINT ( 'NONE',  ( 15.44008868035555793, 36.39701867748816966, -9.422509992056140149 ) ) ;
#79439 = CARTESIAN_POINT ( 'NONE',  ( 6.565887622018943937, 0.1653013365970866511, 12.81628187352647430 ) ) ;
#79440 = DIRECTION ( 'NONE',  ( -0.000000000000000000, -1.000000000000000000, -0.000000000000000000 ) ) ;
#79441 = CARTESIAN_POINT ( 'NONE',  ( 17.39651004071841101, 57.93575266056827644, 6.500000000000005329 ) ) ;
#79442 = CARTESIAN_POINT ( 'NONE',  ( 7.361572987183170547, 7.050597817667451750, 9.846743663894590881 ) ) ;
#79443 = ORIENTED_EDGE ( 'NONE', *, *, #27348, .T. ) ;
#79444 = CARTESIAN_POINT ( 'NONE',  ( 15.44008868035555260, 29.73035201082150891, 9.422509992056143702 ) ) ;
#79445 = CARTESIAN_POINT ( 'NONE',  ( 16.40814093676323893, 10.79030133659708923, 11.09922568453595026 ) ) ;
#79446 = CARTESIAN_POINT ( 'NONE',  ( 7.084665262690076126, 69.10535201082151957, 10.88017736071109987 ) ) ;
#79447 = CARTESIAN_POINT ( 'NONE',  ( 0.1532563361054082862, 6.217264484334118713, 2.638427012816831674 ) ) ;
#79448 = VECTOR ( 'NONE', #80858, 1000.000000000000000 ) ;
#79449 = CARTESIAN_POINT ( 'NONE',  ( 19.38216949554541202, 30.99863466993042138, 9.382169495545424454 ) ) ;
#79450 = CARTESIAN_POINT ( 'NONE',  ( 0.1532563361054083140, 6.008931151000784787, 1.131784320476157264E-15 ) ) ;
#79451 = EDGE_LOOP ( 'NONE', ( #90336, #22673, #12280, #52673 ) ) ;
#79452 = SURFACE_SIDE_STYLE ('',( #48944 ) ) ;
#79453 = FILL_AREA_STYLE ('',( #9480 ) ) ;
#79454 = CARTESIAN_POINT ( 'NONE',  ( 7.084665262690076126, 9.105352010821503583, 10.88017736071109987 ) ) ;
#79456 = CARTESIAN_POINT ( 'NONE',  ( -0.3689425029237881626, 27.42874883491397142, 10.36894250292379027 ) ) ;
#79455 = CARTESIAN_POINT ( 'NONE',  ( 22.81628187352648496, 61.83196800326376774, -3.434112377981050290 ) ) ;
#79457 = CARTESIAN_POINT ( 'NONE',  ( 1.472469842513823179, 16.42559781766745175, 4.923371831947296329 ) ) ;
#79458 = CARTESIAN_POINT ( 'NONE',  ( 19.42250999205614193, 5.147018677488171434, 5.440088680355555262 ) ) ;
#79459 = CIRCLE ( 'NONE', #48874, 0.2500000000000002220 ) ;
#79460 = CARTESIAN_POINT ( 'NONE',  ( 2.791683348922240793, 26.63393115100078745, 7.208316651077764092 ) ) ;
#79461 = CARTESIAN_POINT ( 'NONE',  ( 20.36894250292379738, 64.92874883491397497, -10.36894250292379027 ) ) ;
#79462 = ORIENTED_EDGE ( 'NONE', *, *, #46641, .T. ) ;
#79463 = CARTESIAN_POINT ( 'NONE',  ( 20.88017736071110519, 10.56368534415483751, 2.639326808657452039E-16 ) ) ;
#79464 = ADVANCED_FACE ( 'NONE', ( #98522 ), #40139, .T. ) ;
#79465 = CARTESIAN_POINT ( 'NONE',  ( 7.084665262690076126, 17.02201867748817676, -10.88017736071110164 ) ) ;
#79466 = CARTESIAN_POINT ( 'NONE',  ( 2.603489959281586774, 5.435752660568278216, -6.500000000000001776 ) ) ;
#79467 = CIRCLE ( 'NONE', #26773, 15.00000000000000000 ) ;
#79468 = ORIENTED_EDGE ( 'NONE', *, *, #45855, .T. ) ;
#79469 = CARTESIAN_POINT ( 'NONE',  ( 12.87930560075669284, 0.04962897030442307150, 7.195887444332472072 ) ) ;
#79470 = CARTESIAN_POINT ( 'NONE',  ( 7.084665262690076126, 29.10535201082150181, 10.88017736071109987 ) ) ;
#79471 = CARTESIAN_POINT ( 'NONE',  ( 10.00000000000000000, 54.75893115100078745, -9.846743663894594434 ) ) ;
#79472 = CARTESIAN_POINT ( 'NONE',  ( 0.000000000000000000, 15.00000000000000000, 0.000000000000000000 ) ) ;
#79473 = CARTESIAN_POINT ( 'NONE',  ( -2.816281873526473856, 49.33196800326374643, 3.434112377981055619 ) ) ;
#79474 = CARTESIAN_POINT ( 'NONE',  ( -1.926860441876563801, 4.896642702460841434, 3.195792623639529761 ) ) ;
#79475 = CARTESIAN_POINT ( 'NONE',  ( 20.36894250292379738, 39.92874883491396787, -10.36894250292379027 ) ) ;
#79476 = CARTESIAN_POINT ( 'NONE',  ( 4.559911319644449179, 37.23035201082150536, -9.422509992056141925 ) ) ;
#79477 = CARTESIAN_POINT ( 'NONE',  ( -0.8801773607111009756, 13.06368534415483929, 1.068504757029289695E-15 ) ) ;
#79478 = CARTESIAN_POINT ( 'NONE',  ( 18.52753015748617571, 53.09226448433412315, 4.923371831947298993 ) ) ;
#79479 = CARTESIAN_POINT ( 'NONE',  ( 19.05866839779139710, 60.95508385108959715, -6.499999999999974243 ) ) ;
#79480 = CARTESIAN_POINT ( 'NONE',  ( 12.63842701281683034, 37.46726448433411605, 9.846743663894596210 ) ) ;
#79481 = CARTESIAN_POINT ( 'NONE',  ( 6.880000000000011440, 40.74999999999999289, -4.000000000000000000 ) ) ;
#79482 = CARTESIAN_POINT ( 'NONE',  ( 12.63842701281683922, 14.55059781766744997, -9.846743663894590881 ) ) ;
#79483 = CARTESIAN_POINT ( 'NONE',  ( -6.408140936763232709, -30.04303199673624292, 11.09922568453595026 ) ) ;
#79484 = CIRCLE ( 'NONE', #73094, 0.2500000000000002220 ) ;
#79485 = ORIENTED_EDGE ( 'NONE', *, *, #15942, .T. ) ;
#79486 = CARTESIAN_POINT ( 'NONE',  ( 7.084665262690076126, 19.10535201082150181, 10.88017736071109987 ) ) ;
#79487 = CARTESIAN_POINT ( 'NONE',  ( 0.1532563361054100626, 10.80059781766745175, -2.638427012816831230 ) ) ;
#79488 = CARTESIAN_POINT ( 'NONE',  ( 10.00000000000000000, 2.873634669930420049, -12.81628187352647608 ) ) ;
#79489 = CARTESIAN_POINT ( 'NONE',  ( 17.96484262340118221, 39.93868534415484106, 7.964842623401181321 ) ) ;
#79491 = CARTESIAN_POINT ( 'NONE',  ( 19.38216949554541557, 47.24863466993041783, -9.382169495545420901 ) ) ;
#79490 = CARTESIAN_POINT ( 'NONE',  ( 17.96484262340118221, 21.18868534415483396, -7.964842623401177768 ) ) ;
#79492 = CARTESIAN_POINT ( 'NONE',  ( 22.26659068614895176, 29.72041550158063572, -7.082119434687042414 ) ) ;
#79493 = DIRECTION ( 'NONE',  ( 0.000000000000000000, 0.000000000000000000, 1.000000000000000000 ) ) ;
#79494 = MECHANICAL_DESIGN_GEOMETRIC_PRESENTATION_REPRESENTATION (  '', ( #85918 ), #42804 ) ;
#79495 = ADVANCED_FACE ( 'NONE', ( #60480 ), #92797, .T. ) ;
#79496 = CARTESIAN_POINT ( 'NONE',  ( 0.6178305044545818747, 53.49863466993041072, -9.382169495545419124 ) ) ;
#79497 = ORIENTED_EDGE ( 'NONE', *, *, #32039, .F. ) ;
#79498 = CARTESIAN_POINT ( 'NONE',  ( 1.472469842513823179, 55.59226448433412315, -4.923371831947296329 ) ) ;
#79499 = CARTESIAN_POINT ( 'NONE',  ( 3.591859063236761518, 64.95696800326376774, 11.09922568453594849 ) ) ;
#79500 = EDGE_CURVE ( 'NONE', #50694, #11231, #43257, .T. ) ;
#79501 = CARTESIAN_POINT ( 'NONE',  ( 20.88017736071110164, 30.35535201082151247, 2.915334737309930979 ) ) ;
#79502 = ORIENTED_EDGE ( 'NONE', *, *, #30600, .T. ) ;
#79504 = CARTESIAN_POINT ( 'NONE',  ( -3.638307330400850415, -8.269691488429797843, 2.499999999999999556 ) ) ;
#79503 = CARTESIAN_POINT ( 'NONE',  ( 10.00000000000000178, 2.258931151000784787, 9.846743663894594434 ) ) ;
#79505 = CARTESIAN_POINT ( 'NONE',  ( 19.84674366389459266, 23.71726448433412315, -2.638427012816827677 ) ) ;
#79506 = CARTESIAN_POINT ( 'NONE',  ( 5.076628168052703671, 16.84226448433411960, 8.527530157486179263 ) ) ;
#79507 = CARTESIAN_POINT ( 'NONE',  ( 12.63842701281683034, 7.467264484334118713, 9.846743663894596210 ) ) ;
#79508 = CARTESIAN_POINT ( 'NONE',  ( -0.8801773607110991993, 62.85535201082150536, -2.915334737309923874 ) ) ;
#79509 = CARTESIAN_POINT ( 'NONE',  ( 19.42250999205614548, 65.98035201082151957, -5.440088680355545492 ) ) ;
#79511 = ORIENTED_EDGE ( 'NONE', *, *, #53761, .F. ) ;
#79510 = CARTESIAN_POINT ( 'NONE',  ( 7.361572987183169658, 24.96726448433412315, -9.846743663894592657 ) ) ;
#79512 = DIRECTION ( 'NONE',  ( 0.000000000000000000, 0.000000000000000000, 1.000000000000000000 ) ) ;
#79513 = CARTESIAN_POINT ( 'NONE',  ( 17.20831665107776587, 54.13393115100079456, -7.208316651077762316 ) ) ;
#79514 = ORIENTED_EDGE ( 'NONE', *, *, #8485, .F. ) ;
#79515 = ORIENTED_EDGE ( 'NONE', *, *, #57225, .F. ) ;
#79516 = DIRECTION ( 'NONE',  ( -0.4305110968082861977, 0.000000000000000000, -0.9025852843498647360 ) ) ;
#79517 = EDGE_CURVE ( 'NONE', #39559, #38526, #67998, .T. ) ;
#79518 = CARTESIAN_POINT ( 'NONE',  ( -2.266590686148945544, 11.38708216824730179, -7.082119434687050408 ) ) ;
#79519 = UNCERTAINTY_MEASURE_WITH_UNIT (LENGTH_MEASURE( 1.000000000000000082E-05 ), #29817, 'distance_accuracy_value', 'NONE');
#79520 = LINE ( 'NONE', #33992, #53547 ) ;
#79521 = CARTESIAN_POINT ( 'NONE',  ( 24.16423886937410614, 4.512082168247300906, -3.795296366450302550 ) ) ;
#79522 = CARTESIAN_POINT ( 'NONE',  ( 6.204703633549690345, 27.84541550158063217, 14.16423886937410082 ) ) ;
#79523 =( NAMED_UNIT ( * ) SI_UNIT ( $, .STERADIAN. ) SOLID_ANGLE_UNIT ( ) );
#79524 = FACE_OUTER_BOUND ( 'NONE', #85035, .T. ) ;
#79525 = CARTESIAN_POINT ( 'NONE',  ( 19.42250999205614548, 40.98035201082150536, -5.440088680355545492 ) ) ;
#79526 = FILL_AREA_STYLE_COLOUR ( '', #97849 ) ;
#79527 = VERTEX_POINT ( 'NONE', #37505 ) ;
#79528 = CARTESIAN_POINT ( 'NONE',  ( 12.63842701281683922, 19.55059781766745175, -9.846743663894590881 ) ) ;
#79530 = CARTESIAN_POINT ( 'NONE',  ( 14.92337183194729988, 9.342264484334119601, -8.527530157486177487 ) ) ;
#79529 = CARTESIAN_POINT ( 'NONE',  ( 20.88017736071110164, 60.35535201082151957, 2.915334737309930979 ) ) ;
#79531 = CARTESIAN_POINT ( 'NONE',  ( 3.591859063236763294, 43.29030133659708923, -11.09922568453595026 ) ) ;
#79532 = CARTESIAN_POINT ( 'NONE',  ( 10.00000000000000178, 32.25893115100078745, 9.846743663894594434 ) ) ;
#79533 = CARTESIAN_POINT ( 'NONE',  ( -0.1023957841222422477, 25.13377557478296964, 6.340343622311917393 ) ) ;
#79534 = CARTESIAN_POINT ( 'NONE',  ( 19.42250999205614193, 55.14701867748817676, 5.440088680355555262 ) ) ;
#79535 = CARTESIAN_POINT ( 'NONE',  ( -2.816281873526471635, 28.91530133659708213, -3.434112377981056508 ) ) ;
#79536 = CARTESIAN_POINT ( 'NONE',  ( -14.16423886937410437, -33.40458449841936783, -3.795296366450299885 ) ) ;
#79537 = AXIS2_PLACEMENT_3D ( 'NONE', #51930, #58424, #28911 ) ;
#79538 = CARTESIAN_POINT ( 'NONE',  ( 5.076628168052703671, 26.84226448433411960, 8.527530157486179263 ) ) ;
#79539 = CARTESIAN_POINT ( 'NONE',  ( -0.3689425029237881626, 12.42874883491396609, 10.36894250292379027 ) ) ;
#79540 = EDGE_LOOP ( 'NONE', ( #91425, #38055, #90839, #72207 ) ) ;
#79541 = CARTESIAN_POINT ( 'NONE',  ( 10.00000000000000178, 39.31368534415484106, 10.88017736071110342 ) ) ;
#79542 = CARTESIAN_POINT ( 'NONE',  ( 12.91533473730992121, 59.52201867748816966, 10.88017736071110164 ) ) ;
#79543 = CARTESIAN_POINT ( 'NONE',  ( 2.917880565312948704, 37.63708216824731068, 12.26659068614894643 ) ) ;
#79544 = CARTESIAN_POINT ( 'NONE',  ( 0.1532563361054100626, 55.80059781766745175, -2.638427012816831230 ) ) ;
#79545 = CARTESIAN_POINT ( 'NONE',  ( 1.472469842513823179, 11.42559781766745175, 4.923371831947296329 ) ) ;
#79547 = DIRECTION ( 'NONE',  ( 0.000000000000000000, 1.000000000000000000, 0.000000000000000000 ) ) ;
#79546 = CARTESIAN_POINT ( 'NONE',  ( 5.500000000000000000, 61.50000000000000711, 6.000000000000000000 ) ) ;
#79548 = CARTESIAN_POINT ( 'NONE',  ( 17.96484262340118221, 44.93868534415483396, 7.964842623401181321 ) ) ;
#79549 = CARTESIAN_POINT ( 'NONE',  ( 19.72487221294570858, 70.00000000000000000, 6.000000000000000000 ) ) ;
#79550 = VECTOR ( 'NONE', #17183, 1000.000000000000000 ) ;
#79551 = CARTESIAN_POINT ( 'NONE',  ( 22.81628187352647785, 16.41530133659708923, 3.434112377981063169 ) ) ;
#79552 = CARTESIAN_POINT ( 'NONE',  ( 16.40814093676323893, 15.79030133659708746, 11.09922568453595026 ) ) ;
#79553 = CARTESIAN_POINT ( 'NONE',  ( 18.52753015748618282, 53.92559781766745175, -4.923371831947291888 ) ) ;
#79554 = CARTESIAN_POINT ( 'NONE',  ( 7.964842623401177768, 11.18868534415484106, -7.964842623401181321 ) ) ;
#79556 = CARTESIAN_POINT ( 'NONE',  ( 18.17884179759833074, 33.66688879859532335, -6.499999999999955591 ) ) ;
#79555 = CARTESIAN_POINT ( 'NONE',  ( -0.8801773607110991993, 67.85535201082151957, -2.915334737309923874 ) ) ;
#79557 =( GEOMETRIC_REPRESENTATION_CONTEXT ( 3 ) GLOBAL_UNCERTAINTY_ASSIGNED_CONTEXT ( ( #9350 ) ) GLOBAL_UNIT_ASSIGNED_CONTEXT ( ( #41081, #55073, #7461 ) ) REPRESENTATION_CONTEXT ( 'NONE', 'WORKASPACE' ) );
#79558 = DIRECTION ( 'NONE',  ( -0.000000000000000000, -1.000000000000000000, -0.000000000000000000 ) ) ;
#79559 = CARTESIAN_POINT ( 'NONE',  ( 0.9940297508537879745, -0.03417435944610275333, -14.21528771620249820 ) ) ;
#79560 = VECTOR ( 'NONE', #17019, 1000.000000000000114 ) ;
#79561 = CARTESIAN_POINT ( 'NONE',  ( 4.559911319644449179, 63.89701867748817676, 9.422509992056141925 ) ) ;
#79562 = CARTESIAN_POINT ( 'NONE',  ( 7.084665262690076126, 57.02201867748817676, -10.88017736071110164 ) ) ;
#79563 = FACE_OUTER_BOUND ( 'NONE', #33494, .T. ) ;
#79564 = B_SPLINE_CURVE_WITH_KNOTS ( 'NONE', 3,
 ( #60440, #949, #75941, #16432, #61913, #14969 ),
 .UNSPECIFIED., .F., .F.,
 ( 4, 2, 4 ),
 ( 3.409110551496115783E-05, 0.0004400426677367857043, 0.0008459942299586101829 ),
 .UNSPECIFIED. ) ;
#79565 = CYLINDRICAL_SURFACE ( 'NONE', #12463, 15.00000000000000000 ) ;
#79566 = CARTESIAN_POINT ( 'NONE',  ( 10.00000000000000000, 24.75893115100078745, -9.846743663894594434 ) ) ;
#79567 = CARTESIAN_POINT ( 'NONE',  ( 4.559911319644449179, 18.89701867748817321, 9.422509992056141925 ) ) ;
#79568 = CARTESIAN_POINT ( 'NONE',  ( 10.00000000000000178, 67.25893115100079456, 9.846743663894594434 ) ) ;
#79570 = CARTESIAN_POINT ( 'NONE',  ( -7.079957117332396521, -69.52918679324339735, -3.750000000000000000 ) ) ;
#79569 = CARTESIAN_POINT ( 'NONE',  ( 10.00000000000000000, 41.81368534415484106, -10.88017736071110342 ) ) ;
#79571 = CARTESIAN_POINT ( 'NONE',  ( 21.09922568453595559, 42.04030133659708213, -6.408140936763230044 ) ) ;
#79572 = ORIENTED_EDGE ( 'NONE', *, *, #96999, .F. ) ;
#79573 = CARTESIAN_POINT ( 'NONE',  ( 15.44008868035555260, 44.73035201082151247, 9.422509992056143702 ) ) ;
#79574 = CARTESIAN_POINT ( 'NONE',  ( 22.81628187352648496, 21.83196800326374643, -3.434112377981050290 ) ) ;
#79575 = CARTESIAN_POINT ( 'NONE',  ( 4.559911319644449179, 28.89701867748817321, 9.422509992056141925 ) ) ;
#79576 = CARTESIAN_POINT ( 'NONE',  ( 6.204703633549690345, 55.76208216824730357, -14.16423886937410259 ) ) ;
#79577 = CARTESIAN_POINT ( 'NONE',  ( 0.1532563361054083140, 46.00893115100079456, 1.131784320476157264E-15 ) ) ;
#79578 = CARTESIAN_POINT ( 'NONE',  ( 12.63842701281683034, 7.467264484334118713, 9.846743663894596210 ) ) ;
#79579 = CARTESIAN_POINT ( 'NONE',  ( 12.91533473730993009, 46.60535201082150536, -10.88017736071109987 ) ) ;
#79580 = B_SPLINE_CURVE_WITH_KNOTS ( 'NONE', 3,
 ( #51716, #11736, #82200, #44193 ),
 .UNSPECIFIED., .F., .F.,
 ( 4, 4 ),
 ( 8.673617379884035472E-19, 0.001036303429213374615 ),
 .UNSPECIFIED. ) ;
#79581 = CARTESIAN_POINT ( 'NONE',  ( 13.34343830728404967, 14.63595249122789177, -6.852200678592606842 ) ) ;
#79582 = CARTESIAN_POINT ( 'NONE',  ( -0.3689425029237898834, 21.17874883491396432, -10.36894250292378850 ) ) ;
#79583 = B_SPLINE_CURVE_WITH_KNOTS ( 'NONE', 3,
 ( #8079, #38576, #85552, #31548 ),
 .UNSPECIFIED., .F., .F.,
 ( 4, 4 ),
 ( 0.000000000000000000, 0.001036303429213373964 ),
 .UNSPECIFIED. ) ;
#79584 = ADVANCED_FACE ( 'NONE', ( #52007 ), #32121, .T. ) ;
#79585 = CARTESIAN_POINT ( 'NONE',  ( 20.15039907845753220, 56.74884699246889141, 6.262539305110074395 ) ) ;
#79586 = DIRECTION ( 'NONE',  ( 0.000000000000000000, 0.000000000000000000, 1.000000000000000000 ) ) ;
#79587 = VERTEX_POINT ( 'NONE', #59495 ) ;
#79588 = CARTESIAN_POINT ( 'NONE',  ( -4.164238869374099927, 42.01208216824728936, 3.795296366450308767 ) ) ;
#79589 = CARTESIAN_POINT ( 'NONE',  ( -0.3689425029237898834, 46.17874883491397497, -10.36894250292378850 ) ) ;
#79590 = CARTESIAN_POINT ( 'NONE',  ( 19.84674366389459266, 18.71726448433411960, -2.638427012816827677 ) ) ;
#79591 = CARTESIAN_POINT ( 'NONE',  ( 13.43411237798106583, 17.66530133659708923, -12.81628187352647252 ) ) ;
#79592 = CYLINDRICAL_SURFACE ( 'NONE', #41151, 0.09999999999999939493 ) ;
#79593 = DIRECTION ( 'NONE',  ( 0.000000000000000000, -1.000000000000000000, 0.000000000000000000 ) ) ;
#79595 = CARTESIAN_POINT ( 'NONE',  ( 21.09922568453595559, 27.04030133659708568, -6.408140936763230044 ) ) ;
#79594 = CARTESIAN_POINT ( 'NONE',  ( 2.035157376598822676, 2.438685344154837953, -7.964842623401177768 ) ) ;
#79596 = CARTESIAN_POINT ( 'NONE',  ( -2.266590686148945544, 42.22041550158063217, 7.082119434687048631 ) ) ;
#79597 =( LENGTH_UNIT ( ) NAMED_UNIT ( * ) SI_UNIT ( .MILLI., .METRE. ) );
#79598 = CARTESIAN_POINT ( 'NONE',  ( 4.923371831947295441, -0.6577355156658776236, -8.527530157486179263 ) ) ;
#79599 = EDGE_LOOP ( 'NONE', ( #55636, #73967, #22807, #23787, #21269, #43082 ) ) ;
#79600 = DIRECTION ( 'NONE',  ( -0.4771587602596037980, 0.000000000000000000, -0.8788171126619679363 ) ) ;
#79601 = CARTESIAN_POINT ( 'NONE',  ( 19.84674366389459266, 18.30059781766745175, 2.638427012816836559 ) ) ;
#79602 = ORIENTED_EDGE ( 'NONE', *, *, #21940, .T. ) ;
#79604 = CARTESIAN_POINT ( 'NONE',  ( 20.88017736071110164, 15.35535201082150358, 2.915334737309930979 ) ) ;
#79603 = CARTESIAN_POINT ( 'NONE',  ( 15.44008868035555260, 4.730352010821505360, 9.422509992056143702 ) ) ;
#79606 = CARTESIAN_POINT ( 'NONE',  ( 3.591859063236763294, 8.290301336597087456, -11.09922568453595026 ) ) ;
#79605 = CARTESIAN_POINT ( 'NONE',  ( 19.84674366389459266, 48.30059781766745175, 2.638427012816836559 ) ) ;
#79607 = LINE ( 'NONE', #26592, #13570 ) ;
#79608 = CARTESIAN_POINT ( 'NONE',  ( -14.17193700899788134, 0.000000000000000000, -1.489530601564206247 ) ) ;
#79609 =( GEOMETRIC_REPRESENTATION_CONTEXT ( 3 ) GLOBAL_UNCERTAINTY_ASSIGNED_CONTEXT ( ( #9215 ) ) GLOBAL_UNIT_ASSIGNED_CONTEXT ( ( #31377, #23419, #31864 ) ) REPRESENTATION_CONTEXT ( 'NONE', 'WORKASPACE' ) );
#79610 = EDGE_CURVE ( 'NONE', #54489, #36938, #83488, .T. ) ;
#79611 = CARTESIAN_POINT ( 'NONE',  ( 22.81628187352647785, 16.41530133659708923, 3.434112377981063169 ) ) ;
#79612 = VERTEX_POINT ( 'NONE', #15007 ) ;
#79613 = CARTESIAN_POINT ( 'NONE',  ( 13.79529636645031943, 65.34541550158063217, -14.16423886937409904 ) ) ;
#79614 = ORIENTED_EDGE ( 'NONE', *, *, #93247, .F. ) ;
#79615 = CARTESIAN_POINT ( 'NONE',  ( 22.26659068614895176, 54.72041550158063217, -7.082119434687042414 ) ) ;
#79616 = ORIENTED_EDGE ( 'NONE', *, *, #5483, .F. ) ;
#79617 = CARTESIAN_POINT ( 'NONE',  ( 7.084665262690076126, 29.10535201082150181, 10.88017736071109987 ) ) ;
#79618 = CARTESIAN_POINT ( 'NONE',  ( 4.559911319644449179, 42.23035201082151247, -9.422509992056141925 ) ) ;
#79619 = VECTOR ( 'NONE', #63947, 1000.000000000000000 ) ;
#79620 = CARTESIAN_POINT ( 'NONE',  ( 0.5774900079438590739, 42.64701867748816966, -5.440088680355550821 ) ) ;
#79621 = CARTESIAN_POINT ( 'NONE',  ( 17.75000000000000355, 78.80384757729335377, -4.000000000000000000 ) ) ;
#79622 = CARTESIAN_POINT ( 'NONE',  ( 17.96484262340118221, 41.18868534415484106, -7.964842623401177768 ) ) ;
#79623 = CIRCLE ( 'NONE', #82825, 15.00000000000000000 ) ;
#79624 = CIRCLE ( 'NONE', #3001, 15.00000000000000000 ) ;
#79625 = LINE ( 'NONE', #11126, #15408 ) ;
#79626 = CARTESIAN_POINT ( 'NONE',  ( 7.361572987183170547, 12.05059781766744997, 9.846743663894590881 ) ) ;
#79627 = VERTEX_POINT ( 'NONE', #45477 ) ;
#79628 = CARTESIAN_POINT ( 'NONE',  ( 11.15633734011313294, -69.21829398629044761, 4.000000000000000000 ) ) ;
#79629 = CARTESIAN_POINT ( 'NONE',  ( 2.791683348922240793, 41.63393115100078745, 7.208316651077764092 ) ) ;
#79630 = CARTESIAN_POINT ( 'NONE',  ( 0.2751277870542967463, 0.000000000000000000, 6.500000000000000888 ) ) ;
#79631 = CARTESIAN_POINT ( 'NONE',  ( 22.81628187352648496, 51.83196800326376064, -3.434112377981050290 ) ) ;
#79632 = ADVANCED_FACE ( 'NONE', ( #75979 ), #7508, .T. ) ;
#79633 = CARTESIAN_POINT ( 'NONE',  ( 0.2751277870542868098, 57.28217586085237656, -6.499999999999985789 ) ) ;
#79634 = AXIS2_PLACEMENT_3D ( 'NONE', #14214, #67205, #51713 ) ;
#79635 = CARTESIAN_POINT ( 'NONE',  ( -45.04367043435856743, 105.4369522167675086, 5.288592931995918178 ) ) ;
#79636 = CARTESIAN_POINT ( 'NONE',  ( 1.472469842513823179, 65.59226448433412315, -4.923371831947296329 ) ) ;
#79637 = CARTESIAN_POINT ( 'NONE',  ( 13.79529636645031943, 60.34541550158063927, -14.16423886937409904 ) ) ;
#79638 = CARTESIAN_POINT ( 'NONE',  ( -0.1034006766821534140, 4.816303916663454299E-16, 14.49963131600461175 ) ) ;
#79639 = ORIENTED_EDGE ( 'NONE', *, *, #46291, .T. ) ;
#79640 = CARTESIAN_POINT ( 'NONE',  ( 70.00000000000000000, 0.4999999999999958922, -9.500000000000000000 ) ) ;
#79641 = CARTESIAN_POINT ( 'NONE',  ( 19.84674366389459266, 33.71726448433410894, -2.638427012816827677 ) ) ;
#79642 =( NAMED_UNIT ( * ) SI_UNIT ( $, .STERADIAN. ) SOLID_ANGLE_UNIT ( ) );
#79643 = CARTESIAN_POINT ( 'NONE',  ( 22.81628187352647785, 6.623634669930420493, 6.195893100308588602E-16 ) ) ;
#79645 = EDGE_CURVE ( 'NONE', #29027, #189, #68491, .T. ) ;
#79644 = CARTESIAN_POINT ( 'NONE',  ( -0.8801773607111008646, 68.27201867748817676, 2.915334737309923430 ) ) ;
#79646 = SURFACE_STYLE_FILL_AREA ( #27616 ) ;
#79647 = CARTESIAN_POINT ( 'NONE',  ( 18.52753015748618282, 8.925597817667451750, -4.923371831947291888 ) ) ;
#79648 = CARTESIAN_POINT ( 'NONE',  ( 7.361572987183169658, 64.96726448433412315, -9.846743663894592657 ) ) ;
#79649 = FACE_OUTER_BOUND ( 'NONE', #44077, .T. ) ;
#79650 = ORIENTED_EDGE ( 'NONE', *, *, #24624, .T. ) ;
#79651 = CARTESIAN_POINT ( 'NONE',  ( 0.5774900079438590739, 2.647018677488171434, -5.440088680355550821 ) ) ;
#79652 = DIRECTION ( 'NONE',  ( 0.09584575252022037306, 0.000000000000000000, 0.9953961983671790748 ) ) ;
#79653 = CARTESIAN_POINT ( 'NONE',  ( -0.8801773607111009756, 48.06368534415484817, 1.068504757029289695E-15 ) ) ;
#79655 = CARTESIAN_POINT ( 'NONE',  ( 9.128857603258678566, 12.89891393428310806, -7.267056389305773578 ) ) ;
#79654 = CARTESIAN_POINT ( 'NONE',  ( 3.591859063236761518, 14.95696800326375531, 11.09922568453594849 ) ) ;
#79656 = CARTESIAN_POINT ( 'NONE',  ( 10.00000000000000178, 4.313685344154837509, 10.88017736071110342 ) ) ;
#79658 = EDGE_CURVE ( 'NONE', #76576, #19224, #77346, .T. ) ;
#79657 = B_SPLINE_CURVE_WITH_KNOTS ( 'NONE', 3,
 ( #959, #54911, #10415, #61431 ),
 .UNSPECIFIED., .F., .F.,
 ( 4, 4 ),
 ( -4.898238651910869251E-06, 0.0003854743236894886405 ),
 .UNSPECIFIED. ) ;
#79659 = CARTESIAN_POINT ( 'NONE',  ( -11.62719953690051788, 0.5000000000000004441, -9.476720473301954328 ) ) ;
#79660 = CARTESIAN_POINT ( 'NONE',  ( 19.05914839598886346, 59.96693863883976405, 6.499999999999922728 ) ) ;
#79661 = CARTESIAN_POINT ( 'NONE',  ( 10.00000000000000178, 47.25893115100078745, 9.846743663894594434 ) ) ;
#79662 = CARTESIAN_POINT ( 'NONE',  ( 19.84674366389459266, 8.717264484334116048, -2.638427012816827677 ) ) ;
#79663 = CARTESIAN_POINT ( 'NONE',  ( 9.422509992056141925, -19.85298132251182324, 5.440088680355547268 ) ) ;
#79664 = CARTESIAN_POINT ( 'NONE',  ( -1.099225684535947600, 23.70696800326375708, -6.408140936763238038 ) ) ;
#79665 = DIRECTION ( 'NONE',  ( 0.000000000000000000, 0.000000000000000000, -1.000000000000000000 ) ) ;
#79666 = CARTESIAN_POINT ( 'NONE',  ( -0.8801773607111009756, 23.06368534415484106, 1.068504757029289695E-15 ) ) ;
#79667 = DIRECTION ( 'NONE',  ( -0.000000000000000000, -0.000000000000000000, -1.000000000000000000 ) ) ;
#79668 = CARTESIAN_POINT ( 'NONE',  ( 20.36894250292379382, 38.67874883491396076, 10.36894250292379205 ) ) ;
#79669 = CARTESIAN_POINT ( 'NONE',  ( 17.08211943468705840, 35.13708216824730357, -12.26659068614894466 ) ) ;
#79670 = CARTESIAN_POINT ( 'NONE',  ( 20.88017736071110875, 5.772018677488170546, -2.915334737309920765 ) ) ;
#79671 = CARTESIAN_POINT ( 'NONE',  ( 17.20831665107776587, 47.88393115100078745, 7.208316651077764980 ) ) ;
#79672 = CARTESIAN_POINT ( 'NONE',  ( 10.00000000000000000, 42.87363466993042493, -12.81628187352647608 ) ) ;
#79673 = CARTESIAN_POINT ( 'NONE',  ( 19.42250999205614548, 15.98035201082150714, -5.440088680355545492 ) ) ;
#79674 = CARTESIAN_POINT ( 'NONE',  ( 12.63842701281683922, 39.55059781766744464, -9.846743663894590881 ) ) ;
#79675 = CARTESIAN_POINT ( 'NONE',  ( 2.035157376598824452, 43.68868534415484106, 7.964842623401179544 ) ) ;
#79676 = CARTESIAN_POINT ( 'NONE',  ( 0.6178305044545838731, -0.2513653300695798953, 9.382169495545420901 ) ) ;
#79677 = CARTESIAN_POINT ( 'NONE',  ( 2.917880565312950480, 20.97041550158063217, -12.26659068614894821 ) ) ;
#79678 = CARTESIAN_POINT ( 'NONE',  ( 14.64921366071501119, 14.95037108083552368, 1.748670679918272741 ) ) ;
#79679 = CARTESIAN_POINT ( 'NONE',  ( 5.076628168052703671, 26.84226448433411960, 8.527530157486179263 ) ) ;
#79680 = CARTESIAN_POINT ( 'NONE',  ( 19.38216949554541202, 55.99863466993041072, 9.382169495545424454 ) ) ;
#79681 = CARTESIAN_POINT ( 'NONE',  ( 17.20831665107776587, 52.88393115100078035, 7.208316651077764980 ) ) ;
#79682 = ORIENTED_EDGE ( 'NONE', *, *, #13155, .F. ) ;
#79683 = CARTESIAN_POINT ( 'NONE',  ( 17.82151337995249207, 90.99999999999998579, -8.000000000000000000 ) ) ;
#79684 = CARTESIAN_POINT ( 'NONE',  ( 4.400664535130860422, -1.180071741297640253, 2.750000000000000000 ) ) ;
#79685 = CARTESIAN_POINT ( 'NONE',  ( 7.084665262690076126, 4.105352010821503583, 10.88017736071109987 ) ) ;
#79686 = CARTESIAN_POINT ( 'NONE',  ( 19.42250999205614548, 60.98035201082151247, -5.440088680355545492 ) ) ;
#79687 = CARTESIAN_POINT ( 'NONE',  ( 17.08211943468705840, 10.13708216824730179, -12.26659068614894466 ) ) ;
#79688 = CARTESIAN_POINT ( 'NONE',  ( 4.559911319644449179, 63.89701867748817676, 9.422509992056141925 ) ) ;
#79689 = CARTESIAN_POINT ( 'NONE',  ( 14.92337183194729988, 49.34226448433411605, -8.527530157486177487 ) ) ;
#79690 = CARTESIAN_POINT ( 'NONE',  ( 19.42250999205614193, 35.14701867748816966, 5.440088680355555262 ) ) ;
#79691 = CARTESIAN_POINT ( 'NONE',  ( 2.831191079880678085, 79.91181047996344944, -9.500000000000000000 ) ) ;
#79692 = CARTESIAN_POINT ( 'NONE',  ( 19.42250999205614193, 25.14701867748817321, 5.440088680355555262 ) ) ;
#79693 = MECHANICAL_DESIGN_GEOMETRIC_PRESENTATION_REPRESENTATION (  '', ( #14254 ), #41398 ) ;
#79694 = ADVANCED_FACE ( 'NONE', ( #24473 ), #69963, .T. ) ;
#79695 = VERTEX_POINT ( 'NONE', #31935 ) ;
#79696 = AXIS2_PLACEMENT_3D ( 'NONE', #52692, #21216, #51718 ) ;
#79697 = FILL_AREA_STYLE_COLOUR ( '', #70658 ) ;
#79698 = ORIENTED_EDGE ( 'NONE', *, *, #22584, .T. ) ;
#79699 = ORIENTED_EDGE ( 'NONE', *, *, #72813, .T. ) ;
#79700 = CARTESIAN_POINT ( 'NONE',  ( 17.08211943468705130, 8.470415501580635720, 12.26659068614894998 ) ) ;
#79701 = CARTESIAN_POINT ( 'NONE',  ( -2.266590686148945544, 12.22041550158063394, 7.082119434687048631 ) ) ;
#79702 = CARTESIAN_POINT ( 'NONE',  ( 22.26659068614895176, 54.72041550158063217, -7.082119434687042414 ) ) ;
#79703 = CARTESIAN_POINT ( 'NONE',  ( 10.00000000000000178, 52.25893115100078745, 9.846743663894594434 ) ) ;
#79704 = CARTESIAN_POINT ( 'NONE',  ( 18.52753015748618282, 38.92559781766745175, -4.923371831947291888 ) ) ;
#79705 = DIRECTION ( 'NONE',  ( -0.7009092642998475675, 0.000000000000000000, -0.7132504491541847846 ) ) ;
#79707 = CARTESIAN_POINT ( 'NONE',  ( 0.1532563361054100626, 65.80059781766745175, -2.638427012816831230 ) ) ;
#79706 = CARTESIAN_POINT ( 'NONE',  ( 10.00000000000000178, 34.31368534415484106, 10.88017736071110342 ) ) ;
#79708 = EDGE_CURVE ( 'NONE', #64082, #91314, #21407, .T. ) ;
#79709 = CARTESIAN_POINT ( 'NONE',  ( 10.00000000000000000, 65.55374883491396076, -14.16423886937410082 ) ) ;
#79710 = DIRECTION ( 'NONE',  ( 3.197442310920451468E-14, 0.000000000000000000, 1.000000000000000000 ) ) ;
#79711 = CARTESIAN_POINT ( 'NONE',  ( 0.7375392941518293943, 14.49999999999999822, -14.98185688723470932 ) ) ;
#79712 = CARTESIAN_POINT ( 'NONE',  ( 15.44008868035555793, 66.39701867748817676, -9.422509992056140149 ) ) ;
#79713 = CARTESIAN_POINT ( 'NONE',  ( 5.076628168052704559, 25.17559781766745175, -8.527530157486179263 ) ) ;
#79714 = CARTESIAN_POINT ( 'NONE',  ( -9.846743663894590881, -33.78273551566586974, 2.638427012816840111 ) ) ;
#79715 = ORIENTED_EDGE ( 'NONE', *, *, #81754, .F. ) ;
#79716 = FACE_OUTER_BOUND ( 'NONE', #59071, .T. ) ;
#79717 = VERTEX_POINT ( 'NONE', #76959 ) ;
#79718 = CARTESIAN_POINT ( 'NONE',  ( 5.076628168052703671, 21.84226448433411960, 8.527530157486179263 ) ) ;
#79719 = VERTEX_POINT ( 'NONE', #31449 ) ;
#79720 = CARTESIAN_POINT ( 'NONE',  ( 24.16423886937410614, 29.30374883491396787, 8.672049930838204340E-16 ) ) ;
#79721 = CARTESIAN_POINT ( 'NONE',  ( 0.1532563361054100626, 30.80059781766744820, -2.638427012816831230 ) ) ;
#79722 = CARTESIAN_POINT ( 'NONE',  ( -0.8801773607110991993, 57.85535201082149825, -2.915334737309923874 ) ) ;
#79723 = VECTOR ( 'NONE', #64705, 1000.000000000000000 ) ;
#79724 = CARTESIAN_POINT ( 'NONE',  ( 14.71525861348287734, 0.5000000000000004441, 2.908807992686682109 ) ) ;
#79725 = CARTESIAN_POINT ( 'NONE',  ( 15.44008868035555260, 39.73035201082150536, 9.422509992056143702 ) ) ;
#79726 = CARTESIAN_POINT ( 'NONE',  ( 12.63842701281683034, 47.46726448433412315, 9.846743663894596210 ) ) ;
#79727 = EDGE_CURVE ( 'NONE', #74593, #8279, #8956, .T. ) ;
#79728 = CARTESIAN_POINT ( 'NONE',  ( 11.09922568453595026, -8.793031996736241140, 6.408140936763232709 ) ) ;
#79729 = ORIENTED_EDGE ( 'NONE', *, *, #69638, .T. ) ;
#79730 = CARTESIAN_POINT ( 'NONE',  ( 24.16423886937409904, 24.09541550158063927, 3.795296366450317205 ) ) ;
#79731 = VERTEX_POINT ( 'NONE', #23977 ) ;
#79732 = EDGE_CURVE ( 'NONE', #74723, #18712, #13141, .T. ) ;
#79733 = VERTEX_POINT ( 'NONE', #61951 ) ;
#79734 = CARTESIAN_POINT ( 'NONE',  ( 16.40814093676323893, 35.79030133659708923, 11.09922568453595026 ) ) ;
#79735 = VECTOR ( 'NONE', #94079, 1000.000000000000000 ) ;
#79736 = CARTESIAN_POINT ( 'NONE',  ( 17.20831665107776587, 19.13393115100078035, -7.208316651077762316 ) ) ;
#79737 = CARTESIAN_POINT ( 'NONE',  ( -0.8801773607111009756, 3.063685344154837509, 1.068504757029289695E-15 ) ) ;
#79738 = CARTESIAN_POINT ( 'NONE',  ( -1.099225684535947600, 58.70696800326375353, -6.408140936763238038 ) ) ;
#79739 = DIRECTION ( 'NONE',  ( -0.000000000000000000, -1.000000000000000000, -0.000000000000000000 ) ) ;
#79740 = CARTESIAN_POINT ( 'NONE',  ( 7.361572987183170547, 32.05059781766745175, 9.846743663894590881 ) ) ;
#79741 = VECTOR ( 'NONE', #25582, 1000.000000000000000 ) ;
#79742 = CARTESIAN_POINT ( 'NONE',  ( 0.5774900079438607392, 63.48035201082149825, 5.440088680355550821 ) ) ;
#79743 = CARTESIAN_POINT ( 'NONE',  ( -8.000000000000000000, 83.99999999999994316, -3.750000000000000000 ) ) ;
#79744 = FACE_OUTER_BOUND ( 'NONE', #96619, .T. ) ;
#79745 = CARTESIAN_POINT ( 'NONE',  ( 19.72487221294570858, 61.86607318730076344, 6.500000000000000888 ) ) ;
#79746 = CARTESIAN_POINT ( 'NONE',  ( 14.02068044289375415, 0.5000000000000004441, 5.331089937175756965 ) ) ;
#79747 = CARTESIAN_POINT ( 'NONE',  ( 4.559911319644449179, 68.89701867748817676, 9.422509992056141925 ) ) ;
#79748 = CARTESIAN_POINT ( 'NONE',  ( -2.816281873526473856, 24.33196800326375353, 3.434112377981055619 ) ) ;
#79749 = DIRECTION ( 'NONE',  ( 0.000000000000000000, 0.000000000000000000, -1.000000000000000000 ) ) ;
#79750 = CARTESIAN_POINT ( 'NONE',  ( 1.472469842513823179, 45.59226448433412315, -4.923371831947296329 ) ) ;
#79751 = CARTESIAN_POINT ( 'NONE',  ( -1.099225684535947600, 63.70696800326376774, -6.408140936763238038 ) ) ;
#79752 = CARTESIAN_POINT ( 'NONE',  ( 24.16423886937410614, 9.303748834913967869, 8.672049930838204340E-16 ) ) ;
#79753 = CARTESIAN_POINT ( 'NONE',  ( 7.361572987183170547, 27.05059781766745175, 9.846743663894590881 ) ) ;
#79754 = CARTESIAN_POINT ( 'NONE',  ( 16.40814093676323893, 35.79030133659708923, 11.09922568453595026 ) ) ;
#79756 = CARTESIAN_POINT ( 'NONE',  ( 20.03932841506543028, 15.62161441960501485, -6.397827110478962354 ) ) ;
#79755 = LINE ( 'NONE', #42256, #94754 ) ;
#79757 = CARTESIAN_POINT ( 'NONE',  ( -0.8801773607110991993, 67.85535201082151957, -2.915334737309923874 ) ) ;
#79758 = B_SPLINE_CURVE_WITH_KNOTS ( 'NONE', 3,
 ( #89213, #58199, #19240, #48745, #88715, #3763 ),
 .UNSPECIFIED., .F., .F.,
 ( 4, 2, 4 ),
 ( 3.409110551493088148E-05, 0.0004400426677367781148, 0.0008459942299586253617 ),
 .UNSPECIFIED. ) ;
#79759 = CARTESIAN_POINT ( 'NONE',  ( 14.49999999999999822, 11.00000000000000000, 6.000000000000000000 ) ) ;
#79760 = CARTESIAN_POINT ( 'NONE',  ( 18.52753015748618282, 38.92559781766745175, -4.923371831947291888 ) ) ;
#79762 = EDGE_CURVE ( 'NONE', #9609, #41967, #70955, .T. ) ;
#79761 = CARTESIAN_POINT ( 'NONE',  ( 0.5774900079438590739, 27.64701867748817676, -5.440088680355550821 ) ) ;
#79763 = CARTESIAN_POINT ( 'NONE',  ( 10.00000000000000000, 27.87363466993042138, -12.81628187352647608 ) ) ;
#79764 = CARTESIAN_POINT ( 'NONE',  ( 0.1532563361054082862, 21.21726448433412315, 2.638427012816831674 ) ) ;
#79765 = CARTESIAN_POINT ( 'NONE',  ( -12.98310705059785164, 90.76710648773764945, 7.614994760437721055 ) ) ;
#79766 = CARTESIAN_POINT ( 'NONE',  ( 17.96484262340118221, 31.18868534415483751, -7.964842623401177768 ) ) ;
#79767 = EDGE_LOOP ( 'NONE', ( #71523, #71384, #56291 ) ) ;
#79768 = CARTESIAN_POINT ( 'NONE',  ( 4.559911319644449179, 63.89701867748817676, 9.422509992056141925 ) ) ;
#79770 = CARTESIAN_POINT ( 'NONE',  ( -0.8801773607111009756, 28.06368534415484106, 1.068504757029289695E-15 ) ) ;
#79769 = CARTESIAN_POINT ( 'NONE',  ( 12.63842701281683034, 37.46726448433411605, 9.846743663894596210 ) ) ;
#79771 = CARTESIAN_POINT ( 'NONE',  ( -0.8801773607111008646, 48.27201867748816966, 2.915334737309923430 ) ) ;
#79772 = AXIS2_PLACEMENT_3D ( 'NONE', #11423, #85458, #20413 ) ;
#79774 = CARTESIAN_POINT ( 'NONE',  ( 0.2751277870542911397, 40.30223176428831522, 6.499999999999992006 ) ) ;
#79773 = CARTESIAN_POINT ( 'NONE',  ( 19.42250999205614193, 15.14701867748817143, 5.440088680355555262 ) ) ;
#79775 = CARTESIAN_POINT ( 'NONE',  ( 20.15039907845753220, 54.72266099184918886, 6.262539305110078836 ) ) ;
#79776 = CARTESIAN_POINT ( 'NONE',  ( 14.92337183194729988, 49.34226448433411605, -8.527530157486177487 ) ) ;
#79778 = CARTESIAN_POINT ( 'NONE',  ( 4.380000000000001670, 0.09073877121621831687, 3.750000000000000888 ) ) ;
#79777 = CARTESIAN_POINT ( 'NONE',  ( -0.3689425029237898834, 56.17874883491396076, -10.36894250292378850 ) ) ;
#79779 = DIRECTION ( 'NONE',  ( 1.000000000000000000, 0.000000000000000000, 0.000000000000000000 ) ) ;
#79780 = CARTESIAN_POINT ( 'NONE',  ( 13.82671409943293739, 0.000000000000000000, 3.447387012295318076 ) ) ;
#79781 = CARTESIAN_POINT ( 'NONE',  ( 24.16423886937409904, 39.09541550158062506, 3.795296366450317205 ) ) ;
#79782 = CARTESIAN_POINT ( 'NONE',  ( 0.000000000000000000, 14.49999999999999822, 0.000000000000000000 ) ) ;
#79783 = EDGE_LOOP ( 'NONE', ( #30270, #29063, #87986, #36848 ) ) ;
#79784 = CARTESIAN_POINT ( 'NONE',  ( -0.8801773607111009756, 3.063685344154838397, 1.068504757029289695E-15 ) ) ;
#79785 = CARTESIAN_POINT ( 'NONE',  ( 19.84674366389459266, 33.71726448433410894, -2.638427012816827677 ) ) ;
#79787 = CARTESIAN_POINT ( 'NONE',  ( -8.048010592883702685, 84.92462609336300261, -4.034077756265262771 ) ) ;
#79786 = DIRECTION ( 'NONE',  ( -0.000000000000000000, 1.000000000000000000, -0.000000000000000000 ) ) ;
#79788 = CARTESIAN_POINT ( 'NONE',  ( 7.084665262690076126, 62.02201867748816966, -10.88017736071110164 ) ) ;
#79789 = DIRECTION ( 'NONE',  ( 1.000000000000000000, 0.000000000000000000, 0.000000000000000000 ) ) ;
#79790 = CARTESIAN_POINT ( 'NONE',  ( 2.035157376598824452, 28.68868534415484106, 7.964842623401179544 ) ) ;
#79791 = EDGE_CURVE ( 'NONE', #88687, #54112, #41716, .T. ) ;
#79792 = CARTESIAN_POINT ( 'NONE',  ( 13.43411237798106583, 57.66530133659708923, -12.81628187352647252 ) ) ;
#79793 = CARTESIAN_POINT ( 'NONE',  ( 21.09922568453594849, 16.20696800326375353, 6.408140936763242479 ) ) ;
#79794 = CARTESIAN_POINT ( 'NONE',  ( 10.00000000000000000, 19.75893115100078390, -9.846743663894594434 ) ) ;
#79795 = ORIENTED_EDGE ( 'NONE', *, *, #28919, .F. ) ;
#79796 = SURFACE_STYLE_FILL_AREA ( #78817 ) ;
#79797 = CARTESIAN_POINT ( 'NONE',  ( -12.67122524790580762, 0.04922511925147277784, -7.555537761805941166 ) ) ;
#79798 = CARTESIAN_POINT ( 'NONE',  ( -4.164238869374098151, 66.59541550158060375, -3.795296366450310543 ) ) ;
#79799 = CARTESIAN_POINT ( 'NONE',  ( 20.36894250292379382, 23.67874883491397142, 10.36894250292379205 ) ) ;
#79800 = CARTESIAN_POINT ( 'NONE',  ( 12.91533473730993009, 26.60535201082150536, -10.88017736071109987 ) ) ;
#79801 = CARTESIAN_POINT ( 'NONE',  ( 0.5774900079438607392, 53.48035201082151247, 5.440088680355550821 ) ) ;
#79802 = AXIS2_PLACEMENT_3D ( 'NONE', #61322, #59842, #7850 ) ;
#79803 = FACE_OUTER_BOUND ( 'NONE', #84071, .T. ) ;
#79804 = CARTESIAN_POINT ( 'NONE',  ( 19.84674366389459266, 13.71726448433411782, -2.638427012816827677 ) ) ;
#79805 = DIRECTION ( 'NONE',  ( 0.000000000000000000, 0.000000000000000000, 1.000000000000000000 ) ) ;
#79806 = DIRECTION ( 'NONE',  ( 0.000000000000000000, 0.000000000000000000, 1.000000000000000000 ) ) ;
#79807 = CARTESIAN_POINT ( 'NONE',  ( 2.791683348922240793, 26.63393115100078745, 7.208316651077764092 ) ) ;
#79808 = CARTESIAN_POINT ( 'NONE',  ( 19.84674366389459621, 43.50893115100078745, 7.409399052514197653E-17 ) ) ;
#79809 = CARTESIAN_POINT ( 'NONE',  ( 0.5774900079438607392, 23.48035201082150536, 5.440088680355550821 ) ) ;
#79810 = CARTESIAN_POINT ( 'NONE',  ( 6.565887622018943937, 43.08196800326374643, -12.81628187352647608 ) ) ;
#79811 = CARTESIAN_POINT ( 'NONE',  ( 0.000000000000000000, 0.5000000000000004441, 0.000000000000000000 ) ) ;
#79812 = CARTESIAN_POINT ( 'NONE',  ( 5.076628168052703671, 1.842264484334118047, 8.527530157486179263 ) ) ;
#79813 = CARTESIAN_POINT ( 'NONE',  ( 14.92337183194729988, 34.34226448433411605, -8.527530157486177487 ) ) ;
#79815 = CARTESIAN_POINT ( 'NONE',  ( 0.1532563361054083140, 26.00893115100078745, 1.131784320476157264E-15 ) ) ;
#79814 = CARTESIAN_POINT ( 'NONE',  ( 22.26659068614894466, 58.88708216824729647, 7.082119434687054849 ) ) ;
#79817 = EDGE_CURVE ( 'NONE', #64436, #18416, #26177, .T. ) ;
#79816 = CARTESIAN_POINT ( 'NONE',  ( 0.2751277870542909731, 44.36607318730131055, -6.499999999999992006 ) ) ;
#79818 = EDGE_CURVE ( 'NONE', #14873, #45794, #65664, .T. ) ;
#79819 = CARTESIAN_POINT ( 'NONE',  ( 2.791683348922237240, 60.38393115100078745, -7.208316651077763204 ) ) ;
#79820 = CARTESIAN_POINT ( 'NONE',  ( 13.79529636645030344, 13.26208216824729824, 14.16423886937410614 ) ) ;
#79821 = CARTESIAN_POINT ( 'NONE',  ( -4.164238869374099927, 27.01208216824730357, 3.795296366450308767 ) ) ;
#79822 = CARTESIAN_POINT ( 'NONE',  ( 14.92337183194729988, 34.34226448433411605, -8.527530157486177487 ) ) ;
#79823 = CARTESIAN_POINT ( 'NONE',  ( 18.72515096720569616, 10.05509018479935968, 6.500000000000001776 ) ) ;
#79824 = CARTESIAN_POINT ( 'NONE',  ( 12.91533473730992121, 29.52201867748817321, 10.88017736071110164 ) ) ;
#79825 = CARTESIAN_POINT ( 'NONE',  ( 7.084665262690076126, 54.10535201082151247, 10.88017736071109987 ) ) ;
#79826 = EDGE_LOOP ( 'NONE', ( #15684, #75526, #85945, #25747 ) ) ;
#79827 = CARTESIAN_POINT ( 'NONE',  ( 10.00000000000000000, 47.87363466993042493, -12.81628187352647608 ) ) ;
#79828 = CARTESIAN_POINT ( 'NONE',  ( 17.96484262340118221, 54.93868534415484106, 7.964842623401181321 ) ) ;
#79829 = VERTEX_POINT ( 'NONE', #93937 ) ;
#79830 = SURFACE_STYLE_USAGE ( .BOTH. , #18848 ) ;
#79831 = CARTESIAN_POINT ( 'NONE',  ( 19.42250999205614548, 65.98035201082151957, -5.440088680355545492 ) ) ;
#79832 = ORIENTED_EDGE ( 'NONE', *, *, #70598, .T. ) ;
#79833 = CARTESIAN_POINT ( 'NONE',  ( 4.559911319644449179, 68.89701867748817676, 9.422509992056141925 ) ) ;
#79834 = LINE ( 'NONE', #19339, #43592 ) ;
#79835 = LINE ( 'NONE', #72323, #979 ) ;
#79836 = CARTESIAN_POINT ( 'NONE',  ( 2.035157376598822676, 2.438685344154838397, -7.964842623401177768 ) ) ;
#79837 = CARTESIAN_POINT ( 'NONE',  ( 18.52753015748618282, 3.925597817667451306, -4.923371831947291888 ) ) ;
#79838 = CARTESIAN_POINT ( 'NONE',  ( 13.79529636645030344, 13.26208216824729824, 14.16423886937410614 ) ) ;
#79839 = CARTESIAN_POINT ( 'NONE',  ( 2.791683348922237240, 5.383931151000785675, -7.208316651077763204 ) ) ;
#79840 = CARTESIAN_POINT ( 'NONE',  ( 15.44008868035555260, 29.73035201082150891, 9.422509992056143702 ) ) ;
#79841 = CARTESIAN_POINT ( 'NONE',  ( 18.52753015748618282, 48.92559781766745886, -4.923371831947291888 ) ) ;
#79842 = ORIENTED_EDGE ( 'NONE', *, *, #65694, .T. ) ;
#79843 = EDGE_CURVE ( 'NONE', #21583, #32106, #27886, .T. ) ;
#79844 = PRESENTATION_LAYER_ASSIGNMENT (  '', '', ( #43155 ) ) ;
#79845 = CARTESIAN_POINT ( 'NONE',  ( 0.1532563361054083140, 46.00893115100079456, 1.131784320476157264E-15 ) ) ;
#79846 = VERTEX_POINT ( 'NONE', #79431 ) ;
#79847 = CARTESIAN_POINT ( 'NONE',  ( -10.27090289957521207, -3.117928278843078365E-15, -10.41235154178118805 ) ) ;
#79848 = CARTESIAN_POINT ( 'NONE',  ( 7.084665262690076126, 54.10535201082151247, 10.88017736071109987 ) ) ;
#79849 = CARTESIAN_POINT ( 'NONE',  ( 12.63842701281683034, 47.46726448433412315, 9.846743663894596210 ) ) ;
#79850 = CARTESIAN_POINT ( 'NONE',  ( -2.816281873526473856, 29.33196800326376064, 3.434112377981055619 ) ) ;
#79852 = CYLINDRICAL_SURFACE ( 'NONE', #28743, 0.09999999999999939493 ) ;
#79851 = CARTESIAN_POINT ( 'NONE',  ( -0.8801773607111008646, 13.27201867748817143, 2.915334737309923430 ) ) ;
#79853 = CARTESIAN_POINT ( 'NONE',  ( 20.88017736071110875, 55.77201867748816966, -2.915334737309920765 ) ) ;
#79854 = CIRCLE ( 'NONE', #36688, 14.49999999999999822 ) ;
#79855 = CARTESIAN_POINT ( 'NONE',  ( 7.084665262690076126, 9.105352010821503583, 10.88017736071109987 ) ) ;
#79856 = PRESENTATION_LAYER_ASSIGNMENT (  '', '', ( #19187 ) ) ;
#79857 = CARTESIAN_POINT ( 'NONE',  ( 22.81628187352648496, 36.83196800326376064, -3.434112377981050290 ) ) ;
#79858 = CARTESIAN_POINT ( 'NONE',  ( 2.035157376598822676, 32.43868534415483396, -7.964842623401177768 ) ) ;
#79859 = LINE ( 'NONE', #94366, #73805 ) ;
#79860 = ORIENTED_EDGE ( 'NONE', *, *, #79251, .F. ) ;
#79861 = CARTESIAN_POINT ( 'NONE',  ( 13.43411237798106583, 47.66530133659709634, -12.81628187352647252 ) ) ;
#79862 = CARTESIAN_POINT ( 'NONE',  ( 17.96484262340118221, 39.93868534415484106, 7.964842623401181321 ) ) ;
#79863 = ORIENTED_EDGE ( 'NONE', *, *, #15312, .F. ) ;
#79864 = CIRCLE ( 'NONE', #36778, 7.000000000000006217 ) ;
#79865 = CARTESIAN_POINT ( 'NONE',  ( 2.791683348922237240, 65.38393115100078035, -7.208316651077763204 ) ) ;
#79867 = CARTESIAN_POINT ( 'NONE',  ( 12.63842701281683922, 49.55059781766744464, -9.846743663894590881 ) ) ;
#79866 = CARTESIAN_POINT ( 'NONE',  ( 0.1532563361054083140, 16.00893115100078390, 1.131784320476157264E-15 ) ) ;
#79868 = CARTESIAN_POINT ( 'NONE',  ( 20.88017736071110519, 20.56368534415484106, 2.639326808657452039E-16 ) ) ;
#79869 = CARTESIAN_POINT ( 'NONE',  ( -36.44000000000001194, 92.00000000000000000, 9.500000000000000000 ) ) ;
#79870 = CARTESIAN_POINT ( 'NONE',  ( 0.1532563361054082862, 36.21726448433410894, 2.638427012816831674 ) ) ;
#79871 = CARTESIAN_POINT ( 'NONE',  ( 14.99999999999997868, 79.82179676972448590, 6.250000000000000000 ) ) ;
#79872 = CARTESIAN_POINT ( 'NONE',  ( 13.55255535720591986, -0.03417435944610275333, 4.403492169843056914 ) ) ;
#79874 = CARTESIAN_POINT ( 'NONE',  ( 17.20831665107776587, 9.133931151000787452, -7.208316651077762316 ) ) ;
#79873 = CARTESIAN_POINT ( 'NONE',  ( 12.63842701281683034, 22.46726448433411605, 9.846743663894596210 ) ) ;
#79875 = CARTESIAN_POINT ( 'NONE',  ( 0.2751277870542981341, 8.218334437839383000, 6.500000000000002665 ) ) ;
#79877 = VERTEX_POINT ( 'NONE', #33897 ) ;
#79876 = CARTESIAN_POINT ( 'NONE',  ( 12.63842701281683922, 54.55059781766745175, -9.846743663894590881 ) ) ;
#79878 = CARTESIAN_POINT ( 'NONE',  ( 6.565887622018943937, 30.16530133659708568, 12.81628187352647430 ) ) ;
#79879 = CARTESIAN_POINT ( 'NONE',  ( 0.1532563361054100626, 45.80059781766745886, -2.638427012816831230 ) ) ;
#79880 = CARTESIAN_POINT ( 'NONE',  ( -13.61802159414306423, 15.00000000000000533, 5.334603887713395665 ) ) ;
#79881 = CARTESIAN_POINT ( 'NONE',  ( 2.917880565312948704, 62.63708216824730357, 12.26659068614894643 ) ) ;
#79882 = CARTESIAN_POINT ( 'NONE',  ( 7.361572987183170547, 12.05059781766744997, 9.846743663894590881 ) ) ;
#79883 = CARTESIAN_POINT ( 'NONE',  ( 20.00000000000141043, 85.78121477524163652, 5.248003389972544674 ) ) ;
#79884 = CARTESIAN_POINT ( 'NONE',  ( 2.917880565312948704, 62.63708216824730357, 12.26659068614894643 ) ) ;
#79885 = CARTESIAN_POINT ( 'NONE',  ( 19.84674366389459621, 63.50893115100078745, 7.409399052514197653E-17 ) ) ;
#79886 = CARTESIAN_POINT ( 'NONE',  ( -4.164238869374099927, 67.01208216824728936, 3.795296366450308767 ) ) ;
#79887 = CARTESIAN_POINT ( 'NONE',  ( -4.164238869374098151, 36.59541550158063217, -3.795296366450310543 ) ) ;
#79888 = CARTESIAN_POINT ( 'NONE',  ( 24.16423886937410614, 34.51208216824731068, -3.795296366450302550 ) ) ;
#79889 = DIRECTION ( 'NONE',  ( -0.5664062369248259454, 0.000000000000000000, -0.8241261886220204724 ) ) ;
#79891 = CARTESIAN_POINT ( 'NONE',  ( 1.472469842513823179, 50.59226448433411605, -4.923371831947296329 ) ) ;
#79890 = CARTESIAN_POINT ( 'NONE',  ( -0.8801773607110990882, 27.85535201082150181, -2.915334737309924318 ) ) ;
#79892 = EDGE_LOOP ( 'NONE', ( #3652, #69912, #5477, #63475 ) ) ;
#79893 = CARTESIAN_POINT ( 'NONE',  ( 19.42250999205614193, 55.14701867748817676, 5.440088680355555262 ) ) ;
#79894 = ADVANCED_FACE ( 'NONE', ( #64403 ), #33410, .F. ) ;
#79895 = CARTESIAN_POINT ( 'NONE',  ( 11.40653762822727835, -69.23734991727425836, 3.750000000000000444 ) ) ;
#79896 = CARTESIAN_POINT ( 'NONE',  ( 17.20831665107776587, 52.88393115100078035, 7.208316651077764980 ) ) ;
#79897 = CARTESIAN_POINT ( 'NONE',  ( -2.816281873526473856, 64.33196800326376774, 3.434112377981055619 ) ) ;
#79898 = CARTESIAN_POINT ( 'NONE',  ( 18.52753015748617571, 53.09226448433412315, 4.923371831947298993 ) ) ;
#79899 = CARTESIAN_POINT ( 'NONE',  ( -0.3093388210927642268, 0.5000000000000004441, 14.99680997725065978 ) ) ;
#79900 = ORIENTED_EDGE ( 'NONE', *, *, #2514, .F. ) ;
#79901 = CARTESIAN_POINT ( 'NONE',  ( 20.36894250292379382, 28.67874883491396787, 10.36894250292379205 ) ) ;
#79902 = CARTESIAN_POINT ( 'NONE',  ( 5.076628168052703671, 1.842264484334118047, 8.527530157486179263 ) ) ;
#79903 = CARTESIAN_POINT ( 'NONE',  ( -10.93781366033334557, 14.63606902047462199, -10.26470809774084181 ) ) ;
#79904 = CARTESIAN_POINT ( 'NONE',  ( -0.8801773607110991993, 22.85535201082150181, -2.915334737309923874 ) ) ;
#79905 = CARTESIAN_POINT ( 'NONE',  ( 3.591859063236761518, 19.95696800326375353, 11.09922568453594849 ) ) ;
#79906 = CARTESIAN_POINT ( 'NONE',  ( 20.24186590665278018, 62.61633188102329228, -6.114288769123040090 ) ) ;
#79907 = CARTESIAN_POINT ( 'NONE',  ( 10.00000000000000178, 12.25893115100078568, 9.846743663894594434 ) ) ;
#79908 = AXIS2_PLACEMENT_3D ( 'NONE', #29373, #90864, #74375 ) ;
#79909 = EDGE_LOOP ( 'NONE', ( #32581, #69883, #39086, #82408 ) ) ;
#79910 = CARTESIAN_POINT ( 'NONE',  ( 4.657035931814768048, -8.268334176803392666, -3.749999999999597211 ) ) ;
#79911 = CARTESIAN_POINT ( 'NONE',  ( 22.26659068614894466, 33.88708216824730357, 7.082119434687054849 ) ) ;
#79912 = LINE ( 'NONE', #49908, #45836 ) ;
#79913 = CARTESIAN_POINT ( 'NONE',  ( -3.878335320991981305, -3.629921146508676255, 4.000000000000000000 ) ) ;
#79914 = CARTESIAN_POINT ( 'NONE',  ( 2.035157376598824452, 3.688685344154837953, 7.964842623401179544 ) ) ;
#79915 = CARTESIAN_POINT ( 'NONE',  ( 14.49440716394870954, 15.00000000000000000, 0.4026921475167317688 ) ) ;
#79916 = CARTESIAN_POINT ( 'NONE',  ( 0.5774900079438607392, 33.48035201082150536, 5.440088680355550821 ) ) ;
#79917 = CARTESIAN_POINT ( 'NONE',  ( 17.96484262340118221, 39.93868534415484106, 7.964842623401181321 ) ) ;
#79918 = CARTESIAN_POINT ( 'NONE',  ( 19.38216949554541557, 17.24863466993041783, -9.382169495545420901 ) ) ;
#79919 = CARTESIAN_POINT ( 'NONE',  ( 0.1532563361054100626, 65.80059781766745175, -2.638427012816831230 ) ) ;
#79920 = CARTESIAN_POINT ( 'NONE',  ( 0.2751277870542967463, 70.00000000000000000, 6.000000000000000000 ) ) ;
#79921 = CARTESIAN_POINT ( 'NONE',  ( 7.361572987183170547, 12.05059781766744997, 9.846743663894590881 ) ) ;
#79922 = EDGE_CURVE ( 'NONE', #59678, #54738, #75057, .T. ) ;
#79923 = VECTOR ( 'NONE', #83184, 1000.000000000000000 ) ;
#79924 = CARTESIAN_POINT ( 'NONE',  ( 18.28836319691943046, 49.34492782695771496, 6.500000000000079936 ) ) ;
#79925 = CARTESIAN_POINT ( 'NONE',  ( 12.91533473730992121, 49.52201867748817676, 10.88017736071110164 ) ) ;
#79926 = EDGE_CURVE ( 'NONE', #58432, #44471, #72893, .T. ) ;
#79927 = CARTESIAN_POINT ( 'NONE',  ( 16.40814093676323893, 0.7903013365970867898, 11.09922568453595026 ) ) ;
#79928 = CARTESIAN_POINT ( 'NONE',  ( -0.8801773607111009756, 63.06368534415484106, 1.068504757029289695E-15 ) ) ;
#79929 = EDGE_CURVE ( 'NONE', #17551, #56358, #72551, .T. ) ;
#79930 = CARTESIAN_POINT ( 'NONE',  ( 0.1532563361054100626, 30.80059781766744820, -2.638427012816831230 ) ) ;
#79931 = CARTESIAN_POINT ( 'NONE',  ( 6.565887622018943937, 33.08196800326374643, -12.81628187352647608 ) ) ;
#79933 = DIRECTION ( 'NONE',  ( 0.000000000000000000, 0.000000000000000000, -1.000000000000000000 ) ) ;
#79932 = CARTESIAN_POINT ( 'NONE',  ( 2.791683348922240793, 1.633931151000784565, 7.208316651077764092 ) ) ;
#79934 = ORIENTED_EDGE ( 'NONE', *, *, #44715, .F. ) ;
#79935 = CARTESIAN_POINT ( 'NONE',  ( 4.600000000000003197, 98.49999999999998579, -8.000000000000000000 ) ) ;
#79936 = DIRECTION ( 'NONE',  ( 1.000000000000000000, 1.257402221000611116E-16, -0.000000000000000000 ) ) ;
#79937 = CARTESIAN_POINT ( 'NONE',  ( 10.00000000000000178, 9.313685344154839285, 10.88017736071110342 ) ) ;
#79939 = CARTESIAN_POINT ( 'NONE',  ( -4.164238869374099927, 22.01208216824730357, 3.795296366450308767 ) ) ;
#79938 = CARTESIAN_POINT ( 'NONE',  ( 19.38216949554541557, 62.24863466993041072, -9.382169495545420901 ) ) ;
#79940 = CARTESIAN_POINT ( 'NONE',  ( 14.92337183194729633, 32.67559781766745175, 8.527530157486181039 ) ) ;
#79941 = CARTESIAN_POINT ( 'NONE',  ( 0.5774900079438590739, 22.64701867748817321, -5.440088680355550821 ) ) ;
#79942 = AXIS2_PLACEMENT_3D ( 'NONE', #93069, #8112, #24103 ) ;
#79943 = CARTESIAN_POINT ( 'NONE',  ( 17.96484262340118221, 9.938685344154839285, 7.964842623401181321 ) ) ;
#79944 = ORIENTED_EDGE ( 'NONE', *, *, #29563, .T. ) ;
#79945 = B_SPLINE_CURVE_WITH_KNOTS ( 'NONE', 3,
 ( #67837, #14848, #37839, #60322, #76798, #31291 ),
 .UNSPECIFIED., .F., .F.,
 ( 4, 2, 4 ),
 ( 3.409110551333654864E-05, 0.0004400426677351659062, 0.0008459942299569952638 ),
 .UNSPECIFIED. ) ;
#79946 = TOROIDAL_SURFACE ( 'NONE', #8162, 14.49999999999999822, 0.5000000000000000000 ) ;
#79947 = CARTESIAN_POINT ( 'NONE',  ( 7.084665262690076126, 7.022018677488169658, -10.88017736071110164 ) ) ;
#79948 = CARTESIAN_POINT ( 'NONE',  ( 15.44008868035555260, 24.73035201082150891, 9.422509992056143702 ) ) ;
#79949 = CARTESIAN_POINT ( 'NONE',  ( 20.15039907845753575, 32.62777174578613426, -6.262539305110076171 ) ) ;
#79950 = ORIENTED_EDGE ( 'NONE', *, *, #80162, .T. ) ;
#79951 = CARTESIAN_POINT ( 'NONE',  ( 20.15039907845753220, 27.62777174578613071, -6.262539305110077947 ) ) ;
#79952 = CARTESIAN_POINT ( 'NONE',  ( 20.88017736071110164, 25.35535201082150891, 2.915334737309930979 ) ) ;
#79953 = CARTESIAN_POINT ( 'NONE',  ( 18.52753015748618282, 58.92559781766745886, -4.923371831947291888 ) ) ;
#79954 = MECHANICAL_DESIGN_GEOMETRIC_PRESENTATION_REPRESENTATION (  '', ( #124 ), #78304 ) ;
#79955 = FACE_OUTER_BOUND ( 'NONE', #87863, .T. ) ;
#79956 = CARTESIAN_POINT ( 'NONE',  ( 21.09922568453595559, 47.04030133659708923, -6.408140936763230044 ) ) ;
#79957 = DIRECTION ( 'NONE',  ( 1.000000000000000000, -5.818595309480553908E-17, 0.000000000000000000 ) ) ;
#79958 = CARTESIAN_POINT ( 'NONE',  ( 13.79529636645030344, 28.26208216824729647, 14.16423886937410614 ) ) ;
#79959 = CARTESIAN_POINT ( 'NONE',  ( -0.8801773607110991993, 37.85535201082151247, -2.915334737309923874 ) ) ;
#79960 = CARTESIAN_POINT ( 'NONE',  ( 12.91533473730992121, 19.52201867748816611, 10.88017736071110164 ) ) ;
#79961 = CARTESIAN_POINT ( 'NONE',  ( 0.1532563361054082862, 61.21726448433412315, 2.638427012816831674 ) ) ;
#79962 = CARTESIAN_POINT ( 'NONE',  ( -11.19838940738413235, -94.49360967301636549, -3.750000000000000000 ) ) ;
#79963 = CARTESIAN_POINT ( 'NONE',  ( 0.1532563361054100626, 55.80059781766745175, -2.638427012816831230 ) ) ;
#79964 = EDGE_CURVE ( 'NONE', #46643, #60588, #26906, .T. ) ;
#79965 = CARTESIAN_POINT ( 'NONE',  ( 0.1532563361054083140, 6.008931151000784787, 1.131784320476157264E-15 ) ) ;
#79966 = CARTESIAN_POINT ( 'NONE',  ( 3.434112377981060948, -34.41803199673624647, 12.81628187352647430 ) ) ;
#79967 = ORIENTED_EDGE ( 'NONE', *, *, #22911, .T. ) ;
#79968 = CARTESIAN_POINT ( 'NONE',  ( 15.44008868035555260, 9.730352010821505360, 9.422509992056143702 ) ) ;
#79969 = CARTESIAN_POINT ( 'NONE',  ( 19.84674366389459621, 8.508931151000785675, 7.409399052514197653E-17 ) ) ;
#79970 = CARTESIAN_POINT ( 'NONE',  ( -2.816281873526473856, 4.331968003263754419, 3.434112377981055619 ) ) ;
#79971 = CARTESIAN_POINT ( 'NONE',  ( 12.91533473730993009, 61.60535201082150536, -10.88017736071109987 ) ) ;
#79973 = CARTESIAN_POINT ( 'NONE',  ( -1.099225684535947600, 39.54030133659708923, 6.408140936763237150 ) ) ;
#79972 = CARTESIAN_POINT ( 'NONE',  ( 7.084665262690076126, 24.10535201082150181, 10.88017736071109987 ) ) ;
#79974 = CARTESIAN_POINT ( 'NONE',  ( -4.164238869374099927, 32.01208216824730357, 3.795296366450308767 ) ) ;
#79975 = CARTESIAN_POINT ( 'NONE',  ( 14.16722289976686966, 14.49999999999999112, 4.928467845925658786 ) ) ;
#79976 = EDGE_CURVE ( 'NONE', #28751, #46643, #15400, .T. ) ;
#79977 = CIRCLE ( 'NONE', #70424, 0.2000000000000000944 ) ;
#79978 = CARTESIAN_POINT ( 'NONE',  ( 3.591859063236763294, 58.29030133659708923, -11.09922568453595026 ) ) ;
#79979 = EDGE_LOOP ( 'NONE', ( #36473, #81567, #18371, #64686 ) ) ;
#79980 = CARTESIAN_POINT ( 'NONE',  ( 22.81628187352648496, 6.831968003263753531, -3.434112377981050290 ) ) ;
#79981 = PRESENTATION_STYLE_ASSIGNMENT (( #65956 ) ) ;
#79982 = CARTESIAN_POINT ( 'NONE',  ( 15.44008868035555793, 36.39701867748816966, -9.422509992056140149 ) ) ;
#79983 =( GEOMETRIC_REPRESENTATION_CONTEXT ( 3 ) GLOBAL_UNCERTAINTY_ASSIGNED_CONTEXT ( ( #66398 ) ) GLOBAL_UNIT_ASSIGNED_CONTEXT ( ( #75256, #22278, #29746 ) ) REPRESENTATION_CONTEXT ( 'NONE', 'WORKASPACE' ) );
#79984 = CARTESIAN_POINT ( 'NONE',  ( 5.076628168052703671, 61.84226448433412315, 8.527530157486179263 ) ) ;
#79985 = ORIENTED_EDGE ( 'NONE', *, *, #17637, .F. ) ;
#79987 = CARTESIAN_POINT ( 'NONE',  ( -0.2418659066527703017, 64.26028685723176181, -6.114288769123047196 ) ) ;
#79986 = CARTESIAN_POINT ( 'NONE',  ( 17.20831665107776587, 7.883931151000784787, 7.208316651077764980 ) ) ;
#79988 = CARTESIAN_POINT ( 'NONE',  ( 0.1532563361054083140, 11.00893115100078568, 1.131784320476157264E-15 ) ) ;
#79989 = CARTESIAN_POINT ( 'NONE',  ( 1.472469842513823179, 20.59226448433411960, -4.923371831947296329 ) ) ;
#79990 = CARTESIAN_POINT ( 'NONE',  ( 1.472469842513823179, 11.42559781766745175, 4.923371831947296329 ) ) ;
#79992 = CARTESIAN_POINT ( 'NONE',  ( -0.8801773607111009756, 38.06368534415484106, 1.068504757029289695E-15 ) ) ;
#79991 = CARTESIAN_POINT ( 'NONE',  ( 17.96484262340118221, 51.18868534415483396, -7.964842623401177768 ) ) ;
#79993 = CARTESIAN_POINT ( 'NONE',  ( 15.44008868035555260, 59.73035201082151247, 9.422509992056143702 ) ) ;
#79995 = EDGE_LOOP ( 'NONE', ( #79462, #38591, #75138, #53256 ) ) ;
#79994 = CARTESIAN_POINT ( 'NONE',  ( 19.84674366389459266, 13.30059781766745353, 2.638427012816836559 ) ) ;
#79996 = CARTESIAN_POINT ( 'NONE',  ( 5.076628168052704559, 60.17559781766745175, -8.527530157486179263 ) ) ;
#79997 = ORIENTED_EDGE ( 'NONE', *, *, #66199, .F. ) ;
#79998 = FILL_AREA_STYLE_COLOUR ( '', #80920 ) ;
#79999 = CARTESIAN_POINT ( 'NONE',  ( 13.79529636645030344, 23.26208216824730002, 14.16423886937410614 ) ) ;
#80000 = CARTESIAN_POINT ( 'NONE',  ( 14.67697702673042848, 15.00000000000000000, -6.361111679013412790 ) ) ;
#80001 = CARTESIAN_POINT ( 'NONE',  ( 10.00000000000000000, 10.55374883491396787, -14.16423886937410082 ) ) ;
#80002 = CARTESIAN_POINT ( 'NONE',  ( 20.36894250292379382, 28.67874883491396787, 10.36894250292379205 ) ) ;
#80003 = EDGE_CURVE ( 'NONE', #71011, #14567, #16965, .T. ) ;
#80004 = DIRECTION ( 'NONE',  ( 0.000000000000000000, -1.000000000000000000, 0.000000000000000000 ) ) ;
#80005 = CARTESIAN_POINT ( 'NONE',  ( 20.88017736071110519, 35.56368534415484106, 2.639326808657452039E-16 ) ) ;
#80006 = CARTESIAN_POINT ( 'NONE',  ( 8.776446609406717059, 70.10355339059326241, 6.500000000000001776 ) ) ;
#80007 = ORIENTED_EDGE ( 'NONE', *, *, #68311, .F. ) ;
#80008 = CARTESIAN_POINT ( 'NONE',  ( 7.361572987183169658, 19.96726448433411960, -9.846743663894592657 ) ) ;
#80010 = CARTESIAN_POINT ( 'NONE',  ( 2.791683348922240793, 11.63393115100078568, 7.208316651077764092 ) ) ;
#80009 = CARTESIAN_POINT ( 'NONE',  ( 12.91533473730992121, 59.52201867748816966, 10.88017736071110164 ) ) ;
#80011 = VECTOR ( 'NONE', #52849, 1000.000000000000000 ) ;
#80012 = MECHANICAL_DESIGN_GEOMETRIC_PRESENTATION_REPRESENTATION (  '', ( #1820 ), #30547 ) ;
#80013 = CARTESIAN_POINT ( 'NONE',  ( 13.43411237798106583, 47.66530133659709634, -12.81628187352647252 ) ) ;
#80014 = CARTESIAN_POINT ( 'NONE',  ( 14.92337183194729988, 34.34226448433411605, -8.527530157486177487 ) ) ;
#80015 = ADVANCED_FACE ( 'NONE', ( #87893 ), #19410, .F. ) ;
#80016 = FACE_OUTER_BOUND ( 'NONE', #65940, .T. ) ;
#80017 = CARTESIAN_POINT ( 'NONE',  ( 21.09922568453595559, 32.04030133659708923, -6.408140936763230044 ) ) ;
#80018 = CARTESIAN_POINT ( 'NONE',  ( 7.082119434687054849, -36.52958449841936783, 12.26659068614894288 ) ) ;
#80019 = CARTESIAN_POINT ( 'NONE',  ( 0.1532563361054083140, 31.00893115100078390, 1.131784320476157264E-15 ) ) ;
#80020 = MECHANICAL_DESIGN_GEOMETRIC_PRESENTATION_REPRESENTATION (  '', ( #30484 ), #76809 ) ;
#80021 = CARTESIAN_POINT ( 'NONE',  ( -4.164238869374099927, 7.012082168247302683, 3.795296366450308767 ) ) ;
#80022 = ORIENTED_EDGE ( 'NONE', *, *, #70069, .T. ) ;
#80023 = ORIENTED_EDGE ( 'NONE', *, *, #95402, .F. ) ;
#80024 = CARTESIAN_POINT ( 'NONE',  ( 20.88017736071110875, 50.77201867748817676, -2.915334737309920765 ) ) ;
#80025 = CARTESIAN_POINT ( 'NONE',  ( 17.96484262340118221, 56.18868534415484817, -7.964842623401177768 ) ) ;
#80026 = CARTESIAN_POINT ( 'NONE',  ( -4.164238869374098151, 41.59541550158061796, -3.795296366450310543 ) ) ;
#80027 = CARTESIAN_POINT ( 'NONE',  ( 19.84674366389459266, 58.71726448433411605, -2.638427012816827677 ) ) ;
#80028 = CARTESIAN_POINT ( 'NONE',  ( 5.076628168052703671, 16.84226448433411960, 8.527530157486179263 ) ) ;
#80029 = CARTESIAN_POINT ( 'NONE',  ( -2.816281873526473856, 64.12363466993042493, 9.499525473075851096E-16 ) ) ;
#80030 = CARTESIAN_POINT ( 'NONE',  ( 0.5774900079438607392, 43.48035201082151247, 5.440088680355550821 ) ) ;
#80031 = CARTESIAN_POINT ( 'NONE',  ( 0.2751277870543045734, 27.28217586085238011, -6.500000000000012434 ) ) ;
#80032 = CARTESIAN_POINT ( 'NONE',  ( 22.81628187352647785, 26.62363466993042138, 6.195893100308588602E-16 ) ) ;
#80033 = CARTESIAN_POINT ( 'NONE',  ( 5.076628168052703671, 56.84226448433412315, 8.527530157486179263 ) ) ;
#80034 = CARTESIAN_POINT ( 'NONE',  ( 3.469446951953614189E-15, 14.31368534415484284, 10.88017736071110342 ) ) ;
#80035 = CARTESIAN_POINT ( 'NONE',  ( 19.42250999205614548, 5.980352010821504471, -5.440088680355545492 ) ) ;
#80036 = CARTESIAN_POINT ( 'NONE',  ( -0.1503990784575359729, 13.10158574516642105, 6.262539305110062848 ) ) ;
#80037 = CARTESIAN_POINT ( 'NONE',  ( 15.44008868035555260, 9.730352010821505360, 9.422509992056143702 ) ) ;
#80038 =( NAMED_UNIT ( * ) PLANE_ANGLE_UNIT ( ) SI_UNIT ( $, .RADIAN. ) );
#80039 = CARTESIAN_POINT ( 'NONE',  ( 1.472469842513823179, 0.5922644843341181575, -4.923371831947296329 ) ) ;
#80040 = VECTOR ( 'NONE', #96658, 1000.000000000000114 ) ;
#80041 = CARTESIAN_POINT ( 'NONE',  ( 12.91533473730993009, 66.60535201082150536, -10.88017736071109987 ) ) ;
#80042 = LINE ( 'NONE', #28021, #63231 ) ;
#80043 = EDGE_CURVE ( 'NONE', #45188, #55250, #23401, .T. ) ;
#80044 = CARTESIAN_POINT ( 'NONE',  ( 2.791683348922240793, 41.63393115100078745, 7.208316651077764092 ) ) ;
#80045 = CARTESIAN_POINT ( 'NONE',  ( 7.084665262690076126, 24.10535201082150181, 10.88017736071109987 ) ) ;
#80046 = ADVANCED_FACE ( 'NONE', ( #63908 ), #26581, .T. ) ;
#80047 = CARTESIAN_POINT ( 'NONE',  ( 2.791683348922240793, 66.63393115100079456, 7.208316651077764092 ) ) ;
#80049 = CARTESIAN_POINT ( 'NONE',  ( -5.329506769333839600, -28.66963596002775816, -3.750000000000001332 ) ) ;
#80048 = CARTESIAN_POINT ( 'NONE',  ( 7.084665262690076126, 34.10535201082151247, 10.88017736071109987 ) ) ;
#80050 = DIRECTION ( 'NONE',  ( 0.000000000000000000, -1.000000000000000000, 0.000000000000000000 ) ) ;
#80051 = AXIS2_PLACEMENT_3D ( 'NONE', #13028, #42547, #88536 ) ;
#80052 = CARTESIAN_POINT ( 'NONE',  ( 22.81628187352648496, 41.83196800326375353, -3.434112377981050290 ) ) ;
#80053 = ORIENTED_EDGE ( 'NONE', *, *, #51059, .T. ) ;
#80054 = CARTESIAN_POINT ( 'NONE',  ( -0.8801773607111008646, 48.27201867748816966, 2.915334737309923430 ) ) ;
#80056 = CARTESIAN_POINT ( 'NONE',  ( 11.12471383767606525, 12.50000000000035527, 1.674288514511126591 ) ) ;
#80055 = CARTESIAN_POINT ( 'NONE',  ( 16.40814093676323893, 20.79030133659708923, 11.09922568453595026 ) ) ;
#80057 = FACE_OUTER_BOUND ( 'NONE', #59065, .T. ) ;
#80058 = CARTESIAN_POINT ( 'NONE',  ( 7.084665262690076126, 29.10535201082150181, 10.88017736071109987 ) ) ;
#80059 = CARTESIAN_POINT ( 'NONE',  ( 0.5774900079438590739, 2.647018677488171434, -5.440088680355550821 ) ) ;
#80060 = CARTESIAN_POINT ( 'NONE',  ( 5.076628168052704559, 45.17559781766745175, -8.527530157486179263 ) ) ;
#80061 = CARTESIAN_POINT ( 'NONE',  ( 7.084665262690076126, 69.10535201082151957, 10.88017736071109987 ) ) ;
#80062 = CARTESIAN_POINT ( 'NONE',  ( 7.084665262690076126, 59.10535201082150536, 10.88017736071109987 ) ) ;
#80063 = CARTESIAN_POINT ( 'NONE',  ( 0.000000000000000000, 15.00000000000000000, 0.000000000000000000 ) ) ;
#80064 = CARTESIAN_POINT ( 'NONE',  ( 13.79529636645031943, 35.34541550158063927, -14.16423886937409904 ) ) ;
#80065 = B_SPLINE_CURVE_WITH_KNOTS ( 'NONE', 3,
 ( #26686, #41717, #56699, #18713, #49675, #72186 ),
 .UNSPECIFIED., .F., .F.,
 ( 4, 2, 4 ),
 ( 0.0002800858945027856570, 0.0006862919646584887288, 0.001092498034814191801 ),
 .UNSPECIFIED. ) ;
#80066 = CIRCLE ( 'NONE', #67516, 15.00000000000000000 ) ;
#80067 = DIRECTION ( 'NONE',  ( -1.000000000000000000, -0.000000000000000000, -0.000000000000000000 ) ) ;
#80068 = ORIENTED_EDGE ( 'NONE', *, *, #5431, .T. ) ;
#80069 = CARTESIAN_POINT ( 'NONE',  ( 10.00000000000000178, 43.05374883491397497, 14.16423886937410082 ) ) ;
#80070 = CARTESIAN_POINT ( 'NONE',  ( 2.917880565312950480, 55.97041550158063217, -12.26659068614894821 ) ) ;
#80071 = CARTESIAN_POINT ( 'NONE',  ( 2.791683348922237240, 20.38393115100078745, -7.208316651077763204 ) ) ;
#80072 = CARTESIAN_POINT ( 'NONE',  ( 6.565887622018943937, 18.08196800326375708, -12.81628187352647608 ) ) ;
#80073 = DIRECTION ( 'NONE',  ( 0.6087614290087186575, 0.000000000000000000, 0.7933533402912366084 ) ) ;
#80074 = FACE_OUTER_BOUND ( 'NONE', #41734, .T. ) ;
#80076 = CARTESIAN_POINT ( 'NONE',  ( 10.00000000000000178, 35.37363466993042493, 12.81628187352647608 ) ) ;
#80075 = CARTESIAN_POINT ( 'NONE',  ( 7.084665262690076126, 2.022018677488170990, -10.88017736071110164 ) ) ;
#80077 = CARTESIAN_POINT ( 'NONE',  ( -0.3689425029237898834, 41.17874883491397497, -10.36894250292378850 ) ) ;
#80078 = DIRECTION ( 'NONE',  ( -0.5519369853120617009, 0.000000000000000000, 0.8338858220671657717 ) ) ;
#80079 = CARTESIAN_POINT ( 'NONE',  ( 19.84674366389459621, 8.508931151000785675, 7.409399052514197653E-17 ) ) ;
#80080 = EDGE_CURVE ( 'NONE', #71943, #32664, #32922, .T. ) ;
#80081 = CARTESIAN_POINT ( 'NONE',  ( 4.923371831947301658, 7.675597817667460632, 8.527530157486175710 ) ) ;
#80082 = ORIENTED_EDGE ( 'NONE', *, *, #1701, .F. ) ;
#80083 =( NAMED_UNIT ( * ) PLANE_ANGLE_UNIT ( ) SI_UNIT ( $, .RADIAN. ) );
#80084 = CARTESIAN_POINT ( 'NONE',  ( 7.361572987183169658, 19.96726448433411960, -9.846743663894592657 ) ) ;
#80085 = CARTESIAN_POINT ( 'NONE',  ( 66.56412365047464164, 14.00000000000000888, -9.500000000000000000 ) ) ;
#80086 = ORIENTED_EDGE ( 'NONE', *, *, #42026, .F. ) ;
#80088 = CARTESIAN_POINT ( 'NONE',  ( 2.035157376598824452, 23.68868534415484461, 7.964842623401179544 ) ) ;
#80087 = CARTESIAN_POINT ( 'NONE',  ( 15.44008868035555793, 6.397018677488171434, -9.422509992056140149 ) ) ;
#80090 = CARTESIAN_POINT ( 'NONE',  ( 16.40814093676324603, 2.456968003263753531, -11.09922568453594671 ) ) ;
#80089 = CARTESIAN_POINT ( 'NONE',  ( 17.20831665107776587, 44.13393115100078745, -7.208316651077762316 ) ) ;
#80091 =( GEOMETRIC_REPRESENTATION_CONTEXT ( 3 ) GLOBAL_UNCERTAINTY_ASSIGNED_CONTEXT ( ( #19430 ) ) GLOBAL_UNIT_ASSIGNED_CONTEXT ( ( #27753, #81255, #19277 ) ) REPRESENTATION_CONTEXT ( 'NONE', 'WORKASPACE' ) );
#80092 = CARTESIAN_POINT ( 'NONE',  ( 18.52753015748617571, 43.09226448433412315, 4.923371831947298993 ) ) ;
#80093 =( GEOMETRIC_REPRESENTATION_CONTEXT ( 3 ) GLOBAL_UNCERTAINTY_ASSIGNED_CONTEXT ( ( #29447 ) ) GLOBAL_UNIT_ASSIGNED_CONTEXT ( ( #97388, #88885, #4420 ) ) REPRESENTATION_CONTEXT ( 'NONE', 'WORKASPACE' ) );
#80094 = CARTESIAN_POINT ( 'NONE',  ( 0.6178305044545838731, 14.74863466993041783, 9.382169495545420901 ) ) ;
#80095 = VERTEX_POINT ( 'NONE', #71905 ) ;
#80096 = CARTESIAN_POINT ( 'NONE',  ( 17.08211943468705130, 58.47041550158063927, 12.26659068614894998 ) ) ;
#80097 = VERTEX_POINT ( 'NONE', #16952 ) ;
#80098 = CARTESIAN_POINT ( 'NONE',  ( -4.164238869374099927, 62.01208216824728936, 3.795296366450308767 ) ) ;
#80099 = VERTEX_POINT ( 'NONE', #93927 ) ;
#80100 = CARTESIAN_POINT ( 'NONE',  ( 0.5774900079438590739, 37.64701867748817676, -5.440088680355550821 ) ) ;
#80101 = CARTESIAN_POINT ( 'NONE',  ( 17.96484262340118221, 46.18868534415484106, -7.964842623401177768 ) ) ;
#80102 = CARTESIAN_POINT ( 'NONE',  ( 15.44008868035555793, 56.39701867748817676, -9.422509992056140149 ) ) ;
#80103 = DIRECTION ( 'NONE',  ( -0.4305110968082862533, 0.000000000000000000, -0.9025852843498647360 ) ) ;
#80104 = CARTESIAN_POINT ( 'NONE',  ( 12.91533473730992121, 44.52201867748816966, 10.88017736071110164 ) ) ;
#80105 =( NAMED_UNIT ( * ) SI_UNIT ( $, .STERADIAN. ) SOLID_ANGLE_UNIT ( ) );
#80106 = CIRCLE ( 'NONE', #24255, 0.09999999999999982514 ) ;
#80107 = CARTESIAN_POINT ( 'NONE',  ( 5.076628168052703671, 16.84226448433411960, 8.527530157486179263 ) ) ;
#80108 = ORIENTED_EDGE ( 'NONE', *, *, #53064, .T. ) ;
#80109 = CARTESIAN_POINT ( 'NONE',  ( 9.209315896096745391, -9.300848983894347555, 4.000000000000000000 ) ) ;
#80110 = CARTESIAN_POINT ( 'NONE',  ( 14.92337183194729633, 42.67559781766745886, 8.527530157486181039 ) ) ;
#80111 = CARTESIAN_POINT ( 'NONE',  ( 17.39651004071838969, 54.08210964143329846, -6.500000000000027534 ) ) ;
#80112 = CARTESIAN_POINT ( 'NONE',  ( 10.00000000000000178, 60.37363466993041783, 12.81628187352647608 ) ) ;
#80113 = AXIS2_PLACEMENT_3D ( 'NONE', #10858, #55868, #77864 ) ;
#80114 = FACE_OUTER_BOUND ( 'NONE', #19092, .T. ) ;
#80115 = CARTESIAN_POINT ( 'NONE',  ( 6.000000000000000000, 60.50000000000000711, 6.000000000000000000 ) ) ;
#80116 = CARTESIAN_POINT ( 'NONE',  ( -5.999999999999994671, 43.00000000000000000, 6.250000000000000000 ) ) ;
#80118 = CARTESIAN_POINT ( 'NONE',  ( 14.92337183194729633, 27.67559781766745530, 8.527530157486181039 ) ) ;
#80117 = CARTESIAN_POINT ( 'NONE',  ( 7.361572987183170547, 62.05059781766745886, 9.846743663894590881 ) ) ;
#80119 = CARTESIAN_POINT ( 'NONE',  ( 20.36894250292379738, 59.92874883491397497, -10.36894250292379027 ) ) ;
#80120 = DIRECTION ( 'NONE',  ( 0.08715574274765129636, 0.9961946980917462113, 0.000000000000000000 ) ) ;
#80121 = ORIENTED_EDGE ( 'NONE', *, *, #64138, .F. ) ;
#80123 =( GEOMETRIC_REPRESENTATION_CONTEXT ( 3 ) GLOBAL_UNCERTAINTY_ASSIGNED_CONTEXT ( ( #24130 ) ) GLOBAL_UNIT_ASSIGNED_CONTEXT ( ( #91066, #90082, #43597 ) ) REPRESENTATION_CONTEXT ( 'NONE', 'WORKASPACE' ) );
#80122 = CARTESIAN_POINT ( 'NONE',  ( 0.000000000000000000, 15.00000000000000000, 0.000000000000000000 ) ) ;
#80124 = CARTESIAN_POINT ( 'NONE',  ( 12.63842701281683034, 32.46726448433412315, 9.846743663894596210 ) ) ;
#80125 = CARTESIAN_POINT ( 'NONE',  ( 21.09922568453595559, 12.04030133659708746, -6.408140936763230044 ) ) ;
#80126 = CARTESIAN_POINT ( 'NONE',  ( 10.00000000000000000, -0.2410688489992152128, -9.846743663894594434 ) ) ;
#80127 = EDGE_CURVE ( 'NONE', #60118, #24768, #12997, .T. ) ;
#80128 = CARTESIAN_POINT ( 'NONE',  ( 11.62719953690061558, 14.49999999999999112, 9.476720473301933012 ) ) ;
#80129 = CARTESIAN_POINT ( 'NONE',  ( 18.52753015748617571, 13.09226448433411960, 4.923371831947298993 ) ) ;
#80130 = CARTESIAN_POINT ( 'NONE',  ( 10.00000000000000178, 52.25893115100078745, 9.846743663894594434 ) ) ;
#80131 = CARTESIAN_POINT ( 'NONE',  ( 20.88017736071110875, 20.77201867748816966, -2.915334737309920321 ) ) ;
#80132 = EDGE_CURVE ( 'NONE', #27691, #47516, #25453, .T. ) ;
#80133 = VERTEX_POINT ( 'NONE', #39944 ) ;
#80134 = CARTESIAN_POINT ( 'NONE',  ( 6.204703633549690345, 60.76208216824730357, -14.16423886937410259 ) ) ;
#80135 = CARTESIAN_POINT ( 'NONE',  ( 17.20831665107776587, 7.883931151000784787, 7.208316651077764980 ) ) ;
#80136 = CARTESIAN_POINT ( 'NONE',  ( 10.00000000000000178, 39.31368534415484106, 10.88017736071110342 ) ) ;
#80138 = CARTESIAN_POINT ( 'NONE',  ( 8.265815358934768042, 12.95537237636708916, -8.294953093294440194 ) ) ;
#80137 = CARTESIAN_POINT ( 'NONE',  ( 19.38216949554541202, 20.99863466993042138, 9.382169495545424454 ) ) ;
#80139 = CARTESIAN_POINT ( 'NONE',  ( 19.42250999205614548, 5.980352010821504471, -5.440088680355545492 ) ) ;
#80140 = CARTESIAN_POINT ( 'NONE',  ( 6.564124673094354101, -0.5742864948665229452, 2.900000000000000355 ) ) ;
#80141 = CARTESIAN_POINT ( 'NONE',  ( 19.90229974777923161, 0.3225724651664713671, -6.500000000000000000 ) ) ;
#80142 = CARTESIAN_POINT ( 'NONE',  ( 12.63842701281683034, 52.46726448433413026, 9.846743663894596210 ) ) ;
#80143 = CARTESIAN_POINT ( 'NONE',  ( 5.076628168052704559, 15.17559781766745175, -8.527530157486179263 ) ) ;
#80144 = CARTESIAN_POINT ( 'NONE',  ( 10.88017736071110519, -24.43631465584515539, -2.602085213965210642E-15 ) ) ;
#80145 = CARTESIAN_POINT ( 'NONE',  ( 22.81628187352647785, 26.41530133659708923, 3.434112377981063169 ) ) ;
#80146 = CARTESIAN_POINT ( 'NONE',  ( -10.85639882392407074, -98.10817599973766789, -3.750000000004759304 ) ) ;
#80147 = CARTESIAN_POINT ( 'NONE',  ( 12.91533473730993009, 31.60535201082150891, -10.88017736071109987 ) ) ;
#80148 = FACE_OUTER_BOUND ( 'NONE', #76567, .T. ) ;
#80149 = CARTESIAN_POINT ( 'NONE',  ( 22.26659068614895176, 44.72041550158063927, -7.082119434687042414 ) ) ;
#80150 = CARTESIAN_POINT ( 'NONE',  ( -0.3689425029237898834, 36.17874883491396787, -10.36894250292378850 ) ) ;
#80151 = CARTESIAN_POINT ( 'NONE',  ( 19.84674366389459266, 43.71726448433410894, -2.638427012816827677 ) ) ;
#80152 = CARTESIAN_POINT ( 'NONE',  ( 3.591859063236761518, 34.95696800326375353, 11.09922568453594849 ) ) ;
#80153 = CARTESIAN_POINT ( 'NONE',  ( -0.8801773607111009756, 23.06368534415484106, 1.068504757029289695E-15 ) ) ;
#80154 = PRESENTATION_LAYER_ASSIGNMENT (  '', '', ( #97751 ) ) ;
#80155 = CARTESIAN_POINT ( 'NONE',  ( 0.1532563361054100626, 45.80059781766745886, -2.638427012816831230 ) ) ;
#80156 = EDGE_CURVE ( 'NONE', #97107, #63207, #33400, .T. ) ;
#80157 = CARTESIAN_POINT ( 'NONE',  ( 20.88017736071110164, 40.35535201082150536, 2.915334737309930979 ) ) ;
#80158 = CARTESIAN_POINT ( 'NONE',  ( 21.09922568453595559, 2.040301336597086568, -6.408140936763230044 ) ) ;
#80159 = CARTESIAN_POINT ( 'NONE',  ( 17.08211943468705130, 38.47041550158063217, 12.26659068614894998 ) ) ;
#80160 = FACE_BOUND ( 'NONE', #24564, .T. ) ;
#80161 = UNCERTAINTY_MEASURE_WITH_UNIT (LENGTH_MEASURE( 1.000000000000000082E-05 ), #16742, 'distance_accuracy_value', 'NONE');
#80162 = EDGE_CURVE ( 'NONE', #68316, #21109, #18425, .T. ) ;
#80163 = CARTESIAN_POINT ( 'NONE',  ( 0.1532563361054100626, 30.80059781766744820, -2.638427012816831230 ) ) ;
#80164 =( NAMED_UNIT ( * ) PLANE_ANGLE_UNIT ( ) SI_UNIT ( $, .RADIAN. ) );
#80165 = CARTESIAN_POINT ( 'NONE',  ( 2.791683348922237240, 65.38393115100078035, -7.208316651077763204 ) ) ;
#80166 = ORIENTED_EDGE ( 'NONE', *, *, #59734, .F. ) ;
#80167 = CARTESIAN_POINT ( 'NONE',  ( 20.15039907845753575, 6.748846992468889638, 6.262539305110063736 ) ) ;
#80168 = CARTESIAN_POINT ( 'NONE',  ( 6.903457398626330566, -84.61157762779829739, 2.749999999999999556 ) ) ;
#80169 = CARTESIAN_POINT ( 'NONE',  ( 17.96484262340118221, 19.93868534415484106, 7.964842623401181321 ) ) ;
#80170 = CARTESIAN_POINT ( 'NONE',  ( 10.00000000000000178, 59.31368534415484106, 10.88017736071110342 ) ) ;
#80171 = CARTESIAN_POINT ( 'NONE',  ( 13.79529636645031943, 30.34541550158063927, -14.16423886937409904 ) ) ;
#80172 = CARTESIAN_POINT ( 'NONE',  ( 7.361572987183170547, 7.050597817667451750, 9.846743663894590881 ) ) ;
#80173 = CARTESIAN_POINT ( 'NONE',  ( 12.63842701281683034, 52.46726448433413026, 9.846743663894596210 ) ) ;
#80174 = CARTESIAN_POINT ( 'NONE',  ( -0.8801773607111008646, 28.27201867748817321, 2.915334737309923430 ) ) ;
#80175 = CARTESIAN_POINT ( 'NONE',  ( 3.753761956877525119, 0.000000000000000000, -3.955639745193192169 ) ) ;
#80176 = CARTESIAN_POINT ( 'NONE',  ( -44.43653038997627647, 105.4840905893460672, -5.301235023115286715 ) ) ;
#80177 = EDGE_LOOP ( 'NONE', ( #10711, #17827, #96514, #15188 ) ) ;
#80178 = ORIENTED_EDGE ( 'NONE', *, *, #26045, .F. ) ;
#80179 = ORIENTED_EDGE ( 'NONE', *, *, #1458, .T. ) ;
#80180 = LINE ( 'NONE', #64667, #51714 ) ;
#80181 = CARTESIAN_POINT ( 'NONE',  ( 2.917880565312950480, 10.97041550158063572, -12.26659068614894821 ) ) ;
#80182 = CARTESIAN_POINT ( 'NONE',  ( -2.266590686148945544, 6.387082168247300906, -7.082119434687050408 ) ) ;
#80183 = CARTESIAN_POINT ( 'NONE',  ( 13.79529636645031943, 60.34541550158063927, -14.16423886937409904 ) ) ;
#80184 = CARTESIAN_POINT ( 'NONE',  ( 14.92337183194729633, 52.67559781766745175, 8.527530157486181039 ) ) ;
#80185 = CARTESIAN_POINT ( 'NONE',  ( 14.92337183194729988, 39.34226448433412315, -8.527530157486177487 ) ) ;
#80186 = CARTESIAN_POINT ( 'NONE',  ( -0.3289641300568005855, 0.1049760357941743188, 5.963430220938281678 ) ) ;
#80188 = CARTESIAN_POINT ( 'NONE',  ( -2.816281873526471635, -1.084698663402913210, -3.434112377981056508 ) ) ;
#80187 = CARTESIAN_POINT ( 'NONE',  ( 7.084665262690076126, 27.02201867748817676, -10.88017736071110164 ) ) ;
#80189 = PRESENTATION_STYLE_ASSIGNMENT (( #96196 ) ) ;
#80190 = CARTESIAN_POINT ( 'NONE',  ( -0.3689425029237898834, 56.17874883491396076, -10.36894250292378850 ) ) ;
#80191 = STYLED_ITEM ( 'NONE', ( #22335 ), #23940 ) ;
#80192 = CARTESIAN_POINT ( 'NONE',  ( 7.084665262690076126, 2.022018677488171434, -10.88017736071110164 ) ) ;
#80193 = CARTESIAN_POINT ( 'NONE',  ( 19.84674366389459266, 38.30059781766745175, 2.638427012816836559 ) ) ;
#80194 = AXIS2_PLACEMENT_3D ( 'NONE', #95625, #18647, #41167 ) ;
#80195 = FACE_OUTER_BOUND ( 'NONE', #54256, .T. ) ;
#80196 = AXIS2_PLACEMENT_3D ( 'NONE', #80575, #12071, #30021 ) ;
#80197 = LINE ( 'NONE', #36180, #17465 ) ;
#80198 = ADVANCED_FACE ( 'NONE', ( #70447 ), #1964, .F. ) ;
#80199 = ORIENTED_EDGE ( 'NONE', *, *, #77014, .T. ) ;
#80200 = FILL_AREA_STYLE ('',( #64687 ) ) ;
#80201 = AXIS2_PLACEMENT_3D ( 'NONE', #51381, #81868, #73878 ) ;
#80202 = ORIENTED_EDGE ( 'NONE', *, *, #31726, .F. ) ;
#80203 = CARTESIAN_POINT ( 'NONE',  ( 12.63842701281683034, 27.46726448433411250, 9.846743663894596210 ) ) ;
#80204 = ORIENTED_EDGE ( 'NONE', *, *, #21324, .F. ) ;
#80205 = CARTESIAN_POINT ( 'NONE',  ( 2.917880565312948704, 32.63708216824730357, 12.26659068614894643 ) ) ;
#80206 = CARTESIAN_POINT ( 'NONE',  ( 17.20831665107776587, 39.13393115100079456, -7.208316651077762316 ) ) ;
#80207 = CARTESIAN_POINT ( 'NONE',  ( 12.91533473730993009, 51.60535201082149825, -10.88017736071109987 ) ) ;
#80208 = EDGE_CURVE ( 'NONE', #83598, #47034, #94439, .T. ) ;
#80209 = CARTESIAN_POINT ( 'NONE',  ( 20.10384461210893292, 36.74302437010793909, 6.337995344473749348 ) ) ;
#80210 = VECTOR ( 'NONE', #2251, 1000.000000000000000 ) ;
#80211 = CARTESIAN_POINT ( 'NONE',  ( 19.42250999205614193, 50.14701867748817676, 5.440088680355555262 ) ) ;
#80212 = CARTESIAN_POINT ( 'NONE',  ( -9.382169495545413795, 9.748634669930417829, 9.382169495545428006 ) ) ;
#80213 = ORIENTED_EDGE ( 'NONE', *, *, #91022, .T. ) ;
#80214 = CARTESIAN_POINT ( 'NONE',  ( 2.035157376598824452, 48.68868534415483396, 7.964842623401179544 ) ) ;
#80215 = CARTESIAN_POINT ( 'NONE',  ( 6.204703633549690345, 17.84541550158063217, 14.16423886937410082 ) ) ;
#80216 = ORIENTED_EDGE ( 'NONE', *, *, #43799, .T. ) ;
#80217 = ORIENTED_EDGE ( 'NONE', *, *, #45864, .T. ) ;
#80218 =( GEOMETRIC_REPRESENTATION_CONTEXT ( 3 ) GLOBAL_UNCERTAINTY_ASSIGNED_CONTEXT ( ( #62202 ) ) GLOBAL_UNIT_ASSIGNED_CONTEXT ( ( #21044, #4572, #89534 ) ) REPRESENTATION_CONTEXT ( 'NONE', 'WORKASPACE' ) );
#80219 = CARTESIAN_POINT ( 'NONE',  ( 19.38216949554541202, 45.99863466993041072, 9.382169495545424454 ) ) ;
#80220 = CARTESIAN_POINT ( 'NONE',  ( 12.91533473730992121, 19.52201867748816611, 10.88017736071110164 ) ) ;
#80221 = CARTESIAN_POINT ( 'NONE',  ( 0.1532563361054083140, 26.00893115100078745, 1.131784320476157264E-15 ) ) ;
#80222 = CARTESIAN_POINT ( 'NONE',  ( 7.084665262690076126, 7.022018677488169658, -10.88017736071110164 ) ) ;
#80223 = CARTESIAN_POINT ( 'NONE',  ( 22.81628187352647785, 56.62363466993042493, 6.195893100308588602E-16 ) ) ;
#80224 = CARTESIAN_POINT ( 'NONE',  ( -46.46849503609894327, 103.9079590269318629, -5.994465626570869787 ) ) ;
#80225 = CARTESIAN_POINT ( 'NONE',  ( 18.52753015748618282, 33.92559781766745886, -4.923371831947291888 ) ) ;
#80227 = ORIENTED_EDGE ( 'NONE', *, *, #54391, .F. ) ;
#80226 = CARTESIAN_POINT ( 'NONE',  ( 20.32896413005680003, 21.77164270246084143, 5.963430220938287007 ) ) ;
#80228 = CIRCLE ( 'NONE', #43466, 0.5000000000000004441 ) ;
#80229 = DIRECTION ( 'NONE',  ( 0.000000000000000000, -1.000000000000000000, -0.000000000000000000 ) ) ;
#80230 = FACE_OUTER_BOUND ( 'NONE', #8344, .T. ) ;
#80231 = CARTESIAN_POINT ( 'NONE',  ( -1.926860441876564023, 44.68830936912751639, 1.004413902775740781E-15 ) ) ;
#80232 = CARTESIAN_POINT ( 'NONE',  ( 12.63842701281683034, 7.467264484334118713, 9.846743663894596210 ) ) ;
#80233 = CARTESIAN_POINT ( 'NONE',  ( 0.6178305044545818747, 28.49863466993041783, -9.382169495545419124 ) ) ;
#80234 = CARTESIAN_POINT ( 'NONE',  ( 3.270119481323678468, 0.04922511925147240314, -14.38584091150421607 ) ) ;
#80235 = CARTESIAN_POINT ( 'NONE',  ( 7.361572987183169658, 39.96726448433411605, -9.846743663894592657 ) ) ;
#80236 = CARTESIAN_POINT ( 'NONE',  ( -11.10136736363541488, 0.04922511925147367295, 9.716261771424836269 ) ) ;
#80237 = CARTESIAN_POINT ( 'NONE',  ( 2.917880565312948704, 27.63708216824730357, 12.26659068614894643 ) ) ;
#80238 = CARTESIAN_POINT ( 'NONE',  ( 17.20831665107776587, 34.13393115100078745, -7.208316651077762316 ) ) ;
#80239 = CARTESIAN_POINT ( 'NONE',  ( 10.00000000000000000, 37.87363466993041783, -12.81628187352647608 ) ) ;
#80240 = B_SPLINE_CURVE_WITH_KNOTS ( 'NONE', 3,
 ( #80031, #73014, #90971, #51508, #45986, #97526 ),
 .UNSPECIFIED., .F., .F.,
 ( 4, 2, 4 ),
 ( 0.000000000000000000, 0.0002565770811490962521, 0.0005131541622981925042 ),
 .UNSPECIFIED. ) ;
#80242 = FILL_AREA_STYLE_COLOUR ( '', #62474 ) ;
#80241 = CARTESIAN_POINT ( 'NONE',  ( 0.000000000000000000, 99.99999999999998579, 8.000000000000000000 ) ) ;
#80243 = CARTESIAN_POINT ( 'NONE',  ( 0.5774900079438607392, 68.48035201082150536, 5.440088680355550821 ) ) ;
#80244 = CARTESIAN_POINT ( 'NONE',  ( 10.00000000000000178, 10.37363466993041961, 12.81628187352647608 ) ) ;
#80245 = CARTESIAN_POINT ( 'NONE',  ( 18.72515096720609051, 25.05509018479941119, 6.499999999999470646 ) ) ;
#80246 = CARTESIAN_POINT ( 'NONE',  ( 17.20831665107776587, 39.13393115100079456, -7.208316651077762316 ) ) ;
#80247 = CARTESIAN_POINT ( 'NONE',  ( 2.035157376598824452, 23.68868534415484461, 7.964842623401179544 ) ) ;
#80248 = ADVANCED_FACE ( 'NONE', ( #20395 ), #76882, .T. ) ;
#80249 = CARTESIAN_POINT ( 'NONE',  ( 6.565887622018943937, 25.16530133659708213, 12.81628187352647430 ) ) ;
#80250 = COLOUR_RGB ( '', 0.72549020, 0.75294118, 0.79215686) ;
#80251 = CARTESIAN_POINT ( 'NONE',  ( 2.791683348922237240, 35.38393115100079456, -7.208316651077763204 ) ) ;
#80252 = PRODUCT_CONTEXT ( 'NONE', #21905, 'mechanical' ) ;
#80253 = LINE ( 'NONE', #5258, #61413 ) ;
#80254 = CARTESIAN_POINT ( 'NONE',  ( 2.035157376598822676, 27.43868534415483396, -7.964842623401177768 ) ) ;
#80255 = VERTEX_POINT ( 'NONE', #4902 ) ;
#80256 = CIRCLE ( 'NONE', #49928, 0.7500000000000006661 ) ;
#80257 = LINE ( 'NONE', #89724, #40965 ) ;
#80258 = CARTESIAN_POINT ( 'NONE',  ( 0.5774900079438590739, 7.647018677488171434, -5.440088680355550821 ) ) ;
#80260 = CARTESIAN_POINT ( 'NONE',  ( 12.91533473730993009, 26.60535201082150536, -10.88017736071109987 ) ) ;
#80259 = CARTESIAN_POINT ( 'NONE',  ( 0.1532563361054082862, 61.21726448433412315, 2.638427012816831674 ) ) ;
#80261 = CARTESIAN_POINT ( 'NONE',  ( 0.000000000000000000, 15.00000000000000000, 0.000000000000000000 ) ) ;
#80262 = AXIS2_PLACEMENT_3D ( 'NONE', #22442, #68923, #52914 ) ;
#80263 = CARTESIAN_POINT ( 'NONE',  ( 2.035157376598824452, 48.68868534415483396, 7.964842623401179544 ) ) ;
#80265 = CARTESIAN_POINT ( 'NONE',  ( 8.879999999999991900, 76.07179676972447169, -4.250000000000000000 ) ) ;
#80264 = CARTESIAN_POINT ( 'NONE',  ( 17.96484262340118221, 24.93868534415484461, 7.964842623401181321 ) ) ;
#80266 = DIRECTION ( 'NONE',  ( 0.000000000000000000, -1.000000000000000000, 0.000000000000000000 ) ) ;
#80267 = B_SPLINE_CURVE_WITH_KNOTS ( 'NONE', 3,
 ( #68239, #38231, #61208, #54191, #84225, #1230 ),
 .UNSPECIFIED., .F., .F.,
 ( 4, 2, 4 ),
 ( 0.0002800032591452402829, 0.0006862085204419963568, 0.001092413781738752485 ),
 .UNSPECIFIED. ) ;
#80268 = DIRECTION ( 'NONE',  ( -1.000000000000000000, 0.000000000000000000, 0.000000000000000000 ) ) ;
#80269 = TOROIDAL_SURFACE ( 'NONE', #11608, 14.49999999999999822, 0.5000000000000000000 ) ;
#80270 = CARTESIAN_POINT ( 'NONE',  ( 14.92337183194729633, 47.67559781766745175, 8.527530157486181039 ) ) ;
#80271 = CARTESIAN_POINT ( 'NONE',  ( -4.164238869374099039, 46.80374883491397497, 8.674139862899312516E-16 ) ) ;
#80272 = CARTESIAN_POINT ( 'NONE',  ( 0.8719017118913388043, 123.9374316453451286, 5.000000000000000000 ) ) ;
#80273 = CARTESIAN_POINT ( 'NONE',  ( 24.16423886937410614, 14.30374883491396787, 8.672049930838204340E-16 ) ) ;
#80274 = CARTESIAN_POINT ( 'NONE',  ( 17.08211943468705130, 38.47041550158063217, 12.26659068614894998 ) ) ;
#80275 = CARTESIAN_POINT ( 'NONE',  ( 0.6178305044545838731, 4.748634669930420493, 9.382169495545420901 ) ) ;
#80276 = CARTESIAN_POINT ( 'NONE',  ( 11.49658347684016491, 14.95037108522383384, 9.245857368719866187 ) ) ;
#80277 = ORIENTED_EDGE ( 'NONE', *, *, #91447, .F. ) ;
#80278 = EDGE_CURVE ( 'NONE', #74063, #47699, #38065, .T. ) ;
#80279 = CARTESIAN_POINT ( 'NONE',  ( -2.266590686148945544, 61.38708216824730357, -7.082119434687050408 ) ) ;
#80280 = CARTESIAN_POINT ( 'NONE',  ( 1.472469842513823179, 30.59226448433411960, -4.923371831947296329 ) ) ;
#80281 = CARTESIAN_POINT ( 'NONE',  ( -12.98310705059825310, 90.76710648773774892, -7.614994760437855170 ) ) ;
#80282 = CARTESIAN_POINT ( 'NONE',  ( 20.88017736071110875, 55.77201867748816966, -2.915334737309920765 ) ) ;
#80283 = CARTESIAN_POINT ( 'NONE',  ( 0.000000000000000000, 81.99999999999992895, 5.000000000000000000 ) ) ;
#80284 = CARTESIAN_POINT ( 'NONE',  ( 20.88017736071110875, 25.77201867748816966, -2.915334737309920765 ) ) ;
#80285 = CARTESIAN_POINT ( 'NONE',  ( 10.00000000000000000, 62.87363466993042493, -12.81628187352647608 ) ) ;
#80286 = CARTESIAN_POINT ( 'NONE',  ( 16.40814093676323893, 25.79030133659708923, 11.09922568453595026 ) ) ;
#80287 = CARTESIAN_POINT ( 'NONE',  ( 5.076628168052704559, 25.17559781766745175, -8.527530157486179263 ) ) ;
#80289 = ORIENTED_EDGE ( 'NONE', *, *, #49771, .T. ) ;
#80288 = EDGE_CURVE ( 'NONE', #9175, #18711, #52386, .T. ) ;
#80290 = DIRECTION ( 'NONE',  ( 0.8338858220671735433, 0.000000000000000000, -0.5519369853120501546 ) ) ;
#80291 = CARTESIAN_POINT ( 'NONE',  ( 17.08211943468705130, 63.47041550158063927, 12.26659068614894998 ) ) ;
#80292 = CIRCLE ( 'NONE', #78735, 6.349999999999995204 ) ;
#80293 = CARTESIAN_POINT ( 'NONE',  ( 13.79529636645031943, 25.34541550158063572, -14.16423886937409904 ) ) ;
#80294 = CARTESIAN_POINT ( 'NONE',  ( 15.44008868035555793, 31.39701867748817676, -9.422509992056140149 ) ) ;
#80295 = CARTESIAN_POINT ( 'NONE',  ( 10.00000000000000178, 44.31368534415484106, 10.88017736071110342 ) ) ;
#80296 = LINE ( 'NONE', #4311, #35150 ) ;
#80297 = CARTESIAN_POINT ( 'NONE',  ( 19.84674366389459266, 48.30059781766745175, 2.638427012816836559 ) ) ;
#80298 = CARTESIAN_POINT ( 'NONE',  ( 2.791683348922240793, 11.63393115100078568, 7.208316651077764092 ) ) ;
#80299 = CYLINDRICAL_SURFACE ( 'NONE', #14669, 1.249999999999987121 ) ;
#80300 = FILL_AREA_STYLE_COLOUR ( '', #72319 ) ;
#80301 = CARTESIAN_POINT ( 'NONE',  ( 10.00000000000000178, 27.25893115100078390, 9.846743663894594434 ) ) ;
#80302 = CARTESIAN_POINT ( 'NONE',  ( 1.472469842513823179, 56.42559781766745886, 4.923371831947296329 ) ) ;
#80303 = CIRCLE ( 'NONE', #14879, 3.250000000000002665 ) ;
#80304 = ORIENTED_EDGE ( 'NONE', *, *, #47968, .F. ) ;
#80305 = CARTESIAN_POINT ( 'NONE',  ( -2.816281873526473856, 49.33196800326374643, 3.434112377981055619 ) ) ;
#80306 = LINE ( 'NONE', #42314, #70001 ) ;
#80307 = CARTESIAN_POINT ( 'NONE',  ( 2.035157376598824452, 68.68868534415484817, 7.964842623401179544 ) ) ;
#80308 = CARTESIAN_POINT ( 'NONE',  ( 1.472469842513823179, 31.42559781766745530, 4.923371831947296329 ) ) ;
#80310 = CARTESIAN_POINT ( 'NONE',  ( 1.472469842513823179, 25.59226448433412315, -4.923371831947296329 ) ) ;
#80309 = CARTESIAN_POINT ( 'NONE',  ( 10.00000000000000178, 53.05374883491396787, 14.16423886937410082 ) ) ;
#80311 = FACE_OUTER_BOUND ( 'NONE', #41748, .T. ) ;
#80312 = CARTESIAN_POINT ( 'NONE',  ( 0.1532563361054083140, 61.00893115100078745, 1.131784320476157264E-15 ) ) ;
#80313 = CARTESIAN_POINT ( 'NONE',  ( 13.79529636645030344, 23.26208216824730002, 14.16423886937410614 ) ) ;
#80314 = CARTESIAN_POINT ( 'NONE',  ( -4.164238869374099039, 36.80374883491396787, 8.674139862899312516E-16 ) ) ;
#80315 = CARTESIAN_POINT ( 'NONE',  ( 0.1532563361054082862, 46.21726448433411605, 2.638427012816831674 ) ) ;
#80316 = CARTESIAN_POINT ( 'NONE',  ( 20.15039907845753575, 12.62777174578613071, -6.262539305110077059 ) ) ;
#80317 = CARTESIAN_POINT ( 'NONE',  ( 12.91533473730992121, 24.52201867748816966, 10.88017736071110164 ) ) ;
#80318 = CARTESIAN_POINT ( 'NONE',  ( 7.084665262690076126, 64.10535201082150536, 10.88017736071109987 ) ) ;
#80319 = CARTESIAN_POINT ( 'NONE',  ( 18.72515096720579209, 51.07228050351030646, -6.499999999999869438 ) ) ;
#80320 = ORIENTED_EDGE ( 'NONE', *, *, #17873, .T. ) ;
#80321 = CARTESIAN_POINT ( 'NONE',  ( 19.38216949554541202, 50.99863466993042493, 9.382169495545424454 ) ) ;
#80322 = CARTESIAN_POINT ( 'NONE',  ( 2.035157376598824452, 58.68868534415482685, 7.964842623401179544 ) ) ;
#80323 = EDGE_LOOP ( 'NONE', ( #92907, #72841, #84363, #2273 ) ) ;
#80324 = DIRECTION ( 'NONE',  ( 0.6626200482157461602, 0.000000000000000000, -0.7489557207889945278 ) ) ;
#80325 = DIRECTION ( 'NONE',  ( 0.000000000000000000, 0.000000000000000000, -1.000000000000000000 ) ) ;
#80326 = EDGE_CURVE ( 'NONE', #27971, #48509, #86913, .T. ) ;
#80327 = CARTESIAN_POINT ( 'NONE',  ( -0.8801773607111008646, 58.27201867748816966, 2.915334737309923430 ) ) ;
#80328 =( GEOMETRIC_REPRESENTATION_CONTEXT ( 3 ) GLOBAL_UNCERTAINTY_ASSIGNED_CONTEXT ( ( #98298 ) ) GLOBAL_UNIT_ASSIGNED_CONTEXT ( ( #1384, #48321, #92355 ) ) REPRESENTATION_CONTEXT ( 'NONE', 'WORKASPACE' ) );
#80329 = VERTEX_POINT ( 'NONE', #58870 ) ;
#80330 = CARTESIAN_POINT ( 'NONE',  ( 17.96484262340118221, 59.93868534415484106, 7.964842623401181321 ) ) ;
#80331 = CARTESIAN_POINT ( 'NONE',  ( 10.00000000000000000, 16.81368534415483751, -10.88017736071110342 ) ) ;
#80332 = CARTESIAN_POINT ( 'NONE',  ( 13.61464873478166737, 15.00000000000000000, -6.296136897217838424 ) ) ;
#80333 = CARTESIAN_POINT ( 'NONE',  ( 20.15039907845753930, 0.07447313448805115144, 6.262539305110068177 ) ) ;
#80334 = CARTESIAN_POINT ( 'NONE',  ( 19.42250999205614193, 10.14701867748816966, 5.440088680355555262 ) ) ;
#80335 = CARTESIAN_POINT ( 'NONE',  ( 19.84674366389459621, 8.508931151000785675, 7.409399052514197653E-17 ) ) ;
#80336 = CARTESIAN_POINT ( 'NONE',  ( 17.08211943468705130, 18.47041550158063572, 12.26659068614894998 ) ) ;
#80337 = TOROIDAL_SURFACE ( 'NONE', #37242, 14.49999999999999822, 0.5000000000000000000 ) ;
#80338 = VECTOR ( 'NONE', #82348, 1000.000000000000000 ) ;
#80339 = CARTESIAN_POINT ( 'NONE',  ( -0.8801773607110991993, 22.85535201082150181, -2.915334737309923874 ) ) ;
#80340 = CARTESIAN_POINT ( 'NONE',  ( 19.84674366389459266, 63.71726448433412315, -2.638427012816827677 ) ) ;
#80341 = EDGE_LOOP ( 'NONE', ( #69976, #31489, #31640, #19064 ) ) ;
#80342 = CARTESIAN_POINT ( 'NONE',  ( 3.591859063236763294, -1.709698663402913210, -11.09922568453595026 ) ) ;
#80343 = ORIENTED_EDGE ( 'NONE', *, *, #8280, .T. ) ;
#80344 = DIRECTION ( 'NONE',  ( 0.000000000000000000, -1.000000000000000000, 0.000000000000000000 ) ) ;
#80345 = COLOUR_RGB ( '', 0.72549020, 0.75294118, 0.79215686) ;
#80346 = CARTESIAN_POINT ( 'NONE',  ( 2.035157376598822676, 52.43868534415483396, -7.964842623401177768 ) ) ;
#80347 = CARTESIAN_POINT ( 'NONE',  ( 12.63842701281683922, 49.55059781766744464, -9.846743663894590881 ) ) ;
#80348 = CARTESIAN_POINT ( 'NONE',  ( 22.81628187352647785, 41.62363466993042493, 6.195893100308588602E-16 ) ) ;
#80350 = CARTESIAN_POINT ( 'NONE',  ( -6.982525766850298687, -88.11956318484570261, -2.750000000000000444 ) ) ;
#80349 = CARTESIAN_POINT ( 'NONE',  ( 7.084665262690076126, 2.022018677488170990, -10.88017736071110164 ) ) ;
#80351 = CARTESIAN_POINT ( 'NONE',  ( 10.00000000000000000, 56.81368534415484106, -10.88017736071110342 ) ) ;
#80352 = CARTESIAN_POINT ( 'NONE',  ( -0.8801773607111008646, 3.272018677488171434, 2.915334737309923430 ) ) ;
#80353 = CARTESIAN_POINT ( 'NONE',  ( 22.81628187352647785, 36.62363466993041783, 6.195893100308588602E-16 ) ) ;
#80354 = CARTESIAN_POINT ( 'NONE',  ( 7.084665262690076126, 27.02201867748817676, -10.88017736071110164 ) ) ;
#80355 = LINE ( 'NONE', #82314, #53111 ) ;
#80356 = ORIENTED_EDGE ( 'NONE', *, *, #13420, .F. ) ;
#80357 = CARTESIAN_POINT ( 'NONE',  ( 0.6178305044545818747, 48.49863466993042493, -9.382169495545419124 ) ) ;
#80358 = CARTESIAN_POINT ( 'NONE',  ( 0.5774900079438607392, 33.48035201082150536, 5.440088680355550821 ) ) ;
#80359 = CARTESIAN_POINT ( 'NONE',  ( 14.92337183194729633, 62.67559781766745886, 8.527530157486181039 ) ) ;
#80360 = ORIENTED_EDGE ( 'NONE', *, *, #85898, .F. ) ;
#80361 = CARTESIAN_POINT ( 'NONE',  ( -7.674335239599376912, 14.76930270348882068, 12.81961907869210648 ) ) ;
#80362 = CARTESIAN_POINT ( 'NONE',  ( 0.000000000000000000, 14.49999999999999822, 0.000000000000000000 ) ) ;
#80363 = CARTESIAN_POINT ( 'NONE',  ( 0.1532563361054083140, 66.00893115100079456, 1.131784320476157264E-15 ) ) ;
#80365 = CARTESIAN_POINT ( 'NONE',  ( 19.84674366389459266, 53.71726448433411605, -2.638427012816827677 ) ) ;
#80364 = CARTESIAN_POINT ( 'NONE',  ( 10.27090289957528135, -3.182726299308032341E-15, 10.41235154178112055 ) ) ;
#80366 = CARTESIAN_POINT ( 'NONE',  ( 4.559911319644449179, 23.89701867748817321, 9.422509992056141925 ) ) ;
#80367 = CARTESIAN_POINT ( 'NONE',  ( 8.879999999999991900, 76.07179676972447169, -6.250000000000000000 ) ) ;
#80368 = DIRECTION ( 'NONE',  ( 0.9999619230641713097, 0.000000000000000000, 0.008726535498374267744 ) ) ;
#80369 = DIRECTION ( 'NONE',  ( 0.8870108331782150524, 0.000000000000000000, 0.4617486132350466788 ) ) ;
#80370 = TOROIDAL_SURFACE ( 'NONE', #37286, 14.49999999999999822, 0.5000000000000000000 ) ;
#80372 = CARTESIAN_POINT ( 'NONE',  ( 19.84674366389459266, 3.300597817667451750, 2.638427012816836559 ) ) ;
#80371 = CARTESIAN_POINT ( 'NONE',  ( 14.92337183194729633, 42.67559781766745886, 8.527530157486181039 ) ) ;
#80373 = CARTESIAN_POINT ( 'NONE',  ( 17.39651004071890128, 29.08210964143323096, -6.499999999999448441 ) ) ;
#80374 = ADVANCED_FACE ( 'NONE', ( #72390 ), #84121, .T. ) ;
#80376 = ORIENTED_EDGE ( 'NONE', *, *, #94068, .T. ) ;
#80375 = CARTESIAN_POINT ( 'NONE',  ( 1.472469842513823179, 61.42559781766745175, 4.923371831947296329 ) ) ;
#80377 = AXIS2_PLACEMENT_3D ( 'NONE', #15462, #54898, #37961 ) ;
#80378 = CARTESIAN_POINT ( 'NONE',  ( 10.00000000000000000, 37.87363466993041783, -12.81628187352647608 ) ) ;
#80379 = CARTESIAN_POINT ( 'NONE',  ( 10.00000000000000178, 47.25893115100078745, 9.846743663894594434 ) ) ;
#80380 = EDGE_CURVE ( 'NONE', #50878, #51412, #22891, .T. ) ;
#80382 = EDGE_CURVE ( 'NONE', #54853, #45554, #97915, .T. ) ;
#80381 = CARTESIAN_POINT ( 'NONE',  ( 20.36894250292379738, 64.92874883491397497, -10.36894250292379027 ) ) ;
#80383 = CARTESIAN_POINT ( 'NONE',  ( 12.63842701281683034, 37.46726448433411605, 9.846743663894596210 ) ) ;
#80384 = CARTESIAN_POINT ( 'NONE',  ( 8.879999999999991900, 18.00000000000000355, 2.900000000000000355 ) ) ;
#80385 = CARTESIAN_POINT ( 'NONE',  ( -2.266590686148945544, 57.22041550158063217, 7.082119434687048631 ) ) ;
#80386 = DIRECTION ( 'NONE',  ( 1.049065152435176504E-16, -1.000000000000000000, 0.000000000000000000 ) ) ;
#80387 = CARTESIAN_POINT ( 'NONE',  ( 4.559911319644449179, 2.230352010821504916, -9.422509992056141925 ) ) ;
#80388 = CARTESIAN_POINT ( 'NONE',  ( 10.00000000000000000, 30.55374883491397142, -14.16423886937410082 ) ) ;
#80390 = LINE ( 'NONE', #27377, #62153 ) ;
#80389 = CARTESIAN_POINT ( 'NONE',  ( 20.36894250292379738, 44.92874883491396787, -10.36894250292379027 ) ) ;
#80391 = CARTESIAN_POINT ( 'NONE',  ( 17.20831665107776587, 17.88393115100078745, 7.208316651077764980 ) ) ;
#80392 = EDGE_CURVE ( 'NONE', #26706, #49230, #36996, .T. ) ;
#80394 = CARTESIAN_POINT ( 'NONE',  ( -2.816281873526473856, -0.8763653300695799508, 9.499525473075851096E-16 ) ) ;
#80393 = CARTESIAN_POINT ( 'NONE',  ( 6.579634127946653699, -87.99828267815715321, 2.500000000000001332 ) ) ;
#80395 = ORIENTED_EDGE ( 'NONE', *, *, #57910, .F. ) ;
#80396 = CARTESIAN_POINT ( 'NONE',  ( 4.559911319644449179, 52.23035201082151247, -9.422509992056141925 ) ) ;
#80397 = CARTESIAN_POINT ( 'NONE',  ( 0.8952175423694606060, 18.52576239577081196, 5.990408912944278796 ) ) ;
#80398 = CARTESIAN_POINT ( 'NONE',  ( -0.3998276802501956606, 15.00000000000000000, -15.99117050944549234 ) ) ;
#80399 = CARTESIAN_POINT ( 'NONE',  ( 5.076628168052703671, 51.84226448433412315, 8.527530157486179263 ) ) ;
#80400 = CARTESIAN_POINT ( 'NONE',  ( 14.97687855664611867, 14.63606903414041227, 0.8325315005901734455 ) ) ;
#80402 = ADVANCED_FACE ( 'NONE', ( #41346 ), #85343, .T. ) ;
#80401 = ORIENTED_EDGE ( 'NONE', *, *, #91159, .T. ) ;
#80403 = COLOUR_RGB ( '', 0.40784314, 0.44705882, 0.49803922) ;
#80404 = CARTESIAN_POINT ( 'NONE',  ( -2.266590686148945544, 26.38708216824730357, -7.082119434687050408 ) ) ;
#80405 = CARTESIAN_POINT ( 'NONE',  ( 0.6076426042653101378, 37.37576471608601736, -6.499999999999992006 ) ) ;
#80407 = CYLINDRICAL_SURFACE ( 'NONE', #10547, 15.00000000000000000 ) ;
#80406 = CARTESIAN_POINT ( 'NONE',  ( -3.887834249412644994, -8.254296980873727207, -2.749999999999596767 ) ) ;
#80409 = AXIS2_PLACEMENT_3D ( 'NONE', #57604, #43590, #88594 ) ;
#80408 = CARTESIAN_POINT ( 'NONE',  ( 4.559911319644449179, 13.89701867748817321, 9.422509992056141925 ) ) ;
#80410 = CARTESIAN_POINT ( 'NONE',  ( 0.6178305044545838731, 19.74863466993042138, 9.382169495545420901 ) ) ;
#80411 = CARTESIAN_POINT ( 'NONE',  ( 21.92686044187656691, 62.18830936912750218, 4.562052436263911564E-16 ) ) ;
#80412 = CARTESIAN_POINT ( 'NONE',  ( 0.1532563361054100626, 15.80059781766745353, -2.638427012816831230 ) ) ;
#80413 = CARTESIAN_POINT ( 'NONE',  ( 13.43411237798106583, 52.66530133659708213, -12.81628187352647252 ) ) ;
#80415 = ADVANCED_FACE ( 'NONE', ( #62332 ), #70850, .F. ) ;
#80414 = EDGE_LOOP ( 'NONE', ( #69545, #22071, #1784, #57180 ) ) ;
#80416 =( GEOMETRIC_REPRESENTATION_CONTEXT ( 3 ) GLOBAL_UNCERTAINTY_ASSIGNED_CONTEXT ( ( #81474 ) ) GLOBAL_UNIT_ASSIGNED_CONTEXT ( ( #65515, #13012, #43509 ) ) REPRESENTATION_CONTEXT ( 'NONE', 'WORKASPACE' ) );
#80417 = CARTESIAN_POINT ( 'NONE',  ( 5.115475850227041654, -17.53855045868316154, -4.000000000006439294 ) ) ;
#80418 = CARTESIAN_POINT ( 'NONE',  ( -0.3689425029237881626, 32.42874883491395366, 10.36894250292379027 ) ) ;
#80419 = DIRECTION ( 'NONE',  ( 0.9426414910921736556, 0.000000000000000000, 0.3338068592337842255 ) ) ;
#80420 = CARTESIAN_POINT ( 'NONE',  ( -7.232415441807423129, -88.12698951299773853, 4.000000000000000000 ) ) ;
#80421 = CARTESIAN_POINT ( 'NONE',  ( 15.44008868035555793, 6.397018677488171434, -9.422509992056140149 ) ) ;
#80422 = DIRECTION ( 'NONE',  ( -0.000000000000000000, 1.000000000000000000, -0.000000000000000000 ) ) ;
#80423 = CARTESIAN_POINT ( 'NONE',  ( 12.58781651029204163, -3.396178602016116026E-15, -7.446837378630719151 ) ) ;
#80424 = CARTESIAN_POINT ( 'NONE',  ( 20.88017736071110875, 35.77201867748816966, -2.915334737309920765 ) ) ;
#80425 = CARTESIAN_POINT ( 'NONE',  ( 20.88017736071110875, 50.77201867748817676, -2.915334737309920765 ) ) ;
#80426 = CARTESIAN_POINT ( 'NONE',  ( 10.00000000000000000, 12.87363466993042138, -12.81628187352647608 ) ) ;
#80427 = CARTESIAN_POINT ( 'NONE',  ( 13.82671409943296226, 0.000000000000000000, -3.447387012295225261 ) ) ;
#80428 = CARTESIAN_POINT ( 'NONE',  ( 0.8952175423694350709, 3.525762395770809743, 5.990408912944235276 ) ) ;
#80429 = CARTESIAN_POINT ( 'NONE',  ( 2.791683348922240793, 6.633931151000785675, 7.208316651077764092 ) ) ;
#80430 = CARTESIAN_POINT ( 'NONE',  ( 15.44008868035555793, 41.39701867748817676, -9.422509992056140149 ) ) ;
#80431 = UNCERTAINTY_MEASURE_WITH_UNIT (LENGTH_MEASURE( 1.000000000000000082E-05 ), #77688, 'distance_accuracy_value', 'NONE');
#80432 = CARTESIAN_POINT ( 'NONE',  ( 0.6178305044545838731, -0.2513653300695798953, 9.382169495545420901 ) ) ;
#80433 = CARTESIAN_POINT ( 'NONE',  ( 19.42250999205614548, 60.98035201082151247, -5.440088680355545492 ) ) ;
#80434 = CARTESIAN_POINT ( 'NONE',  ( 14.92337183194729988, 19.34226448433411960, -8.527530157486177487 ) ) ;
#80435 = CARTESIAN_POINT ( 'NONE',  ( 19.38216949554541202, 50.99863466993042493, 9.382169495545424454 ) ) ;
#80436 = CARTESIAN_POINT ( 'NONE',  ( 19.84674366389459266, 3.300597817667451750, 2.638427012816836559 ) ) ;
#80437 = ORIENTED_EDGE ( 'NONE', *, *, #5113, .F. ) ;
#80438 = LINE ( 'NONE', #64914, #22974 ) ;
#80439 = CARTESIAN_POINT ( 'NONE',  ( 0.6081133539230469953, 28.33703382326400444, 6.499999999999966249 ) ) ;
#80440 = CARTESIAN_POINT ( 'NONE',  ( 12.91533473730993009, 26.60535201082150536, -10.88017736071109987 ) ) ;
#80442 = CARTESIAN_POINT ( 'NONE',  ( 24.16423886937409904, 24.09541550158063927, 3.795296366450317205 ) ) ;
#80441 = DIRECTION ( 'NONE',  ( -1.000000000000000000, 0.000000000000000000, 0.000000000000000000 ) ) ;
#80443 = CARTESIAN_POINT ( 'NONE',  ( 1.472469842513823179, 36.42559781766745175, 4.923371831947296329 ) ) ;
#80444 = CARTESIAN_POINT ( 'NONE',  ( 20.88017736071110519, 15.56368534415483751, 2.639326808657452039E-16 ) ) ;
#80445 = CARTESIAN_POINT ( 'NONE',  ( 2.917880565312950480, 65.97041550158063217, -12.26659068614894821 ) ) ;
#80446 = VERTEX_POINT ( 'NONE', #1871 ) ;
#80447 = CARTESIAN_POINT ( 'NONE',  ( 10.00000000000000000, 11.81368534415483751, -10.88017736071110342 ) ) ;
#80448 = EDGE_CURVE ( 'NONE', #92377, #45159, #60895, .T. ) ;
#80449 = CARTESIAN_POINT ( 'NONE',  ( 19.42250999205614548, 30.98035201082150536, -5.440088680355545492 ) ) ;
#80451 = CARTESIAN_POINT ( 'NONE',  ( 10.00000000000000000, 31.81368534415483751, -10.88017736071110342 ) ) ;
#80450 = DIRECTION ( 'NONE',  ( -6.217248937900876626E-14, 0.000000000000000000, 1.000000000000000000 ) ) ;
#80452 = ORIENTED_EDGE ( 'NONE', *, *, #34219, .T. ) ;
#80453 = CARTESIAN_POINT ( 'NONE',  ( 0.1532563361054100626, 65.80059781766745175, -2.638427012816831230 ) ) ;
#80454 = CARTESIAN_POINT ( 'NONE',  ( 7.084665262690076126, 27.02201867748817676, -10.88017736071110164 ) ) ;
#80455 = DIRECTION ( 'NONE',  ( 1.000000000000000000, 0.000000000000000000, 0.000000000000000000 ) ) ;
#80456 = CARTESIAN_POINT ( 'NONE',  ( 19.38216949554541557, 57.24863466993042493, -9.382169495545420901 ) ) ;
#80457 = CYLINDRICAL_SURFACE ( 'NONE', #65165, 15.00000000000000000 ) ;
#80458 = CARTESIAN_POINT ( 'NONE',  ( 24.16423886937410614, 29.51208216824729647, -3.795296366450302550 ) ) ;
#80459 = CARTESIAN_POINT ( 'NONE',  ( 20.88017736071110519, 35.56368534415484106, 2.639326808657452039E-16 ) ) ;
#80460 = CARTESIAN_POINT ( 'NONE',  ( 2.035157376598822676, 12.43868534415483751, -7.964842623401177768 ) ) ;
#80461 = CARTESIAN_POINT ( 'NONE',  ( 0.000000000000000000, 14.49999999999999822, 0.000000000000000000 ) ) ;
#80462 = CARTESIAN_POINT ( 'NONE',  ( -8.000000608138725156, -0.01989113958122736350, -3.750000000000000888 ) ) ;
#80463 = CARTESIAN_POINT ( 'NONE',  ( 14.92337183194729633, 47.67559781766745175, 8.527530157486181039 ) ) ;
#80464 = CARTESIAN_POINT ( 'NONE',  ( 1.472469842513823179, 21.42559781766745175, 4.923371831947296329 ) ) ;
#80465 = CARTESIAN_POINT ( 'NONE',  ( 12.81628187352647608, -33.37636533006957507, -2.602085213965210642E-15 ) ) ;
#80466 = CARTESIAN_POINT ( 'NONE',  ( 15.44008868035555793, 16.39701867748817321, -9.422509992056140149 ) ) ;
#80467 = CARTESIAN_POINT ( 'NONE',  ( 2.791683348922240793, 16.63393115100078745, 7.208316651077764092 ) ) ;
#80468 = CARTESIAN_POINT ( 'NONE',  ( 10.00000000000000178, 10.37363466993041961, 12.81628187352647608 ) ) ;
#80470 = CARTESIAN_POINT ( 'NONE',  ( 15.44008868035555793, 51.39701867748816966, -9.422509992056140149 ) ) ;
#80469 = CARTESIAN_POINT ( 'NONE',  ( -0.8801773607110991993, 57.85535201082149825, -2.915334737309923874 ) ) ;
#80472 = CARTESIAN_POINT ( 'NONE',  ( 19.38216949554541557, 62.24863466993041072, -9.382169495545420901 ) ) ;
#80471 = CARTESIAN_POINT ( 'NONE',  ( 17.96484262340118221, 16.18868534415483396, -7.964842623401177768 ) ) ;
#80473 = CARTESIAN_POINT ( 'NONE',  ( 6.204703633549690345, 30.76208216824730357, -14.16423886937410259 ) ) ;
#80474 = FILL_AREA_STYLE ('',( #87963 ) ) ;
#80475 = B_SPLINE_CURVE_WITH_KNOTS ( 'NONE', 3,
 ( #72073, #47608, #85611, #55609 ),
 .UNSPECIFIED., .F., .F.,
 ( 4, 4 ),
 ( 3.878959614448864246E-18, 0.002562518741975557991 ),
 .UNSPECIFIED. ) ;
#80476 = VECTOR ( 'NONE', #42202, 1000.000000000000114 ) ;
#80477 = CARTESIAN_POINT ( 'NONE',  ( 16.40814093676324603, 62.45696800326376064, -11.09922568453594671 ) ) ;
#80478 = EDGE_LOOP ( 'NONE', ( #65836, #43448, #28114, #83628 ) ) ;
#80479 = CARTESIAN_POINT ( 'NONE',  ( 0.1532563361054083140, 66.00893115100079456, 1.131784320476157264E-15 ) ) ;
#80480 = CARTESIAN_POINT ( 'NONE',  ( 19.72487221294571569, 20.71833443783938122, -6.499999999999990230 ) ) ;
#80481 = CARTESIAN_POINT ( 'NONE',  ( 7.084665262690076126, 32.02201867748816966, -10.88017736071110164 ) ) ;
#80482 = CARTESIAN_POINT ( 'NONE',  ( 5.076628168052703671, 66.84226448433412315, 8.527530157486179263 ) ) ;
#80483 = AXIS2_PLACEMENT_3D ( 'NONE', #21752, #98757, #37250 ) ;
#80484 = ORIENTED_EDGE ( 'NONE', *, *, #77918, .T. ) ;
#80486 = CARTESIAN_POINT ( 'NONE',  ( -12.34557190004687044, 0.04922511925147153578, 8.076692058882407821 ) ) ;
#80485 = CARTESIAN_POINT ( 'NONE',  ( 2.791683348922240793, 16.63393115100078745, 7.208316651077764092 ) ) ;
#80487 = CARTESIAN_POINT ( 'NONE',  ( 7.361572987183169658, 9.967264484334119601, -9.846743663894592657 ) ) ;
#80488 = CARTESIAN_POINT ( 'NONE',  ( 0.1532563361054100626, 25.80059781766744820, -2.638427012816831230 ) ) ;
#80489 = ADVANCED_FACE ( 'NONE', ( #48809 ), #1381, .T. ) ;
#80490 = CARTESIAN_POINT ( 'NONE',  ( 7.361572987183169658, 14.96726448433411960, -9.846743663894592657 ) ) ;
#80491 = CARTESIAN_POINT ( 'NONE',  ( 5.076628168052704559, 0.1755978176674514724, -8.527530157486179263 ) ) ;
#80493 = CARTESIAN_POINT ( 'NONE',  ( -18.89999999999999503, 98.99999999999998579, 7.750000000000000000 ) ) ;
#80492 = CARTESIAN_POINT ( 'NONE',  ( 2.035157376598822676, 52.43868534415483396, -7.964842623401177768 ) ) ;
#80494 = CARTESIAN_POINT ( 'NONE',  ( 0.1532563361054082862, 1.217264484334117824, 2.638427012816831674 ) ) ;
#80496 = ORIENTED_EDGE ( 'NONE', *, *, #72367, .T. ) ;
#80495 = CARTESIAN_POINT ( 'NONE',  ( 19.84674366389459621, 23.50893115100078390, 7.409399052514197653E-17 ) ) ;
#80497 = EDGE_CURVE ( 'NONE', #23460, #37318, #39107, .T. ) ;
#80498 = CARTESIAN_POINT ( 'NONE',  ( 0.000000000000000000, 14.49999999999999822, 0.000000000000000000 ) ) ;
#80499 = CARTESIAN_POINT ( 'NONE',  ( 3.591859063236763294, -1.709698663402913210, -11.09922568453595026 ) ) ;
#80500 = ORIENTED_EDGE ( 'NONE', *, *, #40282, .F. ) ;
#80501 = ORIENTED_EDGE ( 'NONE', *, *, #23207, .F. ) ;
#80502 = EDGE_CURVE ( 'NONE', #28519, #36015, #17799, .T. ) ;
#80504 = ADVANCED_FACE ( 'NONE', ( #11798 ), #80299, .F. ) ;
#80503 = CARTESIAN_POINT ( 'NONE',  ( 22.26659068614895176, 14.72041550158063572, -7.082119434687042414 ) ) ;
#80505 = UNCERTAINTY_MEASURE_WITH_UNIT (LENGTH_MEASURE( 1.000000000000000082E-05 ), #8290, 'distance_accuracy_value', 'NONE');
#80506 = DIRECTION ( 'NONE',  ( 1.000000000000000000, 0.000000000000000000, 0.000000000000000000 ) ) ;
#80507 = CARTESIAN_POINT ( 'NONE',  ( 24.16423886937410614, 19.51208216824729647, -3.795296366450302550 ) ) ;
#80508 = CARTESIAN_POINT ( 'NONE',  ( 24.16423886937410614, 34.30374883491396787, 8.672049930838204340E-16 ) ) ;
#80509 = FILL_AREA_STYLE ('',( #85551 ) ) ;
#80510 = CARTESIAN_POINT ( 'NONE',  ( 17.96484262340118221, 36.18868534415484106, -7.964842623401177768 ) ) ;
#80511 = ORIENTED_EDGE ( 'NONE', *, *, #49332, .F. ) ;
#80512 = CARTESIAN_POINT ( 'NONE',  ( 19.84674366389459621, 18.50893115100078745, 7.409399052514197653E-17 ) ) ;
#80514 = CARTESIAN_POINT ( 'NONE',  ( 0.1532563361054100626, 15.80059781766745353, -2.638427012816831230 ) ) ;
#80513 = CARTESIAN_POINT ( 'NONE',  ( 7.084665262690076126, 62.02201867748816966, -10.88017736071110164 ) ) ;
#80515 = ADVANCED_FACE ( 'NONE', ( #59262 ), #89763, .F. ) ;
#80516 = CARTESIAN_POINT ( 'NONE',  ( 12.91533473730993009, 6.605352010821504471, -10.88017736071109987 ) ) ;
#80517 = CARTESIAN_POINT ( 'NONE',  ( 0.6178305044545838731, 39.74863466993041072, 9.382169495545420901 ) ) ;
#80518 = CARTESIAN_POINT ( 'NONE',  ( 0.1532563361054100626, 55.80059781766745175, -2.638427012816831230 ) ) ;
#80519 = DIRECTION ( 'NONE',  ( 1.084202172485504681E-16, 1.000000000000000000, 0.000000000000000000 ) ) ;
#80520 = CARTESIAN_POINT ( 'NONE',  ( 6.565887622018943937, 30.16530133659708568, 12.81628187352647430 ) ) ;
#80521 = CARTESIAN_POINT ( 'NONE',  ( -3.795296366450322534, -29.23791783175269288, -14.16423886937409904 ) ) ;
#80522 = CARTESIAN_POINT ( 'NONE',  ( 19.84674366389459266, 33.30059781766744464, 2.638427012816836559 ) ) ;
#80523 = CARTESIAN_POINT ( 'NONE',  ( 17.08211943468705130, 18.47041550158063572, 12.26659068614894998 ) ) ;
#80524 = VERTEX_POINT ( 'NONE', #95296 ) ;
#80525 = DIRECTION ( 'NONE',  ( -1.000000000000000000, -0.000000000000000000, -0.000000000000000000 ) ) ;
#80526 = CARTESIAN_POINT ( 'NONE',  ( -0.8801773607111008646, 53.27201867748816966, 2.915334737309923430 ) ) ;
#80527 = CARTESIAN_POINT ( 'NONE',  ( 10.00000000000000178, 59.31368534415484106, 10.88017736071110342 ) ) ;
#80528 = CARTESIAN_POINT ( 'NONE',  ( 13.79529636645031943, 45.34541550158062506, -14.16423886937409904 ) ) ;
#80529 = CARTESIAN_POINT ( 'NONE',  ( 0.1532563361054100626, 60.80059781766744464, -2.638427012816831230 ) ) ;
#80530 = CARTESIAN_POINT ( 'NONE',  ( -0.6999999999999957367, 99.99999999999998579, -8.525133428036873795 ) ) ;
#80531 = CARTESIAN_POINT ( 'NONE',  ( 10.00000000000000000, 36.81368534415484106, -10.88017736071110342 ) ) ;
#80532 = EDGE_CURVE ( 'NONE', #84166, #58317, #27781, .T. ) ;
#80533 = CARTESIAN_POINT ( 'NONE',  ( -4.010384638568479154, -13.83464189901983232, -2.500000000000000444 ) ) ;
#80534 = CARTESIAN_POINT ( 'NONE',  ( 7.361572987183170547, 57.05059781766744464, 9.846743663894590881 ) ) ;
#80535 = CARTESIAN_POINT ( 'NONE',  ( -10.88017736071110342, 13.06368534415484817, 3.903127820947815962E-15 ) ) ;
#80536 = CARTESIAN_POINT ( 'NONE',  ( 17.96484262340118221, 4.938685344154837509, 7.964842623401181321 ) ) ;
#80537 = CARTESIAN_POINT ( 'NONE',  ( 7.084665262690076126, 67.02201867748817676, -10.88017736071110164 ) ) ;
#80538 = CARTESIAN_POINT ( 'NONE',  ( -0.8801773607110991993, 2.855352010821504471, -2.915334737309923874 ) ) ;
#80540 = EDGE_CURVE ( 'NONE', #6847, #26894, #35333, .T. ) ;
#80539 = CARTESIAN_POINT ( 'NONE',  ( 4.469999999999999751, 10.25000000000000000, 3.750000000000000000 ) ) ;
#80541 = CARTESIAN_POINT ( 'NONE',  ( 17.20831665107776587, 4.133931151000785675, -7.208316651077762316 ) ) ;
#80542 = CARTESIAN_POINT ( 'NONE',  ( 12.63842701281683922, 4.550597817667451750, -9.846743663894590881 ) ) ;
#80543 = CARTESIAN_POINT ( 'NONE',  ( 18.00000000000000000, 78.06026162106621769, -3.869897288747938369 ) ) ;
#80544 =( GEOMETRIC_REPRESENTATION_CONTEXT ( 3 ) GLOBAL_UNCERTAINTY_ASSIGNED_CONTEXT ( ( #89476 ) ) GLOBAL_UNIT_ASSIGNED_CONTEXT ( ( #86410, #94879, #33863 ) ) REPRESENTATION_CONTEXT ( 'NONE', 'WORKASPACE' ) );
#80545 = CARTESIAN_POINT ( 'NONE',  ( 7.361572987183169658, 29.96726448433411960, -9.846743663894592657 ) ) ;
#80546 = CARTESIAN_POINT ( 'NONE',  ( -0.8801773607111008646, 18.27201867748817321, 2.915334737309923430 ) ) ;
#80547 = CARTESIAN_POINT ( 'NONE',  ( 10.00000000000000178, 5.373634669930420493, 12.81628187352647608 ) ) ;
#80549 = CARTESIAN_POINT ( 'NONE',  ( 19.72487221294570858, 36.86607318730075633, 6.500000000000000888 ) ) ;
#80548 = CARTESIAN_POINT ( 'NONE',  ( 19.42250999205614193, 35.14701867748816966, 5.440088680355555262 ) ) ;
#80550 = FACE_OUTER_BOUND ( 'NONE', #60770, .T. ) ;
#80551 = CARTESIAN_POINT ( 'NONE',  ( 21.09922568453595559, 32.04030133659708923, -6.408140936763230044 ) ) ;
#80552 = VERTEX_POINT ( 'NONE', #12290 ) ;
#80553 = CARTESIAN_POINT ( 'NONE',  ( 4.559911319644449179, 68.89701867748817676, 9.422509992056141925 ) ) ;
#80554 = VECTOR ( 'NONE', #86563, 1000.000000000000000 ) ;
#80555 = B_SPLINE_CURVE_WITH_KNOTS ( 'NONE', 3,
 ( #48217, #69267, #71232, #33211, #63705, #23283 ),
 .UNSPECIFIED., .F., .F.,
 ( 4, 2, 4 ),
 ( 3.409110551496104263E-05, 0.0004400426677367865174, 0.0008459942299586119176 ),
 .UNSPECIFIED. ) ;
#80557 = CARTESIAN_POINT ( 'NONE',  ( 19.72487221294570858, 51.86607318730076344, 6.500000000000000888 ) ) ;
#80556 = CARTESIAN_POINT ( 'NONE',  ( 13.43411237798105340, 20.58196800326374643, 12.81628187352647963 ) ) ;
#80558 = CARTESIAN_POINT ( 'NONE',  ( 0.000000000000000000, 15.00000000000000000, 0.000000000000000000 ) ) ;
#80559 = CARTESIAN_POINT ( 'NONE',  ( 20.88017736071110519, 25.56368534415483751, 2.639326808657452039E-16 ) ) ;
#80560 = CARTESIAN_POINT ( 'NONE',  ( 6.204703633549690345, 67.84541550158060375, 14.16423886937410082 ) ) ;
#80561 = CARTESIAN_POINT ( 'NONE',  ( 2.791683348922237240, 60.38393115100078745, -7.208316651077763204 ) ) ;
#80562 = CARTESIAN_POINT ( 'NONE',  ( 14.92337183194729988, 9.342264484334119601, -8.527530157486177487 ) ) ;
#80563 = CARTESIAN_POINT ( 'NONE',  ( 2.035157376598822676, 57.43868534415484106, -7.964842623401177768 ) ) ;
#80564 = DIRECTION ( 'NONE',  ( 0.000000000000000000, 1.000000000000000000, 0.000000000000000000 ) ) ;
#80565 = CARTESIAN_POINT ( 'NONE',  ( -4.164238869374098151, 36.59541550158063217, -3.795296366450310543 ) ) ;
#80566 = DIRECTION ( 'NONE',  ( 1.000000000000000000, 0.000000000000000000, -0.000000000000000000 ) ) ;
#80567 = CARTESIAN_POINT ( 'NONE',  ( -3.750000000000000888, 1.019547802438453887, -4.000000000000000000 ) ) ;
#80568 = ORIENTED_EDGE ( 'NONE', *, *, #10179, .T. ) ;
#80569 = ORIENTED_EDGE ( 'NONE', *, *, #52851, .F. ) ;
#80570 = CARTESIAN_POINT ( 'NONE',  ( 13.79529636645030344, 48.26208216824728936, 14.16423886937410614 ) ) ;
#80571 = CARTESIAN_POINT ( 'NONE',  ( -2.266590686148945544, 51.38708216824730357, -7.082119434687050408 ) ) ;
#80572 = CARTESIAN_POINT ( 'NONE',  ( 12.63842701281683034, 22.46726448433411605, 9.846743663894596210 ) ) ;
#80573 = CARTESIAN_POINT ( 'NONE',  ( 22.81628187352647785, 26.41530133659708923, 3.434112377981063169 ) ) ;
#80574 = CARTESIAN_POINT ( 'NONE',  ( -13.72572134032981062, 90.95701465610191860, 7.926449989681190189 ) ) ;
#80575 = CARTESIAN_POINT ( 'NONE',  ( 0.000000000000000000, 0.000000000000000000, 0.000000000000000000 ) ) ;
#80576 = CARTESIAN_POINT ( 'NONE',  ( 10.00000000000000178, 69.31368534415484817, 10.88017736071110342 ) ) ;
#80577 = CARTESIAN_POINT ( 'NONE',  ( -4.164238869374098151, 41.59541550158061796, -3.795296366450310543 ) ) ;
#80578 = CARTESIAN_POINT ( 'NONE',  ( 10.04755927614752942, -3.129363223631011419E-15, -10.62803196998856592 ) ) ;
#80579 = CARTESIAN_POINT ( 'NONE',  ( 12.63842701281683922, 14.55059781766744997, -9.846743663894590881 ) ) ;
#80580 = CARTESIAN_POINT ( 'NONE',  ( 9.846743663894590881, -1.282735515665884174, -2.638427012816833894 ) ) ;
#80581 = EDGE_CURVE ( 'NONE', #62017, #28374, #8300, .T. ) ;
#80582 = VERTEX_POINT ( 'NONE', #58774 ) ;
#80583 = FILL_AREA_STYLE ('',( #42105 ) ) ;
#80584 = ORIENTED_EDGE ( 'NONE', *, *, #93514, .F. ) ;
#80585 = CARTESIAN_POINT ( 'NONE',  ( 0.000000000000000000, 15.00000000000000000, 0.000000000000000000 ) ) ;
#80586 = ORIENTED_EDGE ( 'NONE', *, *, #63911, .T. ) ;
#80587 = CARTESIAN_POINT ( 'NONE',  ( 17.08211943468705840, 10.13708216824730179, -12.26659068614894466 ) ) ;
#80589 = CARTESIAN_POINT ( 'NONE',  ( 12.91533473730992121, 24.52201867748816966, 10.88017736071110164 ) ) ;
#80588 = CARTESIAN_POINT ( 'NONE',  ( 17.96484262340118221, 26.18868534415483396, -7.964842623401177768 ) ) ;
#80591 = CARTESIAN_POINT ( 'NONE',  ( 22.81628187352647785, 11.41530133659708390, 3.434112377981063169 ) ) ;
#80590 = CARTESIAN_POINT ( 'NONE',  ( 0.1532563361054100626, 50.80059781766745175, -2.638427012816831230 ) ) ;
#80592 = CYLINDRICAL_SURFACE ( 'NONE', #64636, 11.92686044187656513 ) ;
#80594 = EDGE_CURVE ( 'NONE', #35183, #20515, #11499, .T. ) ;
#80593 = CIRCLE ( 'NONE', #47098, 6.999999999999995559 ) ;
#80595 = CARTESIAN_POINT ( 'NONE',  ( -1.099225684535947600, 24.54030133659708923, 6.408140936763237150 ) ) ;
#80596 = ORIENTED_EDGE ( 'NONE', *, *, #20438, .T. ) ;
#80597 = CARTESIAN_POINT ( 'NONE',  ( 7.361572987183169658, 24.96726448433412315, -9.846743663894592657 ) ) ;
#80598 = CARTESIAN_POINT ( 'NONE',  ( 20.36894250292379382, 53.67874883491397497, 10.36894250292379205 ) ) ;
#80599 = VERTEX_POINT ( 'NONE', #42799 ) ;
#80600 = CARTESIAN_POINT ( 'NONE',  ( 2.917880565312948704, 67.63708216824730357, 12.26659068614894643 ) ) ;
#80601 = ORIENTED_EDGE ( 'NONE', *, *, #62641, .F. ) ;
#80602 = CARTESIAN_POINT ( 'NONE',  ( 12.91533473730992121, 34.52201867748817676, 10.88017736071110164 ) ) ;
#80603 = CARTESIAN_POINT ( 'NONE',  ( -0.8801773607111008646, 48.27201867748816966, 2.915334737309923430 ) ) ;
#80604 = CARTESIAN_POINT ( 'NONE',  ( 0.5774900079438590739, 57.64701867748817676, -5.440088680355550821 ) ) ;
#80605 = CIRCLE ( 'NONE', #79026, 15.00000000000000000 ) ;
#80606 = CARTESIAN_POINT ( 'NONE',  ( 18.00000000000000355, 77.07179676972445748, -4.250000000000000000 ) ) ;
#80607 = CARTESIAN_POINT ( 'NONE',  ( 15.44008868035555793, 46.39701867748817676, -9.422509992056140149 ) ) ;
#80608 = CARTESIAN_POINT ( 'NONE',  ( -6.336100170401012477, 14.76984879808201434, 13.53056138701883881 ) ) ;
#80610 = ORIENTED_EDGE ( 'NONE', *, *, #58802, .T. ) ;
#80609 = DIRECTION ( 'NONE',  ( 1.000000000000000000, 2.107602052970794797E-16, -0.000000000000000000 ) ) ;
#80611 = EDGE_CURVE ( 'NONE', #45739, #63730, #3330, .T. ) ;
#80612 = B_SPLINE_CURVE_WITH_KNOTS ( 'NONE', 3,
 ( #6873, #76833, #22380, #38362, #22874, #7867 ),
 .UNSPECIFIED., .F., .F.,
 ( 4, 2, 4 ),
 ( 0.0002800760588349135915, 0.0006862820326511982327, 0.001092488006467482982 ),
 .UNSPECIFIED. ) ;
#80613 = CARTESIAN_POINT ( 'NONE',  ( 14.92337183194729633, 17.67559781766745175, 8.527530157486181039 ) ) ;
#80614 = ORIENTED_EDGE ( 'NONE', *, *, #15169, .F. ) ;
#80615 = CARTESIAN_POINT ( 'NONE',  ( 10.00000000000000178, 52.25893115100078745, 9.846743663894594434 ) ) ;
#80616 = STYLED_ITEM ( 'NONE', ( #70744 ), #90669 ) ;
#80618 = ADVANCED_FACE ( 'NONE', ( #19789 ), #47019, .T. ) ;
#80617 = CARTESIAN_POINT ( 'NONE',  ( 14.15369600240091330, 15.00000000000000888, -3.689340892730248012 ) ) ;
#80619 = CARTESIAN_POINT ( 'NONE',  ( -7.081429851441987999, -84.79152421822195151, 2.750000000000000000 ) ) ;
#80620 = ORIENTED_EDGE ( 'NONE', *, *, #70198, .F. ) ;
#80621 = CARTESIAN_POINT ( 'NONE',  ( -1.236172813752151045, 14.95077488074853811, -14.70095156538448755 ) ) ;
#80623 = CARTESIAN_POINT ( 'NONE',  ( 7.361572987183170547, 32.05059781766745175, 9.846743663894590881 ) ) ;
#80622 = DIRECTION ( 'NONE',  ( 0.000000000000000000, 0.000000000000000000, 1.000000000000000000 ) ) ;
#80624 = CARTESIAN_POINT ( 'NONE',  ( -4.164238869374099039, 66.80374883491396076, 8.674139862899312516E-16 ) ) ;
#80625 = CARTESIAN_POINT ( 'NONE',  ( -8.000000000000000000, 79.82179676972448590, 6.250000000000000000 ) ) ;
#80626 = ORIENTED_EDGE ( 'NONE', *, *, #70722, .F. ) ;
#80627 = DIRECTION ( 'NONE',  ( 0.6246950475544237324, 0.7808688094430306093, 0.000000000000000000 ) ) ;
#80628 = CARTESIAN_POINT ( 'NONE',  ( 7.361572987183169658, 34.96726448433411605, -9.846743663894592657 ) ) ;
#80629 = CARTESIAN_POINT ( 'NONE',  ( 22.81628187352647785, 1.623634669930420271, 6.195893100308588602E-16 ) ) ;
#80630 = CARTESIAN_POINT ( 'NONE',  ( 7.361572987183170547, 7.050597817667451750, 9.846743663894590881 ) ) ;
#80631 = DIRECTION ( 'NONE',  ( -1.000000000000000000, 0.000000000000000000, 0.000000000000000000 ) ) ;
#80632 = CARTESIAN_POINT ( 'NONE',  ( 12.63842701281683034, 7.467264484334118713, 9.846743663894596210 ) ) ;
#80633 = CARTESIAN_POINT ( 'NONE',  ( 19.84674366389459266, 53.30059781766744464, 2.638427012816836559 ) ) ;
#80634 = CARTESIAN_POINT ( 'NONE',  ( 1.816707512666850599, 20.10290668512022805, -6.499999999999995559 ) ) ;
#80635 = ORIENTED_EDGE ( 'NONE', *, *, #49476, .F. ) ;
#80636 = CARTESIAN_POINT ( 'NONE',  ( -0.8801773607111008646, 8.272018677488171434, 2.915334737309923430 ) ) ;
#80637 = CARTESIAN_POINT ( 'NONE',  ( -2.266590686148945544, 1.387082168247301128, -7.082119434687050408 ) ) ;
#80638 = CARTESIAN_POINT ( 'NONE',  ( 2.791683348922240793, 11.63393115100078568, 7.208316651077764092 ) ) ;
#80639 = CARTESIAN_POINT ( 'NONE',  ( -0.8801773607110991993, 47.85535201082150536, -2.915334737309923874 ) ) ;
#80641 = PLANE ( 'NONE',  #60909 ) ;
#80640 = CARTESIAN_POINT ( 'NONE',  ( 21.09922568453594849, 31.20696800326375353, 6.408140936763242479 ) ) ;
#80642 =( LENGTH_UNIT ( ) NAMED_UNIT ( * ) SI_UNIT ( .MILLI., .METRE. ) );
#80643 = ADVANCED_FACE ( 'NONE', ( #63708 ), #93724, .F. ) ;
#80644 = DIRECTION ( 'NONE',  ( -0.8526401643540953978, 0.000000000000000000, 0.5224985647159435809 ) ) ;
#80645 = DIRECTION ( 'NONE',  ( 0.000000000000000000, 0.000000000000000000, 1.000000000000000000 ) ) ;
#80646 = CARTESIAN_POINT ( 'NONE',  ( -2.816281873526473856, 4.331968003263754419, 3.434112377981055619 ) ) ;
#80647 = CARTESIAN_POINT ( 'NONE',  ( -1.099225684535947600, -0.4596986634029132657, 6.408140936763237150 ) ) ;
#80648 = CARTESIAN_POINT ( 'NONE',  ( 2.791683348922240793, 11.63393115100078568, 7.208316651077764092 ) ) ;
#80649 = CARTESIAN_POINT ( 'NONE',  ( 5.440088680355549045, -28.60298132251182679, -9.422509992056141925 ) ) ;
#80650 = CARTESIAN_POINT ( 'NONE',  ( 19.38216949554541557, 22.24863466993041428, -9.382169495545420901 ) ) ;
#80651 = CARTESIAN_POINT ( 'NONE',  ( 1.602071938427535924, 52.02224192338640307, -6.500000000000077272 ) ) ;
#80652 = CARTESIAN_POINT ( 'NONE',  ( -0.8801773607110991993, 32.85535201082151247, -2.915334737309923874 ) ) ;
#80653 = FACE_OUTER_BOUND ( 'NONE', #95200, .T. ) ;
#80654 = PRESENTATION_LAYER_ASSIGNMENT (  '', '', ( #66296 ) ) ;
#80655 = CARTESIAN_POINT ( 'NONE',  ( 24.16423886937410614, 49.30374883491396787, 8.672049930838204340E-16 ) ) ;
#80656 = CARTESIAN_POINT ( 'NONE',  ( 10.58981376305282041, 0.000000000000000000, 9.535111140613782510 ) ) ;
#80657 = CARTESIAN_POINT ( 'NONE',  ( 21.09922568453595559, 37.04030133659708923, -6.408140936763230044 ) ) ;
#80658 = CARTESIAN_POINT ( 'NONE',  ( 7.084665262690076126, 29.10535201082150181, 10.88017736071109987 ) ) ;
#80659 = B_SPLINE_CURVE_WITH_KNOTS ( 'NONE', 3,
 ( #35729, #6228, #96249, #59707, #14228, #60205 ),
 .UNSPECIFIED., .F., .F.,
 ( 4, 2, 4 ),
 ( 0.0002800392683685237944, 0.0006862448819815547638, 0.001092450495594585571 ),
 .UNSPECIFIED. ) ;
#80660 = CARTESIAN_POINT ( 'NONE',  ( 7.361572987183170547, 47.05059781766745175, 9.846743663894590881 ) ) ;
#80661 = CARTESIAN_POINT ( 'NONE',  ( 4.559911319644449179, 57.23035201082150536, -9.422509992056141925 ) ) ;
#80662 = CARTESIAN_POINT ( 'NONE',  ( 24.16423886937410614, 29.51208216824729647, -3.795296366450302550 ) ) ;
#80663 = CARTESIAN_POINT ( 'NONE',  ( -7.551349515323020789, -0.03417435944610275333, -12.08468537022916323 ) ) ;
#80664 = CARTESIAN_POINT ( 'NONE',  ( 2.791683348922237240, 25.38393115100078390, -7.208316651077763204 ) ) ;
#80665 = DIRECTION ( 'NONE',  ( 0.5547001962252290364, 0.8320502943378437211, 0.000000000000000000 ) ) ;
#80666 = CARTESIAN_POINT ( 'NONE',  ( 14.92337183194729988, 64.34226448433412315, -8.527530157486177487 ) ) ;
#80667 = ORIENTED_EDGE ( 'NONE', *, *, #22728, .F. ) ;
#80668 = CARTESIAN_POINT ( 'NONE',  ( 20.32896413005680003, 6.771642702460840546, 5.963430220938287007 ) ) ;
#80669 = CARTESIAN_POINT ( 'NONE',  ( 8.879999999999995453, 41.24999999999999289, -4.250000000000000000 ) ) ;
#80670 = CARTESIAN_POINT ( 'NONE',  ( 20.88017736071110164, 10.35535201082150714, 2.915334737309930979 ) ) ;
#80671 = CARTESIAN_POINT ( 'NONE',  ( 13.79529636645031943, 25.34541550158063572, -14.16423886937409904 ) ) ;
#80672 = CARTESIAN_POINT ( 'NONE',  ( 19.84674366389459266, 13.30059781766745353, 2.638427012816836559 ) ) ;
#80673 = CARTESIAN_POINT ( 'NONE',  ( 14.92337183194729988, 59.34226448433412315, -8.527530157486177487 ) ) ;
#80674 = CARTESIAN_POINT ( 'NONE',  ( 2.035157376598824452, 38.68868534415483396, 7.964842623401179544 ) ) ;
#80675 = CARTESIAN_POINT ( 'NONE',  ( -10.44999999999999751, 99.99999999999998579, 8.000000000000000000 ) ) ;
#80676 = DIRECTION ( 'NONE',  ( 0.000000000000000000, 0.000000000000000000, 1.000000000000000000 ) ) ;
#80677 = ORIENTED_EDGE ( 'NONE', *, *, #66947, .F. ) ;
#80678 = CARTESIAN_POINT ( 'NONE',  ( 0.4195498155886434599, 0.4999999999999998890, 10.00000000000000000 ) ) ;
#80679 = CARTESIAN_POINT ( 'NONE',  ( 7.361572987183169658, 39.96726448433411605, -9.846743663894592657 ) ) ;
#80680 = EDGE_LOOP ( 'NONE', ( #36877, #30726, #76062, #88741 ) ) ;
#80681 = ORIENTED_EDGE ( 'NONE', *, *, #83069, .F. ) ;
#80682 = CARTESIAN_POINT ( 'NONE',  ( 19.72487221294570858, 70.00000000000000000, 6.500000000000000888 ) ) ;
#80683 = CARTESIAN_POINT ( 'NONE',  ( -2.266590686148945544, 7.220415501580634832, 7.082119434687048631 ) ) ;
#80684 = CARTESIAN_POINT ( 'NONE',  ( 10.00000000000000000, 10.55374883491396787, -14.16423886937410082 ) ) ;
#80685 = CARTESIAN_POINT ( 'NONE',  ( 17.96484262340118221, 46.18868534415484106, -7.964842623401177768 ) ) ;
#80686 = CARTESIAN_POINT ( 'NONE',  ( -4.164238869374098151, 61.59541550158063217, -3.795296366450310543 ) ) ;
#80687 = CARTESIAN_POINT ( 'NONE',  ( 5.076628168052703671, 61.84226448433412315, 8.527530157486179263 ) ) ;
#80688 = CARTESIAN_POINT ( 'NONE',  ( 0.1532563361054100626, 30.80059781766744820, -2.638427012816831230 ) ) ;
#80689 = CARTESIAN_POINT ( 'NONE',  ( 47.41185586981792000, 64.79620302208442695, -8.000000000000000000 ) ) ;
#80691 = CARTESIAN_POINT ( 'NONE',  ( 10.00000000000000000, 7.873634669930421381, -12.81628187352647608 ) ) ;
#80690 = CARTESIAN_POINT ( 'NONE',  ( 15.44008868035555260, 29.73035201082150891, 9.422509992056143702 ) ) ;
#80692 = CARTESIAN_POINT ( 'NONE',  ( 22.26659068614895176, 4.720415501580633943, -7.082119434687042414 ) ) ;
#80693 = CARTESIAN_POINT ( 'NONE',  ( 20.36894250292379738, 54.92874883491396076, -10.36894250292379027 ) ) ;
#80694 = AXIS2_PLACEMENT_3D ( 'NONE', #56397, #17424, #41415 ) ;
#80695 = CARTESIAN_POINT ( 'NONE',  ( 17.96484262340118221, 11.18868534415484106, -7.964842623401177768 ) ) ;
#80696 = CARTESIAN_POINT ( 'NONE',  ( -0.1503990784575294781, 68.10158574516643171, 6.262539305110072618 ) ) ;
#80697 = DIRECTION ( 'NONE',  ( 1.000000000000000000, -0.000000000000000000, 0.000000000000000000 ) ) ;
#80698 = CARTESIAN_POINT ( 'NONE',  ( 9.846743663894594434, -36.49106884899921255, -2.168404344971008868E-15 ) ) ;
#80699 = ORIENTED_EDGE ( 'NONE', *, *, #36828, .F. ) ;
#80700 = ORIENTED_EDGE ( 'NONE', *, *, #79097, .F. ) ;
#80701 = EDGE_CURVE ( 'NONE', #51712, #14094, #54600, .T. ) ;
#80702 = EDGE_LOOP ( 'NONE', ( #59130, #31113 ) ) ;
#80703 = CARTESIAN_POINT ( 'NONE',  ( -2.266590686148945544, 51.38708216824730357, -7.082119434687050408 ) ) ;
#80704 = CARTESIAN_POINT ( 'NONE',  ( 18.52753015748618282, 28.92559781766745175, -4.923371831947291888 ) ) ;
#80705 = CARTESIAN_POINT ( 'NONE',  ( -0.8801773607111008646, 63.27201867748817676, 2.915334737309923430 ) ) ;
#80706 = ADVANCED_FACE ( 'NONE', ( #48220 ), #85745, .F. ) ;
#80707 = DIRECTION ( 'NONE',  ( -0.8788171126619616080, 0.000000000000000000, -0.4771587602596153999 ) ) ;
#80708 = CARTESIAN_POINT ( 'NONE',  ( 20.88017736071110164, 60.35535201082151957, 2.915334737309930979 ) ) ;
#80709 = MECHANICAL_DESIGN_GEOMETRIC_PRESENTATION_REPRESENTATION (  '', ( #865 ), #37608 ) ;
#80710 = CARTESIAN_POINT ( 'NONE',  ( -2.816281873526473856, 54.12363466993041783, 9.499525473075851096E-16 ) ) ;
#80711 = CARTESIAN_POINT ( 'NONE',  ( -12.81628187352647963, 3.915301336597085680, -3.434112377981046293 ) ) ;
#80712 = ORIENTED_EDGE ( 'NONE', *, *, #89464, .T. ) ;
#80713 = CARTESIAN_POINT ( 'NONE',  ( 2.035157376598822676, 47.43868534415484817, -7.964842623401177768 ) ) ;
#80714 = CARTESIAN_POINT ( 'NONE',  ( 22.26659068614895176, 19.72041550158063572, -7.082119434687042414 ) ) ;
#80715 = CARTESIAN_POINT ( 'NONE',  ( 6.565887622018943937, 23.08196800326375708, -12.81628187352647608 ) ) ;
#80716 = VERTEX_POINT ( 'NONE', #40733 ) ;
#80717 = CARTESIAN_POINT ( 'NONE',  ( 10.00000000000000178, 45.37363466993041783, 12.81628187352647608 ) ) ;
#80718 = CARTESIAN_POINT ( 'NONE',  ( 7.361572987183170547, 17.05059781766745530, 9.846743663894590881 ) ) ;
#80719 = CARTESIAN_POINT ( 'NONE',  ( 10.00000000000000000, 16.81368534415483751, -10.88017736071110342 ) ) ;
#80720 = CARTESIAN_POINT ( 'NONE',  ( -2.816281873526471635, 53.91530133659709634, -3.434112377981056508 ) ) ;
#80721 = DIRECTION ( 'NONE',  ( 1.000000000000000000, -0.000000000000000000, 0.000000000000000000 ) ) ;
#80722 = CARTESIAN_POINT ( 'NONE',  ( 19.84674366389459266, 43.71726448433410894, -2.638427012816827677 ) ) ;
#80723 = VECTOR ( 'NONE', #70193, 1000.000000000000000 ) ;
#80724 = CARTESIAN_POINT ( 'NONE',  ( 14.49999999999999822, 11.00000000000000000, -5.000000000000000000 ) ) ;
#80725 = EDGE_CURVE ( 'NONE', #37516, #59170, #26002, .T. ) ;
#80726 = VECTOR ( 'NONE', #69238, 1000.000000000000114 ) ;
#80727 = CARTESIAN_POINT ( 'NONE',  ( 2.035157376598824452, 63.68868534415484106, 7.964842623401179544 ) ) ;
#80728 = LINE ( 'NONE', #49721, #51548 ) ;
#80729 = DIRECTION ( 'NONE',  ( 0.8526401643540846287, 0.000000000000000000, 0.5224985647159611224 ) ) ;
#80730 = CARTESIAN_POINT ( 'NONE',  ( 1.472469842513823179, 21.42559781766745175, 4.923371831947296329 ) ) ;
#80731 = ADVANCED_FACE ( 'NONE', ( #16757 ), #78600, .T. ) ;
#80732 = CARTESIAN_POINT ( 'NONE',  ( 10.00000000000000000, 22.87363466993042138, -12.81628187352647608 ) ) ;
#80733 = CARTESIAN_POINT ( 'NONE',  ( 0.000000000000000000, 15.00000000000000000, 0.000000000000000000 ) ) ;
#80734 = CARTESIAN_POINT ( 'NONE',  ( 0.1532563361054100626, 45.80059781766745886, -2.638427012816831230 ) ) ;
#80735 = DIRECTION ( 'NONE',  ( -0.1496197561345325722, 0.9887436111420609963, 0.000000000000000000 ) ) ;
#80736 = CARTESIAN_POINT ( 'NONE',  ( 24.16423886937410614, 19.51208216824729647, -3.795296366450302550 ) ) ;
#80737 = CARTESIAN_POINT ( 'NONE',  ( 19.84674366389459266, 28.30059781766745886, 2.638427012816836559 ) ) ;
#80738 = CARTESIAN_POINT ( 'NONE',  ( 21.09922568453594849, 36.20696800326375353, 6.408140936763242479 ) ) ;
#80740 = CARTESIAN_POINT ( 'NONE',  ( -0.8801773607111009756, 23.06368534415484106, 1.068504757029289695E-15 ) ) ;
#80739 = DIRECTION ( 'NONE',  ( -6.608470384673550777E-17, -1.000000000000000000, -0.000000000000000000 ) ) ;
#80741 = CARTESIAN_POINT ( 'NONE',  ( 20.88017736071110519, 65.56368534415483396, 2.639326808657452039E-16 ) ) ;
#80742 = CARTESIAN_POINT ( 'NONE',  ( 19.38216949554541557, 2.248634669930420049, -9.382169495545420901 ) ) ;
#80743 = CARTESIAN_POINT ( 'NONE',  ( 0.2751277870542910842, 67.28217586085239077, -6.499999999999992006 ) ) ;
#80744 = CARTESIAN_POINT ( 'NONE',  ( 19.84674366389459621, 33.50893115100078745, 7.409399052514197653E-17 ) ) ;
#80745 = CARTESIAN_POINT ( 'NONE',  ( 10.00000000000000178, 24.31368534415484106, 10.88017736071110342 ) ) ;
#80746 = CARTESIAN_POINT ( 'NONE',  ( -2.816281873526471635, 23.91530133659708568, -3.434112377981056508 ) ) ;
#80747 = MECHANICAL_DESIGN_GEOMETRIC_PRESENTATION_REPRESENTATION (  '', ( #58394 ), #64734 ) ;
#80748 = CARTESIAN_POINT ( 'NONE',  ( 1.472469842513823179, 36.42559781766745175, 4.923371831947296329 ) ) ;
#80749 =( NAMED_UNIT ( * ) SI_UNIT ( $, .STERADIAN. ) SOLID_ANGLE_UNIT ( ) );
#80750 = CARTESIAN_POINT ( 'NONE',  ( -2.361410439757430701, 0.2306972965111891150, 14.75336556272935162 ) ) ;
#80751 = VECTOR ( 'NONE', #53439, 1000.000000000000000 ) ;
#80752 = CARTESIAN_POINT ( 'NONE',  ( 0.5774900079438607392, 28.48035201082150891, 5.440088680355550821 ) ) ;
#80753 = EDGE_LOOP ( 'NONE', ( #96997, #49572, #43060, #74300 ) ) ;
#80754 = CARTESIAN_POINT ( 'NONE',  ( 3.469446951953614189E-15, 4.171802177851546389, 11.25000000000000355 ) ) ;
#80755 = CARTESIAN_POINT ( 'NONE',  ( 10.00000000000000000, 6.813685344154838397, -10.88017736071110342 ) ) ;
#80757 = CARTESIAN_POINT ( 'NONE',  ( 10.00000000000000178, 24.31368534415484106, 10.88017736071110342 ) ) ;
#80756 = CARTESIAN_POINT ( 'NONE',  ( 18.52753015748617571, 58.09226448433411605, 4.923371831947298993 ) ) ;
#80758 = CARTESIAN_POINT ( 'NONE',  ( -14.71525861348291997, 15.00000000000000000, 2.908807992686483601 ) ) ;
#80759 = CARTESIAN_POINT ( 'NONE',  ( -0.8801773607111009756, 58.06368534415484106, 1.068504757029289695E-15 ) ) ;
#80761 = CARTESIAN_POINT ( 'NONE',  ( 8.879999999999995453, 41.24999999999999289, 6.500000000000000888 ) ) ;
#80760 = CARTESIAN_POINT ( 'NONE',  ( 19.42250999205614193, 20.14701867748817321, 5.440088680355555262 ) ) ;
#80762 = CARTESIAN_POINT ( 'NONE',  ( 1.472469842513823179, 1.425597817667451528, 4.923371831947296329 ) ) ;
#80763 = CARTESIAN_POINT ( 'NONE',  ( -46.68456736488007408, 103.6675473310227034, -5.775421524742654356 ) ) ;
#80764 = CARTESIAN_POINT ( 'NONE',  ( 12.63842701281683034, 57.46726448433411605, 9.846743663894596210 ) ) ;
#80766 = CARTESIAN_POINT ( 'NONE',  ( 20.15039907845753220, 20.60158574516643171, -6.262539305110077947 ) ) ;
#80765 = CARTESIAN_POINT ( 'NONE',  ( 24.16423886937409904, 59.09541550158063217, 3.795296366450317205 ) ) ;
#80767 = CARTESIAN_POINT ( 'NONE',  ( -3.749999999999993783, 43.00000000000000711, -4.000000000000000000 ) ) ;
#80768 = EDGE_CURVE ( 'NONE', #51986, #43714, #55742, .T. ) ;
#80769 = CARTESIAN_POINT ( 'NONE',  ( 20.36894250292379382, 3.678748834913967869, 10.36894250292379205 ) ) ;
#80770 = CARTESIAN_POINT ( 'NONE',  ( 24.16423886937409904, 34.09541550158064638, 3.795296366450317205 ) ) ;
#80771 = CARTESIAN_POINT ( 'NONE',  ( -2.816281873526473856, 9.331968003263753531, 3.434112377981055619 ) ) ;
#80772 = CARTESIAN_POINT ( 'NONE',  ( -7.750000000000000000, 80.32179676972448590, 4.000000000000000000 ) ) ;
#80773 = EDGE_LOOP ( 'NONE', ( #12099, #79373, #48208, #98580, #58188, #46991 ) ) ;
#80774 = AXIS2_PLACEMENT_3D ( 'NONE', #40683, #2212, #41188 ) ;
#80775 = CARTESIAN_POINT ( 'NONE',  ( 12.91533473730992121, 9.522018677488171434, 10.88017736071110164 ) ) ;
#80776 = CARTESIAN_POINT ( 'NONE',  ( 1.472469842513823179, 36.42559781766745175, 4.923371831947296329 ) ) ;
#80777 = DIRECTION ( 'NONE',  ( 0.000000000000000000, 1.000000000000000000, 0.000000000000000000 ) ) ;
#80778 = CARTESIAN_POINT ( 'NONE',  ( 10.00000000000000000, 61.81368534415484106, -10.88017736071110342 ) ) ;
#80779 = CARTESIAN_POINT ( 'NONE',  ( 18.00000000000001776, 4.625929269271493211E-15, 4.000000000000000000 ) ) ;
#80780 = CARTESIAN_POINT ( 'NONE',  ( 13.43411237798106583, 62.66530133659708923, -12.81628187352647252 ) ) ;
#80781 = CARTESIAN_POINT ( 'NONE',  ( 6.565887622018943937, 25.16530133659708213, 12.81628187352647430 ) ) ;
#80782 = CARTESIAN_POINT ( 'NONE',  ( 18.52753015748618282, 33.92559781766745886, -4.923371831947291888 ) ) ;
#80783 = ORIENTED_EDGE ( 'NONE', *, *, #65705, .T. ) ;
#80784 = SURFACE_STYLE_FILL_AREA ( #35271 ) ;
#80785 = FACE_OUTER_BOUND ( 'NONE', #64587, .T. ) ;
#80786 = CARTESIAN_POINT ( 'NONE',  ( 17.96484262340118221, 4.938685344154837509, 7.964842623401181321 ) ) ;
#80787 = CARTESIAN_POINT ( 'NONE',  ( 12.91533473730992121, 19.52201867748816611, 10.88017736071110164 ) ) ;
#80788 = CARTESIAN_POINT ( 'NONE',  ( 24.16423886937409904, 44.09541550158063927, 3.795296366450317205 ) ) ;
#80789 = CARTESIAN_POINT ( 'NONE',  ( 15.44008868035555260, 29.73035201082150891, 9.422509992056143702 ) ) ;
#80790 = CARTESIAN_POINT ( 'NONE',  ( 2.035157376598822676, 62.43868534415483396, -7.964842623401177768 ) ) ;
#80791 = CARTESIAN_POINT ( 'NONE',  ( -13.21272562212263502, 14.99999999999808686, 6.271554226548477828 ) ) ;
#80792 = CARTESIAN_POINT ( 'NONE',  ( 34.56412365047464874, 28.99999999999999645, 9.500000000000000000 ) ) ;
#80793 = CARTESIAN_POINT ( 'NONE',  ( 18.52753015748618282, 13.92559781766745175, -4.923371831947291888 ) ) ;
#80794 =( LENGTH_UNIT ( ) NAMED_UNIT ( * ) SI_UNIT ( .MILLI., .METRE. ) );
#80795 = CARTESIAN_POINT ( 'NONE',  ( 17.20831665107776587, 12.88393115100078390, 7.208316651077764980 ) ) ;
#80796 = SURFACE_SIDE_STYLE ('',( #50280 ) ) ;
#80797 = CARTESIAN_POINT ( 'NONE',  ( 19.84674366389459621, 38.50893115100078745, 7.409399052514197653E-17 ) ) ;
#80798 = CARTESIAN_POINT ( 'NONE',  ( 10.00000000000000178, 57.25893115100078745, 9.846743663894594434 ) ) ;
#80799 = CIRCLE ( 'NONE', #52101, 1.500000000000001332 ) ;
#80800 = ORIENTED_EDGE ( 'NONE', *, *, #23608, .F. ) ;
#80801 = CARTESIAN_POINT ( 'NONE',  ( 16.40814093676324603, 42.45696800326375353, -11.09922568453594671 ) ) ;
#80802 = DIRECTION ( 'NONE',  ( 1.000000000000000000, 0.000000000000000000, 0.000000000000000000 ) ) ;
#80803 = CARTESIAN_POINT ( 'NONE',  ( 19.42250999205614193, 65.14701867748817676, 5.440088680355555262 ) ) ;
#80804 = CARTESIAN_POINT ( 'NONE',  ( 6.565887622018943937, 38.08196800326376064, -12.81628187352647608 ) ) ;
#80806 = CARTESIAN_POINT ( 'NONE',  ( 1.472469842513823179, 26.42559781766745175, 4.923371831947296329 ) ) ;
#80805 = CARTESIAN_POINT ( 'NONE',  ( 24.16423886937409904, 59.09541550158063217, 3.795296366450317205 ) ) ;
#80807 = CARTESIAN_POINT ( 'NONE',  ( 0.1077916266722762639, 47.24062864464239908, -6.478736007406001640 ) ) ;
#80808 = CARTESIAN_POINT ( 'NONE',  ( -0.1503990784575328643, 70.00000000000000000, -6.262539305110068177 ) ) ;
#80809 = CARTESIAN_POINT ( 'NONE',  ( -0.3689425029237898834, 31.17874883491396787, -10.36894250292378850 ) ) ;
#80810 = CARTESIAN_POINT ( 'NONE',  ( 19.84674366389459621, 48.50893115100078745, 7.409399052514197653E-17 ) ) ;
#80811 = CARTESIAN_POINT ( 'NONE',  ( 20.03447792253738768, 12.65514106990690024, -6.401564815979734036 ) ) ;
#80812 = CARTESIAN_POINT ( 'NONE',  ( 2.035157376598822676, 37.43868534415484106, -7.964842623401177768 ) ) ;
#80813 = CARTESIAN_POINT ( 'NONE',  ( 7.084665262690076126, 57.02201867748817676, -10.88017736071110164 ) ) ;
#80814 = EDGE_LOOP ( 'NONE', ( #13000, #10249, #65430, #33809 ) ) ;
#80815 = CARTESIAN_POINT ( 'NONE',  ( 22.81628187352648496, 41.83196800326375353, -3.434112377981050290 ) ) ;
#80816 = CARTESIAN_POINT ( 'NONE',  ( 2.035157376598822676, 52.43868534415483396, -7.964842623401177768 ) ) ;
#80817 = VERTEX_POINT ( 'NONE', #47231 ) ;
#80818 = DIRECTION ( 'NONE',  ( 0.000000000000000000, 0.000000000000000000, 1.000000000000000000 ) ) ;
#80819 = EDGE_CURVE ( 'NONE', #94458, #86688, #38634, .T. ) ;
#80820 = FILL_AREA_STYLE_COLOUR ( '', #20146 ) ;
#80821 =( GEOMETRIC_REPRESENTATION_CONTEXT ( 3 ) GLOBAL_UNCERTAINTY_ASSIGNED_CONTEXT ( ( #95430 ) ) GLOBAL_UNIT_ASSIGNED_CONTEXT ( ( #37427, #90893, #22421 ) ) REPRESENTATION_CONTEXT ( 'NONE', 'WORKASPACE' ) );
#80822 = EDGE_LOOP ( 'NONE', ( #16462, #72809, #20828, #16353, #29394, #75672, #11087, #80484 ) ) ;
#80823 = CIRCLE ( 'NONE', #92032, 0.1000000000000001166 ) ;
#80824 = VECTOR ( 'NONE', #89794, 999.9999999999998863 ) ;
#80825 = CARTESIAN_POINT ( 'NONE',  ( 15.44008868035555260, 64.73035201082151957, 9.422509992056143702 ) ) ;
#80826 = CARTESIAN_POINT ( 'NONE',  ( 19.42250999205614548, 10.98035201082150358, -5.440088680355545492 ) ) ;
#80827 = SURFACE_STYLE_USAGE ( .BOTH. , #98194 ) ;
#80828 = CARTESIAN_POINT ( 'NONE',  ( 20.88017736071110164, 10.35535201082150714, 2.915334737309930979 ) ) ;
#80829 = CARTESIAN_POINT ( 'NONE',  ( -2.266590686148945544, 17.22041550158063572, 7.082119434687048631 ) ) ;
#80830 = AXIS2_PLACEMENT_3D ( 'NONE', #20219, #12715, #96732 ) ;
#80831 = CARTESIAN_POINT ( 'NONE',  ( 4.559911319644449179, 17.23035201082150536, -9.422509992056141925 ) ) ;
#80832 = CARTESIAN_POINT ( 'NONE',  ( 19.84674366389459266, 58.71726448433411605, -2.638427012816827677 ) ) ;
#80833 = VERTEX_POINT ( 'NONE', #86233 ) ;
#80834 = CARTESIAN_POINT ( 'NONE',  ( 18.52753015748617571, 63.09226448433412315, 4.923371831947298993 ) ) ;
#80835 = EDGE_LOOP ( 'NONE', ( #39278, #53540, #53979, #21189, #33238, #95829 ) ) ;
#80836 = CARTESIAN_POINT ( 'NONE',  ( -0.8801773607111009756, 58.06368534415484106, 1.068504757029289695E-15 ) ) ;
#80837 = CARTESIAN_POINT ( 'NONE',  ( 10.00000000000000000, 59.75893115100078745, -9.846743663894594434 ) ) ;
#80839 = CARTESIAN_POINT ( 'NONE',  ( 2.831191079880678085, 79.91181047996344944, 9.500000000000000000 ) ) ;
#80838 = CARTESIAN_POINT ( 'NONE',  ( 15.44008868035555793, 6.397018677488170546, -9.422509992056140149 ) ) ;
#80840 = CARTESIAN_POINT ( 'NONE',  ( 0.5774900079438590739, 62.64701867748817676, -5.440088680355550821 ) ) ;
#80841 = CARTESIAN_POINT ( 'NONE',  ( 4.559911319644449179, 22.23035201082150536, -9.422509992056141925 ) ) ;
#80842 = AXIS2_PLACEMENT_3D ( 'NONE', #31188, #83220, #92678 ) ;
#80844 = EDGE_CURVE ( 'NONE', #77069, #26051, #41858, .T. ) ;
#80843 =( GEOMETRIC_REPRESENTATION_CONTEXT ( 3 ) GLOBAL_UNCERTAINTY_ASSIGNED_CONTEXT ( ( #48448 ) ) GLOBAL_UNIT_ASSIGNED_CONTEXT ( ( #23599, #8577, #70068 ) ) REPRESENTATION_CONTEXT ( 'NONE', 'WORKASPACE' ) );
#80845 = CARTESIAN_POINT ( 'NONE',  ( 16.40814093676324603, 57.45696800326375353, -11.09922568453594671 ) ) ;
#80846 = CARTESIAN_POINT ( 'NONE',  ( 17.96484262340118221, 24.93868534415484461, 7.964842623401181321 ) ) ;
#80847 = CARTESIAN_POINT ( 'NONE',  ( 0.6076426042653101378, 47.37576471608601736, -6.499999999999992006 ) ) ;
#80848 = CARTESIAN_POINT ( 'NONE',  ( 22.81628187352648496, 36.83196800326376064, -3.434112377981050290 ) ) ;
#80849 = CARTESIAN_POINT ( 'NONE',  ( 12.91533473730993009, 36.60535201082151247, -10.88017736071109987 ) ) ;
#80850 = CARTESIAN_POINT ( 'NONE',  ( 1.472469842513823179, 61.42559781766745175, 4.923371831947296329 ) ) ;
#80851 = EDGE_CURVE ( 'NONE', #35385, #82533, #41728, .T. ) ;
#80852 = VERTEX_POINT ( 'NONE', #31740 ) ;
#80853 = CARTESIAN_POINT ( 'NONE',  ( -11.36220558718868290, 15.00000000000000000, 9.008345252845137097 ) ) ;
#80854 = CARTESIAN_POINT ( 'NONE',  ( 17.20831665107776587, 59.13393115100078745, -7.208316651077762316 ) ) ;
#80856 = CARTESIAN_POINT ( 'NONE',  ( 5.076628168052704559, 45.17559781766745175, -8.527530157486179263 ) ) ;
#80855 = FACE_OUTER_BOUND ( 'NONE', #26157, .T. ) ;
#80857 = CARTESIAN_POINT ( 'NONE',  ( 12.91533473730993009, 21.60535201082150536, -10.88017736071109987 ) ) ;
#80858 = DIRECTION ( 'NONE',  ( -0.5547001962252291474, -0.8320502943378437211, -0.000000000000000000 ) ) ;
#80859 = CARTESIAN_POINT ( 'NONE',  ( 5.076628168052703671, 41.84226448433411605, 8.527530157486179263 ) ) ;
#80860 = CARTESIAN_POINT ( 'NONE',  ( -14.48718990079890290, 15.00000000000000000, 0.6093675230839377122 ) ) ;
#80861 = CYLINDRICAL_SURFACE ( 'NONE', #83830, 15.00000000000000000 ) ;
#80863 = CARTESIAN_POINT ( 'NONE',  ( 5.076628168052703671, 6.842264484334118713, 8.527530157486179263 ) ) ;
#80862 = CARTESIAN_POINT ( 'NONE',  ( 12.63842701281683034, 37.46726448433411605, 9.846743663894596210 ) ) ;
#80864 = DIRECTION ( 'NONE',  ( -0.4305110968082861977, 0.000000000000000000, -0.9025852843498647360 ) ) ;
#80866 = ORIENTED_EDGE ( 'NONE', *, *, #42403, .F. ) ;
#80865 = CARTESIAN_POINT ( 'NONE',  ( 5.076628168052704559, 55.17559781766745175, -8.527530157486179263 ) ) ;
#80867 = CARTESIAN_POINT ( 'NONE',  ( -1.780824192092605562, 0.5000000000000004441, 14.89391369643512064 ) ) ;
#80868 = CARTESIAN_POINT ( 'NONE',  ( 16.40814093676324603, 37.45696800326376064, -11.09922568453594671 ) ) ;
#80869 = CARTESIAN_POINT ( 'NONE',  ( 0.1532563361054082862, 41.21726448433411605, 2.638427012816831674 ) ) ;
#80870 = CARTESIAN_POINT ( 'NONE',  ( 6.898461952320432466, 4.226027835726576547E-16, -12.75387089053309175 ) ) ;
#80871 = CARTESIAN_POINT ( 'NONE',  ( 24.16423886937410614, 59.51208216824728936, -3.795296366450302550 ) ) ;
#80872 = CARTESIAN_POINT ( 'NONE',  ( 10.00000000000000000, 34.75893115100078745, -9.846743663894594434 ) ) ;
#80873 = DIRECTION ( 'NONE',  ( 0.2503800040544526539, 0.000000000000000000, -0.9681476403781048568 ) ) ;
#80874 = CARTESIAN_POINT ( 'NONE',  ( 20.36894250292379738, 54.92874883491396076, -10.36894250292379027 ) ) ;
#80875 = DIRECTION ( 'NONE',  ( 0.8526401643540917341, 0.000000000000000000, -0.5224985647159495761 ) ) ;
#80876 = CARTESIAN_POINT ( 'NONE',  ( 4.559911319644449179, 18.89701867748817321, 9.422509992056141925 ) ) ;
#80877 = CARTESIAN_POINT ( 'NONE',  ( 6.204703633549690345, 40.76208216824731778, -14.16423886937410259 ) ) ;
#80878 = CARTESIAN_POINT ( 'NONE',  ( 24.16423886937410614, 59.30374883491397497, 8.672049930838204340E-16 ) ) ;
#80879 = DIRECTION ( 'NONE',  ( -0.8320502943378437211, 0.5547001962252290364, 0.000000000000000000 ) ) ;
#80880 = EDGE_CURVE ( 'NONE', #98319, #55638, #51405, .T. ) ;
#80881 = CARTESIAN_POINT ( 'NONE',  ( 7.361572987183170547, 12.05059781766744997, 9.846743663894590881 ) ) ;
#80883 = CARTESIAN_POINT ( 'NONE',  ( 1.472469842513823179, 65.59226448433412315, -4.923371831947296329 ) ) ;
#80882 = CARTESIAN_POINT ( 'NONE',  ( -13.50171220565091090, -3.121739927105722716E-15, 5.622479820943727447 ) ) ;
#80884 = ORIENTED_EDGE ( 'NONE', *, *, #38681, .T. ) ;
#80885 = CARTESIAN_POINT ( 'NONE',  ( 7.084665262690076126, 49.10535201082149825, 10.88017736071109987 ) ) ;
#80886 = CARTESIAN_POINT ( 'NONE',  ( 0.1129803114748867132, 64.29427333184091253, -6.480634945678686698 ) ) ;
#80887 = ADVANCED_FACE ( 'NONE', ( #78730 ), #10240, .F. ) ;
#80888 = LINE ( 'NONE', #12386, #53927 ) ;
#80889 = CIRCLE ( 'NONE', #47337, 14.49999999999999822 ) ;
#80890 = CARTESIAN_POINT ( 'NONE',  ( 1.472469842513823179, 60.59226448433412315, -4.923371831947296329 ) ) ;
#80891 = CARTESIAN_POINT ( 'NONE',  ( 14.93875075227017213, 14.76984974223857172, -0.2365588874159303689 ) ) ;
#80892 = AXIS2_PLACEMENT_3D ( 'NONE', #61753, #92755, #16280 ) ;
#80893 = EDGE_LOOP ( 'NONE', ( #21323, #35075, #66328, #72184 ) ) ;
#80894 = CARTESIAN_POINT ( 'NONE',  ( 6.204703633549690345, 30.76208216824730357, -14.16423886937410259 ) ) ;
#80895 = VECTOR ( 'NONE', #20603, 999.9999999999998863 ) ;
#80896 = CARTESIAN_POINT ( 'NONE',  ( -14.56368227077854272, 14.76930270348881002, -3.337246381125379191 ) ) ;
#80897 = CARTESIAN_POINT ( 'NONE',  ( -6.871342362925322078, -73.24551516664604378, -2.500000000000000000 ) ) ;
#80898 = CARTESIAN_POINT ( 'NONE',  ( 15.44008868035555793, 16.39701867748817321, -9.422509992056140149 ) ) ;
#80899 = CARTESIAN_POINT ( 'NONE',  ( 0.6178305044545838731, 34.74863466993042493, 9.382169495545420901 ) ) ;
#80900 = CARTESIAN_POINT ( 'NONE',  ( 10.97221242068710012, 15.00000000000000533, -9.670525607392798761 ) ) ;
#80901 = CARTESIAN_POINT ( 'NONE',  ( 0.1532563361054100626, 5.800597817667452638, -2.638427012816831230 ) ) ;
#80902 = LINE ( 'NONE', #12888, #90484 ) ;
#80903 = ORIENTED_EDGE ( 'NONE', *, *, #52473, .T. ) ;
#80904 = CARTESIAN_POINT ( 'NONE',  ( 10.64017930668205736, 0.5000000000000004441, -10.57291749337215592 ) ) ;
#80905 = EDGE_CURVE ( 'NONE', #97143, #5600, #67470, .T. ) ;
#80906 = CARTESIAN_POINT ( 'NONE',  ( 10.00000000000000000, 25.55374883491396787, -14.16423886937410082 ) ) ;
#80907 = CARTESIAN_POINT ( 'NONE',  ( 13.79529636645030344, 3.262082168247301350, 14.16423886937410614 ) ) ;
#80908 = CARTESIAN_POINT ( 'NONE',  ( -7.117803565204841476, -58.38168516195395341, 3.999999999999999112 ) ) ;
#80909 = CARTESIAN_POINT ( 'NONE',  ( 12.91533473730992121, 29.52201867748817321, 10.88017736071110164 ) ) ;
#80910 = LINE ( 'NONE', #26915, #35079 ) ;
#80911 = CARTESIAN_POINT ( 'NONE',  ( -5.204170427930421283E-15, 8.438309369127518167, -11.92686044187656513 ) ) ;
#80912 = CARTESIAN_POINT ( 'NONE',  ( 4.559911319644449179, 38.89701867748817676, 9.422509992056141925 ) ) ;
#80913 = CARTESIAN_POINT ( 'NONE',  ( 20.88017736071110164, 55.35535201082149825, 2.915334737309930979 ) ) ;
#80914 = CARTESIAN_POINT ( 'NONE',  ( 22.81628187352648496, 6.831968003263753531, -3.434112377981050290 ) ) ;
#80915 = CARTESIAN_POINT ( 'NONE',  ( 14.02068044289381987, 14.49999999999999112, 5.331089937175756077 ) ) ;
#80916 = CARTESIAN_POINT ( 'NONE',  ( 19.84674366389459266, 23.71726448433412315, -2.638427012816827677 ) ) ;
#80917 = AXIS2_PLACEMENT_3D ( 'NONE', #71841, #50307, #12319 ) ;
#80918 =( LENGTH_UNIT ( ) NAMED_UNIT ( * ) SI_UNIT ( .MILLI., .METRE. ) );
#80919 = CARTESIAN_POINT ( 'NONE',  ( 20.88017736071110875, 45.77201867748816966, -2.915334737309920765 ) ) ;
#80920 = COLOUR_RGB ( '', 0.40784314, 0.44705882, 0.49803922) ;
#80921 = STYLED_ITEM ( 'NONE', ( #69928 ), #72720 ) ;
#80922 = CARTESIAN_POINT ( 'NONE',  ( 21.09922568453595559, 2.040301336597086568, -6.408140936763230044 ) ) ;
#80923 = CARTESIAN_POINT ( 'NONE',  ( 10.00000000000000178, 64.31368534415483396, 10.88017736071110342 ) ) ;
#80924 = CARTESIAN_POINT ( 'NONE',  ( 7.361572987183169658, 19.96726448433411960, -9.846743663894592657 ) ) ;
#80925 = CARTESIAN_POINT ( 'NONE',  ( 19.38216949554541557, 52.24863466993041072, -9.382169495545420901 ) ) ;
#80926 = CARTESIAN_POINT ( 'NONE',  ( 12.63842701281683922, 4.550597817667451750, -9.846743663894590881 ) ) ;
#80927 = ORIENTED_EDGE ( 'NONE', *, *, #48537, .F. ) ;
#80928 = CARTESIAN_POINT ( 'NONE',  ( 1.383448333479217141, 57.37718327197430312, -6.499999999999959144 ) ) ;
#80929 = DIRECTION ( 'NONE',  ( 0.1993679344171971901, 0.000000000000000000, 0.9799247046208295897 ) ) ;
#80930 = CARTESIAN_POINT ( 'NONE',  ( 7.084665262690076126, 22.02201867748817321, -10.88017736071110164 ) ) ;
#80931 = CARTESIAN_POINT ( 'NONE',  ( 0.6178305044545818747, 58.49863466993042493, -9.382169495545419124 ) ) ;
#80932 = CARTESIAN_POINT ( 'NONE',  ( 19.84674366389459266, 28.30059781766745886, 2.638427012816836559 ) ) ;
#80933 = CARTESIAN_POINT ( 'NONE',  ( -0.8801773607111008646, 13.27201867748817143, 2.915334737309923430 ) ) ;
#80934 = CARTESIAN_POINT ( 'NONE',  ( 17.08211943468705840, 65.13708216824730357, -12.26659068614894466 ) ) ;
#80935 = ORIENTED_EDGE ( 'NONE', *, *, #75635, .T. ) ;
#80936 = CARTESIAN_POINT ( 'NONE',  ( 2.035157376598822676, 17.43868534415483751, -7.964842623401177768 ) ) ;
#80937 = EDGE_CURVE ( 'NONE', #20205, #8435, #6863, .T. ) ;
#80938 = CARTESIAN_POINT ( 'NONE',  ( 10.00000000000000178, 34.31368534415484106, 10.88017736071110342 ) ) ;
#80940 = CARTESIAN_POINT ( 'NONE',  ( 7.084665262690076126, 39.10535201082150536, 10.88017736071109987 ) ) ;
#80939 = CARTESIAN_POINT ( 'NONE',  ( -12.21130863673212197, 15.00000000000000533, 8.049375889232891268 ) ) ;
#80941 = ORIENTED_EDGE ( 'NONE', *, *, #74680, .F. ) ;
#80942 = CARTESIAN_POINT ( 'NONE',  ( 20.24186590665277663, 9.734100856612039721, 6.114288769123037426 ) ) ;
#80943 = CARTESIAN_POINT ( 'NONE',  ( 17.96484262340118221, 29.93868534415484106, 7.964842623401181321 ) ) ;
#80944 = CYLINDRICAL_SURFACE ( 'NONE', #66821, 9.999999999999998224 ) ;
#80945 = CARTESIAN_POINT ( 'NONE',  ( 22.26659068614894466, 38.88708216824731068, 7.082119434687054849 ) ) ;
#80946 = CARTESIAN_POINT ( 'NONE',  ( 2.035157376598822676, 37.43868534415484106, -7.964842623401177768 ) ) ;
#80947 = CARTESIAN_POINT ( 'NONE',  ( 20.88017736071110875, 30.77201867748816966, -2.915334737309920765 ) ) ;
#80948 = EDGE_CURVE ( 'NONE', #1705, #19380, #25864, .T. ) ;
#80949 = CARTESIAN_POINT ( 'NONE',  ( 5.076628168052704559, 65.17559781766745175, -8.527530157486179263 ) ) ;
#80950 = DIRECTION ( 'NONE',  ( 0.6225146366376079765, 0.000000000000000000, 0.7826081568524232424 ) ) ;
#80951 = CARTESIAN_POINT ( 'NONE',  ( 2.791683348922240793, 46.63393115100077324, 7.208316651077764092 ) ) ;
#80952 = VERTEX_POINT ( 'NONE', #95703 ) ;
#80953 = DIRECTION ( 'NONE',  ( -0.000000000000000000, -1.000000000000000000, 0.000000000000000000 ) ) ;
#80954 = CARTESIAN_POINT ( 'NONE',  ( 2.791683348922240793, 16.63393115100078745, 7.208316651077764092 ) ) ;
#80955 = CARTESIAN_POINT ( 'NONE',  ( -9.382169495545413795, -35.25136533006957507, 9.382169495545428006 ) ) ;
#80956 = CARTESIAN_POINT ( 'NONE',  ( 12.91533473730992121, 9.522018677488171434, 10.88017736071110164 ) ) ;
#80957 = CARTESIAN_POINT ( 'NONE',  ( 12.63842701281683922, 29.55059781766745175, -9.846743663894590881 ) ) ;
#80958 = CARTESIAN_POINT ( 'NONE',  ( 22.81628187352647785, 11.41530133659708390, 3.434112377981063169 ) ) ;
#80959 = CARTESIAN_POINT ( 'NONE',  ( 4.559911319644449179, 53.89701867748817676, 9.422509992056141925 ) ) ;
#80961 = CARTESIAN_POINT ( 'NONE',  ( 13.43411237798106583, 52.66530133659708213, -12.81628187352647252 ) ) ;
#80960 = CARTESIAN_POINT ( 'NONE',  ( -0.8801773607111008646, 18.27201867748817321, 2.915334737309923430 ) ) ;
#80962 = CARTESIAN_POINT ( 'NONE',  ( -2.266590686148945544, 32.22041550158063927, 7.082119434687048631 ) ) ;
#80963 = EDGE_CURVE ( 'NONE', #58088, #91901, #67805, .T. ) ;
#80965 = CARTESIAN_POINT ( 'NONE',  ( 20.32896413005680358, 34.74545670184113533, 5.963430220938287007 ) ) ;
#80964 = AXIS2_PLACEMENT_3D ( 'NONE', #61064, #91065, #53068 ) ;
#80966 = ORIENTED_EDGE ( 'NONE', *, *, #71910, .T. ) ;
#80967 = CARTESIAN_POINT ( 'NONE',  ( 5.076628168052704559, 65.17559781766745175, -8.527530157486179263 ) ) ;
#80968 = CARTESIAN_POINT ( 'NONE',  ( -8.000000000000000000, 40.74999999999999289, 4.250000000000000000 ) ) ;
#80969 = CARTESIAN_POINT ( 'NONE',  ( 17.96484262340118221, 31.18868534415483751, -7.964842623401177768 ) ) ;
#80971 = EDGE_CURVE ( 'NONE', #90286, #22448, #28181, .T. ) ;
#80970 = CARTESIAN_POINT ( 'NONE',  ( 14.92337183194729633, 62.67559781766745886, 8.527530157486181039 ) ) ;
#80972 = ORIENTED_EDGE ( 'NONE', *, *, #45046, .F. ) ;
#80973 = CARTESIAN_POINT ( 'NONE',  ( 10.00000000000000000, 19.75893115100078390, -9.846743663894594434 ) ) ;
#80974 = CIRCLE ( 'NONE', #10751, 0.4999999999999985567 ) ;
#80975 = CARTESIAN_POINT ( 'NONE',  ( 0.1532563361054100626, 20.80059781766744464, -2.638427012816831230 ) ) ;
#80976 = CARTESIAN_POINT ( 'NONE',  ( 18.52753015748618282, 8.925597817667451750, -4.923371831947291888 ) ) ;
#80977 = CARTESIAN_POINT ( 'NONE',  ( 4.838527690343521925, 15.00000000000000000, 14.19819177887730177 ) ) ;
#80980 = CARTESIAN_POINT ( 'NONE',  ( 11.22915323889574601, 15.00000000000000000, 8.773176023390684364 ) ) ;
#80979 = AXIS2_PLACEMENT_3D ( 'NONE', #17058, #33499, #11018 ) ;
#80978 = CARTESIAN_POINT ( 'NONE',  ( 10.00000000000000000, -0.2410688489992152128, -9.846743663894594434 ) ) ;
#80981 = CARTESIAN_POINT ( 'NONE',  ( 10.00000000000000000, 4.758931151000784787, -9.846743663894594434 ) ) ;
#80983 = ORIENTED_EDGE ( 'NONE', *, *, #80701, .F. ) ;
#80982 = CARTESIAN_POINT ( 'NONE',  ( 2.791683348922237240, 15.38393115100078212, -7.208316651077763204 ) ) ;
#80984 = VECTOR ( 'NONE', #83137, 1000.000000000000000 ) ;
#80985 = CARTESIAN_POINT ( 'NONE',  ( -3.166711953933203372, 0.000000000000000000, -4.439566422914469790 ) ) ;
#80986 = CARTESIAN_POINT ( 'NONE',  ( 6.565887622018943937, 5.165301336597086568, 12.81628187352647430 ) ) ;
#80987 = CARTESIAN_POINT ( 'NONE',  ( 19.42250999205614548, 5.980352010821504471, -5.440088680355545492 ) ) ;
#80988 = CARTESIAN_POINT ( 'NONE',  ( 6.204703633549690345, 12.84541550158063572, 14.16423886937410082 ) ) ;
#80989 = CARTESIAN_POINT ( 'NONE',  ( -12.50534872682722565, 15.00000000000000000, -7.339363270777700343 ) ) ;
#80990 = CARTESIAN_POINT ( 'NONE',  ( 13.79529636645031943, 20.34541550158063572, -14.16423886937409904 ) ) ;
#80991 = CARTESIAN_POINT ( 'NONE',  ( 22.26659068614894466, 38.88708216824731068, 7.082119434687054849 ) ) ;
#80993 = CARTESIAN_POINT ( 'NONE',  ( 2.035157376598824452, 68.68868534415484817, 7.964842623401179544 ) ) ;
#80992 = CARTESIAN_POINT ( 'NONE',  ( 13.79529636645031943, 10.34541550158063394, -14.16423886937409904 ) ) ;
#80994 = CARTESIAN_POINT ( 'NONE',  ( -0.8801773607110991993, 32.85535201082151247, -2.915334737309923874 ) ) ;
#80995 = DIRECTION ( 'NONE',  ( 1.000000000000000000, 0.000000000000000000, 0.000000000000000000 ) ) ;
#80996 = VERTEX_POINT ( 'NONE', #42699 ) ;
#80997 = CARTESIAN_POINT ( 'NONE',  ( 2.791683348922240793, 21.63393115100078745, 7.208316651077764092 ) ) ;
#80999 = CARTESIAN_POINT ( 'NONE',  ( 12.63842701281683034, 27.46726448433411250, 9.846743663894596210 ) ) ;
#80998 = CARTESIAN_POINT ( 'NONE',  ( 17.96484262340118221, 61.18868534415482685, -7.964842623401177768 ) ) ;
#81000 = B_SPLINE_CURVE_WITH_KNOTS ( 'NONE', 3,
 ( #89702, #14720, #221, #60192 ),
 .UNSPECIFIED., .F., .F.,
 ( 4, 4 ),
 ( 0.000000000000000000, 0.001036303429213360086 ),
 .UNSPECIFIED. ) ;
#81001 = CARTESIAN_POINT ( 'NONE',  ( 7.084665262690076126, 17.02201867748817676, -10.88017736071110164 ) ) ;
#81002 = CARTESIAN_POINT ( 'NONE',  ( 3.591859063236761518, 39.95696800326375353, 11.09922568453594849 ) ) ;
#81003 = CARTESIAN_POINT ( 'NONE',  ( 0.1532563361054082862, 51.21726448433412315, 2.638427012816831674 ) ) ;
#81004 = CARTESIAN_POINT ( 'NONE',  ( 0.000000000000000000, 14.49999999999999822, 0.000000000000000000 ) ) ;
#81005 = ADVANCED_FACE ( 'NONE', ( #3727 ), #73176, .T. ) ;
#81006 = CARTESIAN_POINT ( 'NONE',  ( 6.565887622018943937, 48.08196800326375353, -12.81628187352647608 ) ) ;
#81007 = CARTESIAN_POINT ( 'NONE',  ( 14.16423886937410082, -30.48791783175269288, -3.795296366450314096 ) ) ;
#81008 = CARTESIAN_POINT ( 'NONE',  ( 10.00000000000000000, 44.75893115100078745, -9.846743663894594434 ) ) ;
#81009 = CARTESIAN_POINT ( 'NONE',  ( -2.266590686148945544, 27.22041550158063572, 7.082119434687048631 ) ) ;
#81010 = ORIENTED_EDGE ( 'NONE', *, *, #11287, .F. ) ;
#81011 = AXIS2_PLACEMENT_3D ( 'NONE', #34280, #34788, #79805 ) ;
#81012 = CARTESIAN_POINT ( 'NONE',  ( 12.91533473730993009, 46.60535201082150536, -10.88017736071109987 ) ) ;
#81013 = CARTESIAN_POINT ( 'NONE',  ( 2.035157376598822676, 47.43868534415484817, -7.964842623401177768 ) ) ;
#81014 = CARTESIAN_POINT ( 'NONE',  ( 10.00000000000000000, 45.55374883491397497, -14.16423886937410082 ) ) ;
#81015 = CARTESIAN_POINT ( 'NONE',  ( 10.00000000000000000, 64.75893115100078035, -9.846743663894594434 ) ) ;
#81016 = CARTESIAN_POINT ( 'NONE',  ( 0.1916775849787232255, 57.25868815902070708, -6.499999999999983125 ) ) ;
#81017 = CARTESIAN_POINT ( 'NONE',  ( 10.00000000000000178, 39.31368534415484106, 10.88017736071110342 ) ) ;
#81018 = CARTESIAN_POINT ( 'NONE',  ( -4.818654718866499209, -24.96058166501293485, -2.500000000000001776 ) ) ;
#81019 = CARTESIAN_POINT ( 'NONE',  ( 3.591859063236761518, 24.95696800326375353, 11.09922568453594849 ) ) ;
#81020 = CARTESIAN_POINT ( 'NONE',  ( 14.92337183194729988, 54.34226448433412315, -8.527530157486177487 ) ) ;
#81021 = CARTESIAN_POINT ( 'NONE',  ( 2.915334737309921209, 11.60535201082150714, -10.88017736071110164 ) ) ;
#81022 = CARTESIAN_POINT ( 'NONE',  ( 3.969999999999999751, 36.75000000000000000, 2.500000000000000000 ) ) ;
#81023 = ORIENTED_EDGE ( 'NONE', *, *, #47534, .F. ) ;
#81024 = CARTESIAN_POINT ( 'NONE',  ( 7.084665262690076126, 9.105352010821503583, 10.88017736071109987 ) ) ;
#81025 = CARTESIAN_POINT ( 'NONE',  ( 19.72487221294571569, 65.71833443783937412, -6.499999999999983125 ) ) ;
#81026 = CARTESIAN_POINT ( 'NONE',  ( 2.035157376598824452, 63.68868534415484106, 7.964842623401179544 ) ) ;
#81027 = CARTESIAN_POINT ( 'NONE',  ( 1.472469842513823179, 5.592264484334118713, -4.923371831947296329 ) ) ;
#81028 = CARTESIAN_POINT ( 'NONE',  ( 18.00000000000525091, 77.36262727519759608, -4.161036774751641687 ) ) ;
#81029 = CARTESIAN_POINT ( 'NONE',  ( 0.1532563361054083140, 31.00893115100078390, 1.131784320476157264E-15 ) ) ;
#81030 = CARTESIAN_POINT ( 'NONE',  ( 2.035157376598824452, 23.68868534415484461, 7.964842623401179544 ) ) ;
#81031 = CARTESIAN_POINT ( 'NONE',  ( 0.6178305044545818747, 8.498634669930421381, -9.382169495545419124 ) ) ;
#81033 = CARTESIAN_POINT ( 'NONE',  ( -14.09394518620614711, 15.00000000000000000, 3.407449058785264384 ) ) ;
#81032 = CARTESIAN_POINT ( 'NONE',  ( 15.44008868035555793, 36.39701867748816966, -9.422509992056140149 ) ) ;
#81034 = CARTESIAN_POINT ( 'NONE',  ( 18.72515096720591643, 66.07228050351029935, -6.499999999999699796 ) ) ;
#81035 = CARTESIAN_POINT ( 'NONE',  ( 16.40814093676324603, 42.45696800326375353, -11.09922568453594671 ) ) ;
#81036 = ORIENTED_EDGE ( 'NONE', *, *, #83558, .T. ) ;
#81037 = CARTESIAN_POINT ( 'NONE',  ( 7.084665262690076126, 59.10535201082150536, 10.88017736071109987 ) ) ;
#81039 = PLANE ( 'NONE',  #95723 ) ;
#81038 = CARTESIAN_POINT ( 'NONE',  ( 21.09922568453595559, 22.04030133659708923, -6.408140936763230044 ) ) ;
#81040 = CARTESIAN_POINT ( 'NONE',  ( 12.91533473730992121, 34.52201867748817676, 10.88017736071110164 ) ) ;
#81041 = CARTESIAN_POINT ( 'NONE',  ( 0.000000000000000000, 15.00000000000000000, 0.000000000000000000 ) ) ;
#81042 = CARTESIAN_POINT ( 'NONE',  ( 24.16423886937410614, 59.51208216824728936, -3.795296366450302550 ) ) ;
#81043 = AXIS2_PLACEMENT_3D ( 'NONE', #23169, #53647, #15670 ) ;
#81044 = CARTESIAN_POINT ( 'NONE',  ( 17.20831665107776587, 57.88393115100078745, 7.208316651077764980 ) ) ;
#81045 = CARTESIAN_POINT ( 'NONE',  ( 17.20831665107776587, 2.883931151000785231, 7.208316651077764980 ) ) ;
#81046 = CARTESIAN_POINT ( 'NONE',  ( 10.00000000000000178, 64.31368534415483396, 10.88017736071110342 ) ) ;
#81047 = DIRECTION ( 'NONE',  ( 0.000000000000000000, -1.000000000000000000, 0.000000000000000000 ) ) ;
#81048 = CARTESIAN_POINT ( 'NONE',  ( 13.79529636645031943, 25.34541550158063572, -14.16423886937409904 ) ) ;
#81049 = AXIS2_PLACEMENT_3D ( 'NONE', #54166, #16188, #8676 ) ;
#81050 = SURFACE_STYLE_USAGE ( .BOTH. , #44029 ) ;
#81051 = CARTESIAN_POINT ( 'NONE',  ( -10.09048698379360687, 46.92328126389585208, 0.000000000000000000 ) ) ;
#81052 = TOROIDAL_SURFACE ( 'NONE', #37968, 0.5000000000000000000, 0.2500000000000000000 ) ;
#81053 = ORIENTED_EDGE ( 'NONE', *, *, #6012, .T. ) ;
#81054 = ORIENTED_EDGE ( 'NONE', *, *, #76323, .T. ) ;
#81055 = CARTESIAN_POINT ( 'NONE',  ( 10.00000000000000178, 68.05374883491397497, 14.16423886937410082 ) ) ;
#81056 = CARTESIAN_POINT ( 'NONE',  ( 13.79529636645031943, 50.34541550158064638, -14.16423886937409904 ) ) ;
#81057 = CARTESIAN_POINT ( 'NONE',  ( 12.63842701281683034, 32.46726448433412315, 9.846743663894596210 ) ) ;
#81058 = CARTESIAN_POINT ( 'NONE',  ( 21.09922568453594849, 31.20696800326375353, 6.408140936763242479 ) ) ;
#81059 = DIRECTION ( 'NONE',  ( -0.9304175679820255729, 0.000000000000000000, 0.3665012267242946931 ) ) ;
#81060 = CARTESIAN_POINT ( 'NONE',  ( -12.25993886608597094, 14.49999999999999112, -8.642563219313844414 ) ) ;
#81061 = CARTESIAN_POINT ( 'NONE',  ( -0.8801773607111009756, 3.063685344154837509, 1.068504757029289695E-15 ) ) ;
#81062 = CARTESIAN_POINT ( 'NONE',  ( 22.26659068614895176, 59.72041550158063927, -7.082119434687042414 ) ) ;
#81063 = EDGE_CURVE ( 'NONE', #22152, #61681, #4580, .T. ) ;
#81064 = EDGE_CURVE ( 'NONE', #16885, #3586, #98151, .T. ) ;
#81065 = CARTESIAN_POINT ( 'NONE',  ( -13.48086198287156101, 15.00000000000000000, -8.610676897597642210 ) ) ;
#81066 = CARTESIAN_POINT ( 'NONE',  ( 17.20831665107776587, 12.88393115100078390, 7.208316651077764980 ) ) ;
#81067 = DIRECTION ( 'NONE',  ( -0.000000000000000000, -0.000000000000000000, -1.000000000000000000 ) ) ;
#81068 = CARTESIAN_POINT ( 'NONE',  ( -3.469446951953614189E-15, 4.758931151000789228, -9.846743663894594434 ) ) ;
#81069 = VERTEX_POINT ( 'NONE', #96703 ) ;
#81070 = ORIENTED_EDGE ( 'NONE', *, *, #81939, .T. ) ;
#81071 = CARTESIAN_POINT ( 'NONE',  ( 12.83294900548058415, 15.00000000000000000, 7.766300266068450142 ) ) ;
#81072 = ORIENTED_EDGE ( 'NONE', *, *, #92033, .T. ) ;
#81073 = CARTESIAN_POINT ( 'NONE',  ( 17.08211943468705130, 13.47041550158063572, 12.26659068614894998 ) ) ;
#81075 = CARTESIAN_POINT ( 'NONE',  ( 7.084665262690076126, 27.02201867748817676, -10.88017736071110164 ) ) ;
#81074 = CARTESIAN_POINT ( 'NONE',  ( 4.559911319644449179, 13.89701867748817321, 9.422509992056141925 ) ) ;
#81077 = CARTESIAN_POINT ( 'NONE',  ( 16.40814093676324603, 12.45696800326375353, -11.09922568453594671 ) ) ;
#81076 = CARTESIAN_POINT ( 'NONE',  ( 19.84674366389459266, 53.71726448433411605, -2.638427012816827677 ) ) ;
#81078 = DIRECTION ( 'NONE',  ( -0.8141155183563145714, 0.000000000000000000, -0.5807029557109463225 ) ) ;
#81079 = CARTESIAN_POINT ( 'NONE',  ( 3.591859063236763294, 28.29030133659708568, -11.09922568453595026 ) ) ;
#81080 = VERTEX_POINT ( 'NONE', #57689 ) ;
#81081 = CARTESIAN_POINT ( 'NONE',  ( 12.63842701281683034, 37.46726448433411605, 9.846743663894596210 ) ) ;
#81082 = CARTESIAN_POINT ( 'NONE',  ( 24.16423886937410614, 64.30374883491396076, 8.672049930838204340E-16 ) ) ;
#81083 = ORIENTED_EDGE ( 'NONE', *, *, #91110, .T. ) ;
#81084 = EDGE_CURVE ( 'NONE', #34211, #88366, #65282, .T. ) ;
#81085 = CARTESIAN_POINT ( 'NONE',  ( 10.00000000000000000, 6.813685344154838397, -10.88017736071110342 ) ) ;
#81086 = ORIENTED_EDGE ( 'NONE', *, *, #26747, .F. ) ;
#81087 = CARTESIAN_POINT ( 'NONE',  ( 7.084665262690076126, 44.10535201082151247, 10.88017736071109987 ) ) ;
#81088 = CARTESIAN_POINT ( 'NONE',  ( 0.5774900079438590739, 42.64701867748816966, -5.440088680355550821 ) ) ;
#81089 = CARTESIAN_POINT ( 'NONE',  ( 0.5774900079438590739, 47.64701867748817676, -5.440088680355550821 ) ) ;
#81090 = CARTESIAN_POINT ( 'NONE',  ( 0.000000000000000000, 0.000000000000000000, 0.000000000000000000 ) ) ;
#81091 = CARTESIAN_POINT ( 'NONE',  ( -0.8801773607111009756, 38.06368534415484106, 1.068504757029289695E-15 ) ) ;
#81092 = CARTESIAN_POINT ( 'NONE',  ( -5.991992585808713301, 15.00000000000000000, 13.20401548210291054 ) ) ;
#81094 = ORIENTED_EDGE ( 'NONE', *, *, #39298, .T. ) ;
#81093 = DIRECTION ( 'NONE',  ( -0.000000000000000000, -1.000000000000000000, -0.000000000000000000 ) ) ;
#81095 = CARTESIAN_POINT ( 'NONE',  ( 17.20831665107776587, 22.88393115100078745, 7.208316651077764980 ) ) ;
#81096 = ORIENTED_EDGE ( 'NONE', *, *, #21818, .T. ) ;
#81097 = CARTESIAN_POINT ( 'NONE',  ( 18.52753015748618282, 58.92559781766745886, -4.923371831947291888 ) ) ;
#81098 = FACE_OUTER_BOUND ( 'NONE', #47741, .T. ) ;
#81099 = SURFACE_STYLE_FILL_AREA ( #56635 ) ;
#81100 = CIRCLE ( 'NONE', #15689, 0.2500000000000002220 ) ;
#81101 = ORIENTED_EDGE ( 'NONE', *, *, #94961, .T. ) ;
#81102 = CARTESIAN_POINT ( 'NONE',  ( -9.705452947461466806, 12.49999999999999289, -5.689172442861226031 ) ) ;
#81103 = CARTESIAN_POINT ( 'NONE',  ( -8.000000000000000000, 41.24999999999999289, -6.250000000000000000 ) ) ;
#81104 = CARTESIAN_POINT ( 'NONE',  ( -10.09048698379360687, 46.92328126389585208, 3.000000000000000000 ) ) ;
#81105 = CARTESIAN_POINT ( 'NONE',  ( 20.36894250292379382, 63.67874883491396787, 10.36894250292379205 ) ) ;
#81106 = CARTESIAN_POINT ( 'NONE',  ( -0.1503990784575275907, 58.10158574516644592, 6.262539305110076171 ) ) ;
#81107 = ORIENTED_EDGE ( 'NONE', *, *, #52473, .F. ) ;
#81108 = DIRECTION ( 'NONE',  ( 0.000000000000000000, 0.000000000000000000, 1.000000000000000000 ) ) ;
#81109 = CARTESIAN_POINT ( 'NONE',  ( 5.076628168052704559, 30.17559781766745175, -8.527530157486179263 ) ) ;
#81110 = DIRECTION ( 'NONE',  ( 0.000000000000000000, -1.000000000000000000, 0.000000000000000000 ) ) ;
#81111 = CARTESIAN_POINT ( 'NONE',  ( 13.43411237798106583, 7.665301336597086568, -12.81628187352647252 ) ) ;
#81112 = CARTESIAN_POINT ( 'NONE',  ( 10.00000000000000000, 4.758931151000784787, -9.846743663894594434 ) ) ;
#81113 = DIRECTION ( 'NONE',  ( 0.000000000000000000, 1.000000000000000000, 0.000000000000000000 ) ) ;
#81114 = CARTESIAN_POINT ( 'NONE',  ( 5.076628168052704559, 10.17559781766745175, -8.527530157486179263 ) ) ;
#81115 = CARTESIAN_POINT ( 'NONE',  ( 12.63842701281683922, 59.55059781766744464, -9.846743663894590881 ) ) ;
#81116 = VECTOR ( 'NONE', #97693, 1000.000000000000000 ) ;
#81117 = DIRECTION ( 'NONE',  ( 0.000000000000000000, 0.000000000000000000, -1.000000000000000000 ) ) ;
#81118 = ORIENTED_EDGE ( 'NONE', *, *, #89195, .T. ) ;
#81119 = CARTESIAN_POINT ( 'NONE',  ( 15.44008868035555260, 9.730352010821505360, 9.422509992056143702 ) ) ;
#81120 = CARTESIAN_POINT ( 'NONE',  ( -0.3689425029237881626, 7.428748834913967869, 10.36894250292379027 ) ) ;
#81121 = CARTESIAN_POINT ( 'NONE',  ( 19.84674366389459621, 13.50893115100078568, 7.409399052514197653E-17 ) ) ;
#81122 = CARTESIAN_POINT ( 'NONE',  ( 10.00000000000000000, 51.81368534415484106, -10.88017736071110342 ) ) ;
#81124 = DIRECTION ( 'NONE',  ( 1.000000000000000000, 0.000000000000000000, 0.000000000000000000 ) ) ;
#81123 = CARTESIAN_POINT ( 'NONE',  ( 16.40814093676324603, 27.45696800326375708, -11.09922568453594671 ) ) ;
#81125 = CARTESIAN_POINT ( 'NONE',  ( -4.000000000000000000, 37.00000000000000000, -2.500000000000000000 ) ) ;
#81126 = DIRECTION ( 'NONE',  ( -0.000000000000000000, -0.000000000000000000, 1.000000000000000000 ) ) ;
#81127 = CARTESIAN_POINT ( 'NONE',  ( 32.06412365047463453, 14.00000000000001066, 10.00000000000000000 ) ) ;
#81128 = CARTESIAN_POINT ( 'NONE',  ( 19.84674366389459266, 63.71726448433412315, -2.638427012816827677 ) ) ;
#81129 = CARTESIAN_POINT ( 'NONE',  ( 17.20831665107776587, 14.13393115100078568, -7.208316651077762316 ) ) ;
#81130 = CARTESIAN_POINT ( 'NONE',  ( -5.204170427930421283E-15, -28.18631465584515894, -10.88017736071110342 ) ) ;
#81131 = CARTESIAN_POINT ( 'NONE',  ( -2.816281873526473856, 19.12363466993042138, 9.499525473075851096E-16 ) ) ;
#81132 = CARTESIAN_POINT ( 'NONE',  ( 2.153642693323417845, 51.13791097397318453, -6.499999999999929834 ) ) ;
#81134 = LINE ( 'NONE', #10679, #8077 ) ;
#81133 = CARTESIAN_POINT ( 'NONE',  ( 12.91533473730993009, 21.60535201082150536, -10.88017736071109987 ) ) ;
#81135 = CARTESIAN_POINT ( 'NONE',  ( -9.997910040112463648, 15.00000000000000000, -10.50199004140731773 ) ) ;
#81136 = EDGE_CURVE ( 'NONE', #84772, #41516, #73555, .T. ) ;
#81137 = CARTESIAN_POINT ( 'NONE',  ( 24.16423886937410614, 54.30374883491396787, 8.672049930838204340E-16 ) ) ;
#81138 = CARTESIAN_POINT ( 'NONE',  ( 13.82671409943293739, 15.00000000000000000, 3.447387012295318076 ) ) ;
#81139 = CARTESIAN_POINT ( 'NONE',  ( 19.42250999205614193, 30.14701867748817321, 5.440088680355555262 ) ) ;
#81140 = CARTESIAN_POINT ( 'NONE',  ( 0.1532563361054082862, 51.21726448433412315, 2.638427012816831674 ) ) ;
#81141 = CARTESIAN_POINT ( 'NONE',  ( -0.8801773607110991993, 47.85535201082150536, -2.915334737309923874 ) ) ;
#81142 = CARTESIAN_POINT ( 'NONE',  ( 24.16423886937410614, 34.51208216824731068, -3.795296366450302550 ) ) ;
#81143 = LINE ( 'NONE', #72647, #48742 ) ;
#81144 = UNCERTAINTY_MEASURE_WITH_UNIT (LENGTH_MEASURE( 1.000000000000000082E-05 ), #82421, 'distance_accuracy_value', 'NONE');
#81145 = CARTESIAN_POINT ( 'NONE',  ( 7.361572987183169658, 39.96726448433411605, -9.846743663894592657 ) ) ;
#81146 = DIRECTION ( 'NONE',  ( 0.000000000000000000, 0.000000000000000000, 1.000000000000000000 ) ) ;
#81147 = CARTESIAN_POINT ( 'NONE',  ( 17.20831665107776587, 62.88393115100078745, 7.208316651077764980 ) ) ;
#81148 = ORIENTED_EDGE ( 'NONE', *, *, #55529, .F. ) ;
#81149 = CARTESIAN_POINT ( 'NONE',  ( 17.96484262340118221, 31.18868534415483751, -7.964842623401177768 ) ) ;
#81150 = DIRECTION ( 'NONE',  ( 0.6087614290087186575, -0.000000000000000000, 0.7933533402912366084 ) ) ;
#81151 = DIRECTION ( 'NONE',  ( -0.000000000000000000, 0.000000000000000000, 1.000000000000000000 ) ) ;
#81152 = CARTESIAN_POINT ( 'NONE',  ( 12.91533473730992121, 9.522018677488171434, 10.88017736071110164 ) ) ;
#81153 = CARTESIAN_POINT ( 'NONE',  ( 1.472469842513823179, 5.592264484334118713, -4.923371831947296329 ) ) ;
#81154 = CARTESIAN_POINT ( 'NONE',  ( 22.26659068614894466, 28.88708216824730357, 7.082119434687054849 ) ) ;
#81155 = CARTESIAN_POINT ( 'NONE',  ( 17.20831665107776587, 12.88393115100078390, 7.208316651077764980 ) ) ;
#81156 = CARTESIAN_POINT ( 'NONE',  ( 10.00000000000000178, 62.25893115100078745, 9.846743663894594434 ) ) ;
#81157 = CARTESIAN_POINT ( 'NONE',  ( 0.5774900079438590739, 32.64701867748816966, -5.440088680355550821 ) ) ;
#81158 = CARTESIAN_POINT ( 'NONE',  ( -0.03743638938522143161, 34.25197528031020511, -6.399506433553973750 ) ) ;
#81159 = DIRECTION ( 'NONE',  ( 1.000000000000000000, -5.818595309480552676E-17, 0.000000000000000000 ) ) ;
#81160 = EDGE_CURVE ( 'NONE', #19902, #54884, #35565, .T. ) ;
#81161 = ORIENTED_EDGE ( 'NONE', *, *, #19580, .F. ) ;
#81162 = UNCERTAINTY_MEASURE_WITH_UNIT (LENGTH_MEASURE( 1.000000000000000082E-05 ), #4389, 'distance_accuracy_value', 'NONE');
#81163 = SHAPE_REPRESENTATION ( '1.3 Adjustment Nut', ( #27931 ), #10314 ) ;
#81164 = MECHANICAL_DESIGN_GEOMETRIC_PRESENTATION_REPRESENTATION (  '', ( #89159 ), #77963 ) ;
#81165 = CARTESIAN_POINT ( 'NONE',  ( 4.221203097590866982, -3.619724449986670756, 2.500000000000000000 ) ) ;
#81166 = CARTESIAN_POINT ( 'NONE',  ( 1.472469842513823179, 50.59226448433411605, -4.923371831947296329 ) ) ;
#81168 = ORIENTED_EDGE ( 'NONE', *, *, #28883, .F. ) ;
#81167 = EDGE_CURVE ( 'NONE', #78236, #38312, #94328, .T. ) ;
#81169 = ORIENTED_EDGE ( 'NONE', *, *, #96522, .F. ) ;
#81170 = PRESENTATION_STYLE_ASSIGNMENT (( #35672 ) ) ;
#81171 = CARTESIAN_POINT ( 'NONE',  ( -0.3689425029237898834, 26.17874883491396432, -10.36894250292378850 ) ) ;
#81172 = CARTESIAN_POINT ( 'NONE',  ( -0.3689425029237881626, 7.428748834913967869, 10.36894250292379027 ) ) ;
#81173 = CARTESIAN_POINT ( 'NONE',  ( 19.42250999205614548, 55.98035201082150536, -5.440088680355545492 ) ) ;
#81174 = CARTESIAN_POINT ( 'NONE',  ( 24.16423886937410614, 49.30374883491396787, 8.672049930838204340E-16 ) ) ;
#81175 = CARTESIAN_POINT ( 'NONE',  ( 5.076628168052703671, 66.84226448433412315, 8.527530157486179263 ) ) ;
#81176 = CARTESIAN_POINT ( 'NONE',  ( 7.361572987183169658, 29.96726448433411960, -9.846743663894592657 ) ) ;
#81177 = CARTESIAN_POINT ( 'NONE',  ( -11.20041124669619670, -94.46430075987372277, 3.999999999999099387 ) ) ;
#81179 = CARTESIAN_POINT ( 'NONE',  ( 13.43411237798106583, 12.66530133659708746, -12.81628187352647252 ) ) ;
#81178 = CARTESIAN_POINT ( 'NONE',  ( 7.084665262690076126, 37.02201867748817676, -10.88017736071110164 ) ) ;
#81180 = CARTESIAN_POINT ( 'NONE',  ( 6.204703633549690345, 47.84541550158064638, 14.16423886937410082 ) ) ;
#81181 = EDGE_CURVE ( 'NONE', #27759, #87330, #76951, .T. ) ;
#81182 = CARTESIAN_POINT ( 'NONE',  ( -0.8801773607111008646, 13.27201867748817321, 2.915334737309923430 ) ) ;
#81183 = CARTESIAN_POINT ( 'NONE',  ( -0.1503990784575247319, 67.22266099184919597, -6.262539305110083276 ) ) ;
#81184 = CARTESIAN_POINT ( 'NONE',  ( -14.71525861348291997, 0.5000000000000004441, 2.908807992686483601 ) ) ;
#81185 = CARTESIAN_POINT ( 'NONE',  ( 20.88017736071110164, 45.35535201082149115, 2.915334737309930979 ) ) ;
#81186 = AXIS2_PLACEMENT_3D ( 'NONE', #3941, #64901, #95427 ) ;
#81187 = CARTESIAN_POINT ( 'NONE',  ( 3.469446951953614189E-15, -32.74106884899921255, 9.846743663894594434 ) ) ;
#81188 = EDGE_LOOP ( 'NONE', ( #74874, #42346, #84168, #93744 ) ) ;
#81189 = CARTESIAN_POINT ( 'NONE',  ( 8.879999999999991900, 76.07179676972447169, 6.250000000000000000 ) ) ;
#81190 = ORIENTED_EDGE ( 'NONE', *, *, #620, .T. ) ;
#81191 = VERTEX_POINT ( 'NONE', #35058 ) ;
#81192 = CARTESIAN_POINT ( 'NONE',  ( 13.79529636645031943, 50.34541550158064638, -14.16423886937409904 ) ) ;
#81193 = CARTESIAN_POINT ( 'NONE',  ( 0.1532563361054082862, 41.21726448433411605, 2.638427012816831674 ) ) ;
#81194 = CARTESIAN_POINT ( 'NONE',  ( 10.00000000000000178, 59.31368534415484106, 10.88017736071110342 ) ) ;
#81195 = AXIS2_PLACEMENT_3D ( 'NONE', #98302, #6285, #36788 ) ;
#81196 = DIRECTION ( 'NONE',  ( 0.000000000000000000, 0.000000000000000000, 1.000000000000000000 ) ) ;
#81197 = CARTESIAN_POINT ( 'NONE',  ( -0.8801773607111008646, 48.27201867748816966, 2.915334737309923430 ) ) ;
#81198 = EDGE_CURVE ( 'NONE', #765, #31971, #48180, .T. ) ;
#81199 = CARTESIAN_POINT ( 'NONE',  ( -1.099225684535947600, 59.54030133659708923, 6.408140936763237150 ) ) ;
#81200 = CARTESIAN_POINT ( 'NONE',  ( -12.81628187352647252, 9.331968003263757083, 3.434112377981066722 ) ) ;
#81201 = VERTEX_POINT ( 'NONE', #51563 ) ;
#81202 = CARTESIAN_POINT ( 'NONE',  ( 7.084665262690076126, 47.02201867748818387, -10.88017736071110164 ) ) ;
#81203 = CARTESIAN_POINT ( 'NONE',  ( 24.16423886937410614, 14.51208216824730179, -3.795296366450302550 ) ) ;
#81204 = EDGE_CURVE ( 'NONE', #78249, #29252, #98070, .T. ) ;
#81205 = CARTESIAN_POINT ( 'NONE',  ( 19.38216949554541557, 22.24863466993041428, -9.382169495545420901 ) ) ;
#81206 = VERTEX_POINT ( 'NONE', #27565 ) ;
#81207 = CARTESIAN_POINT ( 'NONE',  ( 22.81628187352648496, 46.83196800326376064, -3.434112377981050290 ) ) ;
#81208 = CARTESIAN_POINT ( 'NONE',  ( 12.91533473730992121, 14.52201867748817143, 10.88017736071110164 ) ) ;
#81209 = CARTESIAN_POINT ( 'NONE',  ( 18.52753015748617571, 33.09226448433411605, 4.923371831947298993 ) ) ;
#81210 = CARTESIAN_POINT ( 'NONE',  ( 7.084665262690076126, 12.02201867748817143, -10.88017736071110164 ) ) ;
#81211 = CARTESIAN_POINT ( 'NONE',  ( 21.09922568453594849, 56.20696800326375353, 6.408140936763242479 ) ) ;
#81212 = FACE_OUTER_BOUND ( 'NONE', #32809, .T. ) ;
#81213 = CARTESIAN_POINT ( 'NONE',  ( 14.92337183194729633, 47.67559781766745175, 8.527530157486181039 ) ) ;
#81215 = VERTEX_POINT ( 'NONE', #6066 ) ;
#81214 = CARTESIAN_POINT ( 'NONE',  ( 2.035157376598824452, 68.68868534415484817, 7.964842623401179544 ) ) ;
#81216 = LINE ( 'NONE', #44192, #91391 ) ;
#81217 = CARTESIAN_POINT ( 'NONE',  ( -9.322910753577803078, 0.04922511925148240902, -11.43369735623891081 ) ) ;
#81218 = CARTESIAN_POINT ( 'NONE',  ( 1.780824192092501423, 0.5000000000000004441, -14.89391369643513485 ) ) ;
#81219 = CARTESIAN_POINT ( 'NONE',  ( 18.52753015748618282, 23.92559781766745530, -4.923371831947291888 ) ) ;
#81220 = CARTESIAN_POINT ( 'NONE',  ( 13.43411237798105340, 25.58196800326374998, 12.81628187352647963 ) ) ;
#81221 = DIRECTION ( 'NONE',  ( -0.07626964003977219908, 0.9970872288863213972, 0.000000000000000000 ) ) ;
#81222 = ORIENTED_EDGE ( 'NONE', *, *, #88059, .F. ) ;
#81223 = AXIS2_PLACEMENT_3D ( 'NONE', #11181, #41701, #20158 ) ;
#81224 = CARTESIAN_POINT ( 'NONE',  ( 12.63842701281683034, 62.46726448433410894, 9.846743663894596210 ) ) ;
#81225 = CARTESIAN_POINT ( 'NONE',  ( -13.34343830728394309, 0.5000000000000004441, -6.852200678592783589 ) ) ;
#81226 = CARTESIAN_POINT ( 'NONE',  ( 2.917880565312950480, 25.97041550158063572, -12.26659068614894821 ) ) ;
#81227 = CARTESIAN_POINT ( 'NONE',  ( 7.361572987183170547, 32.05059781766745175, 9.846743663894590881 ) ) ;
#81228 = CARTESIAN_POINT ( 'NONE',  ( 3.591859063236761518, 44.95696800326376064, 11.09922568453594849 ) ) ;
#81230 = DIRECTION ( 'NONE',  ( -0.000000000000000000, -0.000000000000000000, 1.000000000000000000 ) ) ;
#81229 = DIRECTION ( 'NONE',  ( 1.000000000000000000, -5.818595309480553908E-17, 0.000000000000000000 ) ) ;
#81231 = CARTESIAN_POINT ( 'NONE',  ( -0.8801773607111008646, 63.27201867748817676, 2.915334737309923430 ) ) ;
#81232 = FACE_OUTER_BOUND ( 'NONE', #81289, .T. ) ;
#81233 = CARTESIAN_POINT ( 'NONE',  ( 1.472469842513823179, 41.42559781766745886, 4.923371831947296329 ) ) ;
#81234 = CARTESIAN_POINT ( 'NONE',  ( 20.88017736071110164, 35.35535201082150536, 2.915334737309930979 ) ) ;
#81235 = CARTESIAN_POINT ( 'NONE',  ( -2.816281873526473856, 44.33196800326375353, 3.434112377981055619 ) ) ;
#81236 = CYLINDRICAL_SURFACE ( 'NONE', #95447, 0.5000000000000004441 ) ;
#81237 = CARTESIAN_POINT ( 'NONE',  ( 7.084665262690076126, 37.02201867748817676, -10.88017736071110164 ) ) ;
#81238 = VERTEX_POINT ( 'NONE', #51060 ) ;
#81239 = CARTESIAN_POINT ( 'NONE',  ( -0.8801773607111008646, 68.27201867748817676, 2.915334737309923430 ) ) ;
#81240 = CARTESIAN_POINT ( 'NONE',  ( 20.88017736071110164, 15.35535201082150358, 2.915334737309930979 ) ) ;
#81242 = CARTESIAN_POINT ( 'NONE',  ( 19.42250999205614548, 35.98035201082151247, -5.440088680355545492 ) ) ;
#81241 = CARTESIAN_POINT ( 'NONE',  ( 12.63842701281683034, 52.46726448433413026, 9.846743663894596210 ) ) ;
#81243 = DIRECTION ( 'NONE',  ( -0.000000000000000000, -0.000000000000000000, 1.000000000000000000 ) ) ;
#81244 = CARTESIAN_POINT ( 'NONE',  ( -0.8801773607110991993, 62.85535201082150536, -2.915334737309923874 ) ) ;
#81245 = AXIS2_PLACEMENT_3D ( 'NONE', #36943, #67440, #329 ) ;
#81247 = CARTESIAN_POINT ( 'NONE',  ( 0.000000000000000000, 76.61857121896082390, -7.300603792374249501 ) ) ;
#81246 = CARTESIAN_POINT ( 'NONE',  ( -0.8801773607111008646, 23.27201867748817676, 2.915334737309923430 ) ) ;
#81248 = CARTESIAN_POINT ( 'NONE',  ( 5.076628168052704559, 0.1755978176674514724, -8.527530157486179263 ) ) ;
#81249 = CARTESIAN_POINT ( 'NONE',  ( 10.00000000000000000, 29.75893115100078745, -9.846743663894594434 ) ) ;
#81250 = CARTESIAN_POINT ( 'NONE',  ( 14.62617646268085281, 0.5000000000000004441, 3.327906561566980503 ) ) ;
#81251 = CARTESIAN_POINT ( 'NONE',  ( -3.795296366450300773, 7.845415501580634832, 14.16423886937410437 ) ) ;
#81252 = CARTESIAN_POINT ( 'NONE',  ( 10.00000000000000000, 54.75893115100078745, -9.846743663894594434 ) ) ;
#81254 = CARTESIAN_POINT ( 'NONE',  ( 4.920153426831056720, -13.81781469843442345, 3.749999999999998668 ) ) ;
#81253 = CARTESIAN_POINT ( 'NONE',  ( 24.16423886937410614, 59.51208216824728936, -3.795296366450302550 ) ) ;
#81255 =( NAMED_UNIT ( * ) PLANE_ANGLE_UNIT ( ) SI_UNIT ( $, .RADIAN. ) );
#81256 = EDGE_CURVE ( 'NONE', #95526, #8937, #52056, .T. ) ;
#81258 = CARTESIAN_POINT ( 'NONE',  ( 24.16423886937409904, 9.095415501580633943, 3.795296366450317205 ) ) ;
#81257 = VECTOR ( 'NONE', #77133, 1000.000000000000000 ) ;
#81259 = CARTESIAN_POINT ( 'NONE',  ( -4.164238869374099927, 37.01208216824731068, 3.795296366450308767 ) ) ;
#81260 = CARTESIAN_POINT ( 'NONE',  ( 16.40814093676324603, 2.456968003263753531, -11.09922568453594671 ) ) ;
#81261 = ORIENTED_EDGE ( 'NONE', *, *, #95766, .F. ) ;
#81262 = CARTESIAN_POINT ( 'NONE',  ( 2.035157376598822676, 7.438685344154837509, -7.964842623401177768 ) ) ;
#81263 = CARTESIAN_POINT ( 'NONE',  ( 0.1532563361054083140, 41.00893115100078745, 1.131784320476157264E-15 ) ) ;
#81265 = DIRECTION ( 'NONE',  ( 0.000000000000000000, 0.000000000000000000, 1.000000000000000000 ) ) ;
#81264 = CARTESIAN_POINT ( 'NONE',  ( 10.00000000000000000, 0.5537488349139675359, -14.16423886937410082 ) ) ;
#81266 = CARTESIAN_POINT ( 'NONE',  ( 18.00000000000000000, 84.07179676972448590, -3.750000000000000000 ) ) ;
#81267 = CARTESIAN_POINT ( 'NONE',  ( 19.84674366389459266, 3.717264484334118713, -2.638427012816827677 ) ) ;
#81268 = CARTESIAN_POINT ( 'NONE',  ( 6.565887622018943937, 28.08196800326375353, -12.81628187352647608 ) ) ;
#81269 = CARTESIAN_POINT ( 'NONE',  ( 10.00000000000000178, 27.25893115100078390, 9.846743663894594434 ) ) ;
#81270 = ORIENTED_EDGE ( 'NONE', *, *, #61286, .F. ) ;
#81271 = CARTESIAN_POINT ( 'NONE',  ( 14.92337183194729988, 14.34226448433411782, -8.527530157486177487 ) ) ;
#81272 = CARTESIAN_POINT ( 'NONE',  ( -11.35178980618960409, 0.5000000000000004441, -9.804941009312079458 ) ) ;
#81273 = CARTESIAN_POINT ( 'NONE',  ( 17.96484262340118221, 6.188685344154837509, -7.964842623401177768 ) ) ;
#81274 = CARTESIAN_POINT ( 'NONE',  ( 20.88017736071110875, 20.77201867748816611, -2.915334737309920765 ) ) ;
#81275 = CARTESIAN_POINT ( 'NONE',  ( -0.3689425029237898834, 36.17874883491396787, -10.36894250292378850 ) ) ;
#81276 = CARTESIAN_POINT ( 'NONE',  ( 10.00000000000000000, 31.81368534415483751, -10.88017736071110342 ) ) ;
#81277 = CARTESIAN_POINT ( 'NONE',  ( 19.42250999205614548, 65.98035201082151957, -5.440088680355545492 ) ) ;
#81278 = DIRECTION ( 'NONE',  ( 1.000000000000000000, -5.818595309480553908E-17, 0.000000000000000000 ) ) ;
#81279 = CARTESIAN_POINT ( 'NONE',  ( 21.92686044187656691, 39.95379003517447813, 3.195792623639537755 ) ) ;
#81280 = CARTESIAN_POINT ( 'NONE',  ( 10.00000000000000000, 29.75893115100078745, -9.846743663894594434 ) ) ;
#81281 = DIRECTION ( 'NONE',  ( -1.000000000000000000, -0.000000000000000000, -0.000000000000000000 ) ) ;
#81282 = CARTESIAN_POINT ( 'NONE',  ( 1.472469842513823179, 10.59226448433411782, -4.923371831947296329 ) ) ;
#81283 = CARTESIAN_POINT ( 'NONE',  ( -11.75249112336564394, 14.95037104119133886, 8.918310463590344739 ) ) ;
#81284 = CARTESIAN_POINT ( 'NONE',  ( 12.63842701281683034, 32.46726448433412315, 9.846743663894596210 ) ) ;
#81285 = CARTESIAN_POINT ( 'NONE',  ( 6.565887622018943937, -1.918031996736246692, -12.81628187352647608 ) ) ;
#81286 = CARTESIAN_POINT ( 'NONE',  ( 17.96484262340118221, 41.18868534415484106, -7.964842623401177768 ) ) ;
#81287 = UNCERTAINTY_MEASURE_WITH_UNIT (LENGTH_MEASURE( 1.000000000000000082E-05 ), #85310, 'distance_accuracy_value', 'NONE');
#81288 = EDGE_CURVE ( 'NONE', #14954, #65595, #87962, .T. ) ;
#81289 = EDGE_LOOP ( 'NONE', ( #24671, #54023, #92559, #65590 ) ) ;
#81290 = CARTESIAN_POINT ( 'NONE',  ( 16.40814093676323893, 45.79030133659708923, 11.09922568453595026 ) ) ;
#81291 = CARTESIAN_POINT ( 'NONE',  ( 20.88017736071110519, 60.56368534415484106, 2.639326808657452039E-16 ) ) ;
#81292 = CARTESIAN_POINT ( 'NONE',  ( -1.099225684535947600, 44.54030133659708923, 6.408140936763237150 ) ) ;
#81294 = CARTESIAN_POINT ( 'NONE',  ( 19.84674366389459266, 33.71726448433410894, -2.638427012816827677 ) ) ;
#81293 = CARTESIAN_POINT ( 'NONE',  ( 24.16423886937409904, 54.09541550158063217, 3.795296366450317205 ) ) ;
#81295 = CYLINDRICAL_SURFACE ( 'NONE', #77362, 10.90000000000026326 ) ;
#81296 = CARTESIAN_POINT ( 'NONE',  ( 7.361572987183170547, 67.05059781766746596, 9.846743663894590881 ) ) ;
#81297 = B_SPLINE_CURVE_WITH_KNOTS ( 'NONE', 3,
 ( #89708, #36220, #20232, #80236, #35724, #89222 ),
 .UNSPECIFIED., .F., .F.,
 ( 4, 2, 4 ),
 ( 3.409110551463477909E-05, 0.0004400426677364613652, 0.0008459942299582879580 ),
 .UNSPECIFIED. ) ;
#81298 = ADVANCED_FACE ( 'NONE', ( #74549 ), #58060, .T. ) ;
#81299 = CARTESIAN_POINT ( 'NONE',  ( -2.266590686148945544, 46.38708216824730357, -7.082119434687050408 ) ) ;
#81300 = CARTESIAN_POINT ( 'NONE',  ( 14.92337183194729988, 44.34226448433412315, -8.527530157486177487 ) ) ;
#81301 = DIRECTION ( 'NONE',  ( 0.000000000000000000, 0.000000000000000000, 1.000000000000000000 ) ) ;
#81302 = CARTESIAN_POINT ( 'NONE',  ( 4.559911319644449179, 33.89701867748817676, 9.422509992056141925 ) ) ;
#81303 = CARTESIAN_POINT ( 'NONE',  ( -0.8801773607110991993, 57.85535201082149825, -2.915334737309923874 ) ) ;
#81304 = VECTOR ( 'NONE', #83463, 1000.000000000000000 ) ;
#81305 = CARTESIAN_POINT ( 'NONE',  ( 2.603489959281614308, 56.58210964143329846, 6.500000000000031086 ) ) ;
#81306 = ORIENTED_EDGE ( 'NONE', *, *, #93354, .T. ) ;
#81307 = CARTESIAN_POINT ( 'NONE',  ( 22.81628187352647785, 46.62363466993041783, 6.195893100308588602E-16 ) ) ;
#81308 = ORIENTED_EDGE ( 'NONE', *, *, #84118, .T. ) ;
#81309 = CARTESIAN_POINT ( 'NONE',  ( 17.96484262340118221, 61.18868534415482685, -7.964842623401177768 ) ) ;
#81310 = VERTEX_POINT ( 'NONE', #50571 ) ;
#81311 = CARTESIAN_POINT ( 'NONE',  ( -4.164238869374099039, 6.803748834913967869, 8.674139862899312516E-16 ) ) ;
#81312 = CARTESIAN_POINT ( 'NONE',  ( 12.63842701281683034, 2.467264484334118269, 9.846743663894596210 ) ) ;
#81313 = LINE ( 'NONE', #59787, #88736 ) ;
#81314 = ORIENTED_EDGE ( 'NONE', *, *, #58243, .T. ) ;
#81315 = CARTESIAN_POINT ( 'NONE',  ( -4.000000000000000000, 36.75000000000000000, -2.500000000000000000 ) ) ;
#81316 = CARTESIAN_POINT ( 'NONE',  ( 7.084665262690076126, 12.02201867748817143, -10.88017736071110164 ) ) ;
#81317 = CARTESIAN_POINT ( 'NONE',  ( -11.92686044187656336, 12.87045670184115487, 3.195792623639540864 ) ) ;
#81318 = EDGE_CURVE ( 'NONE', #37243, #91269, #29055, .T. ) ;
#81319 = ADVANCED_FACE ( 'NONE', ( #14066 ), #57816, .T. ) ;
#81320 = CARTESIAN_POINT ( 'NONE',  ( 2.917880565312948704, 17.63708216824730357, 12.26659068614894643 ) ) ;
#81321 = CARTESIAN_POINT ( 'NONE',  ( 12.91533473730992121, 19.52201867748816611, 10.88017736071110164 ) ) ;
#81322 = CARTESIAN_POINT ( 'NONE',  ( 0.1532563361054083140, 66.00893115100079456, 1.131784320476157264E-15 ) ) ;
#81323 = ORIENTED_EDGE ( 'NONE', *, *, #70402, .T. ) ;
#81324 = CARTESIAN_POINT ( 'NONE',  ( 19.84674366389459621, 58.50893115100078745, 7.409399052514197653E-17 ) ) ;
#81325 = ORIENTED_EDGE ( 'NONE', *, *, #42056, .F. ) ;
#81326 = CARTESIAN_POINT ( 'NONE',  ( 0.1532563361054083140, 1.008931151000784787, 1.131784320476157264E-15 ) ) ;
#81327 = CARTESIAN_POINT ( 'NONE',  ( 17.20831665107776587, 59.13393115100078745, -7.208316651077762316 ) ) ;
#81328 = CARTESIAN_POINT ( 'NONE',  ( 10.00000000000000178, 35.37363466993042493, 12.81628187352647608 ) ) ;
#81330 = DIRECTION ( 'NONE',  ( 0.1650476058606878405, 0.000000000000000000, -0.9862856015372296614 ) ) ;
#81329 = CARTESIAN_POINT ( 'NONE',  ( 17.96484262340118221, 6.188685344154836621, -7.964842623401177768 ) ) ;
#81331 = CARTESIAN_POINT ( 'NONE',  ( -0.8801773607111009756, 68.06368534415484817, 1.068504757029289695E-15 ) ) ;
#81332 = CARTESIAN_POINT ( 'NONE',  ( 2.035157376598822676, 22.43868534415483396, -7.964842623401177768 ) ) ;
#81333 = CARTESIAN_POINT ( 'NONE',  ( 16.40814093676323893, 55.79030133659708923, 11.09922568453595026 ) ) ;
#81334 = CARTESIAN_POINT ( 'NONE',  ( 19.42250999205614548, 30.98035201082150536, -5.440088680355545492 ) ) ;
#81335 = CARTESIAN_POINT ( 'NONE',  ( 14.37564666802670921, 14.99999999999801759, 2.692451322021577553 ) ) ;
#81336 = CARTESIAN_POINT ( 'NONE',  ( 22.81628187352647785, 46.41530133659708213, 3.434112377981063169 ) ) ;
#81337 = CARTESIAN_POINT ( 'NONE',  ( -0.8801773607111008646, 53.27201867748816966, 2.915334737309923430 ) ) ;
#81338 = CARTESIAN_POINT ( 'NONE',  ( 0.1532563361054100626, 55.80059781766745175, -2.638427012816831230 ) ) ;
#81339 = ORIENTED_EDGE ( 'NONE', *, *, #45437, .T. ) ;
#81340 = CARTESIAN_POINT ( 'NONE',  ( -7.684764310694972345, 14.63595249122790598, 12.88194075009929840 ) ) ;
#81341 = CIRCLE ( 'NONE', #38259, 0.2500000000000002220 ) ;
#81342 = CARTESIAN_POINT ( 'NONE',  ( 19.84674366389459266, 13.30059781766745353, 2.638427012816836559 ) ) ;
#81343 = CARTESIAN_POINT ( 'NONE',  ( 22.81628187352648496, 11.83196800326375531, -3.434112377981050290 ) ) ;
#81345 = CARTESIAN_POINT ( 'NONE',  ( -7.002992508389124460, 15.00000000000000533, 12.84003923133013458 ) ) ;
#81344 = CARTESIAN_POINT ( 'NONE',  ( 10.14667048435138064, 4.748928130477084912E-16, 10.35833375027048042 ) ) ;
#81346 = CARTESIAN_POINT ( 'NONE',  ( 19.42250999205614193, 20.14701867748817321, 5.440088680355555262 ) ) ;
#81347 = CARTESIAN_POINT ( 'NONE',  ( 2.791683348922237240, 45.38393115100079456, -7.208316651077763204 ) ) ;
#81348 = CARTESIAN_POINT ( 'NONE',  ( 10.97221242068703262, -3.201784540621254098E-15, 9.670525607392866263 ) ) ;
#81349 = AXIS2_PLACEMENT_3D ( 'NONE', #11443, #17492, #41962 ) ;
#81350 = CARTESIAN_POINT ( 'NONE',  ( 2.791683348922237240, 10.38393115100078390, -7.208316651077763204 ) ) ;
#81351 = CARTESIAN_POINT ( 'NONE',  ( 17.75000000000000355, 78.80384757729335377, -4.000000000000000000 ) ) ;
#81353 = ORIENTED_EDGE ( 'NONE', *, *, #22063, .T. ) ;
#81352 = CARTESIAN_POINT ( 'NONE',  ( 0.6178305044545838731, -0.2513653300695798953, 9.382169495545420901 ) ) ;
#81354 = DIRECTION ( 'NONE',  ( -1.257568779154408793E-17, -1.000000000000000000, 0.000000000000000000 ) ) ;
#81355 = CARTESIAN_POINT ( 'NONE',  ( 6.565887622018943937, 35.16530133659708923, 12.81628187352647430 ) ) ;
#81356 = CARTESIAN_POINT ( 'NONE',  ( 14.92337183194729633, 37.67559781766745175, 8.527530157486181039 ) ) ;
#81357 = CARTESIAN_POINT ( 'NONE',  ( 64.56412365047461321, 11.99999999999999467, 10.00000000000000000 ) ) ;
#81358 = CARTESIAN_POINT ( 'NONE',  ( 10.00000000000000000, 55.55374883491396787, -14.16423886937410082 ) ) ;
#81359 = CARTESIAN_POINT ( 'NONE',  ( 14.92337183194729633, 27.67559781766745530, 8.527530157486181039 ) ) ;
#81360 = CARTESIAN_POINT ( 'NONE',  ( 8.502626202121348342, 14.95077488074853811, -12.05617882333536528 ) ) ;
#81361 = CARTESIAN_POINT ( 'NONE',  ( 6.204703633549690345, 60.76208216824730357, -14.16423886937410259 ) ) ;
#81362 = CARTESIAN_POINT ( 'NONE',  ( -8.448386164854104763, 87.04264023965325237, -4.560422061235506419 ) ) ;
#81363 = CARTESIAN_POINT ( 'NONE',  ( 19.42250999205614548, 15.98035201082150714, -5.440088680355545492 ) ) ;
#81364 = CARTESIAN_POINT ( 'NONE',  ( 2.917880565312948704, 42.63708216824729647, 12.26659068614894643 ) ) ;
#81366 = SPHERICAL_SURFACE ( 'NONE', #19070, 0.2500000000000000000 ) ;
#81365 = CARTESIAN_POINT ( 'NONE',  ( 24.16423886937410614, 49.51208216824730357, -3.795296366450302550 ) ) ;
#81367 = CARTESIAN_POINT ( 'NONE',  ( -3.420591144908647241, 15.00000000000000000, 14.60477854057953451 ) ) ;
#81368 = CARTESIAN_POINT ( 'NONE',  ( 2.791683348922237240, 10.38393115100078390, -7.208316651077763204 ) ) ;
#81369 = CARTESIAN_POINT ( 'NONE',  ( -1.099225684535947600, 3.706968003263753531, -6.408140936763238038 ) ) ;
#81370 = CARTESIAN_POINT ( 'NONE',  ( 18.61655166652078464, 14.87718327197428714, 6.499999999999960920 ) ) ;
#81371 = EDGE_LOOP ( 'NONE', ( #29769, #33599, #41031, #26022 ) ) ;
#81372 = CARTESIAN_POINT ( 'NONE',  ( 12.91533473730993009, 51.60535201082149825, -10.88017736071109987 ) ) ;
#81373 = AXIS2_PLACEMENT_3D ( 'NONE', #46836, #17348, #71808 ) ;
#81374 = EDGE_CURVE ( 'NONE', #60724, #61703, #20067, .T. ) ;
#81375 = LINE ( 'NONE', #5399, #28373 ) ;
#81376 = CARTESIAN_POINT ( 'NONE',  ( 3.969999999999999751, 10.25000000000000000, 2.500000000000000000 ) ) ;
#81377 = CARTESIAN_POINT ( 'NONE',  ( 14.75001642003106817, 14.95037105299814506, -0.3071237627329282960 ) ) ;
#81378 = CARTESIAN_POINT ( 'NONE',  ( -8.448386164854106539, 87.04264023965323815, 4.560422061235506419 ) ) ;
#81379 = CARTESIAN_POINT ( 'NONE',  ( 10.00000000000000000, 40.55374883491397497, -14.16423886937410082 ) ) ;
#81381 =( NAMED_UNIT ( * ) PLANE_ANGLE_UNIT ( ) SI_UNIT ( $, .RADIAN. ) );
#81380 = PLANE ( 'NONE',  #80201 ) ;
#81382 = CARTESIAN_POINT ( 'NONE',  ( 0.5774900079438590739, 17.64701867748817321, -5.440088680355550821 ) ) ;
#81383 = CARTESIAN_POINT ( 'NONE',  ( 10.00000000000000000, 37.87363466993041783, -12.81628187352647608 ) ) ;
#81384 = CARTESIAN_POINT ( 'NONE',  ( 20.32896413005680714, 62.60497603579418069, -5.963430220938276349 ) ) ;
#81385 = CARTESIAN_POINT ( 'NONE',  ( 6.565887622018943937, 15.16530133659708568, 12.81628187352647430 ) ) ;
#81386 = CARTESIAN_POINT ( 'NONE',  ( 22.81628187352647785, 61.62363466993041783, 6.195893100308588602E-16 ) ) ;
#81387 = ORIENTED_EDGE ( 'NONE', *, *, #89151, .T. ) ;
#81388 = LINE ( 'NONE', #18931, #73970 ) ;
#81389 = DIRECTION ( 'NONE',  ( 0.8141155183563107967, 0.000000000000000000, 0.5807029557109515405 ) ) ;
#81390 = CARTESIAN_POINT ( 'NONE',  ( 24.16423886937410614, 29.30374883491396787, 8.672049930838204340E-16 ) ) ;
#81391 = CARTESIAN_POINT ( 'NONE',  ( -4.164238869374099039, 1.803748834913967647, 8.674139862899312516E-16 ) ) ;
#81392 = CARTESIAN_POINT ( 'NONE',  ( -3.750000000000000888, 0.08806741915676698229, 4.000000000000000000 ) ) ;
#81393 = CARTESIAN_POINT ( 'NONE',  ( 20.88017736071110164, 25.35535201082150891, 2.915334737309930979 ) ) ;
#81394 = LINE ( 'NONE', #12896, #57437 ) ;
#81395 = CARTESIAN_POINT ( 'NONE',  ( -35.67076923076924544, 93.15384615384616041, -9.500000000000000000 ) ) ;
#81396 = CARTESIAN_POINT ( 'NONE',  ( 0.5774900079438607392, 53.48035201082151247, 5.440088680355550821 ) ) ;
#81397 = CARTESIAN_POINT ( 'NONE',  ( 15.44008868035555260, 44.73035201082151247, 9.422509992056143702 ) ) ;
#81398 = CARTESIAN_POINT ( 'NONE',  ( 22.81628187352648496, 16.83196800326374998, -3.434112377981050290 ) ) ;
#81399 = CARTESIAN_POINT ( 'NONE',  ( 0.1922240491738349266, 48.18878173731740588, 6.499999999999949374 ) ) ;
#81400 = DIRECTION ( 'NONE',  ( 0.000000000000000000, 1.000000000000000000, -0.000000000000000000 ) ) ;
#81401 = CARTESIAN_POINT ( 'NONE',  ( 1.472469842513823179, 26.42559781766745175, 4.923371831947296329 ) ) ;
#81402 =( NAMED_UNIT ( * ) SI_UNIT ( $, .STERADIAN. ) SOLID_ANGLE_UNIT ( ) );
#81403 = CARTESIAN_POINT ( 'NONE',  ( 17.96484262340118221, 41.18868534415484106, -7.964842623401177768 ) ) ;
#81404 = ADVANCED_FACE ( 'NONE', ( #14565 ), #30618, .F. ) ;
#81405 = CARTESIAN_POINT ( 'NONE',  ( 6.565887622018943937, 8.081968003263751754, -12.81628187352647608 ) ) ;
#81406 = CARTESIAN_POINT ( 'NONE',  ( 1.472469842513823179, 1.425597817667451528, 4.923371831947296329 ) ) ;
#81407 = CARTESIAN_POINT ( 'NONE',  ( 19.84674366389459621, 28.50893115100078745, 7.409399052514197653E-17 ) ) ;
#81408 = CARTESIAN_POINT ( 'NONE',  ( 19.38216949554541557, 47.24863466993041783, -9.382169495545420901 ) ) ;
#81409 = CARTESIAN_POINT ( 'NONE',  ( 12.63842701281683034, 7.467264484334118713, 9.846743663894596210 ) ) ;
#81410 = EDGE_LOOP ( 'NONE', ( #52271, #32259, #46476, #63826 ) ) ;
#81411 = CARTESIAN_POINT ( 'NONE',  ( -6.982525766850296911, -88.11956318484570261, -3.750000000000000000 ) ) ;
#81412 = LINE ( 'NONE', #66409, #57363 ) ;
#81413 = CARTESIAN_POINT ( 'NONE',  ( 17.96484262340118221, 21.18868534415483396, -7.964842623401177768 ) ) ;
#81415 = CARTESIAN_POINT ( 'NONE',  ( -4.164238869374098151, 36.59541550158063217, -3.795296366450310543 ) ) ;
#81414 = LINE ( 'NONE', #21417, #64818 ) ;
#81416 = CARTESIAN_POINT ( 'NONE',  ( 12.63842701281683034, 32.46726448433412315, 9.846743663894596210 ) ) ;
#81417 = VECTOR ( 'NONE', #55119, 1000.000000000000000 ) ;
#81418 = CARTESIAN_POINT ( 'NONE',  ( 17.96484262340118221, 19.93868534415484106, 7.964842623401181321 ) ) ;
#81419 = CARTESIAN_POINT ( 'NONE',  ( 2.035157376598824452, 8.688685344154839285, 7.964842623401179544 ) ) ;
#81420 = EDGE_LOOP ( 'NONE', ( #30908, #75510, #31001, #70467, #62497 ) ) ;
#81421 = CARTESIAN_POINT ( 'NONE',  ( -0.8801773607111009756, 33.06368534415484106, 1.068504757029289695E-15 ) ) ;
#81422 = CARTESIAN_POINT ( 'NONE',  ( 12.91533473730992121, 34.52201867748817676, 10.88017736071110164 ) ) ;
#81424 = CARTESIAN_POINT ( 'NONE',  ( 17.96484262340118221, 34.93868534415482685, 7.964842623401181321 ) ) ;
#81423 = DIRECTION ( 'NONE',  ( -0.9762960071199346945, 0.000000000000000000, 0.2164396139380971307 ) ) ;
#81425 = ORIENTED_EDGE ( 'NONE', *, *, #18638, .F. ) ;
#81426 = DIRECTION ( 'NONE',  ( 0.000000000000000000, 0.000000000000000000, 1.000000000000000000 ) ) ;
#81427 = CARTESIAN_POINT ( 'NONE',  ( 4.559911319644449179, 33.89701867748817676, 9.422509992056141925 ) ) ;
#81428 =( NAMED_UNIT ( * ) SI_UNIT ( $, .STERADIAN. ) SOLID_ANGLE_UNIT ( ) );
#81429 = CARTESIAN_POINT ( 'NONE',  ( -9.240973841163452107, 15.00000000000000000, -11.17382667070385160 ) ) ;
#81430 = CARTESIAN_POINT ( 'NONE',  ( 0.6178305044545838731, 59.74863466993041783, 9.382169495545420901 ) ) ;
#81431 = CARTESIAN_POINT ( 'NONE',  ( -0.1503990784575403861, 9.248846992468887862, -6.262539305110056631 ) ) ;
#81432 = CARTESIAN_POINT ( 'NONE',  ( 2.917880565312948704, 37.63708216824731068, 12.26659068614894643 ) ) ;
#81433 = CARTESIAN_POINT ( 'NONE',  ( 0.5774900079438590739, 47.64701867748817676, -5.440088680355550821 ) ) ;
#81434 = CARTESIAN_POINT ( 'NONE',  ( 20.03447792253738768, 42.65514106990691090, -6.401564815979734036 ) ) ;
#81435 = DIRECTION ( 'NONE',  ( 1.000000000000000000, 0.000000000000000000, 0.000000000000000000 ) ) ;
#81436 = CARTESIAN_POINT ( 'NONE',  ( 10.00000000000000178, 47.25893115100078745, 9.846743663894594434 ) ) ;
#81437 = B_SPLINE_CURVE_WITH_KNOTS ( 'NONE', 3,
 ( #13237, #97260, #67231, #90213, #21746, #42756 ),
 .UNSPECIFIED., .F., .F.,
 ( 4, 2, 4 ),
 ( 3.409110551487192799E-05, 0.0004400426677366973418, 0.0008459942299585226878 ),
 .UNSPECIFIED. ) ;
#81438 = ORIENTED_EDGE ( 'NONE', *, *, #81572, .F. ) ;
#81439 = LINE ( 'NONE', #43437, #49508 ) ;
#81440 = CARTESIAN_POINT ( 'NONE',  ( 19.84674366389459266, 18.30059781766745175, 2.638427012816836559 ) ) ;
#81441 = CARTESIAN_POINT ( 'NONE',  ( 11.09922568453594671, -22.95969866340291077, -6.408140936763241591 ) ) ;
#81442 = EDGE_CURVE ( 'NONE', #55640, #80446, #29784, .T. ) ;
#81443 = CARTESIAN_POINT ( 'NONE',  ( 7.084665262690076126, 17.02201867748817676, -10.88017736071110164 ) ) ;
#81444 = CARTESIAN_POINT ( 'NONE',  ( 0.1532563361054082862, 31.21726448433412315, 2.638427012816831674 ) ) ;
#81445 = CARTESIAN_POINT ( 'NONE',  ( 21.09922568453594849, 11.20696800326375531, 6.408140936763242479 ) ) ;
#81446 = CARTESIAN_POINT ( 'NONE',  ( 2.035157376598824452, 53.68868534415484817, 7.964842623401179544 ) ) ;
#81448 = CARTESIAN_POINT ( 'NONE',  ( 3.591859063236763294, 53.29030133659708923, -11.09922568453595026 ) ) ;
#81447 = CARTESIAN_POINT ( 'NONE',  ( 15.44008868035555793, 26.39701867748817321, -9.422509992056140149 ) ) ;
#81449 = CARTESIAN_POINT ( 'NONE',  ( 6.204703633549690345, 40.76208216824731778, -14.16423886937410259 ) ) ;
#81450 = EDGE_CURVE ( 'NONE', #2391, #80552, #91292, .T. ) ;
#81451 = CARTESIAN_POINT ( 'NONE',  ( -13.30119215211286132, 0.2301510699511994940, 6.804450086557105593 ) ) ;
#81452 = ORIENTED_EDGE ( 'NONE', *, *, #1567, .T. ) ;
#81453 = CARTESIAN_POINT ( 'NONE',  ( 21.09922568453595559, 2.040301336597086568, -6.408140936763230044 ) ) ;
#81454 = CARTESIAN_POINT ( 'NONE',  ( 19.42250999205614548, 10.98035201082150358, -5.440088680355545492 ) ) ;
#81455 = CARTESIAN_POINT ( 'NONE',  ( 4.559911319644449179, 47.23035201082150536, -9.422509992056141925 ) ) ;
#81456 = CARTESIAN_POINT ( 'NONE',  ( 5.076628168052704559, 65.17559781766745175, -8.527530157486179263 ) ) ;
#81457 = ORIENTED_EDGE ( 'NONE', *, *, #8903, .F. ) ;
#81458 = CARTESIAN_POINT ( 'NONE',  ( 7.361572987183170547, 12.05059781766744997, 9.846743663894590881 ) ) ;
#81459 = CARTESIAN_POINT ( 'NONE',  ( 12.63842701281683034, 42.46726448433412315, 9.846743663894596210 ) ) ;
#81460 = CARTESIAN_POINT ( 'NONE',  ( 1.472469842513823179, 6.425597817667451750, 4.923371831947296329 ) ) ;
#81461 = CARTESIAN_POINT ( 'NONE',  ( 10.00000000000000000, 19.75893115100078390, -9.846743663894594434 ) ) ;
#81462 = CARTESIAN_POINT ( 'NONE',  ( -6.829922651553562929, -69.52824172495176924, 2.500000000000000000 ) ) ;
#81464 = DIRECTION ( 'NONE',  ( 0.6246950475544238435, 0.7808688094430307203, 0.000000000000000000 ) ) ;
#81463 = CARTESIAN_POINT ( 'NONE',  ( 12.63842701281683034, 7.467264484334118713, 9.846743663894596210 ) ) ;
#81465 = CARTESIAN_POINT ( 'NONE',  ( 5.076628168052704559, 10.17559781766745175, -8.527530157486179263 ) ) ;
#81467 = EDGE_LOOP ( 'NONE', ( #53799, #57790, #19118, #72587 ) ) ;
#81466 = CARTESIAN_POINT ( 'NONE',  ( 10.00000000000000178, 22.25893115100078745, 9.846743663894594434 ) ) ;
#81468 = VECTOR ( 'NONE', #71700, 1000.000000000000000 ) ;
#81469 = CARTESIAN_POINT ( 'NONE',  ( 5.365133693937635506, -17.52547282955412200, 4.000000000000000000 ) ) ;
#81470 = CARTESIAN_POINT ( 'NONE',  ( 0.1532563361054082862, 66.21726448433413736, 2.638427012816831674 ) ) ;
#81471 = ORIENTED_EDGE ( 'NONE', *, *, #49595, .T. ) ;
#81472 = PRESENTATION_STYLE_ASSIGNMENT (( #43470 ) ) ;
#81473 = CARTESIAN_POINT ( 'NONE',  ( 24.16423886937410614, 19.30374883491397142, 8.672049930838204340E-16 ) ) ;
#81474 = UNCERTAINTY_MEASURE_WITH_UNIT (LENGTH_MEASURE( 1.000000000000000082E-05 ), #65515, 'distance_accuracy_value', 'NONE');
#81475 = CARTESIAN_POINT ( 'NONE',  ( 0.000000000000000000, 14.49999999999999822, 0.000000000000000000 ) ) ;
#81476 = CARTESIAN_POINT ( 'NONE',  ( 24.16423886937410614, 19.30374883491397142, 8.672049930838204340E-16 ) ) ;
#81477 = CARTESIAN_POINT ( 'NONE',  ( 20.36894250292379738, 49.92874883491396787, -10.36894250292379027 ) ) ;
#81478 = DIRECTION ( 'NONE',  ( 0.9890158633619187123, 0.000000000000000000, -0.1478094111295981949 ) ) ;
#81479 = CARTESIAN_POINT ( 'NONE',  ( 2.917880565312950480, 15.97041550158063217, -12.26659068614894821 ) ) ;
#81480 = CARTESIAN_POINT ( 'NONE',  ( 10.00000000000000178, 39.31368534415484106, 10.88017736071110342 ) ) ;
#81481 = DIRECTION ( 'NONE',  ( 1.000000000000000000, 0.000000000000000000, 0.000000000000000000 ) ) ;
#81482 = CARTESIAN_POINT ( 'NONE',  ( 2.791683348922240793, 26.63393115100078745, 7.208316651077764092 ) ) ;
#81485 = AXIS2_PLACEMENT_3D ( 'NONE', #17773, #87229, #50719 ) ;
#81484 = CARTESIAN_POINT ( 'NONE',  ( 0.1532563361054100626, 35.80059781766745175, -2.638427012816831230 ) ) ;
#81483 = CARTESIAN_POINT ( 'NONE',  ( 0.5774900079438607392, 53.48035201082151247, 5.440088680355550821 ) ) ;
#81486 = CARTESIAN_POINT ( 'NONE',  ( -0.8801773607111008646, 8.272018677488171434, 2.915334737309923430 ) ) ;
#81487 = CARTESIAN_POINT ( 'NONE',  ( 0.6178305044545838731, 64.74863466993043914, 9.382169495545420901 ) ) ;
#81488 = CARTESIAN_POINT ( 'NONE',  ( 19.84674366389459621, 48.50893115100078745, 7.409399052514197653E-17 ) ) ;
#81489 = EDGE_CURVE ( 'NONE', #39153, #56002, #15065, .T. ) ;
#81490 = CARTESIAN_POINT ( 'NONE',  ( 21.09922568453594849, 41.20696800326375353, 6.408140936763242479 ) ) ;
#81491 = CARTESIAN_POINT ( 'NONE',  ( 12.26659068614894821, -26.11291783175269288, 7.082119434687044190 ) ) ;
#81492 = CARTESIAN_POINT ( 'NONE',  ( 0.5774900079438607392, 48.48035201082150536, 5.440088680355550821 ) ) ;
#81493 = CARTESIAN_POINT ( 'NONE',  ( 5.076628168052704559, 40.17559781766745175, -8.527530157486179263 ) ) ;
#81494 = CARTESIAN_POINT ( 'NONE',  ( 22.26659068614894466, 23.88708216824730357, 7.082119434687054849 ) ) ;
#81495 = EDGE_LOOP ( 'NONE', ( #82359, #62822, #32010, #5950, #66308, #35805 ) ) ;
#81496 = CARTESIAN_POINT ( 'NONE',  ( -2.266590686148945544, 2.220415501580634388, 7.082119434687048631 ) ) ;
#81497 = CARTESIAN_POINT ( 'NONE',  ( 17.96484262340118221, 56.18868534415484817, -7.964842623401177768 ) ) ;
#81498 = CARTESIAN_POINT ( 'NONE',  ( -0.8801773607111008646, 63.27201867748817676, 2.915334737309923430 ) ) ;
#81499 = CARTESIAN_POINT ( 'NONE',  ( 10.00000000000000000, 50.55374883491396787, -14.16423886937410082 ) ) ;
#81500 = CARTESIAN_POINT ( 'NONE',  ( 14.92337183194729988, 64.34226448433412315, -8.527530157486177487 ) ) ;
#81501 = CARTESIAN_POINT ( 'NONE',  ( -1.099225684535947600, 64.54030133659709634, 6.408140936763237150 ) ) ;
#81502 = CARTESIAN_POINT ( 'NONE',  ( 19.42250999205614193, 55.14701867748817676, 5.440088680355555262 ) ) ;
#81503 = DIRECTION ( 'NONE',  ( 0.000000000000000000, 0.000000000000000000, 1.000000000000000000 ) ) ;
#81504 = AXIS2_PLACEMENT_3D ( 'NONE', #31578, #70582, #17097 ) ;
#81505 = CARTESIAN_POINT ( 'NONE',  ( 7.361572987183170547, 52.05059781766745175, 9.846743663894590881 ) ) ;
#81506 = B_SPLINE_CURVE_WITH_KNOTS ( 'NONE', 3,
 ( #69425, #45435, #92902, #77400, #38443, #38936 ),
 .UNSPECIFIED., .F., .F.,
 ( 4, 2, 4 ),
 ( 0.000000000000000000, 0.0002701661927229432507, 0.0005403323854458865014 ),
 .UNSPECIFIED. ) ;
#81507 = CARTESIAN_POINT ( 'NONE',  ( 7.964842623401177768, 16.18868534415483396, -7.964842623401181321 ) ) ;
#81508 = CARTESIAN_POINT ( 'NONE',  ( 17.96484262340118221, 6.188685344154837509, -7.964842623401177768 ) ) ;
#81509 = FILL_AREA_STYLE ('',( #5534 ) ) ;
#81510 = EDGE_LOOP ( 'NONE', ( #1256, #57199, #72651, #51766 ) ) ;
#81511 = CARTESIAN_POINT ( 'NONE',  ( 0.5774900079438590739, 7.647018677488171434, -5.440088680355550821 ) ) ;
#81512 = CARTESIAN_POINT ( 'NONE',  ( 12.63842701281683034, 2.467264484334118269, 9.846743663894596210 ) ) ;
#81513 = CARTESIAN_POINT ( 'NONE',  ( 7.084665262690076126, 67.02201867748817676, -10.88017736071110164 ) ) ;
#81514 = VECTOR ( 'NONE', #20617, 1000.000000000000000 ) ;
#81515 = EDGE_CURVE ( 'NONE', #93646, #18045, #54504, .T. ) ;
#81516 = CARTESIAN_POINT ( 'NONE',  ( 19.84674366389459266, 38.30059781766745175, 2.638427012816836559 ) ) ;
#81517 = CARTESIAN_POINT ( 'NONE',  ( 19.42250999205614193, 40.14701867748817676, 5.440088680355555262 ) ) ;
#81518 = CARTESIAN_POINT ( 'NONE',  ( 10.00000000000000000, 7.873634669930421381, -12.81628187352647608 ) ) ;
#81520 = CARTESIAN_POINT ( 'NONE',  ( 14.16722289976686966, 14.49999999999999112, 4.928467845925658786 ) ) ;
#81519 = CARTESIAN_POINT ( 'NONE',  ( -0.8801773607111009756, 38.06368534415484106, 1.068504757029289695E-15 ) ) ;
#81521 = DIRECTION ( 'NONE',  ( -1.000000000000000000, -1.636349903325072848E-16, 0.000000000000000000 ) ) ;
#81522 = CARTESIAN_POINT ( 'NONE',  ( 13.43411237798105340, 40.58196800326375353, 12.81628187352647963 ) ) ;
#81523 = ORIENTED_EDGE ( 'NONE', *, *, #10767, .T. ) ;
#81524 = CARTESIAN_POINT ( 'NONE',  ( 10.00000000000000000, 61.81368534415484106, -10.88017736071110342 ) ) ;
#81525 = EDGE_CURVE ( 'NONE', #86159, #43572, #59387, .T. ) ;
#81526 = CARTESIAN_POINT ( 'NONE',  ( -2.816281873526471635, 28.91530133659708213, -3.434112377981056508 ) ) ;
#81527 = CARTESIAN_POINT ( 'NONE',  ( 2.791683348922237240, 0.3839311510007847872, -7.208316651077763204 ) ) ;
#81528 = CARTESIAN_POINT ( 'NONE',  ( 2.035157376598824452, 38.68868534415483396, 7.964842623401179544 ) ) ;
#81529 = CARTESIAN_POINT ( 'NONE',  ( 5.076628168052703671, 66.84226448433412315, 8.527530157486179263 ) ) ;
#81530 = CARTESIAN_POINT ( 'NONE',  ( 13.79529636645030344, 58.26208216824728936, 14.16423886937410614 ) ) ;
#81531 = CARTESIAN_POINT ( 'NONE',  ( 19.84674366389459266, 53.30059781766744464, 2.638427012816836559 ) ) ;
#81532 = CARTESIAN_POINT ( 'NONE',  ( 10.00000000000000178, 2.258931151000784787, 9.846743663894594434 ) ) ;
#81533 = CARTESIAN_POINT ( 'NONE',  ( 7.084665262690076126, 62.02201867748816966, -10.88017736071110164 ) ) ;
#81534 = DIRECTION ( 'NONE',  ( -1.000000000000000000, 0.000000000000000000, 0.000000000000000000 ) ) ;
#81535 = CARTESIAN_POINT ( 'NONE',  ( -4.164238869374098151, 31.59541550158063927, -3.795296366450310543 ) ) ;
#81536 = AXIS2_PLACEMENT_3D ( 'NONE', #67018, #57039, #50530 ) ;
#81537 = ORIENTED_EDGE ( 'NONE', *, *, #88262, .T. ) ;
#81538 = CARTESIAN_POINT ( 'NONE',  ( 6.204703633549690345, 57.84541550158063927, 14.16423886937410082 ) ) ;
#81539 = CARTESIAN_POINT ( 'NONE',  ( 24.16423886937410614, 64.30374883491396076, 8.672049930838204340E-16 ) ) ;
#81540 = CARTESIAN_POINT ( 'NONE',  ( 0.1532563361054100626, 30.80059781766744820, -2.638427012816831230 ) ) ;
#81541 = CARTESIAN_POINT ( 'NONE',  ( -2.816281873526471635, 28.91530133659708213, -3.434112377981056508 ) ) ;
#81542 = FACE_OUTER_BOUND ( 'NONE', #86996, .T. ) ;
#81543 = DIRECTION ( 'NONE',  ( -0.5547001962252290364, -0.8320502943378437211, 0.000000000000000000 ) ) ;
#81544 = CARTESIAN_POINT ( 'NONE',  ( 4.559911319644449179, 17.23035201082150536, -9.422509992056141925 ) ) ;
#81545 = CARTESIAN_POINT ( 'NONE',  ( 6.204703633549690345, 57.84541550158063927, 14.16423886937410082 ) ) ;
#81546 = CARTESIAN_POINT ( 'NONE',  ( 14.92337183194729988, 24.34226448433411960, -8.527530157486177487 ) ) ;
#81547 = CARTESIAN_POINT ( 'NONE',  ( -14.71525861348291997, 0.5000000000000004441, 2.908807992686483601 ) ) ;
#81548 = CARTESIAN_POINT ( 'NONE',  ( 14.92337183194729988, 9.342264484334119601, -8.527530157486177487 ) ) ;
#81549 = AXIS2_PLACEMENT_3D ( 'NONE', #15877, #61844, #92350 ) ;
#81550 = AXIS2_PLACEMENT_3D ( 'NONE', #84001, #41, #98544 ) ;
#81551 = CARTESIAN_POINT ( 'NONE',  ( 18.50749283717775029, 59.69955587570481725, 6.500000000000035527 ) ) ;
#81552 = CARTESIAN_POINT ( 'NONE',  ( -7.208316651077756099, 21.63393115100078390, 7.208316651077766757 ) ) ;
#81553 = ORIENTED_EDGE ( 'NONE', *, *, #66371, .F. ) ;
#81554 = ORIENTED_EDGE ( 'NONE', *, *, #44340, .F. ) ;
#81555 = DIRECTION ( 'NONE',  ( 1.000000000000000000, 0.000000000000000000, 0.000000000000000000 ) ) ;
#81556 = CIRCLE ( 'NONE', #52800, 15.00000000000000000 ) ;
#81557 = VERTEX_POINT ( 'NONE', #30523 ) ;
#81558 = CARTESIAN_POINT ( 'NONE',  ( 2.791683348922237240, 40.38393115100078035, -7.208316651077763204 ) ) ;
#81560 = CARTESIAN_POINT ( 'NONE',  ( 2.035157376598824452, 18.68868534415484106, 7.964842623401179544 ) ) ;
#81559 = CARTESIAN_POINT ( 'NONE',  ( -0.8801773607111008646, 23.27201867748817676, 2.915334737309923430 ) ) ;
#81562 = CARTESIAN_POINT ( 'NONE',  ( 10.00000000000000178, 15.37363466993042138, 12.81628187352647608 ) ) ;
#81561 = CARTESIAN_POINT ( 'NONE',  ( 0.1532563361054100626, 55.80059781766745175, -2.638427012816831230 ) ) ;
#81563 = CARTESIAN_POINT ( 'NONE',  ( -4.164238869374099039, 6.803748834913967869, 8.674139862899312516E-16 ) ) ;
#81564 = CARTESIAN_POINT ( 'NONE',  ( 19.84674366389459266, 43.30059781766744464, 2.638427012816836559 ) ) ;
#81565 = EDGE_CURVE ( 'NONE', #28808, #26148, #71342, .T. ) ;
#81566 = CARTESIAN_POINT ( 'NONE',  ( 16.40814093676323893, 35.79030133659708923, 11.09922568453595026 ) ) ;
#81567 = ORIENTED_EDGE ( 'NONE', *, *, #84063, .F. ) ;
#81568 = CARTESIAN_POINT ( 'NONE',  ( 18.52753015748618282, 28.92559781766745175, -4.923371831947291888 ) ) ;
#81569 = CARTESIAN_POINT ( 'NONE',  ( 22.26659068614895176, 59.72041550158063927, -7.082119434687042414 ) ) ;
#81570 = ORIENTED_EDGE ( 'NONE', *, *, #68966, .F. ) ;
#81571 = CARTESIAN_POINT ( 'NONE',  ( -0.8801773607111009756, 3.063685344154838397, 1.068504757029289695E-15 ) ) ;
#81572 = EDGE_CURVE ( 'NONE', #26555, #93626, #96161, .T. ) ;
#81573 = ORIENTED_EDGE ( 'NONE', *, *, #45060, .F. ) ;
#81574 = CARTESIAN_POINT ( 'NONE',  ( 17.96484262340118221, 49.93868534415484106, 7.964842623401181321 ) ) ;
#81575 = CARTESIAN_POINT ( 'NONE',  ( 15.44008868035555260, 44.73035201082151247, 9.422509992056143702 ) ) ;
#81576 = CARTESIAN_POINT ( 'NONE',  ( 10.00000000000000000, 51.81368534415484106, -10.88017736071110342 ) ) ;
#81577 = CARTESIAN_POINT ( 'NONE',  ( 0.000000000000000000, -97.00000000000000000, 2.500000000000000000 ) ) ;
#81578 = CARTESIAN_POINT ( 'NONE',  ( 7.084665262690076126, 39.10535201082150536, 10.88017736071109987 ) ) ;
#81579 = CARTESIAN_POINT ( 'NONE',  ( 1.602071938427535702, 47.02224192338641018, -6.500000000000077272 ) ) ;
#81581 = ORIENTED_EDGE ( 'NONE', *, *, #28706, .F. ) ;
#81580 = LINE ( 'NONE', #95611, #80895 ) ;
#81582 = CARTESIAN_POINT ( 'NONE',  ( 18.52753015748618282, 28.92559781766745175, -4.923371831947291888 ) ) ;
#81583 = ORIENTED_EDGE ( 'NONE', *, *, #40324, .T. ) ;
#81584 = CARTESIAN_POINT ( 'NONE',  ( 2.791683348922240793, 51.63393115100078745, 7.208316651077764092 ) ) ;
#81585 = CARTESIAN_POINT ( 'NONE',  ( -8.000000000000000000, 0.000000000000000000, 3.750000000000000000 ) ) ;
#81586 = ADVANCED_FACE ( 'NONE', ( #60535 ), #40022, .T. ) ;
#81587 = CARTESIAN_POINT ( 'NONE',  ( 2.917880565312950480, 10.97041550158063572, -12.26659068614894821 ) ) ;
#81588 = CARTESIAN_POINT ( 'NONE',  ( -10.76421366023792103, 12.61593446625853865, -3.660229437423404342 ) ) ;
#81589 = DIRECTION ( 'NONE',  ( -1.000000000000000000, 0.000000000000000000, 0.000000000000000000 ) ) ;
#81590 = CARTESIAN_POINT ( 'NONE',  ( -10.77730536144846596, -98.63085534186639336, 3.750000000000000000 ) ) ;
#81591 = CARTESIAN_POINT ( 'NONE',  ( 13.79529636645030344, 63.26208216824730357, 14.16423886937410614 ) ) ;
#81592 = CARTESIAN_POINT ( 'NONE',  ( 4.096035146093531587, 15.00000000000000000, -13.90943910019259278 ) ) ;
#81593 = VERTEX_POINT ( 'NONE', #28456 ) ;
#81594 = LINE ( 'NONE', #20113, #25654 ) ;
#81595 = CARTESIAN_POINT ( 'NONE',  ( 18.52753015748617571, 48.09226448433412315, 4.923371831947298993 ) ) ;
#81596 = CARTESIAN_POINT ( 'NONE',  ( -14.04867373755345561, -0.03417435944610275333, -7.649324326489842285 ) ) ;
#81597 = CARTESIAN_POINT ( 'NONE',  ( 0.6178305044545838731, 14.74863466993041783, 9.382169495545420901 ) ) ;
#81598 = CARTESIAN_POINT ( 'NONE',  ( 17.20831665107776587, 4.133931151000785675, -7.208316651077762316 ) ) ;
#81599 = DIRECTION ( 'NONE',  ( 5.151434834260726979E-14, 0.000000000000000000, 1.000000000000000000 ) ) ;
#81600 = ADVANCED_FACE ( 'NONE', ( #73949 ), #29424, .F. ) ;
#81601 = CARTESIAN_POINT ( 'NONE',  ( 12.63842701281683034, 12.46726448433411782, 9.846743663894596210 ) ) ;
#81602 = CARTESIAN_POINT ( 'NONE',  ( 2.791683348922240793, 66.63393115100079456, 7.208316651077764092 ) ) ;
#81603 = CARTESIAN_POINT ( 'NONE',  ( 34.56412365047464874, 11.99999999999999645, 10.00000000000000000 ) ) ;
#81604 = CONICAL_SURFACE ( 'NONE', #49700, 11.25000000000000178, 0.7853981633974497223 ) ;
#81605 = EDGE_CURVE ( 'NONE', #58305, #86598, #65875, .T. ) ;
#81606 = EDGE_CURVE ( 'NONE', #68278, #83096, #11635, .T. ) ;
#81607 = VERTEX_POINT ( 'NONE', #19963 ) ;
#81608 = CARTESIAN_POINT ( 'NONE',  ( 7.084665262690076126, 7.022018677488170546, -10.88017736071110164 ) ) ;
#81609 = CARTESIAN_POINT ( 'NONE',  ( -0.3689425029237881626, 2.428748834913967869, 10.36894250292379027 ) ) ;
#81610 = CARTESIAN_POINT ( 'NONE',  ( 0.1532563361054083140, 26.00893115100078745, 1.131784320476157264E-15 ) ) ;
#81611 = CARTESIAN_POINT ( 'NONE',  ( -0.8801773607110991993, 57.85535201082149825, -2.915334737309923874 ) ) ;
#81612 = AXIS2_PLACEMENT_3D ( 'NONE', #69005, #68512, #30984 ) ;
#81614 = DIRECTION ( 'NONE',  ( -0.000000000000000000, 0.000000000000000000, 1.000000000000000000 ) ) ;
#81613 = CARTESIAN_POINT ( 'NONE',  ( 13.43411237798106583, 32.66530133659708213, -12.81628187352647252 ) ) ;
#81615 = CARTESIAN_POINT ( 'NONE',  ( 10.00000000000000000, 6.813685344154838397, -10.88017736071110342 ) ) ;
#81616 = DIRECTION ( 'NONE',  ( -1.000000000000000000, 0.000000000000000000, 0.000000000000000000 ) ) ;
#81617 = CARTESIAN_POINT ( 'NONE',  ( 17.20831665107776587, 59.13393115100078745, -7.208316651077762316 ) ) ;
#81618 = CARTESIAN_POINT ( 'NONE',  ( 14.92337183194729988, 19.34226448433411960, -8.527530157486177487 ) ) ;
#81619 = CARTESIAN_POINT ( 'NONE',  ( 10.88017736071110164, -24.64464798917849109, 2.915334737309921209 ) ) ;
#81620 = CARTESIAN_POINT ( 'NONE',  ( 22.81628187352648496, 26.83196800326374998, -3.434112377981050290 ) ) ;
#81621 = CARTESIAN_POINT ( 'NONE',  ( -10.77974636317328994, -96.52223143591398014, -4.000000000000000000 ) ) ;
#81622 = AXIS2_PLACEMENT_3D ( 'NONE', #87078, #64551, #80566 ) ;
#81624 = CARTESIAN_POINT ( 'NONE',  ( 10.97324858046193619, 15.00000000000000711, 9.670892530813269161 ) ) ;
#81623 = CARTESIAN_POINT ( 'NONE',  ( 19.42250999205614548, 40.98035201082150536, -5.440088680355545492 ) ) ;
#81625 = CARTESIAN_POINT ( 'NONE',  ( -7.199999999999997513, 99.99999999999998579, -8.000000000000000000 ) ) ;
#81626 = PRESENTATION_STYLE_ASSIGNMENT (( #88636 ) ) ;
#81627 = CARTESIAN_POINT ( 'NONE',  ( 12.91533473730992121, 24.52201867748816966, 10.88017736071110164 ) ) ;
#81628 = CARTESIAN_POINT ( 'NONE',  ( 19.84674366389459266, 48.30059781766745175, 2.638427012816836559 ) ) ;
#81629 = EDGE_CURVE ( 'NONE', #7169, #96379, #48645, .T. ) ;
#81630 = CARTESIAN_POINT ( 'NONE',  ( 20.88017736071110164, 55.35535201082149825, 2.915334737309930979 ) ) ;
#81631 = CARTESIAN_POINT ( 'NONE',  ( -4.164238869374099927, 37.01208216824731068, 3.795296366450308767 ) ) ;
#81632 = CARTESIAN_POINT ( 'NONE',  ( 3.927832320392154575, -0.03417435944610275333, 13.69797916712106733 ) ) ;
#81633 = CARTESIAN_POINT ( 'NONE',  ( 7.361572987183170547, 37.05059781766744464, 9.846743663894590881 ) ) ;
#81634 = CARTESIAN_POINT ( 'NONE',  ( 16.40814093676324603, 62.45696800326376064, -11.09922568453594671 ) ) ;
#81635 = CARTESIAN_POINT ( 'NONE',  ( 19.84674366389459266, 63.30059781766745886, 2.638427012816836559 ) ) ;
#81636 = ORIENTED_EDGE ( 'NONE', *, *, #55444, .T. ) ;
#81637 = CARTESIAN_POINT ( 'NONE',  ( 2.035157376598824452, 28.68868534415484106, 7.964842623401179544 ) ) ;
#81638 = EDGE_CURVE ( 'NONE', #93468, #27652, #57957, .T. ) ;
#81639 = CARTESIAN_POINT ( 'NONE',  ( -0.8801773607111009756, 18.06368534415484106, 1.068504757029289695E-15 ) ) ;
#81640 = CARTESIAN_POINT ( 'NONE',  ( 10.00000000000000178, 69.31368534415484817, 10.88017736071110342 ) ) ;
#81641 = CARTESIAN_POINT ( 'NONE',  ( 22.26659068614895176, 29.72041550158063572, -7.082119434687042414 ) ) ;
#81642 = CARTESIAN_POINT ( 'NONE',  ( 10.00000000000000178, 12.25893115100078568, 9.846743663894594434 ) ) ;
#81643 = CARTESIAN_POINT ( 'NONE',  ( 10.00000000000000178, 67.25893115100079456, 9.846743663894594434 ) ) ;
#81644 = CARTESIAN_POINT ( 'NONE',  ( 12.91533473730992121, 34.52201867748817676, 10.88017736071110164 ) ) ;
#81645 = DIRECTION ( 'NONE',  ( 0.000000000000000000, 0.000000000000000000, -1.000000000000000000 ) ) ;
#81646 = CYLINDRICAL_SURFACE ( 'NONE', #87275, 0.5000000000000000000 ) ;
#81647 = EDGE_LOOP ( 'NONE', ( #64337, #91728, #31044, #8237, #80596, #17035 ) ) ;
#81648 = CARTESIAN_POINT ( 'NONE',  ( 70.00000000000000000, -4.073016716636387686E-15, 10.00000000000000000 ) ) ;
#81649 = CARTESIAN_POINT ( 'NONE',  ( 5.076628168052704559, 45.17559781766745175, -8.527530157486179263 ) ) ;
#81650 = ORIENTED_EDGE ( 'NONE', *, *, #92072, .F. ) ;
#81651 = VERTEX_POINT ( 'NONE', #81941 ) ;
#81652 =( GEOMETRIC_REPRESENTATION_CONTEXT ( 3 ) GLOBAL_UNCERTAINTY_ASSIGNED_CONTEXT ( ( #35483 ) ) GLOBAL_UNIT_ASSIGNED_CONTEXT ( ( #40834, #87302, #24368 ) ) REPRESENTATION_CONTEXT ( 'NONE', 'WORKASPACE' ) );
#81653 = SURFACE_STYLE_FILL_AREA ( #43660 ) ;
#81654 = CARTESIAN_POINT ( 'NONE',  ( 6.204703633549690345, 27.84541550158063217, 14.16423886937410082 ) ) ;
#81655 = CARTESIAN_POINT ( 'NONE',  ( 24.16423886937410614, 9.512082168247301794, -3.795296366450302550 ) ) ;
#81656 = CARTESIAN_POINT ( 'NONE',  ( 4.559911319644449179, 58.89701867748817676, 9.422509992056141925 ) ) ;
#81657 = CARTESIAN_POINT ( 'NONE',  ( 6.204703633549690345, 52.84541550158062506, 14.16423886937410082 ) ) ;
#81658 = CARTESIAN_POINT ( 'NONE',  ( 10.00000000000000178, 67.25893115100079456, 9.846743663894594434 ) ) ;
#81659 = CARTESIAN_POINT ( 'NONE',  ( 19.84674366389459266, 53.71726448433411605, -2.638427012816827677 ) ) ;
#81661 = CARTESIAN_POINT ( 'NONE',  ( -1.099225684535947600, 4.540301336597087456, 6.408140936763237150 ) ) ;
#81660 = CARTESIAN_POINT ( 'NONE',  ( 10.00000000000000000, 46.81368534415484106, -10.88017736071110342 ) ) ;
#81662 = CARTESIAN_POINT ( 'NONE',  ( -4.164238869374099039, 21.80374883491396787, 8.674139862899312516E-16 ) ) ;
#81663 = CARTESIAN_POINT ( 'NONE',  ( 10.00000000000000000, 16.81368534415483751, -10.88017736071110342 ) ) ;
#81664 = CARTESIAN_POINT ( 'NONE',  ( 19.80832241502128355, 14.75868815902069997, 6.499999999999992895 ) ) ;
#81665 = DIRECTION ( 'NONE',  ( -0.000000000000000000, 0.000000000000000000, 1.000000000000000000 ) ) ;
#81666 = CARTESIAN_POINT ( 'NONE',  ( 4.559911319644449179, 47.23035201082150536, -9.422509992056141925 ) ) ;
#81667 = CARTESIAN_POINT ( 'NONE',  ( -4.923371831947292776, -33.15773551566587685, 8.527530157486181039 ) ) ;
#81668 = ORIENTED_EDGE ( 'NONE', *, *, #10500, .T. ) ;
#81669 = CARTESIAN_POINT ( 'NONE',  ( 0.3093388210927754400, 14.63745559856262624, -14.99680997725068821 ) ) ;
#81670 = VERTEX_POINT ( 'NONE', #66948 ) ;
#81671 = ORIENTED_EDGE ( 'NONE', *, *, #88643, .T. ) ;
#81672 = CARTESIAN_POINT ( 'NONE',  ( -4.164238869374099927, 47.01208216824729647, 3.795296366450308767 ) ) ;
#81673 = CARTESIAN_POINT ( 'NONE',  ( 1.472469842513823179, 41.42559781766745886, 4.923371831947296329 ) ) ;
#81674 = CARTESIAN_POINT ( 'NONE',  ( 19.42250999205614193, 60.14701867748817676, 5.440088680355555262 ) ) ;
#81675 = CARTESIAN_POINT ( 'NONE',  ( 13.55255535720591986, 15.00000000000000000, 4.403492169843056914 ) ) ;
#81676 = EDGE_CURVE ( 'NONE', #39981, #45554, #68067, .T. ) ;
#81677 = CARTESIAN_POINT ( 'NONE',  ( 2.035157376598822676, 57.43868534415484106, -7.964842623401177768 ) ) ;
#81678 = CARTESIAN_POINT ( 'NONE',  ( 13.43411237798106583, 57.66530133659708923, -12.81628187352647252 ) ) ;
#81679 = CARTESIAN_POINT ( 'NONE',  ( 3.434112377981060948, 5.581968003263752642, 12.81628187352647430 ) ) ;
#81680 = ORIENTED_EDGE ( 'NONE', *, *, #70473, .F. ) ;
#81681 = CARTESIAN_POINT ( 'NONE',  ( 0.5774900079438590739, 47.64701867748817676, -5.440088680355550821 ) ) ;
#81682 =( GEOMETRIC_REPRESENTATION_CONTEXT ( 3 ) GLOBAL_UNCERTAINTY_ASSIGNED_CONTEXT ( ( #22400 ) ) GLOBAL_UNIT_ASSIGNED_CONTEXT ( ( #69495, #86948, #2505 ) ) REPRESENTATION_CONTEXT ( 'NONE', 'WORKASPACE' ) );
#81683 = CARTESIAN_POINT ( 'NONE',  ( 2.917880565312950480, 25.97041550158063572, -12.26659068614894821 ) ) ;
#81684 = ORIENTED_EDGE ( 'NONE', *, *, #13324, .F. ) ;
#81685 = CARTESIAN_POINT ( 'NONE',  ( 10.00000000000000000, 22.87363466993042138, -12.81628187352647608 ) ) ;
#81686 = ORIENTED_EDGE ( 'NONE', *, *, #76753, .F. ) ;
#81687 = CARTESIAN_POINT ( 'NONE',  ( 3.591859063236763294, 43.29030133659708923, -11.09922568453595026 ) ) ;
#81688 = CARTESIAN_POINT ( 'NONE',  ( -0.8801773607110991993, 17.85535201082150536, -2.915334737309923874 ) ) ;
#81689 = CARTESIAN_POINT ( 'NONE',  ( 17.20831665107776587, 37.88393115100078745, 7.208316651077764980 ) ) ;
#81690 = CARTESIAN_POINT ( 'NONE',  ( 10.00000000000000178, 9.313685344154839285, 10.88017736071110342 ) ) ;
#81691 = AXIS2_PLACEMENT_3D ( 'NONE', #3649, #79139, #3157 ) ;
#81692 = CARTESIAN_POINT ( 'NONE',  ( -2.816281873526471635, 58.91530133659707502, -3.434112377981056508 ) ) ;
#81693 = DIRECTION ( 'NONE',  ( 0.6246950475544237324, 0.7808688094430306093, 0.000000000000000000 ) ) ;
#81694 = CARTESIAN_POINT ( 'NONE',  ( 5.076628168052703671, 41.84226448433411605, 8.527530157486179263 ) ) ;
#81695 = B_SPLINE_CURVE_WITH_KNOTS ( 'NONE', 3,
 ( #44730, #15249, #67242, #29230, #14249, #53223 ),
 .UNSPECIFIED., .F., .F.,
 ( 4, 2, 4 ),
 ( 3.409110551493951444E-05, 0.0004400426677367878184, 0.0008459942299586360953 ),
 .UNSPECIFIED. ) ;
#81697 = ORIENTED_EDGE ( 'NONE', *, *, #18083, .F. ) ;
#81696 = CARTESIAN_POINT ( 'NONE',  ( 2.035157376598822676, 67.43868534415484817, -7.964842623401177768 ) ) ;
#81698 = CARTESIAN_POINT ( 'NONE',  ( -13.69000000000001549, 92.00000000000000000, -10.09898361729590199 ) ) ;
#81699 = PLANE ( 'NONE',  #57834 ) ;
#81700 = CARTESIAN_POINT ( 'NONE',  ( 4.555630843329481650, 77.03495325336413657, 9.500000000000000000 ) ) ;
#81701 = DIRECTION ( 'NONE',  ( 0.000000000000000000, 0.000000000000000000, 1.000000000000000000 ) ) ;
#81702 = CARTESIAN_POINT ( 'NONE',  ( 2.791683348922240793, 11.63393115100078568, 7.208316651077764092 ) ) ;
#81703 = CARTESIAN_POINT ( 'NONE',  ( 19.38216949554541557, 27.24863466993041783, -9.382169495545420901 ) ) ;
#81704 = ORIENTED_EDGE ( 'NONE', *, *, #95410, .F. ) ;
#81705 = CARTESIAN_POINT ( 'NONE',  ( 17.20831665107776587, 52.88393115100078035, 7.208316651077764980 ) ) ;
#81706 = CARTESIAN_POINT ( 'NONE',  ( -13.34343830728394842, 0.3640475087720989600, -6.852200678592788918 ) ) ;
#81707 = CARTESIAN_POINT ( 'NONE',  ( 2.917880565312950480, 20.97041550158063217, -12.26659068614894821 ) ) ;
#81708 = CARTESIAN_POINT ( 'NONE',  ( 17.20831665107776587, 42.88393115100077324, 7.208316651077764980 ) ) ;
#81709 = CARTESIAN_POINT ( 'NONE',  ( 16.40814093676324603, 47.45696800326375353, -11.09922568453594671 ) ) ;
#81711 = FILL_AREA_STYLE ('',( #73719 ) ) ;
#81710 = CARTESIAN_POINT ( 'NONE',  ( 64.56412365047461321, 44.99999999999998579, 0.000000000000000000 ) ) ;
#81712 = CARTESIAN_POINT ( 'NONE',  ( 19.42250999205614548, 60.98035201082151247, -5.440088680355545492 ) ) ;
#81713 = ADVANCED_FACE ( 'NONE', ( #35950 ), #59436, .T. ) ;
#81714 = CARTESIAN_POINT ( 'NONE',  ( 20.24186590665277308, 47.61633188102327097, -6.114288769123048972 ) ) ;
#81715 = CARTESIAN_POINT ( 'NONE',  ( 5.076628168052704559, 35.17559781766745175, -8.527530157486179263 ) ) ;
#81716 = CARTESIAN_POINT ( 'NONE',  ( -0.8801773607111009756, 43.06368534415484106, 1.068504757029289695E-15 ) ) ;
#81717 = CARTESIAN_POINT ( 'NONE',  ( 19.38216949554541557, 37.24863466993041783, -9.382169495545420901 ) ) ;
#81718 = CARTESIAN_POINT ( 'NONE',  ( -13.86076281203281546, 90.90669854496245250, 7.842019570309374465 ) ) ;
#81719 = ADVANCED_FACE ( 'NONE', ( #28931 ), #43936, .T. ) ;
#81720 = CARTESIAN_POINT ( 'NONE',  ( 19.42250999205614548, 40.98035201082150536, -5.440088680355545492 ) ) ;
#81721 = EDGE_CURVE ( 'NONE', #62689, #6556, #97831, .T. ) ;
#81722 = ORIENTED_EDGE ( 'NONE', *, *, #88300, .T. ) ;
#81723 = CARTESIAN_POINT ( 'NONE',  ( -4.289191146912808207E-15, 3.868033628982651795, -11.25000000000000178 ) ) ;
#81724 = CARTESIAN_POINT ( 'NONE',  ( 2.035157376598822676, 12.43868534415483751, -7.964842623401177768 ) ) ;
#81726 = CARTESIAN_POINT ( 'NONE',  ( 20.88017736071110519, 40.56368534415484106, 2.639326808657452039E-16 ) ) ;
#81725 = CARTESIAN_POINT ( 'NONE',  ( 18.52753015748617571, 63.09226448433412315, 4.923371831947298993 ) ) ;
#81727 = CARTESIAN_POINT ( 'NONE',  ( 0.000000000000000000, 0.5000000000000004441, 0.000000000000000000 ) ) ;
#81728 = CARTESIAN_POINT ( 'NONE',  ( 4.559911319644449179, 62.23035201082150536, -9.422509992056141925 ) ) ;
#81730 = CARTESIAN_POINT ( 'NONE',  ( -0.000000000000000000, 71.20572488941321865, -5.000000000000000888 ) ) ;
#81729 = CARTESIAN_POINT ( 'NONE',  ( -0.8801773607111008646, 28.27201867748817321, 2.915334737309923430 ) ) ;
#81731 = CARTESIAN_POINT ( 'NONE',  ( 10.00000000000000000, -0.2410688489992152128, -9.846743663894594434 ) ) ;
#81732 = CARTESIAN_POINT ( 'NONE',  ( 1.472469842513823179, 25.59226448433412315, -4.923371831947296329 ) ) ;
#81733 = DIRECTION ( 'NONE',  ( 0.000000000000000000, 0.000000000000000000, 1.000000000000000000 ) ) ;
#81734 = CARTESIAN_POINT ( 'NONE',  ( -12.26659068614894110, 7.220415501580639273, 7.082119434687058401 ) ) ;
#81735 = CARTESIAN_POINT ( 'NONE',  ( 5.076628168052703671, 46.84226448433412315, 8.527530157486179263 ) ) ;
#81737 = CARTESIAN_POINT ( 'NONE',  ( 20.15039907845753220, 19.72266099184918886, 6.262539305110075283 ) ) ;
#81736 = CARTESIAN_POINT ( 'NONE',  ( 17.08211943468705130, 53.47041550158063217, 12.26659068614894998 ) ) ;
#81738 = CARTESIAN_POINT ( 'NONE',  ( 0.000000000000000000, 14.49999999999999822, 0.000000000000000000 ) ) ;
#81739 = CARTESIAN_POINT ( 'NONE',  ( 13.79529636645030344, 13.26208216824729824, 14.16423886937410614 ) ) ;
#81740 = CARTESIAN_POINT ( 'NONE',  ( -4.164238869374098151, 31.59541550158063927, -3.795296366450310543 ) ) ;
#81741 = CARTESIAN_POINT ( 'NONE',  ( 6.565887622018943937, 8.081968003263751754, -12.81628187352647608 ) ) ;
#81742 = ORIENTED_EDGE ( 'NONE', *, *, #59560, .T. ) ;
#81743 = CARTESIAN_POINT ( 'NONE',  ( 20.88017736071110519, 10.56368534415483929, 2.639326808657452039E-16 ) ) ;
#81744 = CARTESIAN_POINT ( 'NONE',  ( 12.63842701281683034, 42.46726448433412315, 9.846743663894596210 ) ) ;
#81746 = CARTESIAN_POINT ( 'NONE',  ( 0.000000000000000000, 0.000000000000000000, 0.000000000000000000 ) ) ;
#81745 = PLANE ( 'NONE',  #27592 ) ;
#81747 =( LENGTH_UNIT ( ) NAMED_UNIT ( * ) SI_UNIT ( .MILLI., .METRE. ) );
#81748 = TOROIDAL_SURFACE ( 'NONE', #64194, 2.750000000000001776, 0.2500000000000000000 ) ;
#81749 = CARTESIAN_POINT ( 'NONE',  ( 12.63842701281683034, 2.467264484334118269, 9.846743663894596210 ) ) ;
#81750 = CARTESIAN_POINT ( 'NONE',  ( -1.099225684535947600, 28.70696800326375353, -6.408140936763238038 ) ) ;
#81751 = CARTESIAN_POINT ( 'NONE',  ( 7.361572987183170547, 32.05059781766745175, 9.846743663894590881 ) ) ;
#81752 = ORIENTED_EDGE ( 'NONE', *, *, #66046, .F. ) ;
#81753 = CARTESIAN_POINT ( 'NONE',  ( 5.076628168052703671, 6.842264484334118713, 8.527530157486179263 ) ) ;
#81754 = EDGE_CURVE ( 'NONE', #45067, #92561, #70681, .T. ) ;
#81755 =( GEOMETRIC_REPRESENTATION_CONTEXT ( 3 ) GLOBAL_UNCERTAINTY_ASSIGNED_CONTEXT ( ( #65481 ) ) GLOBAL_UNIT_ASSIGNED_CONTEXT ( ( #35171, #21676, #35679 ) ) REPRESENTATION_CONTEXT ( 'NONE', 'WORKASPACE' ) );
#81756 = CARTESIAN_POINT ( 'NONE',  ( 18.50749283717776805, 4.699555875704811925, 6.500000000000004441 ) ) ;
#81757 = FACE_OUTER_BOUND ( 'NONE', #20531, .T. ) ;
#81758 = CARTESIAN_POINT ( 'NONE',  ( 19.42250999205614548, 15.98035201082150714, -5.440088680355545492 ) ) ;
#81759 = CARTESIAN_POINT ( 'NONE',  ( -4.164238869374099927, 42.01208216824728936, 3.795296366450308767 ) ) ;
#81760 = CARTESIAN_POINT ( 'NONE',  ( 2.035157376598824452, 68.68868534415484817, 7.964842623401179544 ) ) ;
#81761 = CARTESIAN_POINT ( 'NONE',  ( -0.1503990784575242878, 49.24884699246889141, -6.262539305110083276 ) ) ;
#81762 = CARTESIAN_POINT ( 'NONE',  ( 19.84674366389459621, 28.50893115100078745, 7.409399052514197653E-17 ) ) ;
#81763 = CARTESIAN_POINT ( 'NONE',  ( 20.15039907845753220, 21.74884699246888786, 6.262539305110078836 ) ) ;
#81764 = CARTESIAN_POINT ( 'NONE',  ( 0.1532563361054100626, 5.800597817667452638, -2.638427012816831230 ) ) ;
#81765 =( GEOMETRIC_REPRESENTATION_CONTEXT ( 3 ) GLOBAL_UNCERTAINTY_ASSIGNED_CONTEXT ( ( #93093 ) ) GLOBAL_UNIT_ASSIGNED_CONTEXT ( ( #26035, #4029, #48025 ) ) REPRESENTATION_CONTEXT ( 'NONE', 'WORKASPACE' ) );
#81766 = CARTESIAN_POINT ( 'NONE',  ( 1.152268111383477178, 1.024801820426059406E-17, -6.000000000000281553 ) ) ;
#81767 = CARTESIAN_POINT ( 'NONE',  ( 1.472469842513823179, 35.59226448433412315, -4.923371831947296329 ) ) ;
#81768 = CARTESIAN_POINT ( 'NONE',  ( 18.52753015748617571, 63.09226448433412315, 4.923371831947298993 ) ) ;
#81769 = CARTESIAN_POINT ( 'NONE',  ( 17.96484262340118221, 39.93868534415484106, 7.964842623401181321 ) ) ;
#81770 = EDGE_CURVE ( 'NONE', #42002, #20489, #66544, .T. ) ;
#81771 = ORIENTED_EDGE ( 'NONE', *, *, #90440, .T. ) ;
#81772 = CARTESIAN_POINT ( 'NONE',  ( 3.591859063236763294, 58.29030133659708923, -11.09922568453595026 ) ) ;
#81773 = CARTESIAN_POINT ( 'NONE',  ( 2.791683348922240793, 1.633931151000784565, 7.208316651077764092 ) ) ;
#81774 = CARTESIAN_POINT ( 'NONE',  ( 6.565887622018943937, 40.16530133659708923, 12.81628187352647430 ) ) ;
#81776 = CARTESIAN_POINT ( 'NONE',  ( 19.84674366389459266, 33.30059781766744464, 2.638427012816836559 ) ) ;
#81775 = CARTESIAN_POINT ( 'NONE',  ( 22.26659068614895176, 59.72041550158063927, -7.082119434687042414 ) ) ;
#81777 = DIRECTION ( 'NONE',  ( 0.000000000000000000, 0.000000000000000000, 1.000000000000000000 ) ) ;
#81778 = CARTESIAN_POINT ( 'NONE',  ( 5.076628168052703671, 1.842264484334118047, 8.527530157486179263 ) ) ;
#81779 = CARTESIAN_POINT ( 'NONE',  ( 20.36894250292379382, 18.67874883491397142, 10.36894250292379205 ) ) ;
#81780 = CARTESIAN_POINT ( 'NONE',  ( 13.79529636645031943, 40.34541550158063217, -14.16423886937409904 ) ) ;
#81781 = CARTESIAN_POINT ( 'NONE',  ( 2.791683348922240793, 41.63393115100078745, 7.208316651077764092 ) ) ;
#81782 = CARTESIAN_POINT ( 'NONE',  ( 4.191187596054804843, -2.692365941978121846, -2.500000000000000444 ) ) ;
#81783 = CARTESIAN_POINT ( 'NONE',  ( 12.91533473730993009, 41.60535201082149825, -10.88017736071109987 ) ) ;
#81784 = CARTESIAN_POINT ( 'NONE',  ( 20.88017736071110164, 55.35535201082149825, 2.915334737309930979 ) ) ;
#81785 = ORIENTED_EDGE ( 'NONE', *, *, #41137, .T. ) ;
#81786 = CARTESIAN_POINT ( 'NONE',  ( 21.09922568453595559, 42.04030133659708213, -6.408140936763230044 ) ) ;
#81787 = CARTESIAN_POINT ( 'NONE',  ( 19.42250999205614193, 65.14701867748817676, 5.440088680355555262 ) ) ;
#81788 = VERTEX_POINT ( 'NONE', #51952 ) ;
#81789 = CARTESIAN_POINT ( 'NONE',  ( 20.36894250292379382, 8.678748834913967869, 10.36894250292379205 ) ) ;
#81790 = CARTESIAN_POINT ( 'NONE',  ( 19.84674366389459266, 8.300597817667451750, 2.638427012816836559 ) ) ;
#81791 = CARTESIAN_POINT ( 'NONE',  ( -0.1503990784575328643, 60.12777174578613426, 6.262539305110068177 ) ) ;
#81792 = EDGE_LOOP ( 'NONE', ( #89079, #31, #77406 ) ) ;
#81793 = CARTESIAN_POINT ( 'NONE',  ( 4.559911319644449179, 17.23035201082150536, -9.422509992056141925 ) ) ;
#81794 = AXIS2_PLACEMENT_3D ( 'NONE', #35456, #27952, #58445 ) ;
#81795 = CARTESIAN_POINT ( 'NONE',  ( -5.963430220938290560, 11.82879003517447281, -10.32896413005679648 ) ) ;
#81796 = CARTESIAN_POINT ( 'NONE',  ( -0.3689425029237898834, 16.17874883491396076, -10.36894250292378850 ) ) ;
#81797 = ORIENTED_EDGE ( 'NONE', *, *, #94013, .F. ) ;
#81798 = CARTESIAN_POINT ( 'NONE',  ( 10.00000000000000000, 26.81368534415484106, -10.88017736071110342 ) ) ;
#81799 = CARTESIAN_POINT ( 'NONE',  ( 12.63842701281683922, 64.55059781766745175, -9.846743663894590881 ) ) ;
#81800 = ORIENTED_EDGE ( 'NONE', *, *, #19747, .F. ) ;
#81801 = CARTESIAN_POINT ( 'NONE',  ( 10.00000000000000178, 62.25893115100078745, 9.846743663894594434 ) ) ;
#81802 = ORIENTED_EDGE ( 'NONE', *, *, #15942, .F. ) ;
#81803 = ADVANCED_FACE ( 'NONE', ( #43447 ), #68929, .T. ) ;
#81804 = CARTESIAN_POINT ( 'NONE',  ( 4.559911319644449179, 68.89701867748817676, 9.422509992056141925 ) ) ;
#81805 = CARTESIAN_POINT ( 'NONE',  ( 19.84674366389459266, 58.71726448433411605, -2.638427012816827677 ) ) ;
#81806 = CARTESIAN_POINT ( 'NONE',  ( 6.565887622018943937, 33.08196800326374643, -12.81628187352647608 ) ) ;
#81808 = FACE_OUTER_BOUND ( 'NONE', #22194, .T. ) ;
#81807 = CARTESIAN_POINT ( 'NONE',  ( 17.96484262340118221, 4.938685344154837509, 7.964842623401181321 ) ) ;
#81809 = CARTESIAN_POINT ( 'NONE',  ( 19.84674366389459621, 3.508931151000785231, 7.409399052514197653E-17 ) ) ;
#81810 = CARTESIAN_POINT ( 'NONE',  ( 15.44008868035555260, 19.73035201082150536, 9.422509992056143702 ) ) ;
#81811 = EDGE_CURVE ( 'NONE', #85332, #35045, #16911, .T. ) ;
#81812 = STYLED_ITEM ( 'NONE', ( #53078 ), #65330 ) ;
#81813 = ORIENTED_EDGE ( 'NONE', *, *, #52829, .F. ) ;
#81814 = CARTESIAN_POINT ( 'NONE',  ( -1.099225684535947600, 58.70696800326375353, -6.408140936763238038 ) ) ;
#81815 = CARTESIAN_POINT ( 'NONE',  ( -0.8801773607111009756, 38.06368534415484106, 1.068504757029289695E-15 ) ) ;
#81816 = CARTESIAN_POINT ( 'NONE',  ( -7.771322705631588335, 4.175205849424987664E-16, 12.24159072199911868 ) ) ;
#81817 = CARTESIAN_POINT ( 'NONE',  ( 22.81628187352647785, 41.62363466993042493, 6.195893100308588602E-16 ) ) ;
#81818 = CARTESIAN_POINT ( 'NONE',  ( 7.084665262690076126, 47.02201867748818387, -10.88017736071110164 ) ) ;
#81819 = CIRCLE ( 'NONE', #16323, 0.2500000000000002220 ) ;
#81820 = CARTESIAN_POINT ( 'NONE',  ( 19.84674366389459266, 58.30059781766745886, 2.638427012816836559 ) ) ;
#81822 = DIRECTION ( 'NONE',  ( -0.000000000000000000, 1.000000000000000000, 0.000000000000000000 ) ) ;
#81821 = AXIS2_PLACEMENT_3D ( 'NONE', #51945, #59922, #82430 ) ;
#81823 = CARTESIAN_POINT ( 'NONE',  ( 0.1532563361054082862, 21.21726448433412315, 2.638427012816831674 ) ) ;
#81824 = AXIS2_PLACEMENT_3D ( 'NONE', #96785, #43753, #21771 ) ;
#81825 = CARTESIAN_POINT ( 'NONE',  ( 16.40814093676323893, 10.79030133659708923, 11.09922568453595026 ) ) ;
#81827 = CARTESIAN_POINT ( 'NONE',  ( 17.20831665107776587, 57.88393115100078745, 7.208316651077764980 ) ) ;
#81826 = CARTESIAN_POINT ( 'NONE',  ( 3.927832320392247389, 0.000000000000000000, -13.69797916712104602 ) ) ;
#81828 = CARTESIAN_POINT ( 'NONE',  ( 10.00000000000000178, 24.31368534415484106, 10.88017736071110342 ) ) ;
#81829 = CARTESIAN_POINT ( 'NONE',  ( 2.791683348922237240, 50.38393115100078035, -7.208316651077763204 ) ) ;
#81830 = DIRECTION ( 'NONE',  ( 0.000000000000000000, 1.000000000000000000, 0.000000000000000000 ) ) ;
#81831 = DIRECTION ( 'NONE',  ( 0.000000000000000000, 0.000000000000000000, -1.000000000000000000 ) ) ;
#81832 = CARTESIAN_POINT ( 'NONE',  ( 14.92337183194729633, 12.67559781766745353, 8.527530157486181039 ) ) ;
#81834 = ORIENTED_EDGE ( 'NONE', *, *, #91599, .F. ) ;
#81833 = CARTESIAN_POINT ( 'NONE',  ( 19.38216949554541557, 2.248634669930420049, -9.382169495545420901 ) ) ;
#81835 = AXIS2_PLACEMENT_3D ( 'NONE', #17824, #63787, #42293 ) ;
#81836 =( NAMED_UNIT ( * ) PLANE_ANGLE_UNIT ( ) SI_UNIT ( $, .RADIAN. ) );
#81837 = ADVANCED_FACE ( 'NONE', ( #98465 ), #15923, .T. ) ;
#81838 = CARTESIAN_POINT ( 'NONE',  ( 3.591859063236763294, 43.29030133659708923, -11.09922568453595026 ) ) ;
#81839 = CARTESIAN_POINT ( 'NONE',  ( 0.1532563361054082862, 31.21726448433412315, 2.638427012816831674 ) ) ;
#81840 = FILL_AREA_STYLE_COLOUR ( '', #29701 ) ;
#81841 = CARTESIAN_POINT ( 'NONE',  ( -0.3689425029237898834, 56.17874883491396076, -10.36894250292378850 ) ) ;
#81842 = CARTESIAN_POINT ( 'NONE',  ( 1.472469842513823179, 35.59226448433412315, -4.923371831947296329 ) ) ;
#81843 = EDGE_CURVE ( 'NONE', #58088, #61640, #7935, .T. ) ;
#81844 = ORIENTED_EDGE ( 'NONE', *, *, #26485, .F. ) ;
#81845 = CARTESIAN_POINT ( 'NONE',  ( 2.603489959281601873, 25.43575266056827289, -6.500000000000015987 ) ) ;
#81846 = CARTESIAN_POINT ( 'NONE',  ( 19.42250999205614193, 10.14701867748816966, 5.440088680355555262 ) ) ;
#81847 = CARTESIAN_POINT ( 'NONE',  ( -7.984789763142468466, 85.83064272735663280, -4.183481735294423132 ) ) ;
#81848 = CARTESIAN_POINT ( 'NONE',  ( -0.8801773607111008646, 18.27201867748817321, 2.915334737309923430 ) ) ;
#81849 = VECTOR ( 'NONE', #29671, 1000.000000000000000 ) ;
#81850 = CARTESIAN_POINT ( 'NONE',  ( -2.266590686148945544, 46.38708216824730357, -7.082119434687050408 ) ) ;
#81852 = CARTESIAN_POINT ( 'NONE',  ( -10.93781366033355695, 0.3639309795253648505, 10.26470809774060911 ) ) ;
#81851 = CARTESIAN_POINT ( 'NONE',  ( 20.36894250292379738, 54.92874883491396076, -10.36894250292379027 ) ) ;
#81853 = DIRECTION ( 'NONE',  ( 0.000000000000000000, 0.000000000000000000, 1.000000000000000000 ) ) ;
#81854 = B_SPLINE_CURVE_WITH_KNOTS ( 'NONE', 3,
 ( #97480, #60437, #21970, #52934 ),
 .UNSPECIFIED., .F., .F.,
 ( 4, 4 ),
 ( 5.204893179191169451E-17, 0.002562518741975293446 ),
 .UNSPECIFIED. ) ;
#81855 = CARTESIAN_POINT ( 'NONE',  ( 2.791683348922237240, 5.383931151000785675, -7.208316651077763204 ) ) ;
#81856 = CARTESIAN_POINT ( 'NONE',  ( -2.816281873526473856, 4.123634669930420493, 9.499525473075851096E-16 ) ) ;
#81857 = ORIENTED_EDGE ( 'NONE', *, *, #4197, .F. ) ;
#81858 = CARTESIAN_POINT ( 'NONE',  ( 20.88017736071110519, 45.56368534415484106, 2.639326808657452039E-16 ) ) ;
#81859 = DIRECTION ( 'NONE',  ( 0.000000000000000000, 1.000000000000000000, 0.000000000000000000 ) ) ;
#81860 = CARTESIAN_POINT ( 'NONE',  ( 7.361572987183169658, 64.96726448433412315, -9.846743663894592657 ) ) ;
#81861 = CARTESIAN_POINT ( 'NONE',  ( -4.164238869374098151, 1.595415501580634388, -3.795296366450310543 ) ) ;
#81862 = AXIS2_PLACEMENT_3D ( 'NONE', #12719, #95737, #89211 ) ;
#81863 = CARTESIAN_POINT ( 'NONE',  ( 5.076628168052703671, 26.84226448433411960, 8.527530157486179263 ) ) ;
#81864 = CARTESIAN_POINT ( 'NONE',  ( 4.130000000000002558, 1.019547802438464545, -2.750000000000000000 ) ) ;
#81865 = CARTESIAN_POINT ( 'NONE',  ( 2.917880565312950480, 40.97041550158063217, -12.26659068614894821 ) ) ;
#81866 = EDGE_CURVE ( 'NONE', #3611, #30159, #60450, .T. ) ;
#81867 = CARTESIAN_POINT ( 'NONE',  ( -14.62617646268090077, 14.49999999999999112, -3.327906561567068433 ) ) ;
#81869 = CARTESIAN_POINT ( 'NONE',  ( -26.69000000000001194, 92.00000000000000000, -10.09898361729590199 ) ) ;
#81868 = DIRECTION ( 'NONE',  ( -0.7933533402912325005, 0.000000000000000000, -0.6087614290087243196 ) ) ;
#81870 = CARTESIAN_POINT ( 'NONE',  ( 17.96484262340118221, 36.18868534415484106, -7.964842623401177768 ) ) ;
#81871 = CARTESIAN_POINT ( 'NONE',  ( 22.81628187352647785, 36.62363466993041783, 6.195893100308588602E-16 ) ) ;
#81872 = CARTESIAN_POINT ( 'NONE',  ( 17.96484262340118221, 6.188685344154836621, -7.964842623401177768 ) ) ;
#81873 = CARTESIAN_POINT ( 'NONE',  ( 10.00000000000000000, 32.87363466993042493, -12.81628187352647608 ) ) ;
#81874 = CARTESIAN_POINT ( 'NONE',  ( -1.099225684535947600, 59.54030133659708923, 6.408140936763237150 ) ) ;
#81875 = VERTEX_POINT ( 'NONE', #84906 ) ;
#81876 = CYLINDRICAL_SURFACE ( 'NONE', #26100, 0.2500000000000002220 ) ;
#81877 = ADVANCED_FACE ( 'NONE', ( #38431 ), #29118, .T. ) ;
#81878 = CARTESIAN_POINT ( 'NONE',  ( 17.39651004071897589, 34.08210964143323451, -6.499999999999361400 ) ) ;
#81879 = CARTESIAN_POINT ( 'NONE',  ( 6.204703633549690345, 25.76208216824730712, -14.16423886937410259 ) ) ;
#81880 = CARTESIAN_POINT ( 'NONE',  ( -0.3689425029237881626, 7.428748834913967869, 10.36894250292379027 ) ) ;
#81881 = CARTESIAN_POINT ( 'NONE',  ( 2.035157376598822676, 12.43868534415483751, -7.964842623401177768 ) ) ;
#81882 = CARTESIAN_POINT ( 'NONE',  ( 15.44008868035555793, 16.39701867748817321, -9.422509992056140149 ) ) ;
#81883 = CYLINDRICAL_SURFACE ( 'NONE', #46245, 0.09999999999999982514 ) ;
#81884 = CYLINDRICAL_SURFACE ( 'NONE', #92680, 0.5000000000000004441 ) ;
#81885 = CARTESIAN_POINT ( 'NONE',  ( 0.5774900079438590739, 47.64701867748817676, -5.440088680355550821 ) ) ;
#81886 = CARTESIAN_POINT ( 'NONE',  ( 0.5774900079438590739, 52.64701867748817676, -5.440088680355550821 ) ) ;
#81887 = CARTESIAN_POINT ( 'NONE',  ( 10.00000000000000000, 7.873634669930421381, -12.81628187352647608 ) ) ;
#81888 = DIRECTION ( 'NONE',  ( -0.000000000000000000, -1.000000000000000000, -0.000000000000000000 ) ) ;
#81889 = DIRECTION ( 'NONE',  ( -0.1650476058606676344, 0.000000000000000000, -0.9862856015372331031 ) ) ;
#81890 = CARTESIAN_POINT ( 'NONE',  ( 2.791683348922240793, 21.63393115100078745, 7.208316651077764092 ) ) ;
#81891 = CARTESIAN_POINT ( 'NONE',  ( 20.88017736071110519, 45.56368534415484106, 2.639326808657452039E-16 ) ) ;
#81892 = PRESENTATION_LAYER_ASSIGNMENT (  '', '', ( #24461 ) ) ;
#81893 = CARTESIAN_POINT ( 'NONE',  ( 13.43411237798105340, 15.58196800326374998, 12.81628187352647963 ) ) ;
#81894 = CARTESIAN_POINT ( 'NONE',  ( 5.076628168052704559, 0.1755978176674514724, -8.527530157486179263 ) ) ;
#81895 = CARTESIAN_POINT ( 'NONE',  ( 2.791683348922240793, 21.63393115100078745, 7.208316651077764092 ) ) ;
#81896 = CARTESIAN_POINT ( 'NONE',  ( -1.099225684535947600, 43.70696800326375353, -6.408140936763238038 ) ) ;
#81897 = AXIS2_PLACEMENT_3D ( 'NONE', #45197, #21219, #37226 ) ;
#81898 = CARTESIAN_POINT ( 'NONE',  ( 17.20831665107776587, 22.88393115100078745, 7.208316651077764980 ) ) ;
#81899 = VECTOR ( 'NONE', #57502, 1000.000000000000000 ) ;
#81900 = ORIENTED_EDGE ( 'NONE', *, *, #62762, .T. ) ;
#81901 = CARTESIAN_POINT ( 'NONE',  ( -2.266590686148945544, 2.220415501580634388, 7.082119434687048631 ) ) ;
#81902 = FACE_OUTER_BOUND ( 'NONE', #57558, .T. ) ;
#81903 = CARTESIAN_POINT ( 'NONE',  ( 2.035157376598824452, 23.68868534415484461, 7.964842623401179544 ) ) ;
#81904 = CARTESIAN_POINT ( 'NONE',  ( 20.36894250292379382, 28.67874883491396787, 10.36894250292379205 ) ) ;
#81905 = CARTESIAN_POINT ( 'NONE',  ( 7.361572987183169658, 34.96726448433411605, -9.846743663894592657 ) ) ;
#81906 = CARTESIAN_POINT ( 'NONE',  ( 2.035157376598822676, 22.43868534415483396, -7.964842623401177768 ) ) ;
#81907 = CARTESIAN_POINT ( 'NONE',  ( 19.42250999205614548, 20.98035201082150891, -5.440088680355545492 ) ) ;
#81908 = ORIENTED_EDGE ( 'NONE', *, *, #61660, .F. ) ;
#81909 = VECTOR ( 'NONE', #68330, 1000.000000000000000 ) ;
#81910 = CARTESIAN_POINT ( 'NONE',  ( 17.96484262340118221, 21.18868534415483396, -7.964842623401177768 ) ) ;
#81911 = CARTESIAN_POINT ( 'NONE',  ( 6.565887622018943937, 40.16530133659708923, 12.81628187352647430 ) ) ;
#81912 = CARTESIAN_POINT ( 'NONE',  ( 15.44008868035555260, 39.73035201082150536, 9.422509992056143702 ) ) ;
#81914 = CARTESIAN_POINT ( 'NONE',  ( -0.8801773607110991993, 37.85535201082151247, -2.915334737309923874 ) ) ;
#81913 = LINE ( 'NONE', #72934, #34478 ) ;
#81915 = ORIENTED_EDGE ( 'NONE', *, *, #72783, .F. ) ;
#81916 = CARTESIAN_POINT ( 'NONE',  ( 5.076628168052703671, 56.84226448433412315, 8.527530157486179263 ) ) ;
#81917 = CARTESIAN_POINT ( 'NONE',  ( -0.8801773607110991993, 32.85535201082151247, -2.915334737309923874 ) ) ;
#81918 = SURFACE_STYLE_USAGE ( .BOTH. , #96456 ) ;
#81919 = SURFACE_STYLE_USAGE ( .BOTH. , #6923 ) ;
#81920 = CARTESIAN_POINT ( 'NONE',  ( 14.82269085861168811, 0.5000000000000004441, -2.299529454046961519 ) ) ;
#81921 = DIRECTION ( 'NONE',  ( 0.000000000000000000, 0.000000000000000000, 1.000000000000000000 ) ) ;
#81922 = CARTESIAN_POINT ( 'NONE',  ( 20.36894250292379738, 44.92874883491396787, -10.36894250292379027 ) ) ;
#81923 = CARTESIAN_POINT ( 'NONE',  ( -0.8801773607111009756, 53.06368534415484106, 1.068504757029289695E-15 ) ) ;
#81924 = CARTESIAN_POINT ( 'NONE',  ( 14.92337183194729988, 64.34226448433412315, -8.527530157486177487 ) ) ;
#81925 = DIRECTION ( 'NONE',  ( 0.000000000000000000, 1.000000000000000000, 0.000000000000000000 ) ) ;
#81926 = CARTESIAN_POINT ( 'NONE',  ( 17.20831665107776587, 44.13393115100078745, -7.208316651077762316 ) ) ;
#81927 = CARTESIAN_POINT ( 'NONE',  ( 7.361572987183169658, 4.967264484334119601, -9.846743663894592657 ) ) ;
#81928 = CARTESIAN_POINT ( 'NONE',  ( 0.1532563361054083140, 21.00893115100078745, 1.131784320476157264E-15 ) ) ;
#81929 = VERTEX_POINT ( 'NONE', #69410 ) ;
#81930 = CARTESIAN_POINT ( 'NONE',  ( 0.1532563361054100626, 25.80059781766744820, -2.638427012816831230 ) ) ;
#81931 = CARTESIAN_POINT ( 'NONE',  ( -3.434112377981047626, -24.83469866340290721, 12.81628187352647963 ) ) ;
#81932 = CARTESIAN_POINT ( 'NONE',  ( 4.559911319644449179, 22.23035201082150536, -9.422509992056141925 ) ) ;
#81933 = CARTESIAN_POINT ( 'NONE',  ( 2.791683348922237240, 20.38393115100078745, -7.208316651077763204 ) ) ;
#81934 = CARTESIAN_POINT ( 'NONE',  ( 15.44008868035555793, 56.39701867748817676, -9.422509992056140149 ) ) ;
#81936 = CARTESIAN_POINT ( 'NONE',  ( 22.81628187352648496, 51.83196800326376064, -3.434112377981050290 ) ) ;
#81935 = CARTESIAN_POINT ( 'NONE',  ( 20.88017736071110875, 35.77201867748816966, -2.915334737309920765 ) ) ;
#81937 = CARTESIAN_POINT ( 'NONE',  ( -0.3689425029237898834, 41.17874883491397497, -10.36894250292378850 ) ) ;
#81938 = AXIS2_PLACEMENT_3D ( 'NONE', #95416, #33901, #10444 ) ;
#81939 = EDGE_CURVE ( 'NONE', #80099, #38899, #85398, .T. ) ;
#81940 = AXIS2_PLACEMENT_3D ( 'NONE', #47655, #71639, #62639 ) ;
#81941 = CARTESIAN_POINT ( 'NONE',  ( -14.49440716394874151, 3.911302179139366829E-16, 0.4026921475165256004 ) ) ;
#81942 = VERTEX_POINT ( 'NONE', #46895 ) ;
#81943 = CARTESIAN_POINT ( 'NONE',  ( 10.00000000000000000, 2.873634669930420049, -12.81628187352647608 ) ) ;
#81944 = CARTESIAN_POINT ( 'NONE',  ( 0.5774900079438590739, 7.647018677488171434, -5.440088680355550821 ) ) ;
#81945 = CARTESIAN_POINT ( 'NONE',  ( 17.96484262340118221, 46.18868534415484106, -7.964842623401177768 ) ) ;
#81946 = DIRECTION ( 'NONE',  ( -0.000000000000000000, -0.000000000000000000, 1.000000000000000000 ) ) ;
#81947 = ORIENTED_EDGE ( 'NONE', *, *, #42696, .T. ) ;
#81948 = CARTESIAN_POINT ( 'NONE',  ( 7.361572987183169658, 14.96726448433411960, -9.846743663894592657 ) ) ;
#81949 = PRODUCT_DEFINITION_SHAPE ( 'NONE', 'NONE',  #98990 ) ;
#81950 = CARTESIAN_POINT ( 'NONE',  ( 19.42250999205614193, 55.14701867748817676, 5.440088680355555262 ) ) ;
#81951 = CARTESIAN_POINT ( 'NONE',  ( 18.52753015748618282, 33.92559781766745886, -4.923371831947291888 ) ) ;
#81952 = CARTESIAN_POINT ( 'NONE',  ( 19.84674366389459621, 28.50893115100078745, 7.409399052514197653E-17 ) ) ;
#81953 = CARTESIAN_POINT ( 'NONE',  ( 18.52753015748617571, 13.09226448433411960, 4.923371831947298993 ) ) ;
#81954 = DIRECTION ( 'NONE',  ( 0.000000000000000000, 0.000000000000000000, -1.000000000000000000 ) ) ;
#81956 = CARTESIAN_POINT ( 'NONE',  ( 64.56412365047461321, 44.99999999999998579, 0.000000000000000000 ) ) ;
#81955 = CARTESIAN_POINT ( 'NONE',  ( 20.88017736071110164, 65.35535201082150536, 2.915334737309930979 ) ) ;
#81957 = CARTESIAN_POINT ( 'NONE',  ( 10.09974179609097611, -32.02510747890637077, 4.000000000000000000 ) ) ;
#81958 = CARTESIAN_POINT ( 'NONE',  ( 5.076628168052703671, 31.84226448433412315, 8.527530157486179263 ) ) ;
#81959 = CARTESIAN_POINT ( 'NONE',  ( -2.816281873526473856, 54.33196800326376064, 3.434112377981055619 ) ) ;
#81960 = DIRECTION ( 'NONE',  ( -2.131628207280300873E-14, 0.000000000000000000, 1.000000000000000000 ) ) ;
#81961 = EDGE_CURVE ( 'NONE', #42454, #18033, #68960, .T. ) ;
#81962 = CARTESIAN_POINT ( 'NONE',  ( 19.84674366389459266, 63.30059781766745886, 2.638427012816836559 ) ) ;
#81963 = CIRCLE ( 'NONE', #51645, 18.53834841531100608 ) ;
#81964 = CARTESIAN_POINT ( 'NONE',  ( -0.8801773607111009756, 3.063685344154837509, 1.068504757029289695E-15 ) ) ;
#81965 = CARTESIAN_POINT ( 'NONE',  ( 24.16423886937409904, 24.09541550158063927, 3.795296366450317205 ) ) ;
#81966 = CIRCLE ( 'NONE', #46858, 0.5000000000000004441 ) ;
#81967 = EDGE_CURVE ( 'NONE', #5362, #58376, #60915, .T. ) ;
#81968 = CARTESIAN_POINT ( 'NONE',  ( 10.00000000000000178, 70.00000000000000000, 0.000000000000000000 ) ) ;
#81969 = AXIS2_PLACEMENT_3D ( 'NONE', #71428, #10912, #19395 ) ;
#81970 = CARTESIAN_POINT ( 'NONE',  ( 24.16423886937410614, 34.30374883491396787, 8.672049930838204340E-16 ) ) ;
#81971 = B_SPLINE_CURVE_WITH_KNOTS ( 'NONE', 3,
 ( #93421, #95388, #47910, #26391, #18912, #40437 ),
 .UNSPECIFIED., .F., .F.,
 ( 4, 2, 4 ),
 ( 0.0002800047503720853067, 0.0006862100262544242307, 0.001092415302136763317 ),
 .UNSPECIFIED. ) ;
#81972 = CARTESIAN_POINT ( 'NONE',  ( 17.08211943468705840, 40.13708216824731068, -12.26659068614894466 ) ) ;
#81973 = CARTESIAN_POINT ( 'NONE',  ( -0.3689425029237898834, 11.17874883491396787, -10.36894250292378850 ) ) ;
#81975 = CARTESIAN_POINT ( 'NONE',  ( -0.8801773607111009756, 68.06368534415484817, 1.068504757029289695E-15 ) ) ;
#81974 = CARTESIAN_POINT ( 'NONE',  ( 17.08211943468705840, 15.13708216824730179, -12.26659068614894466 ) ) ;
#81976 = CARTESIAN_POINT ( 'NONE',  ( 7.084665262690076126, 54.10535201082151247, 10.88017736071109987 ) ) ;
#81977 = CARTESIAN_POINT ( 'NONE',  ( -5.419894505350681513, 0.3640475087720754788, 13.98659156302455209 ) ) ;
#81978 = ORIENTED_EDGE ( 'NONE', *, *, #3169, .T. ) ;
#81980 = AXIS2_PLACEMENT_3D ( 'NONE', #55785, #11748, #57728 ) ;
#81979 = CARTESIAN_POINT ( 'NONE',  ( 1.472469842513823179, 31.42559781766745530, 4.923371831947296329 ) ) ;
#81982 = CARTESIAN_POINT ( 'NONE',  ( 0.1532563361054082862, 26.21726448433411605, 2.638427012816831674 ) ) ;
#81981 = CARTESIAN_POINT ( 'NONE',  ( 5.148594389986301145, 1.711006553453686685E-16, -13.69051944078647054 ) ) ;
#81983 = CARTESIAN_POINT ( 'NONE',  ( 4.559911319644449179, 13.89701867748817321, 9.422509992056141925 ) ) ;
#81984 = CARTESIAN_POINT ( 'NONE',  ( 19.38216949554541557, 62.24863466993041072, -9.382169495545420901 ) ) ;
#81985 = CARTESIAN_POINT ( 'NONE',  ( 19.84674366389459266, 53.30059781766744464, 2.638427012816836559 ) ) ;
#81986 = FACE_OUTER_BOUND ( 'NONE', #65804, .T. ) ;
#81987 = CARTESIAN_POINT ( 'NONE',  ( 16.40814093676324603, 37.45696800326376064, -11.09922568453594671 ) ) ;
#81988 = CARTESIAN_POINT ( 'NONE',  ( -7.082119434687044190, -17.36291783175269288, 12.26659068614894998 ) ) ;
#81989 =( BOUNDED_SURFACE ( )  B_SPLINE_SURFACE ( 1, 2, ( 
 ( #32026, #48517, #31544, #62039, #9053, #18040, #47543, #49014, #94513, #17061, #9543, #32534, #78534, #86535, #63522, #2074, #94026, #26032, #56041, #79521, #40546, #63032, #55545, #79020, #62530, #86044, #71046, #2569, #10531, #33025, #24570, #25549, #39069, #41041, #71541, #3048, #33503, #1083, #92539, #24069, #54537, #85053, #16565, #85549, #47039, #39565, #93037, #55030, #80001, #42030, #34489, #64493, #11506, #72494, #66477, #95000, #72006, #12978, #97005, #19019, #87507, #72988, #34982, #27979, #49497, #65483, #4518, #42991, #95507, #4026, #43475, #5003, #73976, #28483, #58977, #42506, #96506, #89478, #50980, #64982, #88489, #26999, #26508, #57004, #57497, #58477, #87991, #96006, #19991, #50493, #81476, #80507, #19504, #5502, #50001, #80990, #12003, #27489, #57982, #12491, #88989, #73474, #35485, #65981, #20493, #35975, #20991, #51477, #41538, #3535, #11021, #33995, #82467, #14483, #61433, #51980, #6973, #52461, #45958, #13987, #37479, #15475, #21482, #60453, #13483, #75952, #30439, #76447, #44463, #59956, #38460, #83949, #74965, #52948, #67968, #89966, #90447, #485, #91939, #29449, #21986, #53440, #7962, #6470, #91450, #74463, #5989, #36974, #60939, #82964, #30934, #68953, #44954, #75458, #98493, #90942, #22975, #7479, #29947, #37976, #23469, #98986, #81970, #22472, #83459, #14980, #43961, #67473, #45450, #68465, #36484, #66976, #97496, #97994, #28960, #59464, #62410, #25437, #9425, #92916, #85928, #39929, #47905, #1949, #33385, #46441, #1457, #40432, #85426, #8442, #15949, #23951, #84932, #77414, #38949, #54424, #16444, #10416, #69441, #76933, #55920, #40923, #61924, #31421, #16935, #77919, #70931, #92426, #70432, #47416, #17438, #39447, #46922, #86419, #78410, #17920, #71421, #2937, #32413, #2448, #63883, #8930, #62914, #48404, #69938, #93415, #84450, #9928, #32905, #78907, #31909, #24445, #94395, #53943, #54913, #24938, #55420, #63404, #93909, #961, #5386, #72375, #34372, #96388, #27862, #18906, #35368, #18408, #48891, #64378, #4889, #64862, #43359, #50869, #3905, #95382, #19387, #4401, #73361, #50366, #26884, #80874, #12860, #42878, #35861, #34869, #57376, #42388, #65859, #87389, #87871, #49872, #80385, #58347, #65363, #11391, #88376, #73856, #11888, #88869, #72867, #95892, #57864, #27372, #19873, #12372, #66349, #79402, #20375, #81361, #25910, #10906, #86898, #94888, #56886, #49383, #41428, #26386, #79884, #56412, #71889, #3412, #33873, #41913, #5867, #74339, #59837, #21866, #14863, #36358, #52344, #90326, #29828, #82342, #66854, #98868, #90831, #30322, #15359, #45843, #29336, #83341, #76329, #37857, #28840 ),
 ( #82841, #36858, #67854, #14361, #44830, #98373, #97372, #75335, #6849, #37361, #60337, #59343, #52832, #22358, #7846, #89845, #74848, #53324, #60824, #21362, #45335, #75835, #51856, #6349, #38344, #96888, #44342, #67350, #68347, #91324, #13863, #7355, #89358, #20869, #97876, #22851, #83833, #28364, #58852, #51360, #81846, #13359, #43845, #17318, #93295, #8816, #24819, #55804, #85806, #48282, #77795, #46809, #85309, #47793, #31306, #77301, #1345, #92803, #78291, #47294, #54305, #32290, #86297, #39328, #40308, #24330, #69823, #1834, #54793, #62795, #16817, #78794, #61318, #16326, #55295, #31797, #23346, #30819, #38833, #849, #92313, #53829, #69327, #61808, #25317, #84340, #91829, #70814, #17804, #76813, #46326, #62295, #9305, #9807, #8329, #39814, #70317, #2329, #84818, #23839, #32785, #63282, #93788, #10302, #68839, #371, #15843, #58224, #80757, #71780, #19266, #3289, #94273, #86790, #33754, #57746, #25796, #72261, #49750, #80260, #12252, #11269, #64256, #71301, #33272, #94771, #79770, #41307, #3790, #20255, #10790, #64745, #41789, #4769, #26270, #95257, #73241, #79280, #11764, #2822, #34750, #88249, #35241, #19757, #49270, #88745, #65739, #18788, #34245, #26763, #42272, #50242, #65239, #57255, #95764, #27742, #42759, #50756, #72743, #87752, #4276, #96268, #56771, #27248, #81242, #40800, #63766, #56295, #87267, #18291, #48774, #21244, #83223, #67234, #51742, #44722, #97757, #6731, #59722, #91204, #5265, #59223, #98254, #44223, #66231, #73735, #81726, #43734, #36242, #96766, #13240, #74220, #68237, #28241, #35743, #14746, #98754, #20749, #89241, #74727, #36743, #29712, #51240, #29223, #6241, #75219, #97263, #5753, #45220, #37247, #75717, #30204, #60707, #90216, #60220, #22732, #52716, #66738, #21749, #28732, #58736, #89727, #82226, #90714, #13740, #52230, #82722, #14241, #7231, #67736, #22239, #43240, #37738, #53215, #12741, #84223, #16207, #63161, #53702, #8695, #54189, #47681, #15732, #39211, #17204, #23230, #62173, #15237, #77678, #32169, #78175, #46212, #61685, #40182, #85683, #76699, #54674, #69698, #91711, #92202, #2207, #93669, #31191, #23726, #55168, #9686, #8219, #93171, #76220, #7733, #38713, #38229, #45718, #69212, #738, #84702, #68716, #46690, #77187, #70689, #247, #30695, #32668, #25203, #1228, #61205, #31681, #92682, #1711, #24207, #85193, #16700, #47173, #9191, #39705, #83717, #70192, #62670, #24696, #73118, #87143, #42161, #4659, #95644, #86670, #34132, #18174, #10185, #2705, #48656, #72626, #40679, #18666, #64624, #95133, #27130, #26162, #79156, #86180, #48162, #10670, #94654, #56177, #49154, #35120 ) ),
 .UNSPECIFIED., .F., .F., .T. ) 
 B_SPLINE_SURFACE_WITH_KNOTS ( ( 2, 2 ),
 ( 3, 2, 2, 2, 2, 2, 2, 2, 2, 2, 2, 2, 2, 2, 2, 2, 2, 2, 2, 2, 2, 2, 2, 2, 2, 2, 2, 2, 2, 2, 2, 2, 2, 2, 2, 2, 2, 2, 2, 2, 2, 2, 2, 2, 2, 2, 2, 2, 2, 2, 2, 2, 2, 2, 2, 2, 2, 2, 2, 2, 2, 2, 2, 2, 2, 2, 2, 2, 2, 2, 2, 2, 2, 2, 2, 2, 2, 2, 2, 2, 2, 2, 2, 2, 2, 2, 2, 2, 2, 2, 2, 2, 2, 2, 2, 2, 2, 2, 2, 2, 2, 2, 2, 2, 2, 2, 2, 2, 2, 2, 2, 2, 2, 2, 2, 2, 2, 2, 2, 2, 2, 2, 2, 2, 2, 2, 2, 2, 2, 2, 2, 2, 2, 2, 2, 2, 2, 2, 2, 2, 2, 2, 2, 2, 2, 2, 2, 2, 2, 2, 2, 2, 2, 2, 2, 2, 2, 2, 2, 2, 2, 2, 3 ),
 ( 0.000000000000000000, 1.000000000000000000 ),
 ( 0.000000000000000000, 0.005952380952380952051, 0.01190476190476190410, 0.01785714285714285615, 0.02380952380952380820, 0.02976190476190476025, 0.03571428571428571230, 0.04166666666666666435, 0.04761904761904761640, 0.05357142857142856845, 0.05952380952380952051, 0.06547619047619047949, 0.07142857142857142461, 0.07738095238095238360, 0.08333333333333332871, 0.08928571428571428770, 0.09523809523809523281, 0.1011904761904761918, 0.1071428571428571369, 0.1130952380952380959, 0.1190476190476190410, 0.1250000000000000000, 0.1309523809523809590, 0.1369047619047619180, 0.1428571428571428492, 0.1488095238095238082, 0.1547619047619047672, 0.1607142857142857262, 0.1666666666666666574, 0.1726190476190476164, 0.1785714285714285754, 0.1845238095238095344, 0.1904761904761904656, 0.1964285714285714246, 0.2023809523809523836, 0.2083333333333333426, 0.2142857142857142738, 0.2202380952380952328, 0.2261904761904761918, 0.2321428571428571508, 0.2380952380952380820, 0.2440476190476190410, 0.2500000000000000000, 0.2559523809523809312, 0.2619047619047619180, 0.2678571428571428492, 0.2738095238095238360, 0.2797619047619047672, 0.2857142857142856984, 0.2916666666666666852, 0.2976190476190476164, 0.3035714285714285476, 0.3095238095238095344, 0.3154761904761904656, 0.3214285714285714524, 0.3273809523809523836, 0.3333333333333333148, 0.3392857142857143016, 0.3452380952380952328, 0.3511904761904761640, 0.3571428571428571508, 0.3630952380952380820, 0.3690476190476190688, 0.3750000000000000000, 0.3809523809523809312, 0.3869047619047619180, 0.3928571428571428492, 0.3988095238095238360, 0.4047619047619047672, 0.4107142857142856984, 0.4166666666666666852, 0.4226190476190476164, 0.4285714285714285476, 0.4345238095238095344, 0.4404761904761904656, 0.4464285714285714524, 0.4523809523809523836, 0.4583333333333333148, 0.4642857142857143016, 0.4702380952380952328, 0.4761904761904761640, 0.4821428571428571508, 0.4880952380952380820, 0.4940476190476190688, 0.5000000000000000000, 0.5059523809523809312, 0.5119047619047618625, 0.5178571428571429047, 0.5238095238095238360, 0.5297619047619047672, 0.5357142857142856984, 0.5416666666666666297, 0.5476190476190476719, 0.5535714285714286031, 0.5595238095238095344, 0.5654761904761904656, 0.5714285714285713969, 0.5773809523809523281, 0.5833333333333333703, 0.5892857142857143016, 0.5952380952380952328, 0.6011904761904761640, 0.6071428571428570953, 0.6130952380952381375, 0.6190476190476190688, 0.6250000000000000000, 0.6309523809523809312, 0.6369047619047618625, 0.6428571428571429047, 0.6488095238095238360, 0.6547619047619047672, 0.6607142857142856984, 0.6666666666666666297, 0.6726190476190476719, 0.6785714285714286031, 0.6845238095238095344, 0.6904761904761904656, 0.6964285714285713969, 0.7023809523809523281, 0.7083333333333333703, 0.7142857142857143016, 0.7202380952380952328, 0.7261904761904761640, 0.7321428571428570953, 0.7380952380952381375, 0.7440476190476190688, 0.7500000000000000000, 0.7559523809523809312, 0.7619047619047618625, 0.7678571428571429047, 0.7738095238095238360, 0.7797619047619047672, 0.7857142857142856984, 0.7916666666666666297, 0.7976190476190476719, 0.8035714285714286031, 0.8095238095238095344, 0.8154761904761904656, 0.8214285714285713969, 0.8273809523809523281, 0.8333333333333333703, 0.8392857142857143016, 0.8452380952380952328, 0.8511904761904761640, 0.8571428571428570953, 0.8630952380952381375, 0.8690476190476190688, 0.8750000000000000000, 0.8809523809523809312, 0.8869047619047618625, 0.8928571428571429047, 0.8988095238095238360, 0.9047619047619047672, 0.9107142857142856984, 0.9166666666666666297, 0.9226190476190476719, 0.9285714285714286031, 0.9345238095238095344, 0.9404761904761904656, 0.9464285714285713969, 0.9523809523809523281, 0.9583333333333333703, 0.9642857142857143016 ),
 .UNSPECIFIED. ) 
 GEOMETRIC_REPRESENTATION_ITEM ( )  RATIONAL_B_SPLINE_SURFACE ( (
 ( 1.000000000000000000, 0.9659258262890683122, 1.000000000000000000, 0.9659258262890683122, 1.000000000000000000, 0.9659258262890683122, 1.000000000000000000, 0.9659258262890683122, 1.000000000000000000, 0.9659258262890683122, 1.000000000000000000, 0.9659258262890683122, 1.000000000000000000, 0.9659258262890683122, 1.000000000000000000, 0.9659258262890683122, 1.000000000000000000, 0.9659258262890683122, 1.000000000000000000, 0.9659258262890683122, 1.000000000000000000, 0.9659258262890683122, 1.000000000000000000, 0.9659258262890683122, 1.000000000000000000, 0.9659258262890683122, 1.000000000000000000, 0.9659258262890683122, 1.000000000000000000, 0.9659258262890683122, 1.000000000000000000, 0.9659258262890683122, 1.000000000000000000, 0.9659258262890683122, 1.000000000000000000, 0.9659258262890683122, 1.000000000000000000, 0.9659258262890683122, 1.000000000000000000, 0.9659258262890683122, 1.000000000000000000, 0.9659258262890683122, 1.000000000000000000, 0.9659258262890683122, 1.000000000000000000, 0.9659258262890683122, 1.000000000000000000, 0.9659258262890683122, 1.000000000000000000, 0.9659258262890683122, 1.000000000000000000, 0.9659258262890683122, 1.000000000000000000, 0.9659258262890683122, 1.000000000000000000, 0.9659258262890683122, 1.000000000000000000, 0.9659258262890683122, 1.000000000000000000, 0.9659258262890683122, 1.000000000000000000, 0.9659258262890683122, 1.000000000000000000, 0.9659258262890683122, 1.000000000000000000, 0.9659258262890683122, 1.000000000000000000, 0.9659258262890683122, 1.000000000000000000, 0.9659258262890683122, 1.000000000000000000, 0.9659258262890683122, 1.000000000000000000, 0.9659258262890683122, 1.000000000000000000, 0.9659258262890683122, 1.000000000000000000, 0.9659258262890683122, 1.000000000000000000, 0.9659258262890683122, 1.000000000000000000, 0.9659258262890683122, 1.000000000000000000, 0.9659258262890683122, 1.000000000000000000, 0.9659258262890683122, 1.000000000000000000, 0.9659258262890683122, 1.000000000000000000, 0.9659258262890683122, 1.000000000000000000, 0.9659258262890683122, 1.000000000000000000, 0.9659258262890683122, 1.000000000000000000, 0.9659258262890683122, 1.000000000000000000, 0.9659258262890683122, 1.000000000000000000, 0.9659258262890683122, 1.000000000000000000, 0.9659258262890683122, 1.000000000000000000, 0.9659258262890683122, 1.000000000000000000, 0.9659258262890683122, 1.000000000000000000, 0.9659258262890683122, 1.000000000000000000, 0.9659258262890683122, 1.000000000000000000, 0.9659258262890683122, 1.000000000000000000, 0.9659258262890683122, 1.000000000000000000, 0.9659258262890683122, 1.000000000000000000, 0.9659258262890683122, 1.000000000000000000, 0.9659258262890683122, 1.000000000000000000, 0.9659258262890683122, 1.000000000000000000, 0.9659258262890683122, 1.000000000000000000, 0.9659258262890683122, 1.000000000000000000, 0.9659258262890683122, 1.000000000000000000, 0.9659258262890683122, 1.000000000000000000, 0.9659258262890683122, 1.000000000000000000, 0.9659258262890683122, 1.000000000000000000, 0.9659258262890683122, 1.000000000000000000, 0.9659258262890683122, 1.000000000000000000, 0.9659258262890683122, 1.000000000000000000, 0.9659258262890683122, 1.000000000000000000, 0.9659258262890683122, 1.000000000000000000, 0.9659258262890683122, 1.000000000000000000, 0.9659258262890683122, 1.000000000000000000, 0.9659258262890683122, 1.000000000000000000, 0.9659258262890683122, 1.000000000000000000, 0.9659258262890683122, 1.000000000000000000, 0.9659258262890683122, 1.000000000000000000, 0.9659258262890683122, 1.000000000000000000, 0.9659258262890683122, 1.000000000000000000, 0.9659258262890683122, 1.000000000000000000, 0.9659258262890683122, 1.000000000000000000, 0.9659258262890683122, 1.000000000000000000, 0.9659258262890683122, 1.000000000000000000, 0.9659258262890683122, 1.000000000000000000, 0.9659258262890683122, 1.000000000000000000, 0.9659258262890683122, 1.000000000000000000, 0.9659258262890683122, 1.000000000000000000, 0.9659258262890683122, 1.000000000000000000, 0.9659258262890683122, 1.000000000000000000, 0.9659258262890683122, 1.000000000000000000, 0.9659258262890683122, 1.000000000000000000, 0.9659258262890683122, 1.000000000000000000, 0.9659258262890683122, 1.000000000000000000, 0.9659258262890683122, 1.000000000000000000, 0.9659258262890683122, 1.000000000000000000, 0.9659258262890683122, 1.000000000000000000, 0.9659258262890683122, 1.000000000000000000, 0.9659258262890683122, 1.000000000000000000, 0.9659258262890683122, 1.000000000000000000, 0.9659258262890683122, 1.000000000000000000, 0.9659258262890683122, 1.000000000000000000, 0.9659258262890683122, 1.000000000000000000, 0.9659258262890683122, 1.000000000000000000, 0.9659258262890683122, 1.000000000000000000, 0.9659258262890683122, 1.000000000000000000, 0.9659258262890683122, 1.000000000000000000, 0.9659258262890683122, 1.000000000000000000, 0.9659258262890683122, 1.000000000000000000, 0.9659258262890683122, 1.000000000000000000, 0.9659258262890683122, 1.000000000000000000, 0.9659258262890683122, 1.000000000000000000, 0.9659258262890683122, 1.000000000000000000, 0.9659258262890683122, 1.000000000000000000, 0.9659258262890683122, 1.000000000000000000, 0.9659258262890683122, 1.000000000000000000, 0.9659258262890683122, 1.000000000000000000, 0.9659258262890683122, 1.000000000000000000, 0.9659258262890683122, 1.000000000000000000, 0.9659258262890683122, 1.000000000000000000, 0.9659258262890683122, 1.000000000000000000, 0.9659258262890683122, 1.000000000000000000, 0.9659258262890683122, 1.000000000000000000, 0.9659258262890683122, 1.000000000000000000, 0.9659258262890683122, 1.000000000000000000, 0.9659258262890683122, 1.000000000000000000, 0.9659258262890683122, 1.000000000000000000, 0.9659258262890683122, 1.000000000000000000, 0.9659258262890683122, 1.000000000000000000, 0.9659258262890683122, 1.000000000000000000, 0.9659258262890683122, 1.000000000000000000, 0.9659258262890683122, 1.000000000000000000, 0.9659258262890683122, 1.000000000000000000, 0.9659258262890683122, 1.000000000000000000, 0.9659258262890683122, 1.000000000000000000, 0.9659258262890683122, 1.000000000000000000, 0.9659258262890683122, 1.000000000000000000, 0.9659258262890683122, 1.000000000000000000, 0.9659258262890683122, 1.000000000000000000, 0.9659258262890683122, 1.000000000000000000, 0.9659258262890683122, 1.000000000000000000, 0.9659258262890683122, 1.000000000000000000, 0.9659258262890683122, 1.000000000000000000, 0.9659258262890683122, 1.000000000000000000, 0.9659258262890683122, 1.000000000000000000, 0.9659258262890683122, 1.000000000000000000, 0.9659258262890683122, 1.000000000000000000, 0.9659258262890683122, 1.000000000000000000, 0.9659258262890683122, 1.000000000000000000, 0.9659258262890683122, 1.000000000000000000, 0.9659258262890683122, 1.000000000000000000, 0.9659258262890683122, 1.000000000000000000, 0.9659258262890683122, 1.000000000000000000, 0.9659258262890683122, 1.000000000000000000, 0.9659258262890683122, 1.000000000000000000, 0.9659258262890683122, 1.000000000000000000, 0.9659258262890683122, 1.000000000000000000, 0.9659258262890683122, 1.000000000000000000, 0.9659258262890683122, 1.000000000000000000, 0.9659258262890683122, 1.000000000000000000, 0.9659258262890683122, 1.000000000000000000, 0.9659258262890683122, 1.000000000000000000),
 ( 1.000000000000000000, 0.9659258262890683122, 1.000000000000000000, 0.9659258262890683122, 1.000000000000000000, 0.9659258262890683122, 1.000000000000000000, 0.9659258262890683122, 1.000000000000000000, 0.9659258262890683122, 1.000000000000000000, 0.9659258262890683122, 1.000000000000000000, 0.9659258262890683122, 1.000000000000000000, 0.9659258262890683122, 1.000000000000000000, 0.9659258262890683122, 1.000000000000000000, 0.9659258262890683122, 1.000000000000000000, 0.9659258262890683122, 1.000000000000000000, 0.9659258262890683122, 1.000000000000000000, 0.9659258262890683122, 1.000000000000000000, 0.9659258262890683122, 1.000000000000000000, 0.9659258262890683122, 1.000000000000000000, 0.9659258262890683122, 1.000000000000000000, 0.9659258262890683122, 1.000000000000000000, 0.9659258262890683122, 1.000000000000000000, 0.9659258262890683122, 1.000000000000000000, 0.9659258262890683122, 1.000000000000000000, 0.9659258262890683122, 1.000000000000000000, 0.9659258262890683122, 1.000000000000000000, 0.9659258262890683122, 1.000000000000000000, 0.9659258262890683122, 1.000000000000000000, 0.9659258262890683122, 1.000000000000000000, 0.9659258262890683122, 1.000000000000000000, 0.9659258262890683122, 1.000000000000000000, 0.9659258262890683122, 1.000000000000000000, 0.9659258262890683122, 1.000000000000000000, 0.9659258262890683122, 1.000000000000000000, 0.9659258262890683122, 1.000000000000000000, 0.9659258262890683122, 1.000000000000000000, 0.9659258262890683122, 1.000000000000000000, 0.9659258262890683122, 1.000000000000000000, 0.9659258262890683122, 1.000000000000000000, 0.9659258262890683122, 1.000000000000000000, 0.9659258262890683122, 1.000000000000000000, 0.9659258262890683122, 1.000000000000000000, 0.9659258262890683122, 1.000000000000000000, 0.9659258262890683122, 1.000000000000000000, 0.9659258262890683122, 1.000000000000000000, 0.9659258262890683122, 1.000000000000000000, 0.9659258262890683122, 1.000000000000000000, 0.9659258262890683122, 1.000000000000000000, 0.9659258262890683122, 1.000000000000000000, 0.9659258262890683122, 1.000000000000000000, 0.9659258262890683122, 1.000000000000000000, 0.9659258262890683122, 1.000000000000000000, 0.9659258262890683122, 1.000000000000000000, 0.9659258262890683122, 1.000000000000000000, 0.9659258262890683122, 1.000000000000000000, 0.9659258262890683122, 1.000000000000000000, 0.9659258262890683122, 1.000000000000000000, 0.9659258262890683122, 1.000000000000000000, 0.9659258262890683122, 1.000000000000000000, 0.9659258262890683122, 1.000000000000000000, 0.9659258262890683122, 1.000000000000000000, 0.9659258262890683122, 1.000000000000000000, 0.9659258262890683122, 1.000000000000000000, 0.9659258262890683122, 1.000000000000000000, 0.9659258262890683122, 1.000000000000000000, 0.9659258262890683122, 1.000000000000000000, 0.9659258262890683122, 1.000000000000000000, 0.9659258262890683122, 1.000000000000000000, 0.9659258262890683122, 1.000000000000000000, 0.9659258262890683122, 1.000000000000000000, 0.9659258262890683122, 1.000000000000000000, 0.9659258262890683122, 1.000000000000000000, 0.9659258262890683122, 1.000000000000000000, 0.9659258262890683122, 1.000000000000000000, 0.9659258262890683122, 1.000000000000000000, 0.9659258262890683122, 1.000000000000000000, 0.9659258262890683122, 1.000000000000000000, 0.9659258262890683122, 1.000000000000000000, 0.9659258262890683122, 1.000000000000000000, 0.9659258262890683122, 1.000000000000000000, 0.9659258262890683122, 1.000000000000000000, 0.9659258262890683122, 1.000000000000000000, 0.9659258262890683122, 1.000000000000000000, 0.9659258262890683122, 1.000000000000000000, 0.9659258262890683122, 1.000000000000000000, 0.9659258262890683122, 1.000000000000000000, 0.9659258262890683122, 1.000000000000000000, 0.9659258262890683122, 1.000000000000000000, 0.9659258262890683122, 1.000000000000000000, 0.9659258262890683122, 1.000000000000000000, 0.9659258262890683122, 1.000000000000000000, 0.9659258262890683122, 1.000000000000000000, 0.9659258262890683122, 1.000000000000000000, 0.9659258262890683122, 1.000000000000000000, 0.9659258262890683122, 1.000000000000000000, 0.9659258262890683122, 1.000000000000000000, 0.9659258262890683122, 1.000000000000000000, 0.9659258262890683122, 1.000000000000000000, 0.9659258262890683122, 1.000000000000000000, 0.9659258262890683122, 1.000000000000000000, 0.9659258262890683122, 1.000000000000000000, 0.9659258262890683122, 1.000000000000000000, 0.9659258262890683122, 1.000000000000000000, 0.9659258262890683122, 1.000000000000000000, 0.9659258262890683122, 1.000000000000000000, 0.9659258262890683122, 1.000000000000000000, 0.9659258262890683122, 1.000000000000000000, 0.9659258262890683122, 1.000000000000000000, 0.9659258262890683122, 1.000000000000000000, 0.9659258262890683122, 1.000000000000000000, 0.9659258262890683122, 1.000000000000000000, 0.9659258262890683122, 1.000000000000000000, 0.9659258262890683122, 1.000000000000000000, 0.9659258262890683122, 1.000000000000000000, 0.9659258262890683122, 1.000000000000000000, 0.9659258262890683122, 1.000000000000000000, 0.9659258262890683122, 1.000000000000000000, 0.9659258262890683122, 1.000000000000000000, 0.9659258262890683122, 1.000000000000000000, 0.9659258262890683122, 1.000000000000000000, 0.9659258262890683122, 1.000000000000000000, 0.9659258262890683122, 1.000000000000000000, 0.9659258262890683122, 1.000000000000000000, 0.9659258262890683122, 1.000000000000000000, 0.9659258262890683122, 1.000000000000000000, 0.9659258262890683122, 1.000000000000000000, 0.9659258262890683122, 1.000000000000000000, 0.9659258262890683122, 1.000000000000000000, 0.9659258262890683122, 1.000000000000000000, 0.9659258262890683122, 1.000000000000000000, 0.9659258262890683122, 1.000000000000000000, 0.9659258262890683122, 1.000000000000000000, 0.9659258262890683122, 1.000000000000000000, 0.9659258262890683122, 1.000000000000000000, 0.9659258262890683122, 1.000000000000000000, 0.9659258262890683122, 1.000000000000000000, 0.9659258262890683122, 1.000000000000000000, 0.9659258262890683122, 1.000000000000000000, 0.9659258262890683122, 1.000000000000000000, 0.9659258262890683122, 1.000000000000000000, 0.9659258262890683122, 1.000000000000000000, 0.9659258262890683122, 1.000000000000000000, 0.9659258262890683122, 1.000000000000000000, 0.9659258262890683122, 1.000000000000000000, 0.9659258262890683122, 1.000000000000000000, 0.9659258262890683122, 1.000000000000000000, 0.9659258262890683122, 1.000000000000000000, 0.9659258262890683122, 1.000000000000000000, 0.9659258262890683122, 1.000000000000000000, 0.9659258262890683122, 1.000000000000000000, 0.9659258262890683122, 1.000000000000000000, 0.9659258262890683122, 1.000000000000000000, 0.9659258262890683122, 1.000000000000000000, 0.9659258262890683122, 1.000000000000000000, 0.9659258262890683122, 1.000000000000000000, 0.9659258262890683122, 1.000000000000000000, 0.9659258262890683122, 1.000000000000000000, 0.9659258262890683122, 1.000000000000000000, 0.9659258262890683122, 1.000000000000000000, 0.9659258262890683122, 1.000000000000000000, 0.9659258262890683122, 1.000000000000000000, 0.9659258262890683122, 1.000000000000000000, 0.9659258262890683122, 1.000000000000000000, 0.9659258262890683122, 1.000000000000000000, 0.9659258262890683122, 1.000000000000000000, 0.9659258262890683122, 1.000000000000000000) ) ) 
 REPRESENTATION_ITEM ( '' )  SURFACE ( )  );
#81990 = CARTESIAN_POINT ( 'NONE',  ( 0.5774900079438607392, 43.48035201082151247, 5.440088680355550821 ) ) ;
#81991 = CARTESIAN_POINT ( 'NONE',  ( 7.361572987183170547, 42.05059781766745886, 9.846743663894590881 ) ) ;
#81992 = CARTESIAN_POINT ( 'NONE',  ( -4.164238869374099927, 27.01208216824730357, 3.795296366450308767 ) ) ;
#81993 = ORIENTED_EDGE ( 'NONE', *, *, #17478, .T. ) ;
#81994 = CARTESIAN_POINT ( 'NONE',  ( 9.780380530190813104, 27.00871557427475977, -3.000000000000000000 ) ) ;
#81995 = CARTESIAN_POINT ( 'NONE',  ( 4.559911319644449179, 43.89701867748816966, 9.422509992056141925 ) ) ;
#81996 = CARTESIAN_POINT ( 'NONE',  ( 0.000000000000000000, 0.5000000000000004441, 0.000000000000000000 ) ) ;
#81997 = CARTESIAN_POINT ( 'NONE',  ( 24.16423886937409904, 54.09541550158063217, 3.795296366450317205 ) ) ;
#81998 = CARTESIAN_POINT ( 'NONE',  ( 19.84674366389459266, 63.71726448433412315, -2.638427012816827677 ) ) ;
#81999 = CARTESIAN_POINT ( 'NONE',  ( 0.000000000000000000, 0.5000000000000004441, 0.000000000000000000 ) ) ;
#82000 = CARTESIAN_POINT ( 'NONE',  ( 7.084665262690076126, 57.02201867748817676, -10.88017736071110164 ) ) ;
#82001 = LINE ( 'NONE', #43994, #39031 ) ;
#82002 = CARTESIAN_POINT ( 'NONE',  ( -2.816281873526473856, 4.123634669930420493, 9.499525473075851096E-16 ) ) ;
#82003 = CARTESIAN_POINT ( 'NONE',  ( 4.494156999534569152, 0.000000000000000000, 3.088748530746300958 ) ) ;
#82004 = CARTESIAN_POINT ( 'NONE',  ( 12.91533473730992121, 19.52201867748816611, 10.88017736071110164 ) ) ;
#82005 = CARTESIAN_POINT ( 'NONE',  ( -0.8801773607111008646, 13.27201867748817321, 2.915334737309923430 ) ) ;
#82006 = CARTESIAN_POINT ( 'NONE',  ( 10.00000000000000000, 44.75893115100078745, -9.846743663894594434 ) ) ;
#82007 = CARTESIAN_POINT ( 'NONE',  ( 2.393480905993052854, 15.00000000000000000, 14.80781041047752922 ) ) ;
#82008 = ORIENTED_EDGE ( 'NONE', *, *, #50446, .F. ) ;
#82009 = CIRCLE ( 'NONE', #43682, 15.00000000000000000 ) ;
#82010 = EDGE_CURVE ( 'NONE', #80524, #71988, #61035, .T. ) ;
#82011 = CARTESIAN_POINT ( 'NONE',  ( 20.88017736071110519, 5.563685344154837509, 2.639326808657452039E-16 ) ) ;
#82012 = CARTESIAN_POINT ( 'NONE',  ( 22.81628187352647785, 11.41530133659708390, 3.434112377981063169 ) ) ;
#82013 = CARTESIAN_POINT ( 'NONE',  ( 0.1532563361054083140, 16.00893115100078390, 1.131784320476157264E-15 ) ) ;
#82014 = CARTESIAN_POINT ( 'NONE',  ( 0.1532563361054100626, 40.80059781766745886, -2.638427012816831230 ) ) ;
#82015 = CARTESIAN_POINT ( 'NONE',  ( 10.00000000000000000, 41.81368534415484106, -10.88017736071110342 ) ) ;
#82016 = CARTESIAN_POINT ( 'NONE',  ( 19.38216949554541557, 2.248634669930420049, -9.382169495545420901 ) ) ;
#82018 = CARTESIAN_POINT ( 'NONE',  ( 5.963430220938279902, 10.99545670184114066, -10.32896413005680181 ) ) ;
#82017 = CARTESIAN_POINT ( 'NONE',  ( 19.42250999205614193, 55.14701867748817676, 5.440088680355555262 ) ) ;
#82019 = CYLINDRICAL_SURFACE ( 'NONE', #72057, 15.00000000000000000 ) ;
#82020 = CARTESIAN_POINT ( 'NONE',  ( 0.6178305044545838731, 54.74863466993042493, 9.382169495545420901 ) ) ;
#82021 = VERTEX_POINT ( 'NONE', #83432 ) ;
#82022 = CARTESIAN_POINT ( 'NONE',  ( -0.8801773607111009756, 68.06368534415484817, 1.068504757029289695E-15 ) ) ;
#82024 = CARTESIAN_POINT ( 'NONE',  ( -2.266590686148945544, 6.387082168247300906, -7.082119434687050408 ) ) ;
#82023 = CARTESIAN_POINT ( 'NONE',  ( 19.38216949554541557, 37.24863466993041783, -9.382169495545420901 ) ) ;
#82025 = CARTESIAN_POINT ( 'NONE',  ( 20.32896413005680714, 32.60497603579418069, -5.963430220938276349 ) ) ;
#82026 = CARTESIAN_POINT ( 'NONE',  ( 12.91533473730993009, 36.60535201082151247, -10.88017736071109987 ) ) ;
#82027 = CARTESIAN_POINT ( 'NONE',  ( 7.361572987183170547, 62.05059781766745886, 9.846743663894590881 ) ) ;
#82028 = CARTESIAN_POINT ( 'NONE',  ( 10.00000000000000000, 59.75893115100078745, -9.846743663894594434 ) ) ;
#82029 = CARTESIAN_POINT ( 'NONE',  ( 1.472469842513823179, 20.59226448433411960, -4.923371831947296329 ) ) ;
#82030 = CARTESIAN_POINT ( 'NONE',  ( 15.44008868035555793, 66.39701867748817676, -9.422509992056140149 ) ) ;
#82031 = CARTESIAN_POINT ( 'NONE',  ( -9.997910040112669705, 15.00000000000000000, 10.50199004140708325 ) ) ;
#82032 = CARTESIAN_POINT ( 'NONE',  ( 10.00000000000000000, 25.55374883491396787, -14.16423886937410082 ) ) ;
#82033 = B_SPLINE_CURVE_WITH_KNOTS ( 'NONE', 3,
 ( #27095, #89087, #5607, #81579, #93266, #57598, #40275, #70782, #17776, #95607 ),
 .UNSPECIFIED., .F., .F.,
 ( 4, 3, 3, 4 ),
 ( 7.573910767901059648E-18, 0.0006253016069560931147, 0.001250604074564911532, 0.002501455912506553476 ),
 .UNSPECIFIED. ) ;
#82034 = CARTESIAN_POINT ( 'NONE',  ( 10.95627140743379613, -96.88013104273433385, -3.750000000000000888 ) ) ;
#82035 = CARTESIAN_POINT ( 'NONE',  ( 14.02068044289378967, 0.5000000000000004441, -5.331089937175664595 ) ) ;
#82036 = ORIENTED_EDGE ( 'NONE', *, *, #17361, .F. ) ;
#82037 = CARTESIAN_POINT ( 'NONE',  ( 24.16423886937410614, 59.51208216824728936, -3.795296366450302550 ) ) ;
#82038 = CARTESIAN_POINT ( 'NONE',  ( 20.36894250292379738, 59.92874883491397497, -10.36894250292379027 ) ) ;
#82039 = CARTESIAN_POINT ( 'NONE',  ( 1.472469842513823179, 35.59226448433412315, -4.923371831947296329 ) ) ;
#82040 = CARTESIAN_POINT ( 'NONE',  ( 3.591859063236763294, 28.29030133659708568, -11.09922568453595026 ) ) ;
#82041 = AXIS2_PLACEMENT_3D ( 'NONE', #92732, #54720, #48209 ) ;
#82042 = CARTESIAN_POINT ( 'NONE',  ( 15.44008868035555260, 14.73035201082150536, 9.422509992056143702 ) ) ;
#82043 = CARTESIAN_POINT ( 'NONE',  ( 22.26659068614894466, 58.88708216824729647, 7.082119434687054849 ) ) ;
#82044 = CARTESIAN_POINT ( 'NONE',  ( 14.92337183194729633, 22.67559781766745175, 8.527530157486181039 ) ) ;
#82045 = DIRECTION ( 'NONE',  ( 0.7132504491541897806, 0.000000000000000000, -0.7009092642998425715 ) ) ;
#82046 = CARTESIAN_POINT ( 'NONE',  ( 0.1532563361054100626, 15.80059781766745353, -2.638427012816831230 ) ) ;
#82047 = VECTOR ( 'NONE', #28622, 1000.000000000000000 ) ;
#82048 = DIRECTION ( 'NONE',  ( 0.000000000000000000, 1.000000000000000000, 0.000000000000000000 ) ) ;
#82049 = CARTESIAN_POINT ( 'NONE',  ( -9.846743663894594434, 16.00893115100079100, 3.469446951953614189E-15 ) ) ;
#82050 = ORIENTED_EDGE ( 'NONE', *, *, #54085, .T. ) ;
#82051 = B_SPLINE_CURVE_WITH_KNOTS ( 'NONE', 3,
 ( #6322, #80847, #95860, #12832 ),
 .UNSPECIFIED., .F., .F.,
 ( 4, 4 ),
 ( 0.000000000000000000, 0.001036303429213365724 ),
 .UNSPECIFIED. ) ;
#82052 = ORIENTED_EDGE ( 'NONE', *, *, #72291, .T. ) ;
#82053 = CARTESIAN_POINT ( 'NONE',  ( -6.728851239468925272, 15.00000000000000711, -12.98580270086209865 ) ) ;
#82054 = VERTEX_POINT ( 'NONE', #45419 ) ;
#82055 = CARTESIAN_POINT ( 'NONE',  ( 19.84674366389459621, 43.50893115100078745, 7.409399052514197653E-17 ) ) ;
#82056 = CARTESIAN_POINT ( 'NONE',  ( 6.204703633549690345, 17.84541550158063217, 14.16423886937410082 ) ) ;
#82058 = CARTESIAN_POINT ( 'NONE',  ( 20.88017736071110875, 20.77201867748816611, -2.915334737309920765 ) ) ;
#82057 = CARTESIAN_POINT ( 'NONE',  ( 17.96484262340118221, 21.18868534415483396, -7.964842623401177768 ) ) ;
#82060 = CARTESIAN_POINT ( 'NONE',  ( -1.099225684535947600, 14.54030133659708568, 6.408140936763237150 ) ) ;
#82059 = CARTESIAN_POINT ( 'NONE',  ( 1.472469842513823179, 60.59226448433412315, -4.923371831947296329 ) ) ;
#82061 = CARTESIAN_POINT ( 'NONE',  ( 22.26659068614895176, 4.720415501580633943, -7.082119434687042414 ) ) ;
#82063 = ADVANCED_FACE ( 'NONE', ( #75925 ), #53413, .T. ) ;
#82062 = CARTESIAN_POINT ( 'NONE',  ( 7.084665262690076126, 69.10535201082151957, 10.88017736071109987 ) ) ;
#82064 = B_SPLINE_CURVE_WITH_KNOTS ( 'NONE', 3,
 ( #43551, #96581, #60533, #13557, #83540, #73550 ),
 .UNSPECIFIED., .F., .F.,
 ( 4, 2, 4 ),
 ( 3.409110551443771857E-05, 0.0004400426677362852365, 0.0008459942299581327003 ),
 .UNSPECIFIED. ) ;
#82065 = CARTESIAN_POINT ( 'NONE',  ( 13.43411237798106583, 37.66530133659708923, -12.81628187352647252 ) ) ;
#82066 = ORIENTED_EDGE ( 'NONE', *, *, #78556, .F. ) ;
#82067 = CARTESIAN_POINT ( 'NONE',  ( 18.52753015748617571, 33.09226448433411605, 4.923371831947298993 ) ) ;
#82068 = CARTESIAN_POINT ( 'NONE',  ( 0.5774900079438607392, 8.480352010821505360, 5.440088680355550821 ) ) ;
#82069 = CARTESIAN_POINT ( 'NONE',  ( 7.084665262690076126, 2.022018677488171434, -10.88017736071110164 ) ) ;
#82070 = ORIENTED_EDGE ( 'NONE', *, *, #12569, .F. ) ;
#82071 = CARTESIAN_POINT ( 'NONE',  ( 10.00000000000000000, 41.81368534415484106, -10.88017736071110342 ) ) ;
#82072 = CARTESIAN_POINT ( 'NONE',  ( 7.084665262690076126, 64.10535201082150536, 10.88017736071109987 ) ) ;
#82073 = CARTESIAN_POINT ( 'NONE',  ( 10.00000000000000000, 56.81368534415484106, -10.88017736071110342 ) ) ;
#82074 = PLANE ( 'NONE',  #13649 ) ;
#82075 = CARTESIAN_POINT ( 'NONE',  ( 4.559911319644449179, 48.89701867748817676, 9.422509992056141925 ) ) ;
#82076 = DIRECTION ( 'NONE',  ( 0.000000000000000000, -1.000000000000000000, 0.000000000000000000 ) ) ;
#82078 = ORIENTED_EDGE ( 'NONE', *, *, #63780, .F. ) ;
#82077 = PLANE ( 'NONE',  #88888 ) ;
#82079 = EDGE_CURVE ( 'NONE', #87620, #40639, #24879, .T. ) ;
#82080 = CARTESIAN_POINT ( 'NONE',  ( 0.1532563361054100626, 30.80059781766744820, -2.638427012816831230 ) ) ;
#82081 = ORIENTED_EDGE ( 'NONE', *, *, #21122, .T. ) ;
#82082 = CARTESIAN_POINT ( 'NONE',  ( 12.63842701281683922, 59.55059781766744464, -9.846743663894590881 ) ) ;
#82083 = CARTESIAN_POINT ( 'NONE',  ( 6.880000000000009663, 41.24999999999999289, 6.500000000000000888 ) ) ;
#82084 = EDGE_CURVE ( 'NONE', #15233, #86853, #85027, .T. ) ;
#82085 = CARTESIAN_POINT ( 'NONE',  ( -2.266590686148945544, 12.22041550158063394, 7.082119434687048631 ) ) ;
#82086 = ORIENTED_EDGE ( 'NONE', *, *, #30643, .F. ) ;
#82087 = CARTESIAN_POINT ( 'NONE',  ( -11.50383178867919298, 12.89949214739216465, 1.921679737233346730 ) ) ;
#82088 = CARTESIAN_POINT ( 'NONE',  ( -7.124967611315338623, -78.82395889337750816, 3.750000000000000888 ) ) ;
#82089 = CARTESIAN_POINT ( 'NONE',  ( 0.000000000000000000, 0.5000000000000004441, 0.000000000000000000 ) ) ;
#82090 = CARTESIAN_POINT ( 'NONE',  ( 7.084665262690076126, 4.105352010821503583, 10.88017736071109987 ) ) ;
#82091 = FACE_OUTER_BOUND ( 'NONE', #53751, .T. ) ;
#82092 = EDGE_LOOP ( 'NONE', ( #57492, #45280, #67302, #70770, #80179, #54320, #83064, #75075, #39324, #2845 ) ) ;
#82093 = CARTESIAN_POINT ( 'NONE',  ( 9.322910753577957621, 14.95077488074852390, -11.43369735623877226 ) ) ;
#82094 = CARTESIAN_POINT ( 'NONE',  ( 1.472469842513823179, 40.59226448433411605, -4.923371831947296329 ) ) ;
#82095 = CARTESIAN_POINT ( 'NONE',  ( 8.880000000000000782, 1.019547802438459216, -3.750000000000001776 ) ) ;
#82096 = CARTESIAN_POINT ( 'NONE',  ( -2.816281873526473856, 14.12363466993041961, 9.499525473075851096E-16 ) ) ;
#82097 = CARTESIAN_POINT ( 'NONE',  ( 18.52753015748617571, 8.092264484334117824, 4.923371831947298993 ) ) ;
#82098 = CYLINDRICAL_SURFACE ( 'NONE', #60138, 0.2500000000000002220 ) ;
#82099 = CARTESIAN_POINT ( 'NONE',  ( 22.81628187352647785, 1.415301336597087012, 3.434112377981063169 ) ) ;
#82100 = FACE_OUTER_BOUND ( 'NONE', #71587, .T. ) ;
#82101 = VECTOR ( 'NONE', #12670, 1000.000000000000000 ) ;
#82102 = VERTEX_POINT ( 'NONE', #92401 ) ;
#82103 = CARTESIAN_POINT ( 'NONE',  ( 2.035157376598824452, 13.68868534415483751, 7.964842623401179544 ) ) ;
#82104 =( NAMED_UNIT ( * ) SI_UNIT ( $, .STERADIAN. ) SOLID_ANGLE_UNIT ( ) );
#82105 = CARTESIAN_POINT ( 'NONE',  ( 12.63842701281683034, 32.46726448433412315, 9.846743663894596210 ) ) ;
#82106 = CARTESIAN_POINT ( 'NONE',  ( 19.42250999205614548, 50.98035201082151247, -5.440088680355545492 ) ) ;
#82108 =( NAMED_UNIT ( * ) SI_UNIT ( $, .STERADIAN. ) SOLID_ANGLE_UNIT ( ) );
#82107 = CARTESIAN_POINT ( 'NONE',  ( -2.816281873526471635, 43.91530133659708923, -3.434112377981056508 ) ) ;
#82109 = CARTESIAN_POINT ( 'NONE',  ( 17.96484262340118221, 11.18868534415483929, -7.964842623401177768 ) ) ;
#82110 = VECTOR ( 'NONE', #83979, 1000.000000000000000 ) ;
#82111 = CARTESIAN_POINT ( 'NONE',  ( -0.3289641300568009741, 57.24545670184114954, -5.963430220938281678 ) ) ;
#82112 = DIRECTION ( 'NONE',  ( -1.000000000000000000, 0.000000000000000000, 0.000000000000000000 ) ) ;
#82113 = CARTESIAN_POINT ( 'NONE',  ( 2.791683348922240793, 61.63393115100079456, 7.208316651077764092 ) ) ;
#82114 = CARTESIAN_POINT ( 'NONE',  ( 10.00000000000000000, 24.75893115100078745, -9.846743663894594434 ) ) ;
#82115 = CARTESIAN_POINT ( 'NONE',  ( -2.915334737309934532, -7.977981322511819684, -10.88017736071109987 ) ) ;
#82116 = CARTESIAN_POINT ( 'NONE',  ( 13.43411237798105340, 40.58196800326375353, 12.81628187352647963 ) ) ;
#82117 = CARTESIAN_POINT ( 'NONE',  ( 18.50749283717776805, 24.69955587570481725, 6.499999999999999112 ) ) ;
#82119 = CARTESIAN_POINT ( 'NONE',  ( 11.35178980618968048, 14.63595249122790598, 9.804941009312001299 ) ) ;
#82118 = CARTESIAN_POINT ( 'NONE',  ( 7.084665262690076126, 42.02201867748816966, -10.88017736071110164 ) ) ;
#82120 = ADVANCED_FACE ( 'NONE', ( #23924 ), #11574, .F. ) ;
#82121 = DIRECTION ( 'NONE',  ( -1.000000000000000000, 0.000000000000000000, -0.000000000000000000 ) ) ;
#82122 = CARTESIAN_POINT ( 'NONE',  ( 0.5774900079438590739, 27.64701867748817676, -5.440088680355550821 ) ) ;
#82123 = CARTESIAN_POINT ( 'NONE',  ( 15.44008868035555793, 36.39701867748816966, -9.422509992056140149 ) ) ;
#82124 = CARTESIAN_POINT ( 'NONE',  ( 17.20831665107776587, 54.13393115100079456, -7.208316651077762316 ) ) ;
#82125 = CARTESIAN_POINT ( 'NONE',  ( 10.00000000000000178, 59.31368534415484106, 10.88017736071110342 ) ) ;
#82126 = CARTESIAN_POINT ( 'NONE',  ( 10.00000000000000178, 38.05374883491396787, 14.16423886937410082 ) ) ;
#82127 = UNCERTAINTY_MEASURE_WITH_UNIT (LENGTH_MEASURE( 1.000000000000000082E-05 ), #2504, 'distance_accuracy_value', 'NONE');
#82128 = CARTESIAN_POINT ( 'NONE',  ( 10.00000000000000000, 34.75893115100078745, -9.846743663894594434 ) ) ;
#82129 = CARTESIAN_POINT ( 'NONE',  ( 3.591859063236761518, 59.95696800326375353, 11.09922568453594849 ) ) ;
#82130 = CARTESIAN_POINT ( 'NONE',  ( 0.6178305044545838731, -0.2513653300695798953, 9.382169495545420901 ) ) ;
#82131 = EDGE_LOOP ( 'NONE', ( #73455, #41303, #80395, #59304 ) ) ;
#82132 = CARTESIAN_POINT ( 'NONE',  ( 2.035157376598824452, 23.68868534415484461, 7.964842623401179544 ) ) ;
#82133 = EDGE_CURVE ( 'NONE', #66548, #31259, #79859, .T. ) ;
#82134 = CARTESIAN_POINT ( 'NONE',  ( 17.96484262340118221, 9.938685344154839285, 7.964842623401181321 ) ) ;
#82135 = CARTESIAN_POINT ( 'NONE',  ( 10.00000000000000178, 64.31368534415483396, 10.88017736071110342 ) ) ;
#82136 = CARTESIAN_POINT ( 'NONE',  ( 22.26659068614895176, 19.72041550158063572, -7.082119434687042414 ) ) ;
#82137 = CARTESIAN_POINT ( 'NONE',  ( 18.52753015748617571, 8.092264484334117824, 4.923371831947298993 ) ) ;
#82138 = CARTESIAN_POINT ( 'NONE',  ( 10.00000000000000000, 64.75893115100078035, -9.846743663894594434 ) ) ;
#82139 = CARTESIAN_POINT ( 'NONE',  ( 17.96484262340118221, 49.93868534415484106, 7.964842623401181321 ) ) ;
#82140 = DIRECTION ( 'NONE',  ( -0.000000000000000000, -1.000000000000000000, -0.000000000000000000 ) ) ;
#82141 = CARTESIAN_POINT ( 'NONE',  ( 18.00000000000000355, 77.07179676972445748, 6.250000000000000000 ) ) ;
#82142 = AXIS2_PLACEMENT_3D ( 'NONE', #57307, #34295, #18834 ) ;
#82143 = ORIENTED_EDGE ( 'NONE', *, *, #34635, .F. ) ;
#82144 = CARTESIAN_POINT ( 'NONE',  ( 0.000000000000000000, 15.00000000000000000, 0.000000000000000000 ) ) ;
#82145 = CARTESIAN_POINT ( 'NONE',  ( 17.20831665107776587, 44.13393115100078745, -7.208316651077762316 ) ) ;
#82146 = ORIENTED_EDGE ( 'NONE', *, *, #81565, .T. ) ;
#82147 = EDGE_LOOP ( 'NONE', ( #68946, #43871, #6083, #30030 ) ) ;
#82148 =( NAMED_UNIT ( * ) SI_UNIT ( $, .STERADIAN. ) SOLID_ANGLE_UNIT ( ) );
#82149 = CARTESIAN_POINT ( 'NONE',  ( 24.16423886937410614, 19.51208216824729647, -3.795296366450302550 ) ) ;
#82150 = CARTESIAN_POINT ( 'NONE',  ( 24.16423886937410614, 29.30374883491396787, 8.672049930838204340E-16 ) ) ;
#82151 = CARTESIAN_POINT ( 'NONE',  ( -0.8801773607111009756, 58.06368534415484106, 1.068504757029289695E-15 ) ) ;
#82152 = CARTESIAN_POINT ( 'NONE',  ( 10.00000000000000178, 63.05374883491396076, 14.16423886937410082 ) ) ;
#82153 = CARTESIAN_POINT ( 'NONE',  ( 16.40814093676324603, 2.456968003263753531, -11.09922568453594671 ) ) ;
#82154 = CARTESIAN_POINT ( 'NONE',  ( 10.00000000000000000, 49.75893115100078745, -9.846743663894594434 ) ) ;
#82155 = CARTESIAN_POINT ( 'NONE',  ( -11.07542066904767175, -96.02453755659226431, 4.000000000000452971 ) ) ;
#82157 = CARTESIAN_POINT ( 'NONE',  ( 13.43411237798105340, 0.5819680032637533085, 12.81628187352647963 ) ) ;
#82156 = CARTESIAN_POINT ( 'NONE',  ( 20.88017736071110875, 40.77201867748818387, -2.915334737309920765 ) ) ;
#82158 = CARTESIAN_POINT ( 'NONE',  ( -4.164238869374098151, 16.59541550158063927, -3.795296366450310543 ) ) ;
#82159 = CARTESIAN_POINT ( 'NONE',  ( -4.164238869374099039, 51.80374883491396787, 8.674139862899312516E-16 ) ) ;
#82160 = CARTESIAN_POINT ( 'NONE',  ( 4.559911319644449179, 12.23035201082150714, -9.422509992056141925 ) ) ;
#82161 = CARTESIAN_POINT ( 'NONE',  ( -0.1503990784575329198, 2.222660991849184864, -6.262539305110070842 ) ) ;
#82162 = CARTESIAN_POINT ( 'NONE',  ( 15.44008868035555260, 39.73035201082150536, 9.422509992056143702 ) ) ;
#82163 = CARTESIAN_POINT ( 'NONE',  ( 3.469446951953614189E-15, -22.74106884899921255, 9.846743663894594434 ) ) ;
#82164 = ORIENTED_EDGE ( 'NONE', *, *, #14633, .F. ) ;
#82165 = CARTESIAN_POINT ( 'NONE',  ( -38.69000000000001194, 93.50000000000000000, -10.09898361729590199 ) ) ;
#82166 = ORIENTED_EDGE ( 'NONE', *, *, #20593, .T. ) ;
#82167 = CARTESIAN_POINT ( 'NONE',  ( 2.791683348922237240, 30.38393115100078390, -7.208316651077763204 ) ) ;
#82168 = ORIENTED_EDGE ( 'NONE', *, *, #15190, .T. ) ;
#82169 = CARTESIAN_POINT ( 'NONE',  ( -4.164238869374098151, 46.59541550158063927, -3.795296366450310543 ) ) ;
#82171 = CARTESIAN_POINT ( 'NONE',  ( 7.361572987183170547, 47.05059781766745175, 9.846743663894590881 ) ) ;
#82170 = CARTESIAN_POINT ( 'NONE',  ( 12.63842701281683922, 19.55059781766745175, -9.846743663894590881 ) ) ;
#82172 = CARTESIAN_POINT ( 'NONE',  ( 20.88017736071110519, 65.56368534415483396, 2.639326808657452039E-16 ) ) ;
#82173 = LINE ( 'NONE', #5703, #94120 ) ;
#82174 = ADVANCED_FACE ( 'NONE', ( #26360 ), #30689, .T. ) ;
#82175 = CARTESIAN_POINT ( 'NONE',  ( -0.8801773607111009756, 68.06368534415484817, 1.068504757029289695E-15 ) ) ;
#82176 =( GEOMETRIC_REPRESENTATION_CONTEXT ( 3 ) GLOBAL_UNCERTAINTY_ASSIGNED_CONTEXT ( ( #68463 ) ) GLOBAL_UNIT_ASSIGNED_CONTEXT ( ( #92308, #38827, #44821 ) ) REPRESENTATION_CONTEXT ( 'NONE', 'WORKASPACE' ) );
#82177 = ADVANCED_FACE ( 'NONE', ( #47877 ), #63853, .T. ) ;
#82179 = CARTESIAN_POINT ( 'NONE',  ( 22.81628187352647785, 56.41530133659708213, 3.434112377981063169 ) ) ;
#82178 = VECTOR ( 'NONE', #70450, 1000.000000000000000 ) ;
#82180 = CARTESIAN_POINT ( 'NONE',  ( -12.81628187352647963, 13.91530133659708746, -3.434112377981046293 ) ) ;
#82181 = ORIENTED_EDGE ( 'NONE', *, *, #87706, .T. ) ;
#82182 = CARTESIAN_POINT ( 'NONE',  ( 22.26659068614895176, 34.72041550158063927, -7.082119434687042414 ) ) ;
#82183 = AXIS2_PLACEMENT_3D ( 'NONE', #31336, #84847, #399 ) ;
#82184 = CARTESIAN_POINT ( 'NONE',  ( 13.43411237798105340, 25.58196800326374998, 12.81628187352647963 ) ) ;
#82185 = EDGE_LOOP ( 'NONE', ( #39013, #97243, #58917, #25857, #48071, #90801, #80108, #8581 ) ) ;
#82186 = CARTESIAN_POINT ( 'NONE',  ( 0.6178305044545818747, 43.49863466993042493, -9.382169495545419124 ) ) ;
#82187 = CARTESIAN_POINT ( 'NONE',  ( 2.035157376598822676, 17.43868534415483751, -7.964842623401177768 ) ) ;
#82188 = CARTESIAN_POINT ( 'NONE',  ( 2.791683348922237240, 30.38393115100078390, -7.208316651077763204 ) ) ;
#82189 = CARTESIAN_POINT ( 'NONE',  ( -0.8801773607111009756, 8.063685344154837509, 1.068504757029289695E-15 ) ) ;
#82190 =( GEOMETRIC_REPRESENTATION_CONTEXT ( 3 ) GLOBAL_UNCERTAINTY_ASSIGNED_CONTEXT ( ( #67393 ) ) GLOBAL_UNIT_ASSIGNED_CONTEXT ( ( #19755, #64743, #26761 ) ) REPRESENTATION_CONTEXT ( 'NONE', 'WORKASPACE' ) );
#82191 = DIRECTION ( 'NONE',  ( -0.02617694830786282401, 0.000000000000000000, -0.9996573249755575929 ) ) ;
#82192 = ADVANCED_FACE ( 'NONE', ( #71393 ), #78381, .T. ) ;
#82193 = CARTESIAN_POINT ( 'NONE',  ( 17.20831665107776587, 39.13393115100079456, -7.208316651077762316 ) ) ;
#82194 = CARTESIAN_POINT ( 'NONE',  ( 14.92337183194729988, 49.34226448433411605, -8.527530157486177487 ) ) ;
#82196 = ORIENTED_EDGE ( 'NONE', *, *, #41262, .T. ) ;
#82195 = CARTESIAN_POINT ( 'NONE',  ( 20.24186590665278018, 22.61633188102327097, -6.114288769123028544 ) ) ;
#82197 = CIRCLE ( 'NONE', #34288, 15.00000000000000000 ) ;
#82198 = CARTESIAN_POINT ( 'NONE',  ( -0.2851878892742317761, 0.2306287049188357752, -14.93850447011040750 ) ) ;
#82199 = CARTESIAN_POINT ( 'NONE',  ( -3.750000000000000000, 10.25000000000000000, 3.750000000000000000 ) ) ;
#82200 = CARTESIAN_POINT ( 'NONE',  ( 0.9408516040111464251, 27.46693863883976405, -6.499999999999936051 ) ) ;
#82201 = CARTESIAN_POINT ( 'NONE',  ( 19.59355889808634288, 82.60103572628047175, 5.130931023488903620 ) ) ;
#82202 = CARTESIAN_POINT ( 'NONE',  ( 12.63842701281683034, 12.46726448433411782, 9.846743663894596210 ) ) ;
#82203 = CARTESIAN_POINT ( 'NONE',  ( 13.43411237798106583, 42.66530133659707502, -12.81628187352647252 ) ) ;
#82204 = EDGE_CURVE ( 'NONE', #30184, #44141, #80228, .T. ) ;
#82205 = DIRECTION ( 'NONE',  ( 0.000000000000000000, 0.000000000000000000, 1.000000000000000000 ) ) ;
#82206 = ORIENTED_EDGE ( 'NONE', *, *, #4098, .T. ) ;
#82207 = CARTESIAN_POINT ( 'NONE',  ( 0.1532563361054083140, 61.00893115100078745, 1.131784320476157264E-15 ) ) ;
#82208 = CARTESIAN_POINT ( 'NONE',  ( 10.19513985507825637, 15.00000000000000000, 11.00268709613223983 ) ) ;
#82209 = CARTESIAN_POINT ( 'NONE',  ( 22.26659068614894466, 18.88708216824730002, 7.082119434687054849 ) ) ;
#82210 = CARTESIAN_POINT ( 'NONE',  ( 12.63842701281683034, 52.46726448433413026, 9.846743663894596210 ) ) ;
#82211 = CARTESIAN_POINT ( 'NONE',  ( 6.565887622018943937, 45.16530133659708923, 12.81628187352647430 ) ) ;
#82212 = DIRECTION ( 'NONE',  ( 0.09584575252023383451, 0.000000000000000000, -0.9953961983671778535 ) ) ;
#82213 = CARTESIAN_POINT ( 'NONE',  ( 2.791683348922240793, 11.63393115100078568, 7.208316651077764092 ) ) ;
#82214 = DIRECTION ( 'NONE',  ( -0.8073289077885722476, 0.5901017155109032908, -1.999617224239539632E-13 ) ) ;
#82215 = CIRCLE ( 'NONE', #72578, 1.750000000000000666 ) ;
#82216 = CARTESIAN_POINT ( 'NONE',  ( 5.076628168052703671, 41.84226448433411605, 8.527530157486179263 ) ) ;
#82217 = CARTESIAN_POINT ( 'NONE',  ( 20.88017736071110164, 45.35535201082149115, 2.915334737309930979 ) ) ;
#82218 = CARTESIAN_POINT ( 'NONE',  ( 17.20831665107776587, 29.13393115100078390, -7.208316651077762316 ) ) ;
#82219 = CARTESIAN_POINT ( 'NONE',  ( -227.5967939629026091, -115.9521848121535896, -20.80263291704672568 ) ) ;
#82220 = CARTESIAN_POINT ( 'NONE',  ( 3.558677480090427725, 70.40124509038875544, -5.000000000000000000 ) ) ;
#82221 = CARTESIAN_POINT ( 'NONE',  ( 20.88017736071110164, 45.35535201082149115, 2.915334737309930979 ) ) ;
#82222 = ORIENTED_EDGE ( 'NONE', *, *, #86270, .T. ) ;
#82223 = CARTESIAN_POINT ( 'NONE',  ( -0.8801773607111009756, 68.06368534415484817, 1.068504757029289695E-15 ) ) ;
#82224 = CARTESIAN_POINT ( 'NONE',  ( 10.00000000000000178, 14.31368534415483751, 10.88017736071110342 ) ) ;
#82226 = CARTESIAN_POINT ( 'NONE',  ( -0.8801773607111009756, 48.06368534415484817, 1.068504757029289695E-15 ) ) ;
#82225 = CARTESIAN_POINT ( 'NONE',  ( 2.791683348922237240, 60.38393115100078745, -7.208316651077763204 ) ) ;
#82227 = DIRECTION ( 'NONE',  ( -0.4305110968082986878, 0.000000000000000000, 0.9025852843498588518 ) ) ;
#82228 = CARTESIAN_POINT ( 'NONE',  ( 17.96484262340118221, 59.93868534415484106, 7.964842623401181321 ) ) ;
#82230 = CARTESIAN_POINT ( 'NONE',  ( 20.00000000000000355, 82.59735310507680595, -4.636598376030807600 ) ) ;
#82229 = CARTESIAN_POINT ( 'NONE',  ( 19.42250999205614193, 25.14701867748817321, 5.440088680355555262 ) ) ;
#82231 = CARTESIAN_POINT ( 'NONE',  ( 2.791683348922240793, 1.633931151000784565, 7.208316651077764092 ) ) ;
#82232 = CARTESIAN_POINT ( 'NONE',  ( 10.00000000000000178, 22.25893115100078745, 9.846743663894594434 ) ) ;
#82233 = DIRECTION ( 'NONE',  ( 0.000000000000000000, 1.000000000000000000, 0.000000000000000000 ) ) ;
#82234 = CARTESIAN_POINT ( 'NONE',  ( 3.795296366450314540, 8.262082168247296465, 14.16423886937410082 ) ) ;
#82235 = CARTESIAN_POINT ( 'NONE',  ( 2.791683348922240793, 66.63393115100079456, 7.208316651077764092 ) ) ;
#82236 = CARTESIAN_POINT ( 'NONE',  ( 20.88017736071110164, 5.355352010821503583, 2.915334737309930979 ) ) ;
#82237 = FACE_OUTER_BOUND ( 'NONE', #78234, .T. ) ;
#82238 = CARTESIAN_POINT ( 'NONE',  ( -4.164238869374099039, 11.80374883491396965, 8.674139862899312516E-16 ) ) ;
#82239 = ADVANCED_FACE ( 'NONE', ( #25405 ), #45109, .T. ) ;
#82240 = CARTESIAN_POINT ( 'NONE',  ( -0.3689425029237898834, 56.17874883491396076, -10.36894250292378850 ) ) ;
#82241 = CARTESIAN_POINT ( 'NONE',  ( 21.09922568453594849, 1.206968003263753531, 6.408140936763242479 ) ) ;
#82242 = ORIENTED_EDGE ( 'NONE', *, *, #40332, .T. ) ;
#82243 = CARTESIAN_POINT ( 'NONE',  ( 15.44008868035555260, 9.730352010821505360, 9.422509992056143702 ) ) ;
#82244 = CARTESIAN_POINT ( 'NONE',  ( 10.00000000000000178, 42.25893115100078745, 9.846743663894594434 ) ) ;
#82245 = DIRECTION ( 'NONE',  ( 0.000000000000000000, 0.000000000000000000, 1.000000000000000000 ) ) ;
#82246 = PRESENTATION_LAYER_ASSIGNMENT (  '', '', ( #32719 ) ) ;
#82247 = CARTESIAN_POINT ( 'NONE',  ( 1.472469842513823179, 1.425597817667451528, 4.923371831947296329 ) ) ;
#82248 = CARTESIAN_POINT ( 'NONE',  ( 0.6178305044545838731, 24.74863466993042493, 9.382169495545420901 ) ) ;
#82249 = CARTESIAN_POINT ( 'NONE',  ( 10.00000000000000178, 32.25893115100078745, 9.846743663894594434 ) ) ;
#82250 = ORIENTED_EDGE ( 'NONE', *, *, #93444, .F. ) ;
#82251 = CARTESIAN_POINT ( 'NONE',  ( 0.1532563361054083140, 11.00893115100078568, 1.131784320476157264E-15 ) ) ;
#82252 = CARTESIAN_POINT ( 'NONE',  ( 11.04808542137200966, -95.57857389789997171, -4.000000000000000000 ) ) ;
#82253 = CARTESIAN_POINT ( 'NONE',  ( 20.03743638938529159, 16.75197528031016603, 6.399506433553905360 ) ) ;
#82254 = CARTESIAN_POINT ( 'NONE',  ( 19.42250999205614193, 15.14701867748817143, 5.440088680355555262 ) ) ;
#82255 = CARTESIAN_POINT ( 'NONE',  ( 20.36894250292379738, 39.92874883491396787, -10.36894250292379027 ) ) ;
#82256 = CARTESIAN_POINT ( 'NONE',  ( 0.5774900079438607392, 58.48035201082151247, 5.440088680355550821 ) ) ;
#82257 = CARTESIAN_POINT ( 'NONE',  ( 18.52753015748618282, 18.92559781766745175, -4.923371831947291888 ) ) ;
#82258 = CARTESIAN_POINT ( 'NONE',  ( 20.10384461210890450, 21.74302437010793199, 6.337995344473785764 ) ) ;
#82259 = CARTESIAN_POINT ( 'NONE',  ( 0.1532563361054083140, 6.008931151000784787, 1.131784320476157264E-15 ) ) ;
#82260 =( BOUNDED_SURFACE ( )  B_SPLINE_SURFACE ( 1, 2, ( 
 ( #45329, #75826, #77295, #91820, #53822, #84333, #22843, #8808, #76806, #7348, #69319, #62289, #75329, #92793, #69816, #24323, #82831, #14351, #6841, #37355, #90823, #37849, #68340, #98861, #30315, #60815, #91316, #23391, #9349, #70358, #91872, #8857, #15399, #1877, #2367, #85349, #39855, #45886, #16862, #30865, #46850, #31351, #16370, #61363, #8371, #85849, #53876, #84386, #93338, #32333, #61853, #77345, #15885, #32824, #39372, #47336, #93830, #69866, #76375, #54837, #892, #9853, #63322, #31842, #46369, #62838, #76859, #38879, #69371, #24860, #1388, #77839, #7890, #62338, #92358, #53368, #55342, #17362, #38383, #92846, #47831, #78332, #24373, #83877, #40353, #68883, #70854, #23885, #413, #54349, #84863, #42309, #63807, #27288, #87308, #49308, #72784, #86337, #35284, #94810, #3829, #18827, #41352, #73288, #79809, #4318, #19794, #17842, #4811, #79323, #56336, #34792, #65281, #41832, #55844, #71822, #3329, #57788, #50284, #25839, #72299, #26311, #48324, #64298, #40841, #95301, #86829, #34285, #71341, #2860, #56812, #26805, #95810, #88294, #59268, #7277, #98296, #58271, #67278, #73778, #44266, #82263, #28773, #89769, #66273, #52269, #14288, #35784, #51779, #88790, #44761, #45262, #29267, #82765, #20297, #59762, #5308, #21285, #74262, #13780, #96809, #51283, #29753, #28285, #58778, #37287, #75264, #5793, #74771, #89284, #75756, #6281, #90256, #37779, #36785, #50796, #97805, #43772, #52757, #96310, #21790, #20794, #6777, #81769, #13282, #36282, #67776, #60261, #90756, #81286, #22284, #66780, #27785, #83265, #14789, #12784, #43283, #97300, #31722, #46731, #49077, #41101, #11080, #86591, #61246, #71597, #39253, #77229, #18100, #7774, #3109, #31228, #92240, #62221, #30244, #79579, #38755, #8734, #61725, #53748, #56585, #23766, #48577, #64059, #60747, #18584, #23272, #292, #79076, #10589, #54231, #87075, #15766, #84265, #33563, #94571, #68761, #84745, #69256, #68276, #98796, #38269, #26090, #53254, #91751, #30738, #46254, #91248, #16248, #69743, #777, #1269, #22775, #83759, #92726, #15282, #76739, #8254, #24250, #45764, #56098, #76257, #95055, #11566, #42084, #97068, #26564, #80563, #59034, #58536, #49550, #19072, #4577, #65540, #89044, #80062, #96063, #35039, #73535, #27053, #72547, #43536, #35546, #74030, #89539, #21049, #73042, #28041, #51540, #81533, #4080, #20049, #34543, #57061, #87562, #65038, #20555, #95564, #27546, #50551, #81046, #13040, #57551, #12057, #88050, #66540, #19563, #42558, #50059, #58040, #82030, #88548, #12553, #43056, #5561, #5061, #66037, #96566, #51040, #36037, #72068, #28541, #41600, #3593, #34052 ),
 ( #64548, #75518, #75024, #91997, #7033, #45512, #54000, #37539, #6048, #15040, #60015, #69016, #61491, #91005, #82528, #23031, #37038, #14044, #44525, #68523, #68029, #76012, #74527, #22536, #90510, #23528, #15536, #7541, #97558, #98556, #38032, #54, #53007, #13540, #84013, #44024, #30501, #6529, #46019, #83522, #61003, #91514, #52035, #76507, #30007, #53503, #8021, #67536, #60513, #36547, #38518, #67036, #547, #30993, #29019, #59529, #90023, #21544, #22045, #98051, #29508, #52520, #83027, #14543, #45013, #25493, #2510, #92976, #47479, #46984, #63939, #77979, #17499, #25967, #9485, #76995, #85987, #31968, #40981, #33444, #62971, #54481, #93969, #8989, #84992, #16507, #40490, #39988, #47964, #46495, #93476, #62470, #94451, #86481, #78473, #69504, #70491, #9988, #70988, #25002, #84508, #55980, #16006, #32962, #77478, #17979, #55487, #63467, #48463, #24011, #78960, #2011, #32476, #10472, #8507, #39010, #54969, #71478, #2994, #69996, #1020, #31480, #61984, #92483, #39506, #1522, #24507, #85491, #17000, #79460, #18466, #10958, #86953, #48951, #56467, #29330, #73850, #13353, #20863, #14354, #35361, #12854, #6342, #88861, #35854, #5380, #66343, #59828, #43838, #28835, #51355, #81839, #90321, #59337, #96881, #5859, #52339, #96382, #65854, #74334, #67344, #36352, #66847, #27853, #21859, #20370, #51847, #28358, #89840, #97367, #21356, #82336, #58847, #13856, #89353, #44336, #58341, #74841, #36853, #97870, #82834, #50864, #81356, #57371, #2932, #41906, #93903, #87866, #11879, #57859, #94388, #41423, #19864, #65357, #25904, #34367, #87382, #71415, #71884, #80869, #42873, #10901, #3403, #34864, #95886, #56406, #72860, #55913, #86412, #33379, #42383, #33866, #12367, #88370, #64373, #94881, #56880, #72368, #4395, #19383, #26381, #79879, #73356, #18901, #4883, #3898, #49378, #11385, #80379, #86891, #64857, #95377, #26878, #27366, #49866, #48884, #63875, #63397, #50360, #25429, #17913, #48397, #78899, #10409, #40915, #18402, #79394, #5452, #59408, #14430, #36429, #66921, #13426, #67918, #36926, #97442, #66422, #20938, #51427, #29896, #35925, #28906, #60399, #21931, #58925, #28427, #89914, #51925, #52412, #89425, #82409, #21428, #97944, #74409, #81916, #75402, #29402, #6920, #90896, #22424, #13935, #90394, #43425, #44899, #5937, #6414, #44412, #96955, #74915, #67417, #82912, #59904, #37429, #73926, #11951, #42944, #26450, #11457, #87453, #96454, #3481, #73426, #88933, #20443, #3967, #57931, #50932, #12436, #33938, #49948, #64442, #25977, #18474, #94949, #88440, #56473, #34435, #80453, #42455, #4950, #56951, #41975, #18968, #27926, #49446 ) ),
 .UNSPECIFIED., .F., .F., .F. ) 
 B_SPLINE_SURFACE_WITH_KNOTS ( ( 2, 2 ),
 ( 3, 2, 2, 2, 2, 2, 2, 2, 2, 2, 2, 2, 2, 2, 2, 2, 2, 2, 2, 2, 2, 2, 2, 2, 2, 2, 2, 2, 2, 2, 2, 2, 2, 2, 2, 2, 2, 2, 2, 2, 2, 2, 2, 2, 2, 2, 2, 2, 2, 2, 2, 2, 2, 2, 2, 2, 2, 2, 2, 2, 2, 2, 2, 2, 2, 2, 2, 2, 2, 2, 2, 2, 2, 2, 2, 2, 2, 2, 2, 2, 2, 2, 2, 2, 2, 2, 2, 2, 2, 2, 2, 2, 2, 2, 2, 2, 2, 2, 2, 2, 2, 2, 2, 2, 2, 2, 2, 2, 2, 2, 2, 2, 2, 2, 2, 2, 2, 2, 2, 2, 2, 2, 2, 2, 2, 2, 2, 2, 2, 2, 2, 2, 2, 2, 2, 2, 2, 2, 2, 2, 2, 2, 2, 2, 2, 2, 2, 2, 2, 2, 2, 2, 2, 2, 2, 2, 2, 2, 2, 2, 2, 2, 3 ),
 ( 0.000000000000000000, 1.000000000000000000 ),
 ( 0.000000000000000000, 0.005952380952380952051, 0.01190476190476190410, 0.01785714285714285615, 0.02380952380952380820, 0.02976190476190476025, 0.03571428571428571230, 0.04166666666666666435, 0.04761904761904761640, 0.05357142857142856845, 0.05952380952380952051, 0.06547619047619047949, 0.07142857142857142461, 0.07738095238095238360, 0.08333333333333332871, 0.08928571428571428770, 0.09523809523809523281, 0.1011904761904761918, 0.1071428571428571369, 0.1130952380952380959, 0.1190476190476190410, 0.1250000000000000000, 0.1309523809523809590, 0.1369047619047619180, 0.1428571428571428492, 0.1488095238095238082, 0.1547619047619047672, 0.1607142857142857262, 0.1666666666666666574, 0.1726190476190476164, 0.1785714285714285754, 0.1845238095238095344, 0.1904761904761904656, 0.1964285714285714246, 0.2023809523809523836, 0.2083333333333333426, 0.2142857142857142738, 0.2202380952380952328, 0.2261904761904761918, 0.2321428571428571508, 0.2380952380952380820, 0.2440476190476190410, 0.2500000000000000000, 0.2559523809523809312, 0.2619047619047619180, 0.2678571428571428492, 0.2738095238095238360, 0.2797619047619047672, 0.2857142857142856984, 0.2916666666666666852, 0.2976190476190476164, 0.3035714285714285476, 0.3095238095238095344, 0.3154761904761904656, 0.3214285714285714524, 0.3273809523809523836, 0.3333333333333333148, 0.3392857142857143016, 0.3452380952380952328, 0.3511904761904761640, 0.3571428571428571508, 0.3630952380952380820, 0.3690476190476190688, 0.3750000000000000000, 0.3809523809523809312, 0.3869047619047619180, 0.3928571428571428492, 0.3988095238095238360, 0.4047619047619047672, 0.4107142857142856984, 0.4166666666666666852, 0.4226190476190476164, 0.4285714285714285476, 0.4345238095238095344, 0.4404761904761904656, 0.4464285714285714524, 0.4523809523809523836, 0.4583333333333333148, 0.4642857142857143016, 0.4702380952380952328, 0.4761904761904761640, 0.4821428571428571508, 0.4880952380952380820, 0.4940476190476190688, 0.5000000000000000000, 0.5059523809523809312, 0.5119047619047618625, 0.5178571428571429047, 0.5238095238095238360, 0.5297619047619047672, 0.5357142857142856984, 0.5416666666666666297, 0.5476190476190476719, 0.5535714285714286031, 0.5595238095238095344, 0.5654761904761904656, 0.5714285714285713969, 0.5773809523809523281, 0.5833333333333333703, 0.5892857142857143016, 0.5952380952380952328, 0.6011904761904761640, 0.6071428571428570953, 0.6130952380952381375, 0.6190476190476190688, 0.6250000000000000000, 0.6309523809523809312, 0.6369047619047618625, 0.6428571428571429047, 0.6488095238095238360, 0.6547619047619047672, 0.6607142857142856984, 0.6666666666666666297, 0.6726190476190476719, 0.6785714285714286031, 0.6845238095238095344, 0.6904761904761904656, 0.6964285714285713969, 0.7023809523809523281, 0.7083333333333333703, 0.7142857142857143016, 0.7202380952380952328, 0.7261904761904761640, 0.7321428571428570953, 0.7380952380952381375, 0.7440476190476190688, 0.7500000000000000000, 0.7559523809523809312, 0.7619047619047618625, 0.7678571428571429047, 0.7738095238095238360, 0.7797619047619047672, 0.7857142857142856984, 0.7916666666666666297, 0.7976190476190476719, 0.8035714285714286031, 0.8095238095238095344, 0.8154761904761904656, 0.8214285714285713969, 0.8273809523809523281, 0.8333333333333333703, 0.8392857142857143016, 0.8452380952380952328, 0.8511904761904761640, 0.8571428571428570953, 0.8630952380952381375, 0.8690476190476190688, 0.8750000000000000000, 0.8809523809523809312, 0.8869047619047618625, 0.8928571428571429047, 0.8988095238095238360, 0.9047619047619047672, 0.9107142857142856984, 0.9166666666666666297, 0.9226190476190476719, 0.9285714285714286031, 0.9345238095238095344, 0.9404761904761904656, 0.9464285714285713969, 0.9523809523809523281, 0.9583333333333333703, 0.9642857142857143016 ),
 .UNSPECIFIED. ) 
 GEOMETRIC_REPRESENTATION_ITEM ( )  RATIONAL_B_SPLINE_SURFACE ( (
 ( 1.000000000000000000, 0.9659258262890683122, 1.000000000000000000, 0.9659258262890683122, 1.000000000000000000, 0.9659258262890683122, 1.000000000000000000, 0.9659258262890683122, 1.000000000000000000, 0.9659258262890683122, 1.000000000000000000, 0.9659258262890683122, 1.000000000000000000, 0.9659258262890683122, 1.000000000000000000, 0.9659258262890683122, 1.000000000000000000, 0.9659258262890683122, 1.000000000000000000, 0.9659258262890683122, 1.000000000000000000, 0.9659258262890683122, 1.000000000000000000, 0.9659258262890683122, 1.000000000000000000, 0.9659258262890683122, 1.000000000000000000, 0.9659258262890683122, 1.000000000000000000, 0.9659258262890683122, 1.000000000000000000, 0.9659258262890683122, 1.000000000000000000, 0.9659258262890683122, 1.000000000000000000, 0.9659258262890683122, 1.000000000000000000, 0.9659258262890683122, 1.000000000000000000, 0.9659258262890683122, 1.000000000000000000, 0.9659258262890683122, 1.000000000000000000, 0.9659258262890683122, 1.000000000000000000, 0.9659258262890683122, 1.000000000000000000, 0.9659258262890683122, 1.000000000000000000, 0.9659258262890683122, 1.000000000000000000, 0.9659258262890683122, 1.000000000000000000, 0.9659258262890683122, 1.000000000000000000, 0.9659258262890683122, 1.000000000000000000, 0.9659258262890683122, 1.000000000000000000, 0.9659258262890683122, 1.000000000000000000, 0.9659258262890683122, 1.000000000000000000, 0.9659258262890683122, 1.000000000000000000, 0.9659258262890683122, 1.000000000000000000, 0.9659258262890683122, 1.000000000000000000, 0.9659258262890683122, 1.000000000000000000, 0.9659258262890683122, 1.000000000000000000, 0.9659258262890683122, 1.000000000000000000, 0.9659258262890683122, 1.000000000000000000, 0.9659258262890683122, 1.000000000000000000, 0.9659258262890683122, 1.000000000000000000, 0.9659258262890683122, 1.000000000000000000, 0.9659258262890683122, 1.000000000000000000, 0.9659258262890683122, 1.000000000000000000, 0.9659258262890683122, 1.000000000000000000, 0.9659258262890683122, 1.000000000000000000, 0.9659258262890683122, 1.000000000000000000, 0.9659258262890683122, 1.000000000000000000, 0.9659258262890683122, 1.000000000000000000, 0.9659258262890683122, 1.000000000000000000, 0.9659258262890683122, 1.000000000000000000, 0.9659258262890683122, 1.000000000000000000, 0.9659258262890683122, 1.000000000000000000, 0.9659258262890683122, 1.000000000000000000, 0.9659258262890683122, 1.000000000000000000, 0.9659258262890683122, 1.000000000000000000, 0.9659258262890683122, 1.000000000000000000, 0.9659258262890683122, 1.000000000000000000, 0.9659258262890683122, 1.000000000000000000, 0.9659258262890683122, 1.000000000000000000, 0.9659258262890683122, 1.000000000000000000, 0.9659258262890683122, 1.000000000000000000, 0.9659258262890683122, 1.000000000000000000, 0.9659258262890683122, 1.000000000000000000, 0.9659258262890683122, 1.000000000000000000, 0.9659258262890683122, 1.000000000000000000, 0.9659258262890683122, 1.000000000000000000, 0.9659258262890683122, 1.000000000000000000, 0.9659258262890683122, 1.000000000000000000, 0.9659258262890683122, 1.000000000000000000, 0.9659258262890683122, 1.000000000000000000, 0.9659258262890683122, 1.000000000000000000, 0.9659258262890683122, 1.000000000000000000, 0.9659258262890683122, 1.000000000000000000, 0.9659258262890683122, 1.000000000000000000, 0.9659258262890683122, 1.000000000000000000, 0.9659258262890683122, 1.000000000000000000, 0.9659258262890683122, 1.000000000000000000, 0.9659258262890683122, 1.000000000000000000, 0.9659258262890683122, 1.000000000000000000, 0.9659258262890683122, 1.000000000000000000, 0.9659258262890683122, 1.000000000000000000, 0.9659258262890683122, 1.000000000000000000, 0.9659258262890683122, 1.000000000000000000, 0.9659258262890683122, 1.000000000000000000, 0.9659258262890683122, 1.000000000000000000, 0.9659258262890683122, 1.000000000000000000, 0.9659258262890683122, 1.000000000000000000, 0.9659258262890683122, 1.000000000000000000, 0.9659258262890683122, 1.000000000000000000, 0.9659258262890683122, 1.000000000000000000, 0.9659258262890683122, 1.000000000000000000, 0.9659258262890683122, 1.000000000000000000, 0.9659258262890683122, 1.000000000000000000, 0.9659258262890683122, 1.000000000000000000, 0.9659258262890683122, 1.000000000000000000, 0.9659258262890683122, 1.000000000000000000, 0.9659258262890683122, 1.000000000000000000, 0.9659258262890683122, 1.000000000000000000, 0.9659258262890683122, 1.000000000000000000, 0.9659258262890683122, 1.000000000000000000, 0.9659258262890683122, 1.000000000000000000, 0.9659258262890683122, 1.000000000000000000, 0.9659258262890683122, 1.000000000000000000, 0.9659258262890683122, 1.000000000000000000, 0.9659258262890683122, 1.000000000000000000, 0.9659258262890683122, 1.000000000000000000, 0.9659258262890683122, 1.000000000000000000, 0.9659258262890683122, 1.000000000000000000, 0.9659258262890683122, 1.000000000000000000, 0.9659258262890683122, 1.000000000000000000, 0.9659258262890683122, 1.000000000000000000, 0.9659258262890683122, 1.000000000000000000, 0.9659258262890683122, 1.000000000000000000, 0.9659258262890683122, 1.000000000000000000, 0.9659258262890683122, 1.000000000000000000, 0.9659258262890683122, 1.000000000000000000, 0.9659258262890683122, 1.000000000000000000, 0.9659258262890683122, 1.000000000000000000, 0.9659258262890683122, 1.000000000000000000, 0.9659258262890683122, 1.000000000000000000, 0.9659258262890683122, 1.000000000000000000, 0.9659258262890683122, 1.000000000000000000, 0.9659258262890683122, 1.000000000000000000, 0.9659258262890683122, 1.000000000000000000, 0.9659258262890683122, 1.000000000000000000, 0.9659258262890683122, 1.000000000000000000, 0.9659258262890683122, 1.000000000000000000, 0.9659258262890683122, 1.000000000000000000, 0.9659258262890683122, 1.000000000000000000, 0.9659258262890683122, 1.000000000000000000, 0.9659258262890683122, 1.000000000000000000, 0.9659258262890683122, 1.000000000000000000, 0.9659258262890683122, 1.000000000000000000, 0.9659258262890683122, 1.000000000000000000, 0.9659258262890683122, 1.000000000000000000, 0.9659258262890683122, 1.000000000000000000, 0.9659258262890683122, 1.000000000000000000, 0.9659258262890683122, 1.000000000000000000, 0.9659258262890683122, 1.000000000000000000, 0.9659258262890683122, 1.000000000000000000, 0.9659258262890683122, 1.000000000000000000, 0.9659258262890683122, 1.000000000000000000, 0.9659258262890683122, 1.000000000000000000, 0.9659258262890683122, 1.000000000000000000, 0.9659258262890683122, 1.000000000000000000, 0.9659258262890683122, 1.000000000000000000, 0.9659258262890683122, 1.000000000000000000, 0.9659258262890683122, 1.000000000000000000, 0.9659258262890683122, 1.000000000000000000, 0.9659258262890683122, 1.000000000000000000, 0.9659258262890683122, 1.000000000000000000, 0.9659258262890683122, 1.000000000000000000, 0.9659258262890683122, 1.000000000000000000, 0.9659258262890683122, 1.000000000000000000, 0.9659258262890683122, 1.000000000000000000, 0.9659258262890683122, 1.000000000000000000, 0.9659258262890683122, 1.000000000000000000, 0.9659258262890683122, 1.000000000000000000, 0.9659258262890683122, 1.000000000000000000, 0.9659258262890683122, 1.000000000000000000, 0.9659258262890683122, 1.000000000000000000, 0.9659258262890683122, 1.000000000000000000),
 ( 1.000000000000000000, 0.9659258262890683122, 1.000000000000000000, 0.9659258262890683122, 1.000000000000000000, 0.9659258262890683122, 1.000000000000000000, 0.9659258262890683122, 1.000000000000000000, 0.9659258262890683122, 1.000000000000000000, 0.9659258262890683122, 1.000000000000000000, 0.9659258262890683122, 1.000000000000000000, 0.9659258262890683122, 1.000000000000000000, 0.9659258262890683122, 1.000000000000000000, 0.9659258262890683122, 1.000000000000000000, 0.9659258262890683122, 1.000000000000000000, 0.9659258262890683122, 1.000000000000000000, 0.9659258262890683122, 1.000000000000000000, 0.9659258262890683122, 1.000000000000000000, 0.9659258262890683122, 1.000000000000000000, 0.9659258262890683122, 1.000000000000000000, 0.9659258262890683122, 1.000000000000000000, 0.9659258262890683122, 1.000000000000000000, 0.9659258262890683122, 1.000000000000000000, 0.9659258262890683122, 1.000000000000000000, 0.9659258262890683122, 1.000000000000000000, 0.9659258262890683122, 1.000000000000000000, 0.9659258262890683122, 1.000000000000000000, 0.9659258262890683122, 1.000000000000000000, 0.9659258262890683122, 1.000000000000000000, 0.9659258262890683122, 1.000000000000000000, 0.9659258262890683122, 1.000000000000000000, 0.9659258262890683122, 1.000000000000000000, 0.9659258262890683122, 1.000000000000000000, 0.9659258262890683122, 1.000000000000000000, 0.9659258262890683122, 1.000000000000000000, 0.9659258262890683122, 1.000000000000000000, 0.9659258262890683122, 1.000000000000000000, 0.9659258262890683122, 1.000000000000000000, 0.9659258262890683122, 1.000000000000000000, 0.9659258262890683122, 1.000000000000000000, 0.9659258262890683122, 1.000000000000000000, 0.9659258262890683122, 1.000000000000000000, 0.9659258262890683122, 1.000000000000000000, 0.9659258262890683122, 1.000000000000000000, 0.9659258262890683122, 1.000000000000000000, 0.9659258262890683122, 1.000000000000000000, 0.9659258262890683122, 1.000000000000000000, 0.9659258262890683122, 1.000000000000000000, 0.9659258262890683122, 1.000000000000000000, 0.9659258262890683122, 1.000000000000000000, 0.9659258262890683122, 1.000000000000000000, 0.9659258262890683122, 1.000000000000000000, 0.9659258262890683122, 1.000000000000000000, 0.9659258262890683122, 1.000000000000000000, 0.9659258262890683122, 1.000000000000000000, 0.9659258262890683122, 1.000000000000000000, 0.9659258262890683122, 1.000000000000000000, 0.9659258262890683122, 1.000000000000000000, 0.9659258262890683122, 1.000000000000000000, 0.9659258262890683122, 1.000000000000000000, 0.9659258262890683122, 1.000000000000000000, 0.9659258262890683122, 1.000000000000000000, 0.9659258262890683122, 1.000000000000000000, 0.9659258262890683122, 1.000000000000000000, 0.9659258262890683122, 1.000000000000000000, 0.9659258262890683122, 1.000000000000000000, 0.9659258262890683122, 1.000000000000000000, 0.9659258262890683122, 1.000000000000000000, 0.9659258262890683122, 1.000000000000000000, 0.9659258262890683122, 1.000000000000000000, 0.9659258262890683122, 1.000000000000000000, 0.9659258262890683122, 1.000000000000000000, 0.9659258262890683122, 1.000000000000000000, 0.9659258262890683122, 1.000000000000000000, 0.9659258262890683122, 1.000000000000000000, 0.9659258262890683122, 1.000000000000000000, 0.9659258262890683122, 1.000000000000000000, 0.9659258262890683122, 1.000000000000000000, 0.9659258262890683122, 1.000000000000000000, 0.9659258262890683122, 1.000000000000000000, 0.9659258262890683122, 1.000000000000000000, 0.9659258262890683122, 1.000000000000000000, 0.9659258262890683122, 1.000000000000000000, 0.9659258262890683122, 1.000000000000000000, 0.9659258262890683122, 1.000000000000000000, 0.9659258262890683122, 1.000000000000000000, 0.9659258262890683122, 1.000000000000000000, 0.9659258262890683122, 1.000000000000000000, 0.9659258262890683122, 1.000000000000000000, 0.9659258262890683122, 1.000000000000000000, 0.9659258262890683122, 1.000000000000000000, 0.9659258262890683122, 1.000000000000000000, 0.9659258262890683122, 1.000000000000000000, 0.9659258262890683122, 1.000000000000000000, 0.9659258262890683122, 1.000000000000000000, 0.9659258262890683122, 1.000000000000000000, 0.9659258262890683122, 1.000000000000000000, 0.9659258262890683122, 1.000000000000000000, 0.9659258262890683122, 1.000000000000000000, 0.9659258262890683122, 1.000000000000000000, 0.9659258262890683122, 1.000000000000000000, 0.9659258262890683122, 1.000000000000000000, 0.9659258262890683122, 1.000000000000000000, 0.9659258262890683122, 1.000000000000000000, 0.9659258262890683122, 1.000000000000000000, 0.9659258262890683122, 1.000000000000000000, 0.9659258262890683122, 1.000000000000000000, 0.9659258262890683122, 1.000000000000000000, 0.9659258262890683122, 1.000000000000000000, 0.9659258262890683122, 1.000000000000000000, 0.9659258262890683122, 1.000000000000000000, 0.9659258262890683122, 1.000000000000000000, 0.9659258262890683122, 1.000000000000000000, 0.9659258262890683122, 1.000000000000000000, 0.9659258262890683122, 1.000000000000000000, 0.9659258262890683122, 1.000000000000000000, 0.9659258262890683122, 1.000000000000000000, 0.9659258262890683122, 1.000000000000000000, 0.9659258262890683122, 1.000000000000000000, 0.9659258262890683122, 1.000000000000000000, 0.9659258262890683122, 1.000000000000000000, 0.9659258262890683122, 1.000000000000000000, 0.9659258262890683122, 1.000000000000000000, 0.9659258262890683122, 1.000000000000000000, 0.9659258262890683122, 1.000000000000000000, 0.9659258262890683122, 1.000000000000000000, 0.9659258262890683122, 1.000000000000000000, 0.9659258262890683122, 1.000000000000000000, 0.9659258262890683122, 1.000000000000000000, 0.9659258262890683122, 1.000000000000000000, 0.9659258262890683122, 1.000000000000000000, 0.9659258262890683122, 1.000000000000000000, 0.9659258262890683122, 1.000000000000000000, 0.9659258262890683122, 1.000000000000000000, 0.9659258262890683122, 1.000000000000000000, 0.9659258262890683122, 1.000000000000000000, 0.9659258262890683122, 1.000000000000000000, 0.9659258262890683122, 1.000000000000000000, 0.9659258262890683122, 1.000000000000000000, 0.9659258262890683122, 1.000000000000000000, 0.9659258262890683122, 1.000000000000000000, 0.9659258262890683122, 1.000000000000000000, 0.9659258262890683122, 1.000000000000000000, 0.9659258262890683122, 1.000000000000000000, 0.9659258262890683122, 1.000000000000000000, 0.9659258262890683122, 1.000000000000000000, 0.9659258262890683122, 1.000000000000000000, 0.9659258262890683122, 1.000000000000000000, 0.9659258262890683122, 1.000000000000000000, 0.9659258262890683122, 1.000000000000000000, 0.9659258262890683122, 1.000000000000000000, 0.9659258262890683122, 1.000000000000000000, 0.9659258262890683122, 1.000000000000000000, 0.9659258262890683122, 1.000000000000000000, 0.9659258262890683122, 1.000000000000000000, 0.9659258262890683122, 1.000000000000000000, 0.9659258262890683122, 1.000000000000000000, 0.9659258262890683122, 1.000000000000000000, 0.9659258262890683122, 1.000000000000000000, 0.9659258262890683122, 1.000000000000000000, 0.9659258262890683122, 1.000000000000000000, 0.9659258262890683122, 1.000000000000000000, 0.9659258262890683122, 1.000000000000000000, 0.9659258262890683122, 1.000000000000000000, 0.9659258262890683122, 1.000000000000000000, 0.9659258262890683122, 1.000000000000000000) ) ) 
 REPRESENTATION_ITEM ( '' )  SURFACE ( )  );
#82261 = CARTESIAN_POINT ( 'NONE',  ( -1.161435516476850394, -2.368486780965353193E-16, 4.088522901378193630 ) ) ;
#82262 = CARTESIAN_POINT ( 'NONE',  ( 17.20831665107776587, 34.13393115100078745, -7.208316651077762316 ) ) ;
#82263 = CARTESIAN_POINT ( 'NONE',  ( 17.96484262340118221, 31.18868534415483751, -7.964842623401177768 ) ) ;
#82264 = UNCERTAINTY_MEASURE_WITH_UNIT (LENGTH_MEASURE( 1.000000000000000082E-05 ), #67571, 'distance_accuracy_value', 'NONE');
#82265 =( BOUNDED_CURVE ( )  B_SPLINE_CURVE ( 3, ( #78184, #24219, #39715, #54685 ),
 .UNSPECIFIED., .F., .T. ) 
 B_SPLINE_CURVE_WITH_KNOTS ( ( 4, 4 ),
 ( 3.694400132159526340, 4.712388980384689674 ),
 .UNSPECIFIED. ) 
 CURVE ( )  GEOMETRIC_REPRESENTATION_ITEM ( )  RATIONAL_B_SPLINE_CURVE ( ( 1.000000000000000000, 0.9154899770527751279, 0.9154899770527751279, 1.000000000000000000 ) ) 
 REPRESENTATION_ITEM ( '' )  );
#82266 = VERTEX_POINT ( 'NONE', #55891 ) ;
#82267 = CARTESIAN_POINT ( 'NONE',  ( 3.591859063236763294, 63.29030133659708923, -11.09922568453595026 ) ) ;
#82268 = CIRCLE ( 'NONE', #85500, 0.2500000000000002220 ) ;
#82269 = CARTESIAN_POINT ( 'NONE',  ( 8.235571585149873641, 4.796802177851536619, 8.235571585149866536 ) ) ;
#82270 = CARTESIAN_POINT ( 'NONE',  ( 10.00000000000000000, 14.75893115100078568, -9.846743663894594434 ) ) ;
#82271 = CARTESIAN_POINT ( 'NONE',  ( 10.00000000000000000, 37.87363466993041783, -12.81628187352647608 ) ) ;
#82273 = CARTESIAN_POINT ( 'NONE',  ( 7.361572987183169658, 29.96726448433411960, -9.846743663894592657 ) ) ;
#82272 = CARTESIAN_POINT ( 'NONE',  ( -0.8801773607110991993, 2.855352010821504471, -2.915334737309923874 ) ) ;
#82274 = CARTESIAN_POINT ( 'NONE',  ( 20.00000000000000711, 89.81050759285248830, 4.994480956901625746 ) ) ;
#82275 = CARTESIAN_POINT ( 'NONE',  ( 17.20831665107776587, 2.883931151000785231, 7.208316651077764980 ) ) ;
#82276 = CARTESIAN_POINT ( 'NONE',  ( -0.3689425029237898834, 16.17874883491396076, -10.36894250292378850 ) ) ;
#82277 = CARTESIAN_POINT ( 'NONE',  ( -0.3689425029237881626, 47.42874883491396787, 10.36894250292379027 ) ) ;
#82278 = CARTESIAN_POINT ( 'NONE',  ( 0.1532563361054083140, 46.00893115100079456, 1.131784320476157264E-15 ) ) ;
#82279 = CARTESIAN_POINT ( 'NONE',  ( 5.783708210295563923, -36.05554043934295549, -2.500000000000000444 ) ) ;
#82280 = CARTESIAN_POINT ( 'NONE',  ( 4.559911319644449179, 38.89701867748817676, 9.422509992056141925 ) ) ;
#82281 = CARTESIAN_POINT ( 'NONE',  ( 0.1532563361054083140, 1.008931151000784787, 1.131784320476157264E-15 ) ) ;
#82282 = ORIENTED_EDGE ( 'NONE', *, *, #49726, .T. ) ;
#82283 = CARTESIAN_POINT ( 'NONE',  ( 19.38216949554541557, 52.24863466993041072, -9.382169495545420901 ) ) ;
#82284 = ORIENTED_EDGE ( 'NONE', *, *, #54646, .F. ) ;
#82285 = CARTESIAN_POINT ( 'NONE',  ( 4.559911319644449179, 67.23035201082150536, -9.422509992056141925 ) ) ;
#82286 = VERTEX_POINT ( 'NONE', #32875 ) ;
#82287 = AXIS2_PLACEMENT_3D ( 'NONE', #29337, #38834, #37858 ) ;
#82288 = CARTESIAN_POINT ( 'NONE',  ( 1.472469842513823179, 6.425597817667451750, 4.923371831947296329 ) ) ;
#82289 = ORIENTED_EDGE ( 'NONE', *, *, #21078, .F. ) ;
#82290 = EDGE_CURVE ( 'NONE', #5292, #78351, #37141, .T. ) ;
#82291 = CARTESIAN_POINT ( 'NONE',  ( 20.88017736071110164, 20.35535201082150891, 2.915334737309930979 ) ) ;
#82292 = AXIS2_PLACEMENT_3D ( 'NONE', #87659, #4679, #49652 ) ;
#82293 = EDGE_CURVE ( 'NONE', #14929, #16647, #62886, .T. ) ;
#82294 = EDGE_CURVE ( 'NONE', #4379, #64701, #31915, .T. ) ;
#82295 = ORIENTED_EDGE ( 'NONE', *, *, #70069, .F. ) ;
#82296 = CARTESIAN_POINT ( 'NONE',  ( 20.88017736071110519, 40.56368534415484106, 2.639326808657452039E-16 ) ) ;
#82297 = CARTESIAN_POINT ( 'NONE',  ( 12.63842701281683922, 54.55059781766745175, -9.846743663894590881 ) ) ;
#82298 = ORIENTED_EDGE ( 'NONE', *, *, #37815, .T. ) ;
#82299 = CARTESIAN_POINT ( 'NONE',  ( 19.84674366389459266, 58.71726448433411605, -2.638427012816827677 ) ) ;
#82300 = EDGE_LOOP ( 'NONE', ( #590, #76467, #92342, #36428, #72699, #78599 ) ) ;
#82301 = CARTESIAN_POINT ( 'NONE',  ( 17.96484262340118221, 59.93868534415484106, 7.964842623401181321 ) ) ;
#82302 = CARTESIAN_POINT ( 'NONE',  ( -12.15129255554601428, -0.03417435944610275333, -10.40305174771256524 ) ) ;
#82303 = CARTESIAN_POINT ( 'NONE',  ( 19.38216949554541202, 35.99863466993041072, 9.382169495545424454 ) ) ;
#82305 = CARTESIAN_POINT ( 'NONE',  ( 20.15039907845753575, 6.748846992468889638, 6.262539305110063736 ) ) ;
#82304 = CARTESIAN_POINT ( 'NONE',  ( 4.559911319644449179, 27.23035201082150536, -9.422509992056141925 ) ) ;
#82306 = CARTESIAN_POINT ( 'NONE',  ( 19.84674366389459266, 8.717264484334116048, -2.638427012816827677 ) ) ;
#82307 = CARTESIAN_POINT ( 'NONE',  ( 20.88017736071110875, 15.77201867748817143, -2.915334737309920765 ) ) ;
#82308 = ADVANCED_FACE ( 'NONE', ( #86873 ), #93010, .T. ) ;
#82309 = B_SPLINE_CURVE_WITH_KNOTS ( 'NONE', 3,
 ( #80743, #51733, #28225, #73228, #21230, #36733 ),
 .UNSPECIFIED., .F., .F.,
 ( 4, 2, 4 ),
 ( 0.000000000000000000, 0.0002565770811490928911, 0.0005131541622981857821 ),
 .UNSPECIFIED. ) ;
#82310 = CIRCLE ( 'NONE', #47192, 15.00000000000000000 ) ;
#82311 = ORIENTED_EDGE ( 'NONE', *, *, #90341, .F. ) ;
#82312 = CARTESIAN_POINT ( 'NONE',  ( 0.6178305044545818747, 58.49863466993042493, -9.382169495545419124 ) ) ;
#82313 = CARTESIAN_POINT ( 'NONE',  ( 10.00000000000000178, 49.31368534415484106, 10.88017736071110342 ) ) ;
#82314 = CARTESIAN_POINT ( 'NONE',  ( -5.361923921558562789, 0.000000000000000000, -0.9937738586172705224 ) ) ;
#82315 = MECHANICAL_DESIGN_GEOMETRIC_PRESENTATION_REPRESENTATION (  '', ( #32780 ), #63187 ) ;
#82316 = CARTESIAN_POINT ( 'NONE',  ( 19.38216949554541557, 52.24863466993041072, -9.382169495545420901 ) ) ;
#82317 = CARTESIAN_POINT ( 'NONE',  ( -0.8801773607110991993, 42.85535201082150536, -2.915334737309923874 ) ) ;
#82318 = CARTESIAN_POINT ( 'NONE',  ( 12.63842701281683922, 54.55059781766745175, -9.846743663894590881 ) ) ;
#82319 = EDGE_CURVE ( 'NONE', #63645, #78249, #64225, .T. ) ;
#82320 = CARTESIAN_POINT ( 'NONE',  ( 17.20831665107776587, 17.88393115100078745, 7.208316651077764980 ) ) ;
#82321 = CARTESIAN_POINT ( 'NONE',  ( -2.816281873526473856, 4.331968003263754419, 3.434112377981055619 ) ) ;
#82323 = CARTESIAN_POINT ( 'NONE',  ( 18.52753015748618282, 63.92559781766745886, -4.923371831947291888 ) ) ;
#82322 = CARTESIAN_POINT ( 'NONE',  ( 9.065164099344530158, 15.00000000000000000, -11.95084933600767307 ) ) ;
#82324 = CARTESIAN_POINT ( 'NONE',  ( 19.42250999205614193, 35.14701867748816966, 5.440088680355555262 ) ) ;
#82325 = CARTESIAN_POINT ( 'NONE',  ( 5.076628168052704559, 50.17559781766745886, -8.527530157486179263 ) ) ;
#82326 = SURFACE_STYLE_USAGE ( .BOTH. , #44817 ) ;
#82327 = CARTESIAN_POINT ( 'NONE',  ( 1.472469842513823179, 26.42559781766745175, 4.923371831947296329 ) ) ;
#82328 = CARTESIAN_POINT ( 'NONE',  ( 17.20831665107776587, 9.133931151000787452, -7.208316651077762316 ) ) ;
#82330 = ORIENTED_EDGE ( 'NONE', *, *, #50053, .F. ) ;
#82329 = CARTESIAN_POINT ( 'NONE',  ( -2.816281873526471635, 8.915301336597083903, -3.434112377981056508 ) ) ;
#82331 = EDGE_CURVE ( 'NONE', #4363, #48181, #6803, .T. ) ;
#82332 = FACE_OUTER_BOUND ( 'NONE', #96040, .T. ) ;
#82333 = FACE_OUTER_BOUND ( 'NONE', #48596, .T. ) ;
#82334 = CARTESIAN_POINT ( 'NONE',  ( 0.6178305044545838731, 34.74863466993042493, 9.382169495545420901 ) ) ;
#82335 = AXIS2_PLACEMENT_3D ( 'NONE', #93673, #2708, #24213 ) ;
#82336 = CARTESIAN_POINT ( 'NONE',  ( 2.791683348922237240, 35.38393115100079456, -7.208316651077763204 ) ) ;
#82337 = DIRECTION ( 'NONE',  ( -0.000000000000000000, 1.000000000000000000, -0.000000000000000000 ) ) ;
#82338 = CARTESIAN_POINT ( 'NONE',  ( 20.88017736071110875, 10.77201867748817143, -2.915334737309920765 ) ) ;
#82339 = CARTESIAN_POINT ( 'NONE',  ( 12.63842701281683034, 32.46726448433412315, 9.846743663894596210 ) ) ;
#82340 = ORIENTED_EDGE ( 'NONE', *, *, #24209, .F. ) ;
#82341 = CARTESIAN_POINT ( 'NONE',  ( -0.8060400322139609219, 0.000000000000000000, 5.393339789881734347 ) ) ;
#82342 = CARTESIAN_POINT ( 'NONE',  ( 6.204703633549690345, 65.76208216824731778, -14.16423886937410259 ) ) ;
#82343 = CARTESIAN_POINT ( 'NONE',  ( -7.804338076140435732, 84.96756567522902515, -4.038273117401846690 ) ) ;
#82344 = CARTESIAN_POINT ( 'NONE',  ( 20.88017736071110164, 20.35535201082150891, 2.915334737309930979 ) ) ;
#82345 = CARTESIAN_POINT ( 'NONE',  ( -2.266590686148945544, 52.22041550158064638, 7.082119434687048631 ) ) ;
#82347 = DIRECTION ( 'NONE',  ( -0.000000000000000000, -1.000000000000000000, -0.000000000000000000 ) ) ;
#82346 = CARTESIAN_POINT ( 'NONE',  ( 22.26659068614895176, 54.72041550158063217, -7.082119434687042414 ) ) ;
#82348 = DIRECTION ( 'NONE',  ( 0.000000000000000000, 0.000000000000000000, 1.000000000000000000 ) ) ;
#82349 = CARTESIAN_POINT ( 'NONE',  ( 5.076628168052704559, 5.175597817667451750, -8.527530157486179263 ) ) ;
#82350 = CARTESIAN_POINT ( 'NONE',  ( 13.43411237798106583, 2.665301336597086568, -12.81628187352647252 ) ) ;
#82351 = ORIENTED_EDGE ( 'NONE', *, *, #48740, .F. ) ;
#82352 = TOROIDAL_SURFACE ( 'NONE', #61584, 14.49999999999999822, 0.5000000000000000000 ) ;
#82353 = CARTESIAN_POINT ( 'NONE',  ( 5.076628168052703671, 61.84226448433412315, 8.527530157486179263 ) ) ;
#82354 = DIRECTION ( 'NONE',  ( 0.000000000000000000, 0.000000000000000000, 1.000000000000000000 ) ) ;
#82355 = CARTESIAN_POINT ( 'NONE',  ( 19.84674366389459621, 63.50893115100078745, 7.409399052514197653E-17 ) ) ;
#82356 = CARTESIAN_POINT ( 'NONE',  ( -2.266590686148945544, 6.387082168247300906, -7.082119434687050408 ) ) ;
#82357 = CARTESIAN_POINT ( 'NONE',  ( 12.63842701281683034, 22.46726448433411605, 9.846743663894596210 ) ) ;
#82358 = DIRECTION ( 'NONE',  ( -0.000000000000000000, -1.000000000000000000, -0.000000000000000000 ) ) ;
#82359 = ORIENTED_EDGE ( 'NONE', *, *, #92884, .T. ) ;
#82360 = CARTESIAN_POINT ( 'NONE',  ( 22.26659068614895176, 44.72041550158063927, -7.082119434687042414 ) ) ;
#82361 = CARTESIAN_POINT ( 'NONE',  ( 19.84674366389459621, 3.508931151000785231, 7.409399052514197653E-17 ) ) ;
#82362 = CARTESIAN_POINT ( 'NONE',  ( 0.1922240491738418933, 63.18878173731739878, 6.499999999999971578 ) ) ;
#82363 = CARTESIAN_POINT ( 'NONE',  ( 10.00000000000000178, 29.31368534415483751, 10.88017736071110342 ) ) ;
#82364 = CARTESIAN_POINT ( 'NONE',  ( 6.565887622018943937, 35.16530133659708923, 12.81628187352647430 ) ) ;
#82365 = FILL_AREA_STYLE_COLOUR ( '', #4953 ) ;
#82366 = CARTESIAN_POINT ( 'NONE',  ( 19.38216949554541202, 35.99863466993041072, 9.382169495545424454 ) ) ;
#82367 = CARTESIAN_POINT ( 'NONE',  ( 0.6178305044545818747, 58.49863466993042493, -9.382169495545419124 ) ) ;
#82368 = VERTEX_POINT ( 'NONE', #87843 ) ;
#82369 = CARTESIAN_POINT ( 'NONE',  ( 3.969999999999999751, 36.75000000000000000, -2.500000000000000000 ) ) ;
#82370 = FACE_OUTER_BOUND ( 'NONE', #47018, .T. ) ;
#82371 = CARTESIAN_POINT ( 'NONE',  ( 13.79529636645030344, 43.26208216824730357, 14.16423886937410614 ) ) ;
#82372 = CARTESIAN_POINT ( 'NONE',  ( 10.00000000000000178, 3.053748834913967425, 14.16423886937410082 ) ) ;
#82373 = CARTESIAN_POINT ( 'NONE',  ( -0.8801773607110991993, 2.855352010821504471, -2.915334737309923874 ) ) ;
#82374 = CARTESIAN_POINT ( 'NONE',  ( 2.035157376598824452, 18.68868534415484106, 7.964842623401179544 ) ) ;
#82375 = CARTESIAN_POINT ( 'NONE',  ( 5.054308323419911098, 70.51564955044841554, 12.00000000000000000 ) ) ;
#82376 = CARTESIAN_POINT ( 'NONE',  ( 8.979999999999991545, 27.04366094290857347, -3.000000000000000000 ) ) ;
#82377 = CARTESIAN_POINT ( 'NONE',  ( -0.8801773607111009756, 53.06368534415484106, 1.068504757029289695E-15 ) ) ;
#82378 = CARTESIAN_POINT ( 'NONE',  ( -0.8801773607111008646, 53.27201867748816966, 2.915334737309923430 ) ) ;
#82379 = CARTESIAN_POINT ( 'NONE',  ( -2.816281873526471635, 23.91530133659708568, -3.434112377981056508 ) ) ;
#82380 = CARTESIAN_POINT ( 'NONE',  ( -11.81378540890942119, 0.000000000000000000, 7.968498874458034287 ) ) ;
#82381 = DIRECTION ( 'NONE',  ( -0.9366721892483949041, 0.000000000000000000, -0.3502073812594748148 ) ) ;
#82382 = CARTESIAN_POINT ( 'NONE',  ( 18.52753015748617571, 28.09226448433411960, 4.923371831947298993 ) ) ;
#82383 = ADVANCED_FACE ( 'NONE', ( #64350 ), #9398, .T. ) ;
#82384 = CARTESIAN_POINT ( 'NONE',  ( 10.00000000000000000, 51.81368534415484106, -10.88017736071110342 ) ) ;
#82385 = VECTOR ( 'NONE', #82337, 1000.000000000000000 ) ;
#82386 = AXIS2_PLACEMENT_3D ( 'NONE', #76158, #91655, #19824 ) ;
#82387 = CARTESIAN_POINT ( 'NONE',  ( 22.81628187352648496, 16.83196800326374998, -3.434112377981050290 ) ) ;
#82388 = CARTESIAN_POINT ( 'NONE',  ( 15.41943733314631793, 15.00000000000000000, -4.256565371896342320 ) ) ;
#82389 = CARTESIAN_POINT ( 'NONE',  ( 10.00000000000000178, 14.31368534415483751, 10.88017736071110342 ) ) ;
#82390 = VECTOR ( 'NONE', #97729, 1000.000000000000000 ) ;
#82391 = CARTESIAN_POINT ( 'NONE',  ( 5.076628168052704559, 45.17559781766745175, -8.527530157486179263 ) ) ;
#82392 = CARTESIAN_POINT ( 'NONE',  ( 22.81628187352647785, 51.62363466993042493, 6.195893100308588602E-16 ) ) ;
#82393 = CARTESIAN_POINT ( 'NONE',  ( 1.472469842513823179, 25.59226448433412315, -4.923371831947296329 ) ) ;
#82394 = CARTESIAN_POINT ( 'NONE',  ( 22.26659068614895176, 9.720415501580633943, -7.082119434687042414 ) ) ;
#82395 = CARTESIAN_POINT ( 'NONE',  ( 3.927832320392154575, 15.00000000000000000, 13.69797916712106733 ) ) ;
#82396 = CARTESIAN_POINT ( 'NONE',  ( 7.084665262690076126, 19.10535201082150181, 10.88017736071109987 ) ) ;
#82397 = PRESENTATION_STYLE_ASSIGNMENT (( #73913 ) ) ;
#82398 = CARTESIAN_POINT ( 'NONE',  ( 5.076628168052704559, 50.17559781766745886, -8.527530157486179263 ) ) ;
#82399 = CARTESIAN_POINT ( 'NONE',  ( 0.5774900079438590739, 32.64701867748816966, -5.440088680355550821 ) ) ;
#82400 = CARTESIAN_POINT ( 'NONE',  ( 12.91533473730992121, 14.52201867748817143, 10.88017736071110164 ) ) ;
#82401 = ORIENTED_EDGE ( 'NONE', *, *, #63590, .T. ) ;
#82402 = EDGE_CURVE ( 'NONE', #64121, #89795, #2046, .T. ) ;
#82403 = CARTESIAN_POINT ( 'NONE',  ( -0.8801773607111009756, 23.06368534415484106, 1.068504757029289695E-15 ) ) ;
#82404 = CARTESIAN_POINT ( 'NONE',  ( 22.81628187352648496, 46.83196800326376064, -3.434112377981050290 ) ) ;
#82405 = CARTESIAN_POINT ( 'NONE',  ( 7.084665262690076126, 32.02201867748816966, -10.88017736071110164 ) ) ;
#82407 = CARTESIAN_POINT ( 'NONE',  ( 10.00000000000000000, 36.81368534415484106, -10.88017736071110342 ) ) ;
#82406 = FACE_OUTER_BOUND ( 'NONE', #77157, .T. ) ;
#82408 = ORIENTED_EDGE ( 'NONE', *, *, #40716, .T. ) ;
#82409 = CARTESIAN_POINT ( 'NONE',  ( 0.1532563361054083140, 56.00893115100078745, 1.131784320476157264E-15 ) ) ;
#82411 = EDGE_CURVE ( 'NONE', #61124, #74408, #58824, .T. ) ;
#82410 = CARTESIAN_POINT ( 'NONE',  ( -0.8801773607110991993, 42.85535201082150536, -2.915334737309923874 ) ) ;
#82412 = CARTESIAN_POINT ( 'NONE',  ( 5.076628168052703671, 66.84226448433412315, 8.527530157486179263 ) ) ;
#82413 = CARTESIAN_POINT ( 'NONE',  ( 22.81628187352648496, 56.83196800326374643, -3.434112377981050290 ) ) ;
#82414 = CARTESIAN_POINT ( 'NONE',  ( 0.000000000000000000, 14.49999999999999822, 0.000000000000000000 ) ) ;
#82415 = CARTESIAN_POINT ( 'NONE',  ( 17.08211943468705840, 45.13708216824730357, -12.26659068614894466 ) ) ;
#82416 = CARTESIAN_POINT ( 'NONE',  ( 7.084665262690076126, 52.02201867748816255, -10.88017736071110164 ) ) ;
#82417 = CARTESIAN_POINT ( 'NONE',  ( 12.63842701281683034, 62.46726448433410894, 9.846743663894596210 ) ) ;
#82418 = EDGE_CURVE ( 'NONE', #86252, #57318, #57837, .T. ) ;
#82419 = CARTESIAN_POINT ( 'NONE',  ( 0.000000000000000000, 0.5000000000000004441, 0.000000000000000000 ) ) ;
#82420 = CARTESIAN_POINT ( 'NONE',  ( 0.1532563361054082862, 66.21726448433413736, 2.638427012816831674 ) ) ;
#82421 =( LENGTH_UNIT ( ) NAMED_UNIT ( * ) SI_UNIT ( .MILLI., .METRE. ) );
#82422 = CARTESIAN_POINT ( 'NONE',  ( 2.791683348922237240, 20.38393115100078745, -7.208316651077763204 ) ) ;
#82423 = VERTEX_POINT ( 'NONE', #88346 ) ;
#82424 = CARTESIAN_POINT ( 'NONE',  ( 10.00000000000000178, 27.25893115100078390, 9.846743663894594434 ) ) ;
#82425 = CARTESIAN_POINT ( 'NONE',  ( 6.408140936763236262, -17.54303199673624292, -11.09922568453595026 ) ) ;
#82426 = CARTESIAN_POINT ( 'NONE',  ( 15.44008868035555260, 29.73035201082150891, 9.422509992056143702 ) ) ;
#82427 = CARTESIAN_POINT ( 'NONE',  ( 0.1532563361054082862, 21.21726448433412315, 2.638427012816831674 ) ) ;
#82428 =( NAMED_UNIT ( * ) PLANE_ANGLE_UNIT ( ) SI_UNIT ( $, .RADIAN. ) );
#82429 = CARTESIAN_POINT ( 'NONE',  ( 0.6178305044545838731, 14.74863466993041783, 9.382169495545420901 ) ) ;
#82431 = CARTESIAN_POINT ( 'NONE',  ( 0.5774900079438590739, 62.64701867748817676, -5.440088680355550821 ) ) ;
#82430 = DIRECTION ( 'NONE',  ( 0.000000000000000000, 0.000000000000000000, 1.000000000000000000 ) ) ;
#82433 = CARTESIAN_POINT ( 'NONE',  ( 0.6178305044545838731, 54.74863466993042493, 9.382169495545420901 ) ) ;
#82432 = CARTESIAN_POINT ( 'NONE',  ( 0.5774900079438607392, 38.48035201082150536, 5.440088680355550821 ) ) ;
#82434 = CARTESIAN_POINT ( 'NONE',  ( -0.3689425029237898834, 51.17874883491397497, -10.36894250292378850 ) ) ;
#82435 = CIRCLE ( 'NONE', #39337, 14.49999999999999822 ) ;
#82436 = EDGE_CURVE ( 'NONE', #51651, #53171, #47524, .T. ) ;
#82437 = DIRECTION ( 'NONE',  ( 0.000000000000000000, 0.000000000000000000, 1.000000000000000000 ) ) ;
#82438 = ORIENTED_EDGE ( 'NONE', *, *, #58859, .F. ) ;
#82439 = CARTESIAN_POINT ( 'NONE',  ( 16.40814093676323893, 10.79030133659708923, 11.09922568453595026 ) ) ;
#82440 = CARTESIAN_POINT ( 'NONE',  ( 20.88017736071110875, 5.772018677488170546, -2.915334737309920765 ) ) ;
#82441 = CARTESIAN_POINT ( 'NONE',  ( 7.084665262690076126, 44.10535201082151247, 10.88017736071109987 ) ) ;
#82442 = CARTESIAN_POINT ( 'NONE',  ( 0.000000000000000000, 13.17686044187655270, 0.000000000000000000 ) ) ;
#82444 = ORIENTED_EDGE ( 'NONE', *, *, #56566, .F. ) ;
#82443 = EDGE_CURVE ( 'NONE', #53168, #26718, #82051, .T. ) ;
#82445 = CARTESIAN_POINT ( 'NONE',  ( 7.084665262690076126, 59.10535201082150536, 10.88017736071109987 ) ) ;
#82446 = CARTESIAN_POINT ( 'NONE',  ( 17.20831665107776587, 39.13393115100079456, -7.208316651077762316 ) ) ;
#82447 = CARTESIAN_POINT ( 'NONE',  ( 5.076628168052703671, 26.84226448433411960, 8.527530157486179263 ) ) ;
#82448 = B_SPLINE_CURVE_WITH_KNOTS ( 'NONE', 3,
 ( #60684, #76190, #54651, #92656 ),
 .UNSPECIFIED., .F., .F.,
 ( 4, 4 ),
 ( 0.000000000000000000, 0.0004119852744258499034 ),
 .UNSPECIFIED. ) ;
#82449 = CARTESIAN_POINT ( 'NONE',  ( 0.1532563361054082862, 11.21726448433411605, 2.638427012816831674 ) ) ;
#82451 = CARTESIAN_POINT ( 'NONE',  ( -1.099225684535947600, 38.70696800326375353, -6.408140936763238038 ) ) ;
#82450 = CARTESIAN_POINT ( 'NONE',  ( -7.116252256160142231, -80.68108970088715637, 2.749999999999193978 ) ) ;
#82453 = CARTESIAN_POINT ( 'NONE',  ( 9.402796353261145157, 14.49999999999999112, -11.68706210897763320 ) ) ;
#82452 = CARTESIAN_POINT ( 'NONE',  ( 1.472469842513823179, 6.425597817667451750, 4.923371831947296329 ) ) ;
#82454 = CARTESIAN_POINT ( 'NONE',  ( 11.44533298127016074, -77.48611261198149691, 4.000000000000000000 ) ) ;
#82455 = MECHANICAL_DESIGN_GEOMETRIC_PRESENTATION_REPRESENTATION (  '', ( #34547 ), #42562 ) ;
#82457 = EDGE_LOOP ( 'NONE', ( #12689, #96828, #94519, #40483 ) ) ;
#82456 = CARTESIAN_POINT ( 'NONE',  ( 1.472469842513823179, 35.59226448433412315, -4.923371831947296329 ) ) ;
#82458 = MECHANICAL_DESIGN_GEOMETRIC_PRESENTATION_REPRESENTATION (  '', ( #28140 ), #61677 ) ;
#82459 = CARTESIAN_POINT ( 'NONE',  ( -1.099225684535947600, 58.70696800326375353, -6.408140936763238038 ) ) ;
#82460 = CARTESIAN_POINT ( 'NONE',  ( 17.85158348494334035, 54.73726573380444194, -6.500000000000027534 ) ) ;
#82461 = CARTESIAN_POINT ( 'NONE',  ( -2.816281873526473856, -0.6680319967362464695, 3.434112377981055619 ) ) ;
#82462 = CARTESIAN_POINT ( 'NONE',  ( -0.8801773607111009756, 13.06368534415483929, 1.068504757029289695E-15 ) ) ;
#82463 = AXIS2_PLACEMENT_3D ( 'NONE', #19115, #50601, #73581 ) ;
#82464 = CARTESIAN_POINT ( 'NONE',  ( 6.204703633549690345, 37.84541550158063927, 14.16423886937410082 ) ) ;
#82465 = UNCERTAINTY_MEASURE_WITH_UNIT (LENGTH_MEASURE( 1.000000000000000082E-05 ), #45837, 'distance_accuracy_value', 'NONE');
#82466 = CARTESIAN_POINT ( 'NONE',  ( 0.000000000000000000, 15.00000000000000000, 0.000000000000000000 ) ) ;
#82467 = CARTESIAN_POINT ( 'NONE',  ( 22.26659068614894466, 23.88708216824730357, 7.082119434687054849 ) ) ;
#82468 = CARTESIAN_POINT ( 'NONE',  ( 6.204703633549690345, 40.76208216824731778, -14.16423886937410259 ) ) ;
#82469 = CARTESIAN_POINT ( 'NONE',  ( 20.36894250292379382, 8.678748834913967869, 10.36894250292379205 ) ) ;
#82471 = CARTESIAN_POINT ( 'NONE',  ( 7.084665262690076126, 67.02201867748817676, -10.88017736071110164 ) ) ;
#82470 = CARTESIAN_POINT ( 'NONE',  ( 20.36894250292379382, 8.678748834913967869, 10.36894250292379205 ) ) ;
#82472 = CARTESIAN_POINT ( 'NONE',  ( 0.5774900079438607392, 48.48035201082150536, 5.440088680355550821 ) ) ;
#82473 = CARTESIAN_POINT ( 'NONE',  ( -5.377205135396049940, 0.2306972965111756257, 13.94000429068777791 ) ) ;
#82474 = ORIENTED_EDGE ( 'NONE', *, *, #37685, .F. ) ;
#82475 = CARTESIAN_POINT ( 'NONE',  ( 1.472469842513823179, 36.42559781766745175, 4.923371831947296329 ) ) ;
#82477 = CARTESIAN_POINT ( 'NONE',  ( 10.00000000000000000, 29.75893115100078745, -9.846743663894594434 ) ) ;
#82476 = CARTESIAN_POINT ( 'NONE',  ( 4.559911319644449179, 63.89701867748817676, 9.422509992056141925 ) ) ;
#82478 = VECTOR ( 'NONE', #19817, 1000.000000000000000 ) ;
#82479 = CARTESIAN_POINT ( 'NONE',  ( 17.96484262340118221, 6.188685344154837509, -7.964842623401177768 ) ) ;
#82480 = CARTESIAN_POINT ( 'NONE',  ( 10.00000000000000000, 57.87363466993042493, -12.81628187352647608 ) ) ;
#82481 = CARTESIAN_POINT ( 'NONE',  ( 14.92337183194729988, 54.34226448433412315, -8.527530157486177487 ) ) ;
#82482 = FILL_AREA_STYLE ('',( #96019 ) ) ;
#82483 = CARTESIAN_POINT ( 'NONE',  ( 10.00000000000000000, 29.75893115100078745, -9.846743663894594434 ) ) ;
#82484 = CARTESIAN_POINT ( 'NONE',  ( 0.6178305044545818747, 38.49863466993042493, -9.382169495545419124 ) ) ;
#82485 = CARTESIAN_POINT ( 'NONE',  ( 12.26659068614894466, -15.27958449841936073, -7.082119434687053960 ) ) ;
#82486 = AXIS2_PLACEMENT_3D ( 'NONE', #78398, #26870, #64852 ) ;
#82487 = CARTESIAN_POINT ( 'NONE',  ( 2.035157376598822676, 37.43868534415484106, -7.964842623401177768 ) ) ;
#82488 = CARTESIAN_POINT ( 'NONE',  ( 5.076628168052703671, 36.84226448433412315, 8.527530157486179263 ) ) ;
#82489 = CARTESIAN_POINT ( 'NONE',  ( 13.79529636645031943, 30.34541550158063927, -14.16423886937409904 ) ) ;
#82490 = ORIENTED_EDGE ( 'NONE', *, *, #30121, .T. ) ;
#82491 = CARTESIAN_POINT ( 'NONE',  ( 2.917880565312950480, 5.970415501580634832, -12.26659068614894821 ) ) ;
#82492 = CARTESIAN_POINT ( 'NONE',  ( 20.88017736071110875, 65.77201867748817676, -2.915334737309920765 ) ) ;
#82493 = DIRECTION ( 'NONE',  ( -0.000000000000000000, -0.000000000000000000, -1.000000000000000000 ) ) ;
#82494 = CARTESIAN_POINT ( 'NONE',  ( 20.36894250292379738, 59.92874883491397497, -10.36894250292379027 ) ) ;
#82495 = CARTESIAN_POINT ( 'NONE',  ( 0.6178305044545818747, 3.498634669930420049, -9.382169495545419124 ) ) ;
#82496 = CARTESIAN_POINT ( 'NONE',  ( 17.39651004071838969, 44.08210964143329846, -6.500000000000027534 ) ) ;
#82497 = CARTESIAN_POINT ( 'NONE',  ( 20.88017736071110519, 55.56368534415484817, 2.639326808657452039E-16 ) ) ;
#82498 = CARTESIAN_POINT ( 'NONE',  ( 1.326515405096035494, 14.76930270348881002, 14.88215077106016437 ) ) ;
#82499 = CARTESIAN_POINT ( 'NONE',  ( -7.964842623401179544, 22.43868534415484817, -7.964842623401174215 ) ) ;
#82500 = CARTESIAN_POINT ( 'NONE',  ( -0.8801773607110991993, 12.85535201082150358, -2.915334737309923874 ) ) ;
#82501 = CARTESIAN_POINT ( 'NONE',  ( 20.88017736071110875, 15.77201867748817143, -2.915334737309920765 ) ) ;
#82502 = CARTESIAN_POINT ( 'NONE',  ( 0.1532563361054083140, 41.00893115100078745, 1.131784320476157264E-15 ) ) ;
#82503 = CARTESIAN_POINT ( 'NONE',  ( 21.09922568453595559, 57.04030133659708923, -6.408140936763230044 ) ) ;
#82504 = CARTESIAN_POINT ( 'NONE',  ( -0.5000000000000073275, 80.99999999999994316, -1.249999999999987121 ) ) ;
#82505 = ORIENTED_EDGE ( 'NONE', *, *, #18638, .T. ) ;
#82506 = AXIS2_PLACEMENT_3D ( 'NONE', #95681, #42676, #27167 ) ;
#82507 = EDGE_CURVE ( 'NONE', #4006, #55254, #33889, .T. ) ;
#82508 = CARTESIAN_POINT ( 'NONE',  ( 20.88017736071110164, 20.35535201082150891, 2.915334737309930979 ) ) ;
#82509 = CARTESIAN_POINT ( 'NONE',  ( 10.00000000000000178, 5.373634669930420493, 12.81628187352647608 ) ) ;
#82510 = DIRECTION ( 'NONE',  ( -0.000000000000000000, -0.000000000000000000, -1.000000000000000000 ) ) ;
#82511 = CARTESIAN_POINT ( 'NONE',  ( 0.1532563361054082862, 6.217264484334118713, 2.638427012816831674 ) ) ;
#82512 = CARTESIAN_POINT ( 'NONE',  ( 14.92337183194729633, 52.67559781766745175, 8.527530157486181039 ) ) ;
#82513 = CARTESIAN_POINT ( 'NONE',  ( 4.559911319644449179, 33.89701867748817676, 9.422509992056141925 ) ) ;
#82514 = AXIS2_PLACEMENT_3D ( 'NONE', #14546, #7545, #38035 ) ;
#82515 = CARTESIAN_POINT ( 'NONE',  ( 6.565887622018943937, 15.16530133659708568, 12.81628187352647430 ) ) ;
#82517 = DIRECTION ( 'NONE',  ( 1.000000000000000000, -0.000000000000000000, 0.000000000000000000 ) ) ;
#82516 = CARTESIAN_POINT ( 'NONE',  ( 20.88017736071110875, 50.77201867748817676, -2.915334737309920765 ) ) ;
#82518 = FACE_OUTER_BOUND ( 'NONE', #15671, .T. ) ;
#82519 = CARTESIAN_POINT ( 'NONE',  ( 22.81628187352648496, 51.83196800326376064, -3.434112377981050290 ) ) ;
#82520 = ORIENTED_EDGE ( 'NONE', *, *, #30312, .F. ) ;
#82521 = FACE_OUTER_BOUND ( 'NONE', #67845, .T. ) ;
#82522 = CARTESIAN_POINT ( 'NONE',  ( 0.6178305044545818747, 38.49863466993042493, -9.382169495545419124 ) ) ;
#82523 = CARTESIAN_POINT ( 'NONE',  ( 17.20831665107776587, 7.883931151000784787, 7.208316651077764980 ) ) ;
#82524 = CARTESIAN_POINT ( 'NONE',  ( 20.88017736071110875, 35.77201867748816966, -2.915334737309920765 ) ) ;
#82525 = CARTESIAN_POINT ( 'NONE',  ( 0.1532563361054083140, 66.00893115100079456, 1.131784320476157264E-15 ) ) ;
#82526 = CARTESIAN_POINT ( 'NONE',  ( 2.791683348922240793, 51.63393115100078745, 7.208316651077764092 ) ) ;
#82527 = CARTESIAN_POINT ( 'NONE',  ( 17.20831665107776587, 14.13393115100078568, -7.208316651077762316 ) ) ;
#82528 = CARTESIAN_POINT ( 'NONE',  ( 14.92337183194729633, 2.675597817667451750, 8.527530157486181039 ) ) ;
#82529 = CARTESIAN_POINT ( 'NONE',  ( 24.16423886937409904, 49.09541550158063217, 3.795296366450317205 ) ) ;
#82530 = CARTESIAN_POINT ( 'NONE',  ( 34.56412365047464874, 11.49999999999999645, 10.00000000000000000 ) ) ;
#82531 = CARTESIAN_POINT ( 'NONE',  ( -6.868018881919620178, -58.39307134327821558, -3.999999999999999556 ) ) ;
#82532 = ORIENTED_EDGE ( 'NONE', *, *, #26313, .T. ) ;
#82533 = VERTEX_POINT ( 'NONE', #27344 ) ;
#82534 = CARTESIAN_POINT ( 'NONE',  ( 20.36894250292379382, 63.67874883491396787, 10.36894250292379205 ) ) ;
#82536 = EDGE_CURVE ( 'NONE', #41530, #8435, #80355, .T. ) ;
#82535 = CARTESIAN_POINT ( 'NONE',  ( 22.26659068614895176, 64.72041550158064638, -7.082119434687042414 ) ) ;
#82537 = CARTESIAN_POINT ( 'NONE',  ( 18.52753015748618282, 28.92559781766745175, -4.923371831947291888 ) ) ;
#82538 = CARTESIAN_POINT ( 'NONE',  ( 6.565887622018943937, 23.08196800326375708, -12.81628187352647608 ) ) ;
#82539 = CARTESIAN_POINT ( 'NONE',  ( 4.391347328463013788, 14.76984910450983257, -14.28069739540080896 ) ) ;
#82541 = CARTESIAN_POINT ( 'NONE',  ( 24.16423886937409904, 4.095415501580634832, 3.795296366450317205 ) ) ;
#82540 = CARTESIAN_POINT ( 'NONE',  ( 0.000000000000000000, 14.49999999999999822, 0.000000000000000000 ) ) ;
#82542 = CARTESIAN_POINT ( 'NONE',  ( 2.035157376598824452, 8.688685344154839285, 7.964842623401179544 ) ) ;
#82543 = CARTESIAN_POINT ( 'NONE',  ( -4.164238869374099039, 56.80374883491397497, 8.674139862899312516E-16 ) ) ;
#82544 = AXIS2_PLACEMENT_3D ( 'NONE', #46673, #83701, #54170 ) ;
#82545 = CARTESIAN_POINT ( 'NONE',  ( 0.1532563361054100626, 25.80059781766744820, -2.638427012816831230 ) ) ;
#82546 = EDGE_CURVE ( 'NONE', #22102, #45519, #35836, .T. ) ;
#82547 = CARTESIAN_POINT ( 'NONE',  ( -10.14667048435128294, 15.00000000000000000, -10.35833375027054082 ) ) ;
#82548 = CARTESIAN_POINT ( 'NONE',  ( 18.52753015748617571, 18.09226448433411960, 4.923371831947298993 ) ) ;
#82549 = DIRECTION ( 'NONE',  ( 0.000000000000000000, 0.000000000000000000, 1.000000000000000000 ) ) ;
#82550 = CARTESIAN_POINT ( 'NONE',  ( 2.638427012816829897, 14.55059781766744997, -9.846743663894592657 ) ) ;
#82551 = ORIENTED_EDGE ( 'NONE', *, *, #91077, .T. ) ;
#82552 = ORIENTED_EDGE ( 'NONE', *, *, #30255, .F. ) ;
#82553 = CYLINDRICAL_SURFACE ( 'NONE', #9466, 2.999999999999997780 ) ;
#82554 = ORIENTED_EDGE ( 'NONE', *, *, #15404, .F. ) ;
#82556 = CARTESIAN_POINT ( 'NONE',  ( 19.84674366389459266, 48.30059781766745175, 2.638427012816836559 ) ) ;
#82555 = VECTOR ( 'NONE', #9941, 1000.000000000000114 ) ;
#82557 = CARTESIAN_POINT ( 'NONE',  ( 17.08211943468705130, 18.47041550158063572, 12.26659068614894998 ) ) ;
#82559 = CARTESIAN_POINT ( 'NONE',  ( 4.559911319644449179, 43.89701867748816966, 9.422509992056141925 ) ) ;
#82558 = CARTESIAN_POINT ( 'NONE',  ( 0.5774900079438607392, 23.48035201082150536, 5.440088680355550821 ) ) ;
#82561 = CARTESIAN_POINT ( 'NONE',  ( 22.81628187352648496, 21.83196800326374643, -3.434112377981050290 ) ) ;
#82560 = CARTESIAN_POINT ( 'NONE',  ( -15.00000000000004974, 91.25000000000000000, -8.000000000000000000 ) ) ;
#82562 = CARTESIAN_POINT ( 'NONE',  ( 13.79529636645030344, 8.262082168247300018, 14.16423886937410614 ) ) ;
#82563 = CARTESIAN_POINT ( 'NONE',  ( 17.96484262340118221, 64.93868534415483396, 7.964842623401181321 ) ) ;
#82564 = AXIS2_PLACEMENT_3D ( 'NONE', #90567, #39067, #14602 ) ;
#82565 = PRESENTATION_LAYER_ASSIGNMENT (  '', '', ( #72981 ) ) ;
#82566 = CARTESIAN_POINT ( 'NONE',  ( -2.816281873526473856, 34.33196800326376064, 3.434112377981055619 ) ) ;
#82567 = ORIENTED_EDGE ( 'NONE', *, *, #62672, .F. ) ;
#82568 = CARTESIAN_POINT ( 'NONE',  ( 12.63842701281683922, 34.55059781766745886, -9.846743663894590881 ) ) ;
#82569 = CARTESIAN_POINT ( 'NONE',  ( 10.00000000000000000, 6.813685344154838397, -10.88017736071110342 ) ) ;
#82570 = ORIENTED_EDGE ( 'NONE', *, *, #53750, .F. ) ;
#82571 = CARTESIAN_POINT ( 'NONE',  ( -4.164238869374098151, 66.59541550158060375, -3.795296366450310543 ) ) ;
#82572 = ORIENTED_EDGE ( 'NONE', *, *, #49123, .T. ) ;
#82573 = CARTESIAN_POINT ( 'NONE',  ( 19.42250999205614548, 45.98035201082150536, -5.440088680355545492 ) ) ;
#82574 = CARTESIAN_POINT ( 'NONE',  ( 20.88017736071110875, 60.77201867748817676, -2.915334737309920765 ) ) ;
#82575 = CARTESIAN_POINT ( 'NONE',  ( 7.084665262690076126, 67.02201867748817676, -10.88017736071110164 ) ) ;
#82576 = CARTESIAN_POINT ( 'NONE',  ( 12.91533473730993009, 56.60535201082151247, -10.88017736071109987 ) ) ;
#82577 = CARTESIAN_POINT ( 'NONE',  ( -0.1034006766853582671, 15.00000000000000000, 14.49963131601234956 ) ) ;
#82579 = EDGE_LOOP ( 'NONE', ( #61011, #78662, #48444, #64203 ) ) ;
#82578 = CARTESIAN_POINT ( 'NONE',  ( 10.95672398092087718, -56.81605919574143826, 4.000000000000000888 ) ) ;
#82580 = CARTESIAN_POINT ( 'NONE',  ( 10.00000000000000178, 32.25893115100078745, 9.846743663894594434 ) ) ;
#82581 = ORIENTED_EDGE ( 'NONE', *, *, #36141, .T. ) ;
#82582 = CARTESIAN_POINT ( 'NONE',  ( 0.1532563361054082862, 61.21726448433412315, 2.638427012816831674 ) ) ;
#82583 = DIRECTION ( 'NONE',  ( 0.000000000000000000, 0.000000000000000000, 1.000000000000000000 ) ) ;
#82584 = CARTESIAN_POINT ( 'NONE',  ( -0.3689425029237898834, 1.178748834913967869, -10.36894250292378850 ) ) ;
#82585 = ORIENTED_EDGE ( 'NONE', *, *, #79818, .F. ) ;
#82586 = CARTESIAN_POINT ( 'NONE',  ( -11.28404003980378612, 12.70269222139743803, -2.038315274784799236 ) ) ;
#82587 = CARTESIAN_POINT ( 'NONE',  ( 0.000000000000000000, 15.00000000000000000, 0.000000000000000000 ) ) ;
#82588 = CARTESIAN_POINT ( 'NONE',  ( 20.00000000000000355, 70.00000000000000000, 6.500000000000000888 ) ) ;
#82589 = CARTESIAN_POINT ( 'NONE',  ( 20.88017736071110164, 5.355352010821503583, 2.915334737309930979 ) ) ;
#82590 = LINE ( 'NONE', #98108, #65833 ) ;
#82591 = CARTESIAN_POINT ( 'NONE',  ( -8.731067818237036704, 4.063309369127505732, -8.731067818237033151 ) ) ;
#82592 = CARTESIAN_POINT ( 'NONE',  ( 10.00000000000000000, 39.75893115100078745, -9.846743663894594434 ) ) ;
#82593 = CARTESIAN_POINT ( 'NONE',  ( -13.34343830728408697, 14.49999999999999822, 6.852200678592504701 ) ) ;
#82594 = CARTESIAN_POINT ( 'NONE',  ( 0.6178305044545818747, 18.49863466993041428, -9.382169495545419124 ) ) ;
#82595 = CARTESIAN_POINT ( 'NONE',  ( 0.1532563361054082862, 6.217264484334118713, 2.638427012816831674 ) ) ;
#82596 = CARTESIAN_POINT ( 'NONE',  ( -4.000000000000000000, 10.00000000000000000, 2.500000000000000000 ) ) ;
#82597 = CARTESIAN_POINT ( 'NONE',  ( 2.791683348922240793, 16.63393115100078745, 7.208316651077764092 ) ) ;
#82598 = CARTESIAN_POINT ( 'NONE',  ( 10.00000000000000178, 5.373634669930420493, 12.81628187352647608 ) ) ;
#82599 = CARTESIAN_POINT ( 'NONE',  ( -0.5000000000000073275, 80.99999999999994316, 1.249999999999987121 ) ) ;
#82600 = ORIENTED_EDGE ( 'NONE', *, *, #45704, .F. ) ;
#82601 = ORIENTED_EDGE ( 'NONE', *, *, #95856, .T. ) ;
#82602 = CARTESIAN_POINT ( 'NONE',  ( 10.00000000000000178, 29.31368534415483751, 10.88017736071110342 ) ) ;
#82603 = CARTESIAN_POINT ( 'NONE',  ( 22.26659068614895176, 24.72041550158063572, -7.082119434687042414 ) ) ;
#82604 = CARTESIAN_POINT ( 'NONE',  ( 19.84674366389459266, 33.30059781766744464, 2.638427012816836559 ) ) ;
#82605 = CARTESIAN_POINT ( 'NONE',  ( 12.91533473730992121, 59.52201867748816966, 10.88017736071110164 ) ) ;
#82607 = CARTESIAN_POINT ( 'NONE',  ( -3.635384400432159158, -3.854802480546752896, -2.750000000000000444 ) ) ;
#82606 = CARTESIAN_POINT ( 'NONE',  ( -1.099225684535947600, 33.70696800326375353, -6.408140936763238038 ) ) ;
#82608 = CARTESIAN_POINT ( 'NONE',  ( 20.88017736071110875, 10.77201867748817143, -2.915334737309920765 ) ) ;
#82609 = CARTESIAN_POINT ( 'NONE',  ( 0.000000000000000000, 0.000000000000000000, 0.000000000000000000 ) ) ;
#82610 = DIRECTION ( 'NONE',  ( -0.9366721892483995671, 0.000000000000000000, 0.3502073812594621027 ) ) ;
#82611 = VECTOR ( 'NONE', #16765, 1000.000000000000000 ) ;
#82612 = CARTESIAN_POINT ( 'NONE',  ( 10.00000000000000000, 12.87363466993042138, -12.81628187352647608 ) ) ;
#82613 = CARTESIAN_POINT ( 'NONE',  ( 10.00000000000000000, -2.126365330069579951, -12.81628187352647608 ) ) ;
#82614 = CARTESIAN_POINT ( 'NONE',  ( 7.361572987183170547, 27.05059781766745175, 9.846743663894590881 ) ) ;
#82615 = CARTESIAN_POINT ( 'NONE',  ( -2.915334737309917656, -10.89464798917849286, 10.88017736071110164 ) ) ;
#82616 = CARTESIAN_POINT ( 'NONE',  ( 16.40814093676323893, 35.79030133659708923, 11.09922568453595026 ) ) ;
#82617 = CARTESIAN_POINT ( 'NONE',  ( 14.49440716394873618, 4.800686736885023475E-16, -0.4026921475166205244 ) ) ;
#82619 = CARTESIAN_POINT ( 'NONE',  ( -3.750000000000000000, 10.25000000000000000, 2.500000000000000000 ) ) ;
#82618 = CARTESIAN_POINT ( 'NONE',  ( 12.91533473730993009, 36.60535201082151247, -10.88017736071109987 ) ) ;
#82620 = EDGE_CURVE ( 'NONE', #49181, #60398, #10022, .T. ) ;
#82621 = CIRCLE ( 'NONE', #7576, 15.00000000000000000 ) ;
#82622 = LINE ( 'NONE', #74624, #80040 ) ;
#82623 = CARTESIAN_POINT ( 'NONE',  ( 4.559911319644449179, 62.23035201082150536, -9.422509992056141925 ) ) ;
#82624 = AXIS2_PLACEMENT_3D ( 'NONE', #64311, #81301, #35300 ) ;
#82625 = CARTESIAN_POINT ( 'NONE',  ( 10.00000000000000178, 44.31368534415484106, 10.88017736071110342 ) ) ;
#82626 = CARTESIAN_POINT ( 'NONE',  ( -0.8801773607110991993, 42.85535201082150536, -2.915334737309923874 ) ) ;
#82627 = CARTESIAN_POINT ( 'NONE',  ( 14.92337183194729633, 62.67559781766745886, 8.527530157486181039 ) ) ;
#82628 = CARTESIAN_POINT ( 'NONE',  ( 19.42250999205614548, 55.98035201082150536, -5.440088680355545492 ) ) ;
#82629 = CARTESIAN_POINT ( 'NONE',  ( 17.20831665107776587, 42.88393115100077324, 7.208316651077764980 ) ) ;
#82630 = CARTESIAN_POINT ( 'NONE',  ( 20.88017736071110164, 15.35535201082150358, 2.915334737309930979 ) ) ;
#82631 = CARTESIAN_POINT ( 'NONE',  ( 10.00000000000000000, 7.873634669930421381, -12.81628187352647608 ) ) ;
#82632 = ORIENTED_EDGE ( 'NONE', *, *, #72028, .T. ) ;
#82633 = CARTESIAN_POINT ( 'NONE',  ( 20.88017736071110875, 25.77201867748816966, -2.915334737309920765 ) ) ;
#82634 =( NAMED_UNIT ( * ) PLANE_ANGLE_UNIT ( ) SI_UNIT ( $, .RADIAN. ) );
#82635 = CARTESIAN_POINT ( 'NONE',  ( 2.035157376598822676, 2.438685344154837953, -7.964842623401177768 ) ) ;
#82636 = CARTESIAN_POINT ( 'NONE',  ( 20.88017736071110164, 30.35535201082151247, 2.915334737309930979 ) ) ;
#82637 = CARTESIAN_POINT ( 'NONE',  ( -0.8801773607111009756, 68.06368534415484817, 1.068504757029289695E-15 ) ) ;
#82638 = CARTESIAN_POINT ( 'NONE',  ( 10.00000000000000178, 43.05374883491397497, 14.16423886937410082 ) ) ;
#82639 = CARTESIAN_POINT ( 'NONE',  ( 14.92337183194729988, 14.34226448433411782, -8.527530157486177487 ) ) ;
#82640 = CARTESIAN_POINT ( 'NONE',  ( 2.035157376598822676, 42.43868534415483396, -7.964842623401177768 ) ) ;
#82641 = CARTESIAN_POINT ( 'NONE',  ( 9.065164099344587001, 14.49999999999999112, -11.95084933600771038 ) ) ;
#82642 = CARTESIAN_POINT ( 'NONE',  ( 6.204703633549690345, 2.845415501580634388, 14.16423886937410082 ) ) ;
#82643 = ORIENTED_EDGE ( 'NONE', *, *, #62342, .F. ) ;
#82644 = CARTESIAN_POINT ( 'NONE',  ( -0.3093388210927642268, 0.5000000000000004441, 14.99680997725065978 ) ) ;
#82645 = CARTESIAN_POINT ( 'NONE',  ( 10.00000000000000000, 64.75893115100078035, -9.846743663894594434 ) ) ;
#82646 = ORIENTED_EDGE ( 'NONE', *, *, #13814, .F. ) ;
#82647 = ORIENTED_EDGE ( 'NONE', *, *, #5766, .T. ) ;
#82648 = CARTESIAN_POINT ( 'NONE',  ( 24.16423886937409904, 24.09541550158063927, 3.795296366450317205 ) ) ;
#82650 = EDGE_CURVE ( 'NONE', #90281, #31231, #96424, .T. ) ;
#82649 = CARTESIAN_POINT ( 'NONE',  ( 20.36894250292379382, 23.67874883491397142, 10.36894250292379205 ) ) ;
#82651 = CARTESIAN_POINT ( 'NONE',  ( 2.035157376598824452, 58.68868534415482685, 7.964842623401179544 ) ) ;
#82652 = CARTESIAN_POINT ( 'NONE',  ( -2.266590686148945544, 67.22041550158063217, 7.082119434687048631 ) ) ;
#82653 = CARTESIAN_POINT ( 'NONE',  ( 0.6178305044545818747, 3.498634669930420049, -9.382169495545419124 ) ) ;
#82654 = CARTESIAN_POINT ( 'NONE',  ( 0.1532563361054083140, 46.00893115100079456, 1.131784320476157264E-15 ) ) ;
#82655 = FILL_AREA_STYLE_COLOUR ( '', #62624 ) ;
#82657 = CARTESIAN_POINT ( 'NONE',  ( 19.38216949554541557, 7.248634669930421381, -9.382169495545420901 ) ) ;
#82656 = CARTESIAN_POINT ( 'NONE',  ( 20.88017736071110164, 50.35535201082151247, 2.915334737309930979 ) ) ;
#82658 = CARTESIAN_POINT ( 'NONE',  ( -0.3689425029237881626, 17.42874883491397142, 10.36894250292379027 ) ) ;
#82659 = CARTESIAN_POINT ( 'NONE',  ( 0.5774900079438607392, 8.480352010821505360, 5.440088680355550821 ) ) ;
#82660 = CARTESIAN_POINT ( 'NONE',  ( 17.96484262340118221, 16.18868534415483396, -7.964842623401177768 ) ) ;
#82661 = DIRECTION ( 'NONE',  ( 0.09584575252023383451, 0.000000000000000000, -0.9953961983671779645 ) ) ;
#82662 = CARTESIAN_POINT ( 'NONE',  ( 12.91533473730992121, 39.52201867748817676, 10.88017736071110164 ) ) ;
#82663 = CIRCLE ( 'NONE', #36336, 14.49999999999999822 ) ;
#82664 = CARTESIAN_POINT ( 'NONE',  ( -2.638427012816840111, -25.03273551566587685, -9.846743663894590881 ) ) ;
#82665 = EDGE_LOOP ( 'NONE', ( #20319, #40628, #43316, #33596 ) ) ;
#82666 = CARTESIAN_POINT ( 'NONE',  ( 13.61464873478162652, 0.5000000000000004441, 6.296136897217931683 ) ) ;
#82667 = VERTEX_POINT ( 'NONE', #42363 ) ;
#82668 = CARTESIAN_POINT ( 'NONE',  ( 0.1532563361054083140, 31.00893115100078390, 1.131784320476157264E-15 ) ) ;
#82669 = EDGE_LOOP ( 'NONE', ( #16625, #35588, #37883, #40263, #69136, #46158 ) ) ;
#82670 = CARTESIAN_POINT ( 'NONE',  ( -11.22915323889568562, 15.00000000000000000, -8.773176023390764300 ) ) ;
#82672 = CARTESIAN_POINT ( 'NONE',  ( 10.00000000000000178, 9.313685344154839285, 10.88017736071110342 ) ) ;
#82671 = CARTESIAN_POINT ( 'NONE',  ( 20.36894250292379738, 39.92874883491396787, -10.36894250292379027 ) ) ;
#82674 = CARTESIAN_POINT ( 'NONE',  ( 18.52753015748617571, 43.09226448433412315, 4.923371831947298993 ) ) ;
#82673 = CARTESIAN_POINT ( 'NONE',  ( 19.84674366389459266, 23.71726448433412315, -2.638427012816827677 ) ) ;
#82675 = CARTESIAN_POINT ( 'NONE',  ( 3.927832320392247389, 15.00000000000000000, -13.69797916712104602 ) ) ;
#82676 = AXIS2_PLACEMENT_3D ( 'NONE', #9222, #93202, #61716 ) ;
#82677 = CARTESIAN_POINT ( 'NONE',  ( 2.035157376598822676, 67.43868534415484817, -7.964842623401177768 ) ) ;
#82678 = CARTESIAN_POINT ( 'NONE',  ( 9.382169495545415572, 17.24863466993042138, -9.382169495545422677 ) ) ;
#82679 = ORIENTED_EDGE ( 'NONE', *, *, #88474, .T. ) ;
#82680 = CARTESIAN_POINT ( 'NONE',  ( 24.16423886937410614, 34.51208216824731068, -3.795296366450302550 ) ) ;
#82681 = ORIENTED_EDGE ( 'NONE', *, *, #76164, .F. ) ;
#82682 = CARTESIAN_POINT ( 'NONE',  ( -2.816281873526471635, 28.91530133659708213, -3.434112377981056508 ) ) ;
#82683 = ORIENTED_EDGE ( 'NONE', *, *, #59050, .T. ) ;
#82684 = CARTESIAN_POINT ( 'NONE',  ( 10.00000000000000000, 62.87363466993042493, -12.81628187352647608 ) ) ;
#82685 = COLOUR_RGB ( '', 0.08235294, 0.09019608, 0.10196078) ;
#82686 = EDGE_CURVE ( 'NONE', #37189, #28474, #78750, .T. ) ;
#82687 = CARTESIAN_POINT ( 'NONE',  ( 0.1532563361054100626, 40.80059781766745886, -2.638427012816831230 ) ) ;
#82688 = CARTESIAN_POINT ( 'NONE',  ( 4.559911319644449179, 27.23035201082150536, -9.422509992056141925 ) ) ;
#82689 = LINE ( 'NONE', #89205, #27168 ) ;
#82690 = CARTESIAN_POINT ( 'NONE',  ( 19.84674366389459621, 43.50893115100078745, 7.409399052514197653E-17 ) ) ;
#82691 = CARTESIAN_POINT ( 'NONE',  ( 2.791683348922237240, 50.38393115100078035, -7.208316651077763204 ) ) ;
#82692 = EDGE_CURVE ( 'NONE', #92445, #12912, #38785, .T. ) ;
#82693 = AXIS2_PLACEMENT_3D ( 'NONE', #93671, #86182, #39707 ) ;
#82694 = VECTOR ( 'NONE', #26699, 1000.000000000000000 ) ;
#82695 = ORIENTED_EDGE ( 'NONE', *, *, #85924, .F. ) ;
#82696 = CARTESIAN_POINT ( 'NONE',  ( 0.000000000000000000, 0.000000000000000000, 0.000000000000000000 ) ) ;
#82697 = CARTESIAN_POINT ( 'NONE',  ( -9.000000000000000000, 75.76920769491746910, -2.900000000000000799 ) ) ;
#82698 = CARTESIAN_POINT ( 'NONE',  ( -10.58521204051718101, 15.00000000000000000, -11.99294302885424024 ) ) ;
#82699 = CARTESIAN_POINT ( 'NONE',  ( 5.076628168052703671, 11.84226448433411960, 8.527530157486179263 ) ) ;
#82700 = CARTESIAN_POINT ( 'NONE',  ( 6.565887622018943937, 35.16530133659708923, 12.81628187352647430 ) ) ;
#82701 = DIRECTION ( 'NONE',  ( -0.000000000000000000, -1.000000000000000000, -0.000000000000000000 ) ) ;
#82702 = ORIENTED_EDGE ( 'NONE', *, *, #8576, .T. ) ;
#82703 = CARTESIAN_POINT ( 'NONE',  ( 1.472469842513823179, 56.42559781766745886, 4.923371831947296329 ) ) ;
#82704 = FACE_OUTER_BOUND ( 'NONE', #11733, .T. ) ;
#82705 = CARTESIAN_POINT ( 'NONE',  ( 0.1532563361054100626, 35.80059781766745175, -2.638427012816831230 ) ) ;
#82706 = CARTESIAN_POINT ( 'NONE',  ( 6.204703633549690345, 40.76208216824731778, -14.16423886937410259 ) ) ;
#82707 = CARTESIAN_POINT ( 'NONE',  ( 2.791683348922237240, 50.38393115100078035, -7.208316651077763204 ) ) ;
#82708 = CARTESIAN_POINT ( 'NONE',  ( 19.38216949554541557, 42.24863466993041783, -9.382169495545420901 ) ) ;
#82710 = FACE_OUTER_BOUND ( 'NONE', #33931, .T. ) ;
#82709 = CARTESIAN_POINT ( 'NONE',  ( -9.399392868737892925, 15.00000000000000000, 11.04089732309468097 ) ) ;
#82711 = CARTESIAN_POINT ( 'NONE',  ( 12.63842701281683034, 12.46726448433411782, 9.846743663894596210 ) ) ;
#82712 = LINE ( 'NONE', #20737, #77532 ) ;
#82713 = CARTESIAN_POINT ( 'NONE',  ( 17.20831665107776587, 54.13393115100079456, -7.208316651077762316 ) ) ;
#82714 = CARTESIAN_POINT ( 'NONE',  ( 20.88017736071110875, 35.77201867748816966, -2.915334737309920765 ) ) ;
#82715 = CARTESIAN_POINT ( 'NONE',  ( 66.56412365047464164, 14.00000000000000888, 10.00000000000000000 ) ) ;
#82716 = B_SPLINE_CURVE_WITH_KNOTS ( 'NONE', 3,
 ( #50904, #7398, #37896, #53365, #92841, #23386 ),
 .UNSPECIFIED., .F., .F.,
 ( 4, 2, 4 ),
 ( 3.409110551495873193E-05, 0.0004400426677367972510, 0.0008459942299586357701 ),
 .UNSPECIFIED. ) ;
#82717 = CARTESIAN_POINT ( 'NONE',  ( -0.8801773607110991993, 42.85535201082150536, -2.915334737309923874 ) ) ;
#82718 = ORIENTED_EDGE ( 'NONE', *, *, #39741, .F. ) ;
#82719 = DIRECTION ( 'NONE',  ( 0.000000000000000000, 0.000000000000000000, -1.000000000000000000 ) ) ;
#82720 = CARTESIAN_POINT ( 'NONE',  ( 19.42250999205614548, 20.98035201082150891, -5.440088680355545492 ) ) ;
#82722 = CARTESIAN_POINT ( 'NONE',  ( 4.559911319644449179, 48.89701867748817676, 9.422509992056141925 ) ) ;
#82721 = CARTESIAN_POINT ( 'NONE',  ( 0.1532563361054083140, 66.00893115100079456, 1.131784320476157264E-15 ) ) ;
#82723 = SURFACE_STYLE_FILL_AREA ( #36744 ) ;
#82724 = CARTESIAN_POINT ( 'NONE',  ( 17.96484262340118221, 54.93868534415484106, 7.964842623401181321 ) ) ;
#82725 = CARTESIAN_POINT ( 'NONE',  ( 11.92686044187656691, 5.162123368507804955, -2.602085213965210642E-15 ) ) ;
#82727 = CARTESIAN_POINT ( 'NONE',  ( 3.558677480090426837, 70.40124509038876965, -12.00000000000000000 ) ) ;
#82726 = CARTESIAN_POINT ( 'NONE',  ( 7.084665262690076126, 34.10535201082151247, 10.88017736071109987 ) ) ;
#82728 = CARTESIAN_POINT ( 'NONE',  ( 14.92337183194729633, 7.675597817667451750, 8.527530157486181039 ) ) ;
#82729 = CARTESIAN_POINT ( 'NONE',  ( 18.52753015748618282, 23.92559781766745530, -4.923371831947291888 ) ) ;
#82730 = CARTESIAN_POINT ( 'NONE',  ( 20.03447792253738768, 57.65514106990691090, -6.401564815979734924 ) ) ;
#82731 = CARTESIAN_POINT ( 'NONE',  ( -3.795296366450300773, 17.84541550158062861, 14.16423886937410437 ) ) ;
#82732 = CARTESIAN_POINT ( 'NONE',  ( 0.6178305044545838731, -0.2513653300695798953, 9.382169495545420901 ) ) ;
#82733 = B_SPLINE_CURVE_WITH_KNOTS ( 'NONE', 3,
 ( #62176, #9195, #2707, #40682, #48658, #70195 ),
 .UNSPECIFIED., .F., .F.,
 ( 4, 2, 4 ),
 ( 6.254634441385501517E-18, 0.0002605067024380970848, 0.0005210134048761879896 ),
 .UNSPECIFIED. ) ;
#82734 = CARTESIAN_POINT ( 'NONE',  ( 13.79529636645031943, 60.34541550158063927, -14.16423886937409904 ) ) ;
#82735 =( LENGTH_UNIT ( ) NAMED_UNIT ( * ) SI_UNIT ( .MILLI., .METRE. ) );
#82736 = CARTESIAN_POINT ( 'NONE',  ( 6.204703633549690345, 27.84541550158063217, 14.16423886937410082 ) ) ;
#82737 = EDGE_CURVE ( 'NONE', #87966, #37275, #73716, .T. ) ;
#82738 = CARTESIAN_POINT ( 'NONE',  ( 6.204703633549690345, 45.76208216824729647, -14.16423886937410259 ) ) ;
#82739 = CARTESIAN_POINT ( 'NONE',  ( 20.88017736071110164, 5.355352010821502695, 2.915334737309930979 ) ) ;
#82740 = ORIENTED_EDGE ( 'NONE', *, *, #77235, .F. ) ;
#82741 = CARTESIAN_POINT ( 'NONE',  ( 10.00000000000000000, 24.75893115100078745, -9.846743663894594434 ) ) ;
#82742 = CARTESIAN_POINT ( 'NONE',  ( 0.5774900079438607392, 18.48035201082150536, 5.440088680355550821 ) ) ;
#82743 = EDGE_CURVE ( 'NONE', #17129, #21583, #67720, .T. ) ;
#82744 = CARTESIAN_POINT ( 'NONE',  ( 0.1532563361054083140, 51.00893115100078745, 1.131784320476157264E-15 ) ) ;
#82746 = DIRECTION ( 'NONE',  ( -1.000000000000000000, 5.818595309480552676E-17, -0.000000000000000000 ) ) ;
#82745 = DIRECTION ( 'NONE',  ( 0.9999619230641713097, 0.000000000000000000, 0.008726535498374266009 ) ) ;
#82747 = CYLINDRICAL_SURFACE ( 'NONE', #79088, 15.00000000000000000 ) ;
#82748 = CARTESIAN_POINT ( 'NONE',  ( 2.863845842055826818, 0.04922511925147237538, 14.47219703936415591 ) ) ;
#82749 = CARTESIAN_POINT ( 'NONE',  ( -2.816281873526473856, 39.33196800326374643, 3.434112377981055619 ) ) ;
#82750 = CARTESIAN_POINT ( 'NONE',  ( 0.1532563361054082862, 46.21726448433411605, 2.638427012816831674 ) ) ;
#82751 = ORIENTED_EDGE ( 'NONE', *, *, #87605, .F. ) ;
#82752 = CARTESIAN_POINT ( 'NONE',  ( 19.84674366389459621, 13.50893115100078568, 7.409399052514197653E-17 ) ) ;
#82753 = CARTESIAN_POINT ( 'NONE',  ( 17.85999999999999943, 37.99999999999997868, -9.500000000000000000 ) ) ;
#82754 = CARTESIAN_POINT ( 'NONE',  ( 19.42250999205614193, 10.14701867748816966, 5.440088680355555262 ) ) ;
#82755 = CARTESIAN_POINT ( 'NONE',  ( 17.08211943468705130, 58.47041550158063927, 12.26659068614894998 ) ) ;
#82756 = CARTESIAN_POINT ( 'NONE',  ( 20.88017736071110164, 45.35535201082149115, 2.915334737309930979 ) ) ;
#82757 = CIRCLE ( 'NONE', #6100, 7.000000000000002665 ) ;
#82758 = CARTESIAN_POINT ( 'NONE',  ( 10.00000000000000000, 56.81368534415484106, -10.88017736071110342 ) ) ;
#82759 = CARTESIAN_POINT ( 'NONE',  ( 20.24186590665276952, 39.73410085661203794, 6.114288769123060518 ) ) ;
#82760 = CARTESIAN_POINT ( 'NONE',  ( 2.791683348922240793, 26.63393115100078745, 7.208316651077764092 ) ) ;
#82761 = CARTESIAN_POINT ( 'NONE',  ( 20.88017736071110875, 10.77201867748817143, -2.915334737309920765 ) ) ;
#82762 = CARTESIAN_POINT ( 'NONE',  ( 19.84674366389459266, 8.717264484334116048, -2.638427012816827677 ) ) ;
#82763 = PRESENTATION_STYLE_ASSIGNMENT (( #52267 ) ) ;
#82764 = CARTESIAN_POINT ( 'NONE',  ( 7.361572987183169658, 39.96726448433411605, -9.846743663894592657 ) ) ;
#82765 = CARTESIAN_POINT ( 'NONE',  ( 2.035157376598824452, 33.68868534415484106, 7.964842623401179544 ) ) ;
#82766 = AXIS2_PLACEMENT_3D ( 'NONE', #89288, #50289, #50801 ) ;
#82767 = CIRCLE ( 'NONE', #84352, 0.2500000000000002220 ) ;
#82768 = B_SPLINE_CURVE_WITH_KNOTS ( 'NONE', 3,
 ( #65923, #96451, #58415, #27923, #90392, #6917 ),
 .UNSPECIFIED., .F., .F.,
 ( 4, 2, 4 ),
 ( 0.0002800452451301706442, 0.0006862509172429716916, 0.001092456589355772847 ),
 .UNSPECIFIED. ) ;
#82769 = ORIENTED_EDGE ( 'NONE', *, *, #4764, .F. ) ;
#82770 = CARTESIAN_POINT ( 'NONE',  ( 16.40814093676324603, 62.45696800326376064, -11.09922568453594671 ) ) ;
#82772 = EDGE_CURVE ( 'NONE', #87018, #28474, #43332, .T. ) ;
#82771 = CARTESIAN_POINT ( 'NONE',  ( 8.235571585149870089, 6.046802177851540172, -8.235571585149873641 ) ) ;
#82773 = CARTESIAN_POINT ( 'NONE',  ( 2.791683348922237240, 5.383931151000785675, -7.208316651077763204 ) ) ;
#82774 = CARTESIAN_POINT ( 'NONE',  ( -2.816281873526473856, 49.12363466993042493, 9.499525473075851096E-16 ) ) ;
#82776 = CARTESIAN_POINT ( 'NONE',  ( 17.20831665107776587, 39.13393115100079456, -7.208316651077762316 ) ) ;
#82775 = CARTESIAN_POINT ( 'NONE',  ( 2.035157376598822676, 7.438685344154837509, -7.964842623401177768 ) ) ;
#82777 = DIRECTION ( 'NONE',  ( 8.659560562354910671E-17, -0.7071067811865492381, 0.7071067811865457964 ) ) ;
#82778 = CARTESIAN_POINT ( 'NONE',  ( 6.000000000000000000, 60.50000000000000000, -6.000000000000000000 ) ) ;
#82779 = CARTESIAN_POINT ( 'NONE',  ( 13.79529636645030344, 33.26208216824730357, 14.16423886937410614 ) ) ;
#82780 = CARTESIAN_POINT ( 'NONE',  ( -0.3689425029237898834, 41.17874883491397497, -10.36894250292378850 ) ) ;
#82781 = CARTESIAN_POINT ( 'NONE',  ( 17.20831665107776587, 54.13393115100079456, -7.208316651077762316 ) ) ;
#82782 = DIRECTION ( 'NONE',  ( 1.000000000000000000, 1.850371707708593182E-14, 0.000000000000000000 ) ) ;
#82783 = CARTESIAN_POINT ( 'NONE',  ( -0.8801773607111009756, 33.06368534415484106, 1.068504757029289695E-15 ) ) ;
#82784 = ADVANCED_FACE ( 'NONE', ( #52805 ), #67544, .T. ) ;
#82785 = CARTESIAN_POINT ( 'NONE',  ( 0.5774900079438590739, 67.64701867748817676, -5.440088680355550821 ) ) ;
#82786 = ORIENTED_EDGE ( 'NONE', *, *, #36598, .F. ) ;
#82787 = CARTESIAN_POINT ( 'NONE',  ( -1.099225684535947600, 53.70696800326376064, -6.408140936763238038 ) ) ;
#82788 = CARTESIAN_POINT ( 'NONE',  ( 10.00000000000000000, 66.81368534415484817, -10.88017736071110342 ) ) ;
#82789 = VERTEX_POINT ( 'NONE', #823 ) ;
#82790 = CARTESIAN_POINT ( 'NONE',  ( 10.00000000000000000, 10.55374883491396787, -14.16423886937410082 ) ) ;
#82791 = CARTESIAN_POINT ( 'NONE',  ( 0.1532563361054082862, 11.21726448433411605, 2.638427012816831674 ) ) ;
#82792 = CARTESIAN_POINT ( 'NONE',  ( 15.44008868035555793, 26.39701867748817321, -9.422509992056140149 ) ) ;
#82793 = FACE_OUTER_BOUND ( 'NONE', #47561, .T. ) ;
#82794 = ORIENTED_EDGE ( 'NONE', *, *, #78495, .T. ) ;
#82795 = CARTESIAN_POINT ( 'NONE',  ( 7.084665262690076126, 34.10535201082151247, 10.88017736071109987 ) ) ;
#82796 = ORIENTED_EDGE ( 'NONE', *, *, #18867, .F. ) ;
#82797 = CARTESIAN_POINT ( 'NONE',  ( 20.88017736071110164, 35.35535201082150536, 2.915334737309930979 ) ) ;
#82798 = CARTESIAN_POINT ( 'NONE',  ( 0.2751277870542967463, 70.00000000000000000, -6.000000000000000000 ) ) ;
#82799 = ORIENTED_EDGE ( 'NONE', *, *, #21393, .T. ) ;
#82800 = ORIENTED_EDGE ( 'NONE', *, *, #29295, .T. ) ;
#82801 = CARTESIAN_POINT ( 'NONE',  ( 17.96484262340118221, 64.93868534415483396, 7.964842623401181321 ) ) ;
#82802 = DIRECTION ( 'NONE',  ( 0.000000000000000000, 0.000000000000000000, 1.000000000000000000 ) ) ;
#82804 = DIRECTION ( 'NONE',  ( 0.000000000000000000, -1.000000000000000000, 0.000000000000000000 ) ) ;
#82803 = CARTESIAN_POINT ( 'NONE',  ( 7.084665262690076126, 17.02201867748817676, -10.88017736071110164 ) ) ;
#82805 = CARTESIAN_POINT ( 'NONE',  ( 14.92337183194729988, 9.342264484334119601, -8.527530157486177487 ) ) ;
#82806 = CARTESIAN_POINT ( 'NONE',  ( 17.96484262340118221, 21.18868534415483396, -7.964842623401177768 ) ) ;
#82807 = ADVANCED_FACE ( 'NONE', ( #76303 ), #15797, .T. ) ;
#82808 = COLOUR_RGB ( '', 0.08235294, 0.09019608, 0.10196078) ;
#82809 = ORIENTED_EDGE ( 'NONE', *, *, #68966, .T. ) ;
#82810 = CARTESIAN_POINT ( 'NONE',  ( 10.00000000000000178, 50.37363466993042493, 12.81628187352647608 ) ) ;
#82811 = CARTESIAN_POINT ( 'NONE',  ( -0.8801773607111008646, 48.27201867748816966, 2.915334737309923430 ) ) ;
#82812 = CARTESIAN_POINT ( 'NONE',  ( -1.326515405096241107, 0.2306972965111871998, 14.88215077106014306 ) ) ;
#82813 = CARTESIAN_POINT ( 'NONE',  ( 6.565887622018943937, 55.16530133659709634, 12.81628187352647430 ) ) ;
#82814 = CARTESIAN_POINT ( 'NONE',  ( 20.88017736071110164, 45.35535201082149115, 2.915334737309930979 ) ) ;
#82815 = CARTESIAN_POINT ( 'NONE',  ( 21.09922568453594849, 6.206968003263753531, 6.408140936763242479 ) ) ;
#82816 = COLOUR_RGB ( '', 0.66274510, 0.83137255, 0.94901961) ;
#82817 = CARTESIAN_POINT ( 'NONE',  ( 18.52753015748617571, 13.09226448433411960, 4.923371831947298993 ) ) ;
#82818 = CARTESIAN_POINT ( 'NONE',  ( 0.000000000000000000, 0.5000000000000004441, 0.000000000000000000 ) ) ;
#82819 = CARTESIAN_POINT ( 'NONE',  ( 19.38216949554541202, 10.99863466993042138, 9.382169495545424454 ) ) ;
#82821 = CARTESIAN_POINT ( 'NONE',  ( 10.00000000000000178, 67.25893115100079456, 9.846743663894594434 ) ) ;
#82820 = SURFACE_STYLE_USAGE ( .BOTH. , #22341 ) ;
#82822 = CARTESIAN_POINT ( 'NONE',  ( 7.084665262690076126, 37.02201867748817676, -10.88017736071110164 ) ) ;
#82823 = CARTESIAN_POINT ( 'NONE',  ( 17.20831665107776587, 49.13393115100078745, -7.208316651077762316 ) ) ;
#82824 = FACE_OUTER_BOUND ( 'NONE', #3882, .T. ) ;
#82826 = CARTESIAN_POINT ( 'NONE',  ( 1.472469842513823179, 21.42559781766745175, 4.923371831947296329 ) ) ;
#82825 = AXIS2_PLACEMENT_3D ( 'NONE', #62608, #41127, #18127 ) ;
#82827 = CARTESIAN_POINT ( 'NONE',  ( 2.791683348922240793, 6.633931151000785675, 7.208316651077764092 ) ) ;
#82829 = ORIENTED_EDGE ( 'NONE', *, *, #78395, .T. ) ;
#82828 = CARTESIAN_POINT ( 'NONE',  ( 3.591859063236763294, -1.709698663402913210, -11.09922568453595026 ) ) ;
#82830 = VECTOR ( 'NONE', #80950, 999.9999999999998863 ) ;
#82831 = CARTESIAN_POINT ( 'NONE',  ( 19.42250999205614193, 5.147018677488171434, 5.440088680355555262 ) ) ;
#82832 = SURFACE_SIDE_STYLE ('',( #52337 ) ) ;
#82833 = CARTESIAN_POINT ( 'NONE',  ( 17.20831665107776587, 59.13393115100078745, -7.208316651077762316 ) ) ;
#82834 = CARTESIAN_POINT ( 'NONE',  ( 10.00000000000000178, 37.25893115100078745, 9.846743663894594434 ) ) ;
#82835 = CARTESIAN_POINT ( 'NONE',  ( 4.406185888753203272, -8.255243720366360449, -2.499999999999999112 ) ) ;
#82836 = CARTESIAN_POINT ( 'NONE',  ( 17.96484262340118221, 4.938685344154837509, 7.964842623401181321 ) ) ;
#82837 = CARTESIAN_POINT ( 'NONE',  ( 0.1532563361054082862, 51.21726448433412315, 2.638427012816831674 ) ) ;
#82838 = ORIENTED_EDGE ( 'NONE', *, *, #92728, .T. ) ;
#82839 = EDGE_CURVE ( 'NONE', #81238, #74503, #68319, .T. ) ;
#82840 = LINE ( 'NONE', #59342, #2632 ) ;
#82841 = CARTESIAN_POINT ( 'NONE',  ( 10.00000000000000000, 1.813685344154838175, -10.88017736071110342 ) ) ;
#82842 = CARTESIAN_POINT ( 'NONE',  ( 64.56412365047461321, 11.99999999999999467, 6.999999999999999112 ) ) ;
#82843 = CARTESIAN_POINT ( 'NONE',  ( 7.084665262690076126, 17.02201867748817676, -10.88017736071110164 ) ) ;
#82844 = CARTESIAN_POINT ( 'NONE',  ( 2.917880565312950480, 50.97041550158064638, -12.26659068614894821 ) ) ;
#82846 = CARTESIAN_POINT ( 'NONE',  ( -0.2838433074297238012, 13.12729635533385597, 9.500000000000000000 ) ) ;
#82845 = CARTESIAN_POINT ( 'NONE',  ( 24.16423886937409904, 54.09541550158063217, 3.795296366450317205 ) ) ;
#82847 = CARTESIAN_POINT ( 'NONE',  ( 10.00000000000000000, 4.758931151000784787, -9.846743663894594434 ) ) ;
#82848 =( BOUNDED_CURVE ( )  B_SPLINE_CURVE ( 2, ( #63674, #55706, #17225, #70219, #62199, #40207, #41208, #93692, #2231 ),
 .UNSPECIFIED., .F., .T. ) 
 B_SPLINE_CURVE_WITH_KNOTS ( ( 3, 2, 2, 2, 3 ),
 ( 0.7258552226545171848, 0.7261904761904762751, 0.7321428571428572063, 0.7380952380952381375, 0.7384304916311973388 ),
 .UNSPECIFIED. ) 
 CURVE ( )  GEOMETRIC_REPRESENTATION_ITEM ( )  RATIONAL_B_SPLINE_CURVE ( ( 0.9963778908391764944, 0.9980808541467923733, 1.000000000000000000, 0.9659258262890682012, 1.000000000000000000, 0.9659258262890682012, 1.000000000000000000, 0.9980808541467917072, 0.9963778908391753841 ) ) 
 REPRESENTATION_ITEM ( '' )  );
#82849 = CARTESIAN_POINT ( 'NONE',  ( 0.1532563361054083140, 31.00893115100078390, 1.131784320476157264E-15 ) ) ;
#82850 = CARTESIAN_POINT ( 'NONE',  ( 6.565887622018943937, 8.081968003263751754, -12.81628187352647608 ) ) ;
#82851 = ORIENTED_EDGE ( 'NONE', *, *, #33204, .T. ) ;
#82852 = EDGE_LOOP ( 'NONE', ( #8403, #83687, #96330, #7955, #29583, #39778 ) ) ;
#82853 = CARTESIAN_POINT ( 'NONE',  ( -14.67697702673046933, -0.03417435944610275333, 6.361111679013309761 ) ) ;
#82854 = CARTESIAN_POINT ( 'NONE',  ( 0.1532563361054100626, 60.80059781766744464, -2.638427012816831230 ) ) ;
#82855 = AXIS2_PLACEMENT_3D ( 'NONE', #3866, #80344, #86378 ) ;
#82856 = CARTESIAN_POINT ( 'NONE',  ( 9.879999999999990123, 20.99999999999999645, -1.249999999999987121 ) ) ;
#82857 = EDGE_CURVE ( 'NONE', #34814, #42118, #45189, .T. ) ;
#82858 =( BOUNDED_CURVE ( )  B_SPLINE_CURVE ( 2, ( #10709, #41224, #79692, #11190, #36155, #36661, #20666, #43654, #49666 ),
 .UNSPECIFIED., .F., .F. ) 
 B_SPLINE_CURVE_WITH_KNOTS ( ( 3, 2, 2, 2, 3 ),
 ( 0.3320003743640375649, 0.3333333333333333148, 0.3392857142857143016, 0.3452380952380952328, 0.3465710542073918710 ),
 .UNSPECIFIED. ) 
 CURVE ( )  GEOMETRIC_REPRESENTATION_ITEM ( )  RATIONAL_B_SPLINE_CURVE ( ( 0.9881565478350775589, 0.9923695281211528663, 1.000000000000000000, 0.9659258262890683122, 1.000000000000000000, 0.9659258262890683122, 1.000000000000000000, 0.9923695281211478703, 0.9881565478350720078 ) ) 
 REPRESENTATION_ITEM ( '' )  );
#82859 = DIRECTION ( 'NONE',  ( -0.9995586998285019842, -0.02970531260826359682, 0.000000000000000000 ) ) ;
#82860 = CARTESIAN_POINT ( 'NONE',  ( 17.08211943468705130, 8.470415501580635720, 12.26659068614894998 ) ) ;
#82861 = CARTESIAN_POINT ( 'NONE',  ( 18.52753015748618282, 23.92559781766745530, -4.923371831947291888 ) ) ;
#82862 = DIRECTION ( 'NONE',  ( 0.000000000000000000, 0.000000000000000000, 1.000000000000000000 ) ) ;
#82863 = ORIENTED_EDGE ( 'NONE', *, *, #348, .F. ) ;
#82864 = CARTESIAN_POINT ( 'NONE',  ( 22.26659068614894466, 38.88708216824731068, 7.082119434687054849 ) ) ;
#82865 = EDGE_CURVE ( 'NONE', #16073, #74198, #33162, .T. ) ;
#82866 = EDGE_CURVE ( 'NONE', #39274, #4466, #90364, .T. ) ;
#82867 = CARTESIAN_POINT ( 'NONE',  ( 7.361572987183169658, 4.967264484334119601, -9.846743663894592657 ) ) ;
#82869 = DIRECTION ( 'NONE',  ( 0.000000000000000000, 0.000000000000000000, 1.000000000000000000 ) ) ;
#82868 = CARTESIAN_POINT ( 'NONE',  ( -6.829922651553562929, -69.52824172495176924, -2.500000000000000000 ) ) ;
#82870 = CARTESIAN_POINT ( 'NONE',  ( 2.035157376598822676, 27.43868534415483396, -7.964842623401177768 ) ) ;
#82871 = CARTESIAN_POINT ( 'NONE',  ( 19.38216949554541557, 42.24863466993041783, -9.382169495545420901 ) ) ;
#82872 = CARTESIAN_POINT ( 'NONE',  ( -0.8801773607110991993, 7.855352010821504471, -2.915334737309923874 ) ) ;
#82873 = CARTESIAN_POINT ( 'NONE',  ( 22.81628187352647785, 36.62363466993041783, 6.195893100308588602E-16 ) ) ;
#82874 = CARTESIAN_POINT ( 'NONE',  ( 7.361572987183169658, 4.967264484334119601, -9.846743663894592657 ) ) ;
#82875 = ORIENTED_EDGE ( 'NONE', *, *, #30256, .F. ) ;
#82876 = DIRECTION ( 'NONE',  ( -0.000000000000000000, -0.000000000000000000, 1.000000000000000000 ) ) ;
#82877 = LINE ( 'NONE', #75366, #12714 ) ;
#82878 = CARTESIAN_POINT ( 'NONE',  ( -0.3689425029237881626, 47.42874883491396787, 10.36894250292379027 ) ) ;
#82879 = CARTESIAN_POINT ( 'NONE',  ( -0.8801773607110991993, 22.85535201082150181, -2.915334737309923874 ) ) ;
#82880 = CARTESIAN_POINT ( 'NONE',  ( -9.972640495195461696, 15.00000000000000000, 12.50695158660338890 ) ) ;
#82881 = LINE ( 'NONE', #81395, #1709 ) ;
#82882 = CARTESIAN_POINT ( 'NONE',  ( 19.42250999205614548, 55.98035201082150536, -5.440088680355545492 ) ) ;
#82883 = CARTESIAN_POINT ( 'NONE',  ( 20.88017736071110164, 65.35535201082150536, 2.915334737309930979 ) ) ;
#82884 = CARTESIAN_POINT ( 'NONE',  ( 19.38216949554541202, 20.99863466993042138, 9.382169495545424454 ) ) ;
#82885 = DIRECTION ( 'NONE',  ( 0.000000000000000000, -1.000000000000000000, 0.000000000000000000 ) ) ;
#82886 = CARTESIAN_POINT ( 'NONE',  ( -3.193136578976892626, 15.00000000000000888, -14.27383009353655119 ) ) ;
#82887 = CARTESIAN_POINT ( 'NONE',  ( 10.00000000000000178, 22.25893115100078745, 9.846743663894594434 ) ) ;
#82888 = CARTESIAN_POINT ( 'NONE',  ( -0.8801773607111009756, 53.06368534415484106, 1.068504757029289695E-15 ) ) ;
#82890 = EDGE_CURVE ( 'NONE', #38545, #9043, #90529, .T. ) ;
#82889 = CARTESIAN_POINT ( 'NONE',  ( -2.816281873526473856, 24.12363466993042138, 9.499525473075851096E-16 ) ) ;
#82891 = CARTESIAN_POINT ( 'NONE',  ( 5.448048636097845510, 0.000000000000000000, -0.2378669404634490003 ) ) ;
#82892 = CARTESIAN_POINT ( 'NONE',  ( 20.88017736071110875, 5.772018677488170546, -2.915334737309920765 ) ) ;
#82893 = CARTESIAN_POINT ( 'NONE',  ( 17.20831665107776587, 42.88393115100077324, 7.208316651077764980 ) ) ;
#82894 = CARTESIAN_POINT ( 'NONE',  ( 6.565887622018943937, 63.08196800326376064, -12.81628187352647608 ) ) ;
#82895 = CARTESIAN_POINT ( 'NONE',  ( 0.1532563361054083140, 16.00893115100078390, 1.131784320476157264E-15 ) ) ;
#82896 = CARTESIAN_POINT ( 'NONE',  ( 19.10478245763047056, 31.02576239577081907, -5.990408912944402253 ) ) ;
#82897 = CARTESIAN_POINT ( 'NONE',  ( 17.96484262340118221, 39.93868534415484106, 7.964842623401181321 ) ) ;
#82898 = CARTESIAN_POINT ( 'NONE',  ( -2.266590686148945544, 31.38708216824730002, -7.082119434687050408 ) ) ;
#82899 = EDGE_CURVE ( 'NONE', #77019, #23582, #69796, .T. ) ;
#82900 = CARTESIAN_POINT ( 'NONE',  ( 1.472469842513823179, 40.59226448433411605, -4.923371831947296329 ) ) ;
#82901 = VECTOR ( 'NONE', #69762, 1000.000000000000000 ) ;
#82902 = CARTESIAN_POINT ( 'NONE',  ( 12.91533473730993009, 26.60535201082150536, -10.88017736071109987 ) ) ;
#82903 = CARTESIAN_POINT ( 'NONE',  ( 4.559911319644449179, 17.23035201082150536, -9.422509992056141925 ) ) ;
#82904 = VERTEX_POINT ( 'NONE', #344 ) ;
#82905 = CARTESIAN_POINT ( 'NONE',  ( 7.084665262690076126, 24.10535201082150181, 10.88017736071109987 ) ) ;
#82907 = CARTESIAN_POINT ( 'NONE',  ( 10.00000000000000178, 45.37363466993041783, 12.81628187352647608 ) ) ;
#82906 = VECTOR ( 'NONE', #35063, 1000.000000000000000 ) ;
#82908 = CARTESIAN_POINT ( 'NONE',  ( 2.035157376598822676, 42.43868534415483396, -7.964842623401177768 ) ) ;
#82910 = CARTESIAN_POINT ( 'NONE',  ( 17.96484262340118221, 36.18868534415484106, -7.964842623401177768 ) ) ;
#82909 = DIRECTION ( 'NONE',  ( 0.000000000000000000, 0.000000000000000000, 1.000000000000000000 ) ) ;
#82911 = ORIENTED_EDGE ( 'NONE', *, *, #62975, .F. ) ;
#82912 = CARTESIAN_POINT ( 'NONE',  ( 5.076628168052704559, 60.17559781766745175, -8.527530157486179263 ) ) ;
#82913 = CARTESIAN_POINT ( 'NONE',  ( 19.42250999205614548, 35.98035201082151247, -5.440088680355545492 ) ) ;
#82914 = CARTESIAN_POINT ( 'NONE',  ( 4.920853330210497312, -13.83152733635706433, 3.750000000000804690 ) ) ;
#82915 = DIRECTION ( 'NONE',  ( 0.6246950475544238435, 0.7808688094430307203, 0.000000000000000000 ) ) ;
#82916 = CARTESIAN_POINT ( 'NONE',  ( 13.79529636645031943, 40.34541550158063217, -14.16423886937409904 ) ) ;
#82917 = CARTESIAN_POINT ( 'NONE',  ( 12.91533473730992121, 59.52201867748816966, 10.88017736071110164 ) ) ;
#82918 = CARTESIAN_POINT ( 'NONE',  ( 20.88017736071110875, 55.77201867748816966, -2.915334737309920321 ) ) ;
#82919 = DIRECTION ( 'NONE',  ( 0.6360782202777648386, 0.000000000000000000, 0.7716245833877193316 ) ) ;
#82920 = CARTESIAN_POINT ( 'NONE',  ( 2.791683348922240793, 56.63393115100078035, 7.208316651077764092 ) ) ;
#82921 = CARTESIAN_POINT ( 'NONE',  ( -0.8801773607111009756, 3.063685344154837509, 1.068504757029289695E-15 ) ) ;
#82922 = CARTESIAN_POINT ( 'NONE',  ( 7.361572987183169658, 34.96726448433411605, -9.846743663894592657 ) ) ;
#82923 = ORIENTED_EDGE ( 'NONE', *, *, #95271, .F. ) ;
#82924 = CARTESIAN_POINT ( 'NONE',  ( 2.791683348922240793, 31.63393115100078745, 7.208316651077764092 ) ) ;
#82925 = CARTESIAN_POINT ( 'NONE',  ( -12.81628187352647608, -15.87636533006957507, 3.903127820947815962E-15 ) ) ;
#82926 = CARTESIAN_POINT ( 'NONE',  ( 4.559911319644449179, 32.23035201082150536, -9.422509992056141925 ) ) ;
#82927 = CARTESIAN_POINT ( 'NONE',  ( 5.076628168052703671, 21.84226448433411960, 8.527530157486179263 ) ) ;
#82928 = CARTESIAN_POINT ( 'NONE',  ( -2.816281873526473856, 24.33196800326375353, 3.434112377981055619 ) ) ;
#82930 = CARTESIAN_POINT ( 'NONE',  ( -0.8801773607111009756, 53.06368534415484106, 1.068504757029289695E-15 ) ) ;
#82929 = CARTESIAN_POINT ( 'NONE',  ( 2.035157376598824452, 68.68868534415484817, 7.964842623401179544 ) ) ;
#82932 = CARTESIAN_POINT ( 'NONE',  ( 6.565887622018943937, 65.16530133659709634, 12.81628187352647430 ) ) ;
#82931 = CARTESIAN_POINT ( 'NONE',  ( 7.084665262690076126, 34.10535201082151247, 10.88017736071109987 ) ) ;
#82933 = CARTESIAN_POINT ( 'NONE',  ( 20.36894250292379382, 38.67874883491396076, 10.36894250292379205 ) ) ;
#82934 = CIRCLE ( 'NONE', #95714, 1.249999999999987121 ) ;
#82935 =( BOUNDED_SURFACE ( )  B_SPLINE_SURFACE ( 3, 2, ( 
 ( #39475, #9953, #2962 ),
 ( #40459, #17945, #46951 ),
 ( #78933, #61461, #85454 ),
 ( #69471, #23497, #1484 ),
 ( #31937, #62438, #4431 ),
 ( #63912, #49409, #94913 ),
 ( #3441, #73885, #79910 ),
 ( #57891, #79433, #35394 ),
 ( #96415, #80417, #33899 ),
 ( #87414, #88406, #57407 ),
 ( #71920, #42905, #19414 ),
 ( #27399, #11418, #49905 ),
 ( #34897, #34399, #41940 ),
 ( #65886, #11915, #64406 ),
 ( #3929, #72402, #64887 ),
 ( #95415, #27890, #12890 ),
 ( #26910, #26412, #19904 ),
 ( #87898, #58378, #56913 ) ),
 .UNSPECIFIED., .F., .F., .F. ) 
 B_SPLINE_SURFACE_WITH_KNOTS ( ( 4, 2, 2, 2, 2, 2, 2, 2, 4 ),
 ( 3, 3 ),
 ( 0.000000000000000000, 0.002783952809522130881, 0.005567905619044261761, 0.01113581123808852352, 0.02227162247617704705, 0.04454324495235409409, 0.06681486742853114114, 0.07795067866661967160, 0.08908648990470818818 ),
 ( 0.000000000000000000, 1.000000000000000000 ),
 .UNSPECIFIED. ) 
 GEOMETRIC_REPRESENTATION_ITEM ( )  RATIONAL_B_SPLINE_SURFACE ( (
 ( 1.000000000000000000, 0.7071067811865475727, 1.000000000000000000),
 ( 1.000000000000000000, 0.7071067811865475727, 1.000000000000000000),
 ( 1.000000000000000000, 0.7071067811865475727, 1.000000000000000000),
 ( 1.000000000000000000, 0.7071067811865475727, 1.000000000000000000),
 ( 1.000000000000000000, 0.7071067811865475727, 1.000000000000000000),
 ( 1.000000000000000000, 0.7071067811865475727, 1.000000000000000000),
 ( 1.000000000000000000, 0.7071067811865475727, 1.000000000000000000),
 ( 1.000000000000000000, 0.7071067811865475727, 1.000000000000000000),
 ( 1.000000000000000000, 0.7071067811865475727, 1.000000000000000000),
 ( 1.000000000000000000, 0.7071067811865475727, 1.000000000000000000),
 ( 1.000000000000000000, 0.7071067811865487940, 1.000000000000000000),
 ( 1.000000000000000000, 0.7071067811865487940, 1.000000000000000000),
 ( 1.000000000000000000, 0.7071067811865487940, 1.000000000000000000),
 ( 1.000000000000000000, 0.7071067811865487940, 1.000000000000000000),
 ( 1.000000000000000000, 0.7071067811865475727, 1.000000000000000000),
 ( 1.000000000000000000, 0.7071067811865475727, 1.000000000000000000),
 ( 1.000000000000000000, 0.7071067811865479058, 1.000000000000000000),
 ( 1.000000000000000000, 0.7071067811865479058, 1.000000000000000000) ) ) 
 REPRESENTATION_ITEM ( '' )  SURFACE ( )  );
#82936 = CARTESIAN_POINT ( 'NONE',  ( -14.66196617519561052, 14.76930270348882068, 2.874856965127719377 ) ) ;
#82937 = ORIENTED_EDGE ( 'NONE', *, *, #31500, .T. ) ;
#82938 = CARTESIAN_POINT ( 'NONE',  ( 10.00000000000000000, 12.87363466993042138, -12.81628187352647608 ) ) ;
#82939 = CARTESIAN_POINT ( 'NONE',  ( 20.88017736071110519, 10.56368534415483751, 2.639326808657452039E-16 ) ) ;
#82940 = CARTESIAN_POINT ( 'NONE',  ( -0.8801773607111008646, 53.27201867748816966, 2.915334737309923430 ) ) ;
#82941 = CARTESIAN_POINT ( 'NONE',  ( 6.000000000000000000, 60.50000000000000711, 6.000000000000000000 ) ) ;
#82942 = ORIENTED_EDGE ( 'NONE', *, *, #27556, .T. ) ;
#82943 = AXIS2_PLACEMENT_3D ( 'NONE', #44959, #62415, #83953 ) ;
#82944 = B_SPLINE_CURVE_WITH_KNOTS ( 'NONE', 3,
 ( #23625, #38128, #68616, #22132, #60607, #91101 ),
 .UNSPECIFIED., .F., .F.,
 ( 4, 2, 4 ),
 ( 0.0002800715030460580518, 0.0006862774322447752397, 0.001092483361443492536 ),
 .UNSPECIFIED. ) ;
#82945 = CARTESIAN_POINT ( 'NONE',  ( 7.084665262690076126, 57.02201867748817676, -10.88017736071110164 ) ) ;
#82946 = CARTESIAN_POINT ( 'NONE',  ( 0.1532563361054082862, 36.21726448433410894, 2.638427012816831674 ) ) ;
#82947 = CARTESIAN_POINT ( 'NONE',  ( 0.1532563361054100626, 25.80059781766744820, -2.638427012816831230 ) ) ;
#82948 = CARTESIAN_POINT ( 'NONE',  ( 0.1532563361054082862, 16.21726448433411960, 2.638427012816831674 ) ) ;
#82949 = EDGE_CURVE ( 'NONE', #75676, #83267, #70768, .T. ) ;
#82950 = VECTOR ( 'NONE', #32321, 1000.000000000000000 ) ;
#82952 = CARTESIAN_POINT ( 'NONE',  ( 22.81628187352648496, 36.83196800326376064, -3.434112377981050290 ) ) ;
#82951 = CARTESIAN_POINT ( 'NONE',  ( 18.95386800104996539, 63.23810908735725889, -6.499999999999984901 ) ) ;
#82954 = CARTESIAN_POINT ( 'NONE',  ( 5.000000000000000000, -2.909297654740273256E-16, 0.000000000000000000 ) ) ;
#82953 = CARTESIAN_POINT ( 'NONE',  ( 2.791683348922240793, 16.63393115100078745, 7.208316651077764092 ) ) ;
#82955 = LINE ( 'NONE', #21975, #53722 ) ;
#82957 = EDGE_LOOP ( 'NONE', ( #71857, #16766, #63840, #83746, #16879, #33346 ) ) ;
#82956 = CARTESIAN_POINT ( 'NONE',  ( 18.52753015748617571, 28.09226448433411960, 4.923371831947298993 ) ) ;
#82958 = CARTESIAN_POINT ( 'NONE',  ( -1.099225684535947600, 53.70696800326376064, -6.408140936763238038 ) ) ;
#82959 = CARTESIAN_POINT ( 'NONE',  ( 0.000000000000000000, 15.00000000000000000, 0.000000000000000000 ) ) ;
#82960 = CARTESIAN_POINT ( 'NONE',  ( 19.38216949554541557, 7.248634669930421381, -9.382169495545420901 ) ) ;
#82961 = CARTESIAN_POINT ( 'NONE',  ( -0.8801773607111009756, 48.06368534415484817, 1.068504757029289695E-15 ) ) ;
#82962 = CARTESIAN_POINT ( 'NONE',  ( 22.26659068614895176, 34.72041550158063927, -7.082119434687042414 ) ) ;
#82963 = CARTESIAN_POINT ( 'NONE',  ( 1.274849032794278747, 42.55509018479936856, -6.499999999999960032 ) ) ;
#82964 = CARTESIAN_POINT ( 'NONE',  ( -4.164238869374098151, 31.59541550158063927, -3.795296366450310543 ) ) ;
#82965 = CARTESIAN_POINT ( 'NONE',  ( 17.08211943468705840, 50.13708216824730357, -12.26659068614894466 ) ) ;
#82966 = CARTESIAN_POINT ( 'NONE',  ( 20.36894250292379382, 13.67874883491396965, 10.36894250292379205 ) ) ;
#82968 = CARTESIAN_POINT ( 'NONE',  ( 18.72515096720568906, 36.07228050351032778, -6.500000000000007105 ) ) ;
#82967 = CARTESIAN_POINT ( 'NONE',  ( -2.266590686148945544, 11.38708216824730179, -7.082119434687050408 ) ) ;
#82969 = CARTESIAN_POINT ( 'NONE',  ( -0.8801773607111008646, 43.27201867748817676, 2.915334737309923430 ) ) ;
#82970 = CARTESIAN_POINT ( 'NONE',  ( 14.52941021839284375, -2.151463686025920889E-16, 1.683622718073147562 ) ) ;
#82971 = CARTESIAN_POINT ( 'NONE',  ( 12.63842701281683034, 32.46726448433412315, 9.846743663894596210 ) ) ;
#82972 = ADVANCED_FACE ( 'NONE', ( #15332 ), #92290, .T. ) ;
#82974 = CARTESIAN_POINT ( 'NONE',  ( 17.20831665107776587, 24.13393115100078035, -7.208316651077762316 ) ) ;
#82973 = CARTESIAN_POINT ( 'NONE',  ( 12.91533473730992121, 64.52201867748817676, 10.88017736071110164 ) ) ;
#82975 = CARTESIAN_POINT ( 'NONE',  ( 20.88017736071110875, 20.77201867748816611, -2.915334737309920765 ) ) ;
#82976 = CARTESIAN_POINT ( 'NONE',  ( -2.816281873526473856, 59.33196800326374643, 3.434112377981055619 ) ) ;
#82977 = CARTESIAN_POINT ( 'NONE',  ( 2.791683348922237240, 65.38393115100078035, -7.208316651077763204 ) ) ;
#82978 = DIRECTION ( 'NONE',  ( 0.000000000000000000, 0.000000000000000000, -1.000000000000000000 ) ) ;
#82979 = CARTESIAN_POINT ( 'NONE',  ( 1.472469842513823179, 26.42559781766745175, 4.923371831947296329 ) ) ;
#82980 = CARTESIAN_POINT ( 'NONE',  ( 13.43411237798106583, 42.66530133659707502, -12.81628187352647252 ) ) ;
#82981 = CARTESIAN_POINT ( 'NONE',  ( 14.16423886937410082, -25.48791783175269643, -3.795296366450314096 ) ) ;
#82982 = CARTESIAN_POINT ( 'NONE',  ( 12.91533473730992121, 39.52201867748817676, 10.88017736071110164 ) ) ;
#82983 = CARTESIAN_POINT ( 'NONE',  ( 17.20831665107776587, 59.13393115100078745, -7.208316651077762316 ) ) ;
#82984 = EDGE_CURVE ( 'NONE', #82423, #51651, #64300, .T. ) ;
#82985 = CARTESIAN_POINT ( 'NONE',  ( 24.16423886937410614, 29.51208216824729647, -3.795296366450302550 ) ) ;
#82986 = ORIENTED_EDGE ( 'NONE', *, *, #66249, .F. ) ;
#82987 = CARTESIAN_POINT ( 'NONE',  ( 6.204703633549690345, 0.7620821682473009062, -14.16423886937410259 ) ) ;
#82988 = EDGE_CURVE ( 'NONE', #92281, #16383, #53803, .T. ) ;
#82989 = CARTESIAN_POINT ( 'NONE',  ( 7.084665262690076126, 67.02201867748817676, -10.88017736071110164 ) ) ;
#82990 = CARTESIAN_POINT ( 'NONE',  ( 0.5774900079438607392, 68.48035201082150536, 5.440088680355550821 ) ) ;
#82991 = CARTESIAN_POINT ( 'NONE',  ( 22.26659068614894466, 58.88708216824729647, 7.082119434687054849 ) ) ;
#82992 = CARTESIAN_POINT ( 'NONE',  ( -2.816281873526473856, 4.331968003263754419, 3.434112377981055619 ) ) ;
#82993 = DIRECTION ( 'NONE',  ( 0.000000000000000000, 0.000000000000000000, -1.000000000000000000 ) ) ;
#82994 = CARTESIAN_POINT ( 'NONE',  ( -0.8801773607111009756, 58.06368534415484106, 1.068504757029289695E-15 ) ) ;
#82995 = CARTESIAN_POINT ( 'NONE',  ( -0.2418659066527515111, 27.23410085661203439, -6.114288769123079170 ) ) ;
#82996 = VECTOR ( 'NONE', #66889, 1000.000000000000114 ) ;
#82997 = CARTESIAN_POINT ( 'NONE',  ( 10.00000000000000000, 50.55374883491396787, -14.16423886937410082 ) ) ;
#82998 = CARTESIAN_POINT ( 'NONE',  ( -2.915334737309917656, 29.10535201082149825, 10.88017736071110164 ) ) ;
#82999 = CARTESIAN_POINT ( 'NONE',  ( 15.44008868035555260, 9.730352010821505360, 9.422509992056143702 ) ) ;
#83000 = CARTESIAN_POINT ( 'NONE',  ( 19.42250999205614548, 20.98035201082150891, -5.440088680355545492 ) ) ;
#83001 = CARTESIAN_POINT ( 'NONE',  ( 0.1532563361054100626, 60.80059781766744464, -2.638427012816831230 ) ) ;
#83002 = CARTESIAN_POINT ( 'NONE',  ( -1.099225684535947600, 44.54030133659708923, 6.408140936763237150 ) ) ;
#83003 = CARTESIAN_POINT ( 'NONE',  ( -14.82269085861170232, 0.5000000000000004441, 2.299529454046861154 ) ) ;
#83005 = ORIENTED_EDGE ( 'NONE', *, *, #9939, .F. ) ;
#83004 = CIRCLE ( 'NONE', #15988, 2.750000000000000888 ) ;
#83006 = AXIS2_PLACEMENT_3D ( 'NONE', #60878, #29388, #39748 ) ;
#83007 = CARTESIAN_POINT ( 'NONE',  ( 4.559911319644449179, 12.23035201082150536, -9.422509992056141925 ) ) ;
#83008 = CARTESIAN_POINT ( 'NONE',  ( 19.38216949554541557, 22.24863466993041428, -9.382169495545420901 ) ) ;
#83009 = DIRECTION ( 'NONE',  ( -0.9999619230641713097, 0.000000000000000000, 0.008726535498367547425 ) ) ;
#83010 = CARTESIAN_POINT ( 'NONE',  ( 0.1532563361054083140, 46.00893115100079456, 1.131784320476157264E-15 ) ) ;
#83011 = CARTESIAN_POINT ( 'NONE',  ( 2.035157376598824452, 38.68868534415483396, 7.964842623401179544 ) ) ;
#83012 = CARTESIAN_POINT ( 'NONE',  ( 16.40814093676323893, 25.79030133659708923, 11.09922568453595026 ) ) ;
#83014 = CARTESIAN_POINT ( 'NONE',  ( 14.24131928502211686, -0.03417435944610275333, -0.4973178280105898241 ) ) ;
#83013 = CARTESIAN_POINT ( 'NONE',  ( 19.42250999205614548, 45.98035201082150536, -5.440088680355545492 ) ) ;
#83015 = FACE_OUTER_BOUND ( 'NONE', #16251, .T. ) ;
#83016 = CARTESIAN_POINT ( 'NONE',  ( 19.38216949554541202, 45.99863466993041072, 9.382169495545424454 ) ) ;
#83017 = ORIENTED_EDGE ( 'NONE', *, *, #9622, .F. ) ;
#83018 = DIRECTION ( 'NONE',  ( -1.000000000000000000, 0.000000000000000000, 0.000000000000000000 ) ) ;
#83019 = CARTESIAN_POINT ( 'NONE',  ( 19.42250999205614193, 45.14701867748817676, 5.440088680355555262 ) ) ;
#83020 = CARTESIAN_POINT ( 'NONE',  ( -1.099225684535947600, 39.54030133659708923, 6.408140936763237150 ) ) ;
#83021 = EDGE_CURVE ( 'NONE', #95671, #80833, #14069, .T. ) ;
#83022 = CARTESIAN_POINT ( 'NONE',  ( 15.44008868035555260, 44.73035201082151247, 9.422509992056143702 ) ) ;
#83023 = CARTESIAN_POINT ( 'NONE',  ( 14.92337183194729633, 62.67559781766745886, 8.527530157486181039 ) ) ;
#83024 = CARTESIAN_POINT ( 'NONE',  ( 2.791683348922237240, 65.38393115100078035, -7.208316651077763204 ) ) ;
#83025 = CIRCLE ( 'NONE', #30263, 1.999999999999996669 ) ;
#83026 = CARTESIAN_POINT ( 'NONE',  ( 14.92337183194729633, 22.67559781766745175, 8.527530157486181039 ) ) ;
#83027 = CARTESIAN_POINT ( 'NONE',  ( 14.92337183194729633, 12.67559781766745353, 8.527530157486181039 ) ) ;
#83028 = CARTESIAN_POINT ( 'NONE',  ( 24.16423886937410614, 49.51208216824730357, -3.795296366450302550 ) ) ;
#83029 = CARTESIAN_POINT ( 'NONE',  ( 21.92686044187656691, 24.95379003517448169, 3.195792623639537755 ) ) ;
#83030 =( NAMED_UNIT ( * ) SI_UNIT ( $, .STERADIAN. ) SOLID_ANGLE_UNIT ( ) );
#83031 = EDGE_CURVE ( 'NONE', #32731, #9920, #16792, .T. ) ;
#83032 = CARTESIAN_POINT ( 'NONE',  ( -5.331138373814036768, -28.69357394139028017, -3.750000000000000000 ) ) ;
#83033 = VERTEX_POINT ( 'NONE', #17291 ) ;
#83034 = ORIENTED_EDGE ( 'NONE', *, *, #35977, .T. ) ;
#83035 = CARTESIAN_POINT ( 'NONE',  ( 6.204703633549690345, 62.84541550158063927, 14.16423886937410082 ) ) ;
#83036 = CARTESIAN_POINT ( 'NONE',  ( -2.266590686148945544, 67.22041550158063217, 7.082119434687048631 ) ) ;
#83037 = CARTESIAN_POINT ( 'NONE',  ( 10.00000000000000178, 27.25893115100078390, 9.846743663894594434 ) ) ;
#83038 = CARTESIAN_POINT ( 'NONE',  ( 3.591859063236761518, 44.95696800326376064, 11.09922568453594849 ) ) ;
#83039 = CARTESIAN_POINT ( 'NONE',  ( -4.096035146093331747, 15.00000000000000000, -13.90943910019262653 ) ) ;
#83041 = CARTESIAN_POINT ( 'NONE',  ( -2.266590686148945544, 6.387082168247300906, -7.082119434687050408 ) ) ;
#83040 = CARTESIAN_POINT ( 'NONE',  ( -11.22722615951306935, 89.90850287678604502, -6.380836486324904300 ) ) ;
#83042 = CARTESIAN_POINT ( 'NONE',  ( 7.084665262690076126, 19.10535201082150181, 10.88017736071109987 ) ) ;
#83043 = CARTESIAN_POINT ( 'NONE',  ( -0.3689425029237881626, 62.42874883491396787, 10.36894250292379027 ) ) ;
#83044 = CARTESIAN_POINT ( 'NONE',  ( 14.92337183194729633, 42.67559781766745886, 8.527530157486181039 ) ) ;
#83045 = CARTESIAN_POINT ( 'NONE',  ( 10.00000000000000000, 19.75893115100078390, -9.846743663894594434 ) ) ;
#83046 = CARTESIAN_POINT ( 'NONE',  ( 17.84635730667654840, 58.63791097397317742, 6.500000000000043521 ) ) ;
#83047 = CARTESIAN_POINT ( 'NONE',  ( 9.846743663894594434, 18.50893115100080166, -2.168404344971008868E-15 ) ) ;
#83048 = ORIENTED_EDGE ( 'NONE', *, *, #26429, .T. ) ;
#83049 = ORIENTED_EDGE ( 'NONE', *, *, #21121, .F. ) ;
#83050 = FACE_OUTER_BOUND ( 'NONE', #27722, .T. ) ;
#83051 = EDGE_LOOP ( 'NONE', ( #30691, #73761, #76169, #75546 ) ) ;
#83052 = CARTESIAN_POINT ( 'NONE',  ( -2.266590686148945544, 17.22041550158063572, 7.082119434687048631 ) ) ;
#83054 = CARTESIAN_POINT ( 'NONE',  ( 0.5774900079438590739, 32.64701867748816966, -5.440088680355550821 ) ) ;
#83053 = CARTESIAN_POINT ( 'NONE',  ( 7.084665262690076126, 39.10535201082150536, 10.88017736071109987 ) ) ;
#83055 = CARTESIAN_POINT ( 'NONE',  ( 21.09922568453595559, 27.04030133659708568, -6.408140936763230044 ) ) ;
#83056 = CARTESIAN_POINT ( 'NONE',  ( 24.16423886937410614, 9.512082168247301794, -3.795296366450302550 ) ) ;
#83057 = CARTESIAN_POINT ( 'NONE',  ( 12.91533473730993009, 66.60535201082150536, -10.88017736071109987 ) ) ;
#83058 = CARTESIAN_POINT ( 'NONE',  ( -2.816281873526471635, 33.91530133659708213, -3.434112377981056508 ) ) ;
#83059 = VERTEX_POINT ( 'NONE', #72232 ) ;
#83060 = CARTESIAN_POINT ( 'NONE',  ( 1.472469842513823179, 45.59226448433412315, -4.923371831947296329 ) ) ;
#83061 = CARTESIAN_POINT ( 'NONE',  ( 10.00000000000000000, 1.813685344154838175, -10.88017736071110342 ) ) ;
#83062 = VERTEX_POINT ( 'NONE', #3261 ) ;
#83063 = CARTESIAN_POINT ( 'NONE',  ( 10.00000000000000178, 19.31368534415484106, 10.88017736071110342 ) ) ;
#83064 = ORIENTED_EDGE ( 'NONE', *, *, #5536, .T. ) ;
#83065 = CARTESIAN_POINT ( 'NONE',  ( 7.084665262690076126, 64.10535201082150536, 10.88017736071109987 ) ) ;
#83066 = AXIS2_PLACEMENT_3D ( 'NONE', #20289, #19302, #87786 ) ;
#83067 = CARTESIAN_POINT ( 'NONE',  ( 15.44008868035555793, 56.39701867748817676, -9.422509992056140149 ) ) ;
#83069 = EDGE_CURVE ( 'NONE', #3928, #42348, #49813, .T. ) ;
#83068 = CARTESIAN_POINT ( 'NONE',  ( 15.44008868035555260, 64.73035201082151957, 9.422509992056143702 ) ) ;
#83070 = CARTESIAN_POINT ( 'NONE',  ( 5.076628168052704559, 0.1755978176674514724, -8.527530157486179263 ) ) ;
#83071 = CARTESIAN_POINT ( 'NONE',  ( 2.035157376598824452, 53.68868534415484817, 7.964842623401179544 ) ) ;
#83072 = LINE ( 'NONE', #75570, #17181 ) ;
#83073 = EDGE_CURVE ( 'NONE', #3586, #72554, #40267, .T. ) ;
#83074 = CARTESIAN_POINT ( 'NONE',  ( 4.922013193295424749, 0.000000000000000000, 2.347679864819481654 ) ) ;
#83075 = ORIENTED_EDGE ( 'NONE', *, *, #32433, .T. ) ;
#83076 = CARTESIAN_POINT ( 'NONE',  ( 12.63842701281683922, 29.55059781766745175, -9.846743663894590881 ) ) ;
#83077 = ORIENTED_EDGE ( 'NONE', *, *, #75076, .F. ) ;
#83078 = CARTESIAN_POINT ( 'NONE',  ( 2.791683348922240793, 66.63393115100079456, 7.208316651077764092 ) ) ;
#83079 = CARTESIAN_POINT ( 'NONE',  ( 0.1955144967548914092, 24.32703681773340421, -6.500000000002779998 ) ) ;
#83080 = CARTESIAN_POINT ( 'NONE',  ( -4.164238869374099927, 2.012082168247300906, 3.795296366450308767 ) ) ;
#83081 = CARTESIAN_POINT ( 'NONE',  ( -1.926860441876562247, 7.453790035174473694, -3.195792623639530650 ) ) ;
#83082 = CARTESIAN_POINT ( 'NONE',  ( 0.000000000000000000, 0.000000000000000000, 0.000000000000000000 ) ) ;
#83083 = CARTESIAN_POINT ( 'NONE',  ( 19.42250999205614193, 10.14701867748816966, 5.440088680355555262 ) ) ;
#83084 = CARTESIAN_POINT ( 'NONE',  ( 1.114591949025029338, 4.390405144365474573E-16, -14.45709807627964416 ) ) ;
#83085 = ORIENTED_EDGE ( 'NONE', *, *, #58588, .F. ) ;
#83086 = DIRECTION ( 'NONE',  ( 8.673617379884027583E-16, 1.000000000000000000, 0.000000000000000000 ) ) ;
#83087 = CARTESIAN_POINT ( 'NONE',  ( 7.361572987183169658, 44.96726448433412315, -9.846743663894592657 ) ) ;
#83088 = CARTESIAN_POINT ( 'NONE',  ( 10.93781366033349833, 14.49999999999999112, -10.26470809774071569 ) ) ;
#83089 = CARTESIAN_POINT ( 'NONE',  ( -1.099225684535947600, 24.54030133659708923, 6.408140936763237150 ) ) ;
#83090 = CARTESIAN_POINT ( 'NONE',  ( 1.472469842513823179, 20.59226448433411960, -4.923371831947296329 ) ) ;
#83091 = CYLINDRICAL_SURFACE ( 'NONE', #64905, 1.499999999999998890 ) ;
#83092 = CARTESIAN_POINT ( 'NONE',  ( 0.1532563361054082862, 66.21726448433413736, 2.638427012816831674 ) ) ;
#83093 =( NAMED_UNIT ( * ) PLANE_ANGLE_UNIT ( ) SI_UNIT ( $, .RADIAN. ) );
#83094 = EDGE_CURVE ( 'NONE', #58939, #84500, #85092, .T. ) ;
#83095 = ORIENTED_EDGE ( 'NONE', *, *, #8322, .T. ) ;
#83096 = VERTEX_POINT ( 'NONE', #34218 ) ;
#83097 = EDGE_CURVE ( 'NONE', #4700, #43197, #18761, .T. ) ;
#83098 = CARTESIAN_POINT ( 'NONE',  ( -0.8801773607111009756, 18.06368534415484106, 1.068504757029289695E-15 ) ) ;
#83099 = CARTESIAN_POINT ( 'NONE',  ( 24.16423886937409904, 19.09541550158063927, 3.795296366450317205 ) ) ;
#83100 = CARTESIAN_POINT ( 'NONE',  ( 19.84674366389459266, 23.71726448433412315, -2.638427012816827677 ) ) ;
#83101 = CARTESIAN_POINT ( 'NONE',  ( 20.88017736071110875, 60.77201867748817676, -2.915334737309920765 ) ) ;
#83103 = CARTESIAN_POINT ( 'NONE',  ( 0.000000000000000000, 14.49999999999999822, 0.000000000000000000 ) ) ;
#83102 = CARTESIAN_POINT ( 'NONE',  ( -1.099225684535947600, 44.54030133659708923, 6.408140936763237150 ) ) ;
#83104 = CARTESIAN_POINT ( 'NONE',  ( 17.96484262340118221, 14.93868534415483751, 7.964842623401181321 ) ) ;
#83105 = CARTESIAN_POINT ( 'NONE',  ( 7.002992508389039195, 15.00000000000000533, -12.84003923133018077 ) ) ;
#83106 = DIRECTION ( 'NONE',  ( -0.000000000000000000, 1.000000000000000000, 0.000000000000000000 ) ) ;
#83107 = CARTESIAN_POINT ( 'NONE',  ( 16.40814093676324603, 7.456968003263754419, -11.09922568453594671 ) ) ;
#83108 = CARTESIAN_POINT ( 'NONE',  ( 19.84674366389459266, 28.71726448433411960, -2.638427012816827677 ) ) ;
#83109 = CARTESIAN_POINT ( 'NONE',  ( 3.469446951953614189E-15, -15.68631465584515539, 10.88017736071110342 ) ) ;
#83110 = CARTESIAN_POINT ( 'NONE',  ( 22.81628187352647785, 36.62363466993041783, 6.195893100308588602E-16 ) ) ;
#83111 = LINE ( 'NONE', #21637, #14918 ) ;
#83113 = DIRECTION ( 'NONE',  ( 0.000000000000000000, -0.000000000000000000, 1.000000000000000000 ) ) ;
#83112 = CARTESIAN_POINT ( 'NONE',  ( 15.44008868035555260, 34.73035201082151247, 9.422509992056143702 ) ) ;
#83114 = LINE ( 'NONE', #145, #22685 ) ;
#83115 = CARTESIAN_POINT ( 'NONE',  ( 4.559911319644449179, 68.89701867748817676, 9.422509992056141925 ) ) ;
#83116 = CARTESIAN_POINT ( 'NONE',  ( -0.8801773607111009756, 38.06368534415484106, 1.068504757029289695E-15 ) ) ;
#83117 =( GEOMETRIC_REPRESENTATION_CONTEXT ( 3 ) GLOBAL_UNCERTAINTY_ASSIGNED_CONTEXT ( ( #23273 ) ) GLOBAL_UNIT_ASSIGNED_CONTEXT ( ( #6774, #29750, #45257 ) ) REPRESENTATION_CONTEXT ( 'NONE', 'WORKASPACE' ) );
#83118 = CARTESIAN_POINT ( 'NONE',  ( 15.44008868035555260, 39.73035201082150536, 9.422509992056143702 ) ) ;
#83119 = CARTESIAN_POINT ( 'NONE',  ( 12.63842701281683922, 64.55059781766745175, -9.846743663894590881 ) ) ;
#83120 = CARTESIAN_POINT ( 'NONE',  ( 20.88017736071110875, 65.77201867748817676, -2.915334737309920765 ) ) ;
#83121 = UNCERTAINTY_MEASURE_WITH_UNIT (LENGTH_MEASURE( 1.000000000000000082E-05 ), #64268, 'distance_accuracy_value', 'NONE');
#83122 = CARTESIAN_POINT ( 'NONE',  ( 19.84674366389459266, 38.30059781766745175, 2.638427012816836559 ) ) ;
#83123 = CARTESIAN_POINT ( 'NONE',  ( 4.559911319644449179, 8.897018677488171434, 9.422509992056141925 ) ) ;
#83124 = VECTOR ( 'NONE', #24972, 1000.000000000000000 ) ;
#83125 = CARTESIAN_POINT ( 'NONE',  ( 6.565887622018943937, 18.08196800326375708, -12.81628187352647608 ) ) ;
#83126 = ORIENTED_EDGE ( 'NONE', *, *, #92578, .F. ) ;
#83127 = CARTESIAN_POINT ( 'NONE',  ( 19.42250999205614548, 25.98035201082150891, -5.440088680355545492 ) ) ;
#83128 = PLANE ( 'NONE',  #87640 ) ;
#83129 = EDGE_CURVE ( 'NONE', #49599, #41530, #17778, .T. ) ;
#83130 = CARTESIAN_POINT ( 'NONE',  ( 4.559911319644449179, 2.230352010821504471, -9.422509992056141925 ) ) ;
#83131 = CARTESIAN_POINT ( 'NONE',  ( 4.559911319644449179, 33.89701867748817676, 9.422509992056141925 ) ) ;
#83132 = CARTESIAN_POINT ( 'NONE',  ( 2.791683348922237240, 5.383931151000785675, -7.208316651077763204 ) ) ;
#83133 = CARTESIAN_POINT ( 'NONE',  ( 24.16423886937410614, 44.30374883491397497, 8.672049930838204340E-16 ) ) ;
#83134 = CARTESIAN_POINT ( 'NONE',  ( 19.84674366389459266, 23.30059781766745530, 2.638427012816836559 ) ) ;
#83135 = CARTESIAN_POINT ( 'NONE',  ( 7.084665262690076126, 44.10535201082151247, 10.88017736071109987 ) ) ;
#83136 =( BOUNDED_CURVE ( )  B_SPLINE_CURVE ( 2, ( #53392, #84888, #38905, #39398, #92868, #15432, #24398, #16889, #7914 ),
 .UNSPECIFIED., .F., .F. ) 
 B_SPLINE_CURVE_WITH_KNOTS ( ( 3, 2, 2, 2, 3 ),
 ( 0.5829980797973742801, 0.5833333333333333703, 0.5892857142857143016, 0.5952380952380952328, 0.5955733487740544341 ),
 .UNSPECIFIED. ) 
 CURVE ( )  GEOMETRIC_REPRESENTATION_ITEM ( )  RATIONAL_B_SPLINE_CURVE ( ( 0.9963778908391764944, 0.9980808541467923733, 1.000000000000000000, 0.9659258262890683122, 1.000000000000000000, 0.9659258262890683122, 1.000000000000000000, 0.9980808541467918182, 0.9963778908391756062 ) ) 
 REPRESENTATION_ITEM ( '' )  );
#83137 = DIRECTION ( 'NONE',  ( 0.000000000000000000, 1.000000000000000000, 0.000000000000000000 ) ) ;
#83138 = VECTOR ( 'NONE', #80707, 1000.000000000000114 ) ;
#83139 = ORIENTED_EDGE ( 'NONE', *, *, #54625, .T. ) ;
#83140 = PLANE ( 'NONE',  #88053 ) ;
#83141 = CARTESIAN_POINT ( 'NONE',  ( 5.076628168052704559, 55.17559781766745175, -8.527530157486179263 ) ) ;
#83142 = ORIENTED_EDGE ( 'NONE', *, *, #50795, .F. ) ;
#83143 = VERTEX_POINT ( 'NONE', #10763 ) ;
#83144 = DIRECTION ( 'NONE',  ( -0.3173046564050965856, 0.000000000000000000, 0.9483236552061978797 ) ) ;
#83145 = CARTESIAN_POINT ( 'NONE',  ( -4.164238869374098151, 21.59541550158063217, -3.795296366450310543 ) ) ;
#83146 = CARTESIAN_POINT ( 'NONE',  ( -4.164238869374099927, 17.01208216824730357, 3.795296366450308767 ) ) ;
#83147 = CARTESIAN_POINT ( 'NONE',  ( 0.5774900079438590739, 62.64701867748817676, -5.440088680355550821 ) ) ;
#83148 = CARTESIAN_POINT ( 'NONE',  ( 24.16423886937410614, 64.51208216824728936, -3.795296366450302550 ) ) ;
#83149 = CARTESIAN_POINT ( 'NONE',  ( 18.52753015748617571, 48.09226448433412315, 4.923371831947298993 ) ) ;
#83150 = CARTESIAN_POINT ( 'NONE',  ( -7.750000000000000000, 1.019547802438466100, 4.000000000000000000 ) ) ;
#83152 = CARTESIAN_POINT ( 'NONE',  ( 6.565887622018943937, 15.16530133659708568, 12.81628187352647430 ) ) ;
#83151 = CARTESIAN_POINT ( 'NONE',  ( 2.035157376598824452, 48.68868534415483396, 7.964842623401179544 ) ) ;
#83153 = CARTESIAN_POINT ( 'NONE',  ( 13.79529636645031943, 15.34541550158063750, -14.16423886937409904 ) ) ;
#83154 = CARTESIAN_POINT ( 'NONE',  ( 19.42250999205614193, 15.14701867748817143, 5.440088680355555262 ) ) ;
#83155 = CARTESIAN_POINT ( 'NONE',  ( 17.96484262340118221, 21.18868534415483396, -7.964842623401177768 ) ) ;
#83156 =( LENGTH_UNIT ( ) NAMED_UNIT ( * ) SI_UNIT ( .MILLI., .METRE. ) );
#83157 = CARTESIAN_POINT ( 'NONE',  ( 12.91533473730993009, 61.60535201082150536, -10.88017736071109987 ) ) ;
#83158 = CARTESIAN_POINT ( 'NONE',  ( -1.099225684535947600, 48.70696800326375353, -6.408140936763238038 ) ) ;
#83159 = CARTESIAN_POINT ( 'NONE',  ( -7.208316651077764980, -19.61606884899921255, -7.208316651077759651 ) ) ;
#83160 = EDGE_LOOP ( 'NONE', ( #96169, #69694, #35146, #40214 ) ) ;
#83161 = DIRECTION ( 'NONE',  ( 0.000000000000000000, 0.000000000000000000, -1.000000000000000000 ) ) ;
#83162 = ORIENTED_EDGE ( 'NONE', *, *, #31652, .T. ) ;
#83163 = DIRECTION ( 'NONE',  ( 0.000000000000000000, 0.000000000000000000, 1.000000000000000000 ) ) ;
#83164 = EDGE_LOOP ( 'NONE', ( #11950, #92771, #89219, #81438 ) ) ;
#83165 = DIRECTION ( 'NONE',  ( 1.000000000000000000, 0.000000000000000000, 0.000000000000000000 ) ) ;
#83167 = CARTESIAN_POINT ( 'NONE',  ( 17.96484262340118221, 4.938685344154837509, 7.964842623401181321 ) ) ;
#83166 = CARTESIAN_POINT ( 'NONE',  ( 20.36894250292379738, 64.92874883491397497, -10.36894250292379027 ) ) ;
#83169 = CARTESIAN_POINT ( 'NONE',  ( 5.076628168052703671, 46.84226448433412315, 8.527530157486179263 ) ) ;
#83168 = CARTESIAN_POINT ( 'NONE',  ( 2.791683348922237240, 25.38393115100078390, -7.208316651077763204 ) ) ;
#83170 = CARTESIAN_POINT ( 'NONE',  ( 20.88017736071110875, 65.77201867748817676, -2.915334737309920765 ) ) ;
#83171 = CARTESIAN_POINT ( 'NONE',  ( -2.189108318723844704, 15.00000000000000178, 14.46085460646896870 ) ) ;
#83172 = CARTESIAN_POINT ( 'NONE',  ( 5.076628168052703671, 1.842264484334118047, 8.527530157486179263 ) ) ;
#83173 = AXIS2_PLACEMENT_3D ( 'NONE', #48149, #3161, #47669 ) ;
#83174 = CARTESIAN_POINT ( 'NONE',  ( 12.81628187352647608, 16.41530133659708923, 3.434112377981052511 ) ) ;
#83175 = ORIENTED_EDGE ( 'NONE', *, *, #21271, .F. ) ;
#83176 = CARTESIAN_POINT ( 'NONE',  ( 2.917880565312950480, 30.97041550158063572, -12.26659068614894821 ) ) ;
#83177 = CARTESIAN_POINT ( 'NONE',  ( -4.164238869374099039, 36.80374883491396787, 8.674139862899312516E-16 ) ) ;
#83178 = VERTEX_POINT ( 'NONE', #79745 ) ;
#83179 = CARTESIAN_POINT ( 'NONE',  ( 6.565887622018943937, 60.16530133659707502, 12.81628187352647430 ) ) ;
#83180 = CARTESIAN_POINT ( 'NONE',  ( 2.035157376598822676, 27.43868534415483396, -7.964842623401177768 ) ) ;
#83181 = CARTESIAN_POINT ( 'NONE',  ( 14.92337183194729988, 39.34226448433412315, -8.527530157486177487 ) ) ;
#83182 = CARTESIAN_POINT ( 'NONE',  ( 20.88017736071110519, 30.56368534415484106, 2.639326808657452039E-16 ) ) ;
#83183 = CARTESIAN_POINT ( 'NONE',  ( 13.43411237798105340, 60.58196800326376064, 12.81628187352647963 ) ) ;
#83184 = DIRECTION ( 'NONE',  ( -0.000000000000000000, 1.000000000000000000, -0.000000000000000000 ) ) ;
#83185 = CARTESIAN_POINT ( 'NONE',  ( 5.076628168052703671, 56.84226448433412315, 8.527530157486179263 ) ) ;
#83186 = CARTESIAN_POINT ( 'NONE',  ( 7.361572987183170547, 52.05059781766745175, 9.846743663894590881 ) ) ;
#83187 =( GEOMETRIC_REPRESENTATION_CONTEXT ( 3 ) GLOBAL_UNCERTAINTY_ASSIGNED_CONTEXT ( ( #34415 ) ) GLOBAL_UNIT_ASSIGNED_CONTEXT ( ( #44707, #65723, #98235 ) ) REPRESENTATION_CONTEXT ( 'NONE', 'WORKASPACE' ) );
#83188 = ADVANCED_FACE ( 'NONE', ( #78265 ), #40277, .T. ) ;
#83191 = ORIENTED_EDGE ( 'NONE', *, *, #54565, .T. ) ;
#83190 = CIRCLE ( 'NONE', #95979, 15.00000000000000000 ) ;
#83189 = CARTESIAN_POINT ( 'NONE',  ( 2.603489959281613420, 45.43575266056827644, -6.500000000000031086 ) ) ;
#83192 = DIRECTION ( 'NONE',  ( -1.000000000000000000, 0.000000000000000000, 0.000000000000000000 ) ) ;
#83193 = DIRECTION ( 'NONE',  ( -0.9099612708765455471, 0.000000000000000000, 0.4146932426562339735 ) ) ;
#83194 = DIRECTION ( 'NONE',  ( 0.000000000000000000, 0.000000000000000000, 1.000000000000000000 ) ) ;
#83195 = ORIENTED_EDGE ( 'NONE', *, *, #73651, .F. ) ;
#83196 = CARTESIAN_POINT ( 'NONE',  ( 19.54820696779682976, 81.00406362210809164, 5.000000000000000000 ) ) ;
#83197 = CARTESIAN_POINT ( 'NONE',  ( 10.00000000000000178, 27.25893115100078390, 9.846743663894594434 ) ) ;
#83198 = CARTESIAN_POINT ( 'NONE',  ( 20.15039907845753575, 10.60158574516642460, -6.262539305110077059 ) ) ;
#83199 = CARTESIAN_POINT ( 'NONE',  ( 0.6178305044545838731, 39.74863466993041072, 9.382169495545420901 ) ) ;
#83200 = VECTOR ( 'NONE', #91745, 1000.000000000000000 ) ;
#83201 = CARTESIAN_POINT ( 'NONE',  ( -6.382347221874512755, 0.5000000000000004441, 13.57444820018223375 ) ) ;
#83202 = ORIENTED_EDGE ( 'NONE', *, *, #43046, .T. ) ;
#83203 = CARTESIAN_POINT ( 'NONE',  ( 7.361572987183169658, 59.96726448433410894, -9.846743663894592657 ) ) ;
#83204 = CARTESIAN_POINT ( 'NONE',  ( -5.419894505350392855, 15.00000000000000000, -13.98659156302466045 ) ) ;
#83205 = CARTESIAN_POINT ( 'NONE',  ( 2.791683348922237240, 35.38393115100079456, -7.208316651077763204 ) ) ;
#83206 = CARTESIAN_POINT ( 'NONE',  ( 2.917880565312950480, 35.97041550158063217, -12.26659068614894821 ) ) ;
#83207 = CARTESIAN_POINT ( 'NONE',  ( 5.076628168052703671, 46.84226448433412315, 8.527530157486179263 ) ) ;
#83208 = CARTESIAN_POINT ( 'NONE',  ( -1.099225684535947600, 64.54030133659709634, 6.408140936763237150 ) ) ;
#83210 = CARTESIAN_POINT ( 'NONE',  ( -19.00000000000000000, 75.76920769491739804, -2.900000000000000799 ) ) ;
#83209 = APPLICATION_CONTEXT ( 'automotive_design' ) ;
#83211 = CARTESIAN_POINT ( 'NONE',  ( 5.076628168052703671, 1.842264484334118047, 8.527530157486179263 ) ) ;
#83212 = CARTESIAN_POINT ( 'NONE',  ( 10.00000000000000000, 5.553748834913967869, -14.16423886937410082 ) ) ;
#83213 = CARTESIAN_POINT ( 'NONE',  ( 7.361572987183169658, 44.96726448433412315, -9.846743663894592657 ) ) ;
#83214 = CARTESIAN_POINT ( 'NONE',  ( 10.00000000000000000, 36.81368534415484106, -10.88017736071110342 ) ) ;
#83215 = LINE ( 'NONE', #44714, #57103 ) ;
#83216 = EDGE_CURVE ( 'NONE', #92463, #74651, #4501, .T. ) ;
#83217 = CARTESIAN_POINT ( 'NONE',  ( 15.44008868035555260, 44.73035201082151247, 9.422509992056143702 ) ) ;
#83218 = VERTEX_POINT ( 'NONE', #71272 ) ;
#83219 = EDGE_CURVE ( 'NONE', #90159, #14667, #64142, .T. ) ;
#83220 = DIRECTION ( 'NONE',  ( 0.000000000000000000, 1.000000000000000000, 0.000000000000000000 ) ) ;
#83221 = CARTESIAN_POINT ( 'NONE',  ( 0.5774900079438607392, 13.48035201082150358, 5.440088680355550821 ) ) ;
#83223 = CARTESIAN_POINT ( 'NONE',  ( 0.5774900079438590739, 37.64701867748817676, -5.440088680355550821 ) ) ;
#83222 = CARTESIAN_POINT ( 'NONE',  ( 3.591859063236761518, -0.04303199673624671928, 11.09922568453594849 ) ) ;
#83224 = CARTESIAN_POINT ( 'NONE',  ( -0.8801773607111008646, 68.27201867748817676, 2.915334737309923430 ) ) ;
#83226 = CARTESIAN_POINT ( 'NONE',  ( 24.35999999999999233, 37.99999999999997868, -9.500000000000000000 ) ) ;
#83225 = CARTESIAN_POINT ( 'NONE',  ( 4.559911319644449179, 38.89701867748817676, 9.422509992056141925 ) ) ;
#83227 = CARTESIAN_POINT ( 'NONE',  ( 1.472469842513823179, 16.42559781766745175, 4.923371831947296329 ) ) ;
#83228 = CARTESIAN_POINT ( 'NONE',  ( 10.00000000000000178, 42.25893115100078745, 9.846743663894594434 ) ) ;
#83229 = CARTESIAN_POINT ( 'NONE',  ( -3.927832320392339316, -0.03417435944610275333, 13.69797916712101404 ) ) ;
#83230 = CARTESIAN_POINT ( 'NONE',  ( 10.36894250292379027, 13.67874883491396254, 10.36894250292378672 ) ) ;
#83231 = CARTESIAN_POINT ( 'NONE',  ( 14.92337183194729988, 64.34226448433412315, -8.527530157486177487 ) ) ;
#83232 = CARTESIAN_POINT ( 'NONE',  ( -4.164238869374098151, 66.59541550158060375, -3.795296366450310543 ) ) ;
#83233 = AXIS2_PLACEMENT_3D ( 'NONE', #44362, #6363, #43860 ) ;
#83235 = AXIS2_PLACEMENT_3D ( 'NONE', #56424, #87881, #49393 ) ;
#83234 = DIRECTION ( 'NONE',  ( 0.000000000000000000, 1.000000000000000000, 0.000000000000000000 ) ) ;
#83236 = CARTESIAN_POINT ( 'NONE',  ( 6.204703633549690345, 22.84541550158062861, 14.16423886937410082 ) ) ;
#83237 = CARTESIAN_POINT ( 'NONE',  ( 10.00000000000000000, 50.55374883491396787, -14.16423886937410082 ) ) ;
#83238 = CARTESIAN_POINT ( 'NONE',  ( -10.77730536144846596, -98.63085534186639336, -3.750000000000000000 ) ) ;
#83239 = CIRCLE ( 'NONE', #89586, 2.999999999999999112 ) ;
#83240 = ORIENTED_EDGE ( 'NONE', *, *, #49046, .T. ) ;
#83241 = CARTESIAN_POINT ( 'NONE',  ( 12.63842701281683922, 24.55059781766745175, -9.846743663894590881 ) ) ;
#83242 = CARTESIAN_POINT ( 'NONE',  ( 4.559911319644449179, 32.23035201082150536, -9.422509992056141925 ) ) ;
#83243 = CARTESIAN_POINT ( 'NONE',  ( 17.20831665107776587, 44.13393115100078745, -7.208316651077762316 ) ) ;
#83245 = CARTESIAN_POINT ( 'NONE',  ( 2.603489959281584998, 6.582109641433292246, 6.499999999999998224 ) ) ;
#83244 = CARTESIAN_POINT ( 'NONE',  ( -0.3689425029237898834, 6.178748834913968757, -10.36894250292378850 ) ) ;
#83246 = CARTESIAN_POINT ( 'NONE',  ( -11.62719953690073282, 0.3639310419529863116, 9.476720473301741166 ) ) ;
#83247 =( BOUNDED_CURVE ( )  B_SPLINE_CURVE ( 2, ( #60927, #69923, #84919, #91433, #22960, #76919, #31896, #54897, #85412 ),
 .UNSPECIFIED., .F., .F. ) 
 B_SPLINE_CURVE_WITH_KNOTS ( ( 3, 2, 2, 2, 3 ),
 ( 0.1187123655116599508, 0.1190476190476190688, 0.1250000000000000000, 0.1309523809523809312, 0.1312876344883400492 ),
 .UNSPECIFIED. ) 
 CURVE ( )  GEOMETRIC_REPRESENTATION_ITEM ( )  RATIONAL_B_SPLINE_CURVE ( ( 0.9963778908391762723, 0.9980808541467921513, 1.000000000000000000, 0.9659258262890683122, 1.000000000000000000, 0.9659258262890683122, 1.000000000000000000, 0.9980808541467922623, 0.9963778908391764944 ) ) 
 REPRESENTATION_ITEM ( '' )  );
#83248 = DIRECTION ( 'NONE',  ( -0.3665012267243009103, 0.000000000000000000, 0.9304175679820230194 ) ) ;
#83249 = CARTESIAN_POINT ( 'NONE',  ( -1.099225684535947600, 38.70696800326375353, -6.408140936763238038 ) ) ;
#83250 = CARTESIAN_POINT ( 'NONE',  ( 2.791683348922240793, 46.63393115100077324, 7.208316651077764092 ) ) ;
#83251 = ORIENTED_EDGE ( 'NONE', *, *, #63713, .T. ) ;
#83252 = CARTESIAN_POINT ( 'NONE',  ( 0.1532563361054100626, 5.800597817667452638, -2.638427012816831230 ) ) ;
#83253 = CARTESIAN_POINT ( 'NONE',  ( 10.58840669699852199, -98.14374106289703548, -4.000000000000000000 ) ) ;
#83254 = CARTESIAN_POINT ( 'NONE',  ( -14.76044511231987322, 14.76984987353748835, 2.313329003771987136 ) ) ;
#83255 = CARTESIAN_POINT ( 'NONE',  ( 20.88017736071110164, 15.35535201082150358, 2.915334737309930979 ) ) ;
#83256 = CARTESIAN_POINT ( 'NONE',  ( 24.16423886937410614, 54.51208216824730357, -3.795296366450302550 ) ) ;
#83257 = CARTESIAN_POINT ( 'NONE',  ( 19.42250999205614548, 40.98035201082150536, -5.440088680355545492 ) ) ;
#83258 = CARTESIAN_POINT ( 'NONE',  ( 24.16423886937410614, 4.512082168247300906, -3.795296366450302550 ) ) ;
#83259 = CARTESIAN_POINT ( 'NONE',  ( 6.000000000000000000, 61.50000000000000711, -6.000000000000000000 ) ) ;
#83260 = CARTESIAN_POINT ( 'NONE',  ( 14.92337183194729633, 17.67559781766745175, 8.527530157486181039 ) ) ;
#83261 = CARTESIAN_POINT ( 'NONE',  ( 12.91533473730992121, 4.522018677488169658, 10.88017736071110164 ) ) ;
#83262 = CARTESIAN_POINT ( 'NONE',  ( 18.52753015748618282, 43.92559781766745175, -4.923371831947291888 ) ) ;
#83263 = CARTESIAN_POINT ( 'NONE',  ( 12.63842701281683922, 49.55059781766744464, -9.846743663894590881 ) ) ;
#83264 = EDGE_CURVE ( 'NONE', #40405, #14972, #54765, .T. ) ;
#83265 = CARTESIAN_POINT ( 'NONE',  ( 7.084665262690076126, 42.02201867748816966, -10.88017736071110164 ) ) ;
#83266 = UNCERTAINTY_MEASURE_WITH_UNIT (LENGTH_MEASURE( 1.000000000000000082E-05 ), #85236, 'distance_accuracy_value', 'NONE');
#83267 = VERTEX_POINT ( 'NONE', #41278 ) ;
#83268 = CARTESIAN_POINT ( 'NONE',  ( 0.6178305044545818747, 58.49863466993042493, -9.382169495545419124 ) ) ;
#83269 = CARTESIAN_POINT ( 'NONE',  ( 11.81378540890936080, 15.00000000000000000, -7.968498874458115999 ) ) ;
#83270 = CARTESIAN_POINT ( 'NONE',  ( 1.472469842513823179, 6.425597817667451750, 4.923371831947296329 ) ) ;
#83271 = CARTESIAN_POINT ( 'NONE',  ( 19.38216949554541557, 52.24863466993041072, -9.382169495545420901 ) ) ;
#83273 = CARTESIAN_POINT ( 'NONE',  ( 19.84674366389459266, 48.71726448433413026, -2.638427012816827677 ) ) ;
#83272 = CARTESIAN_POINT ( 'NONE',  ( 20.88017736071110875, 5.772018677488170546, -2.915334737309920765 ) ) ;
#83274 = CARTESIAN_POINT ( 'NONE',  ( 0.000000000000000000, 15.00000000000000000, 0.000000000000000000 ) ) ;
#83275 = SURFACE_STYLE_USAGE ( .BOTH. , #6291 ) ;
#83276 = CARTESIAN_POINT ( 'NONE',  ( 10.00000000000000178, 33.05374883491396787, 14.16423886937410082 ) ) ;
#83277 = CARTESIAN_POINT ( 'NONE',  ( -2.266590686148945544, 51.38708216824730357, -7.082119434687050408 ) ) ;
#83278 = CARTESIAN_POINT ( 'NONE',  ( 19.84674366389459621, 58.50893115100078745, 7.409399052514197653E-17 ) ) ;
#83279 = VECTOR ( 'NONE', #47469, 1000.000000000000000 ) ;
#83280 = DIRECTION ( 'NONE',  ( 1.257402221000611116E-16, -1.000000000000000000, 0.000000000000000000 ) ) ;
#83281 = CARTESIAN_POINT ( 'NONE',  ( 12.91533473730993009, 56.60535201082151247, -10.88017736071109987 ) ) ;
#83282 = CARTESIAN_POINT ( 'NONE',  ( 10.00000000000000000, -0.2410688489992152128, -9.846743663894594434 ) ) ;
#83283 = ORIENTED_EDGE ( 'NONE', *, *, #69692, .T. ) ;
#83284 = CARTESIAN_POINT ( 'NONE',  ( 0.6178305044545818747, 58.49863466993042493, -9.382169495545419124 ) ) ;
#83285 = VECTOR ( 'NONE', #75637, 1000.000000000000000 ) ;
#83286 = ORIENTED_EDGE ( 'NONE', *, *, #36054, .T. ) ;
#83287 = CARTESIAN_POINT ( 'NONE',  ( 0.5774900079438590739, 67.64701867748817676, -5.440088680355550821 ) ) ;
#83288 = EDGE_LOOP ( 'NONE', ( #19176, #18591, #71957, #23209 ) ) ;
#83289 = CARTESIAN_POINT ( 'NONE',  ( 10.00000000000000178, 3.053748834913967425, 14.16423886937410082 ) ) ;
#83290 = CARTESIAN_POINT ( 'NONE',  ( 19.84674366389459621, 3.508931151000785231, 7.409399052514197653E-17 ) ) ;
#83291 = CARTESIAN_POINT ( 'NONE',  ( 12.91533473730992121, 24.52201867748816966, 10.88017736071110164 ) ) ;
#83292 = CARTESIAN_POINT ( 'NONE',  ( 3.836325488036175457, 14.49999999999999112, -14.50112432709429378 ) ) ;
#83293 = ORIENTED_EDGE ( 'NONE', *, *, #31051, .F. ) ;
#83294 = CARTESIAN_POINT ( 'NONE',  ( 7.084665262690076126, 29.10535201082150181, 10.88017736071109987 ) ) ;
#83295 = ORIENTED_EDGE ( 'NONE', *, *, #16157, .F. ) ;
#83296 = DIRECTION ( 'NONE',  ( 0.000000000000000000, 0.000000000000000000, -1.000000000000000000 ) ) ;
#83297 = ORIENTED_EDGE ( 'NONE', *, *, #35159, .F. ) ;
#83298 = ORIENTED_EDGE ( 'NONE', *, *, #21152, .F. ) ;
#83299 = CARTESIAN_POINT ( 'NONE',  ( 22.81628187352648496, 21.83196800326374643, -3.434112377981050290 ) ) ;
#83300 = CARTESIAN_POINT ( 'NONE',  ( 1.472469842513823179, 0.5922644843341181575, -4.923371831947296329 ) ) ;
#83302 = CARTESIAN_POINT ( 'NONE',  ( 0.000000000000000000, 15.00000000000000000, 0.000000000000000000 ) ) ;
#83301 = CARTESIAN_POINT ( 'NONE',  ( 12.91533473730993009, 16.60535201082150891, -10.88017736071109987 ) ) ;
#83303 = CARTESIAN_POINT ( 'NONE',  ( 5.076628168052703671, 6.842264484334118713, 8.527530157486179263 ) ) ;
#83304 = CARTESIAN_POINT ( 'NONE',  ( 17.96484262340118221, 31.18868534415483751, -7.964842623401177768 ) ) ;
#83305 = COLOUR_RGB ( '', 0.72549020, 0.75294118, 0.79215686) ;
#83306 = EDGE_CURVE ( 'NONE', #40720, #76622, #98740, .T. ) ;
#83307 = ORIENTED_EDGE ( 'NONE', *, *, #49054, .T. ) ;
#83308 = COLOUR_RGB ( '', 0.31764706, 0.68627451, 0.89019608) ;
#83309 = ORIENTED_EDGE ( 'NONE', *, *, #64267, .T. ) ;
#83310 = CARTESIAN_POINT ( 'NONE',  ( 0.000000000000000000, 0.5000000000000004441, 0.000000000000000000 ) ) ;
#83311 = CARTESIAN_POINT ( 'NONE',  ( 20.88017736071110875, 40.77201867748818387, -2.915334737309920765 ) ) ;
#83312 = CARTESIAN_POINT ( 'NONE',  ( 0.000000000000000000, 0.5000000000000004441, 0.000000000000000000 ) ) ;
#83313 = CARTESIAN_POINT ( 'NONE',  ( 3.591859063236763294, 53.29030133659708923, -11.09922568453595026 ) ) ;
#83314 = CARTESIAN_POINT ( 'NONE',  ( 0.5774900079438590739, 62.64701867748817676, -5.440088680355550821 ) ) ;
#83315 = CARTESIAN_POINT ( 'NONE',  ( 10.00000000000000000, 64.75893115100078035, -9.846743663894594434 ) ) ;
#83316 = CARTESIAN_POINT ( 'NONE',  ( -7.199999999999996625, 99.99999999999998579, -8.525133428036873795 ) ) ;
#83317 = CARTESIAN_POINT ( 'NONE',  ( 14.92337183194729633, 17.67559781766745175, 8.527530157486181039 ) ) ;
#83318 = CARTESIAN_POINT ( 'NONE',  ( 13.43411237798105340, 50.58196800326375353, 12.81628187352647963 ) ) ;
#83319 = DIRECTION ( 'NONE',  ( 0.000000000000000000, 0.000000000000000000, 1.000000000000000000 ) ) ;
#83320 = CARTESIAN_POINT ( 'NONE',  ( 10.00000000000000000, -0.2410688489992152128, -9.846743663894594434 ) ) ;
#83321 = CARTESIAN_POINT ( 'NONE',  ( 3.591859063236761518, 4.956968003263753531, 11.09922568453594849 ) ) ;
#83323 = CARTESIAN_POINT ( 'NONE',  ( 2.791683348922237240, 65.38393115100078035, -7.208316651077763204 ) ) ;
#83322 =( LENGTH_UNIT ( ) NAMED_UNIT ( * ) SI_UNIT ( .MILLI., .METRE. ) );
#83324 = CARTESIAN_POINT ( 'NONE',  ( 10.00000000000000178, 29.31368534415483751, 10.88017736071110342 ) ) ;
#83325 = CARTESIAN_POINT ( 'NONE',  ( 1.472469842513823179, 50.59226448433411605, -4.923371831947296329 ) ) ;
#83326 = CARTESIAN_POINT ( 'NONE',  ( -0.3289641300567998083, 33.07879003517447813, 5.963430220938281678 ) ) ;
#83327 = CARTESIAN_POINT ( 'NONE',  ( 19.84674366389459621, 18.50893115100078745, 7.409399052514197653E-17 ) ) ;
#83328 = CARTESIAN_POINT ( 'NONE',  ( 5.076628168052703671, 11.84226448433411960, 8.527530157486179263 ) ) ;
#83330 = ORIENTED_EDGE ( 'NONE', *, *, #83097, .F. ) ;
#83329 = CARTESIAN_POINT ( 'NONE',  ( 16.40814093676323893, 0.7903013365970867898, 11.09922568453595026 ) ) ;
#83331 = AXIS2_PLACEMENT_3D ( 'NONE', #21436, #28436, #65440 ) ;
#83332 = CARTESIAN_POINT ( 'NONE',  ( 5.076628168052703671, 66.84226448433412315, 8.527530157486179263 ) ) ;
#83333 = ADVANCED_FACE ( 'NONE', ( #62766 ), #86760, .T. ) ;
#83334 = CARTESIAN_POINT ( 'NONE',  ( 4.655929185140254667, -8.243906417133416653, -2.499999999999999112 ) ) ;
#83335 = CARTESIAN_POINT ( 'NONE',  ( 20.88017736071110875, 5.772018677488170546, -2.915334737309920765 ) ) ;
#83336 = CARTESIAN_POINT ( 'NONE',  ( 1.472469842513823179, 40.59226448433411605, -4.923371831947296329 ) ) ;
#83337 = EDGE_LOOP ( 'NONE', ( #5207, #15669, #14470, #7729 ) ) ;
#83338 = COLOUR_RGB ( '', 0.40784314, 0.44705882, 0.49803922) ;
#83339 = CARTESIAN_POINT ( 'NONE',  ( 0.2751277870542891413, 24.36607318730131411, -6.499999999999989342 ) ) ;
#83340 = EDGE_CURVE ( 'NONE', #85384, #73925, #80728, .T. ) ;
#83341 = CARTESIAN_POINT ( 'NONE',  ( -0.3689425029237881626, 67.42874883491396076, 10.36894250292379027 ) ) ;
#83342 = LINE ( 'NONE', #23347, #5651 ) ;
#83343 = CARTESIAN_POINT ( 'NONE',  ( 12.91533473730992121, 29.52201867748817321, 10.88017736071110164 ) ) ;
#83344 = CARTESIAN_POINT ( 'NONE',  ( 17.08211943468705130, 48.47041550158063927, 12.26659068614894998 ) ) ;
#83346 = CARTESIAN_POINT ( 'NONE',  ( -9.990730578767625047, 46.91630561652144138, 0.000000000000000000 ) ) ;
#83345 = CARTESIAN_POINT ( 'NONE',  ( 4.559911319644449179, 3.897018677488171434, 9.422509992056141925 ) ) ;
#83347 = COLOUR_RGB ( '', 0.66274510, 0.83137255, 0.94901961) ;
#83348 = CARTESIAN_POINT ( 'NONE',  ( 7.361572987183169658, 29.96726448433411960, -9.846743663894592657 ) ) ;
#83349 = CARTESIAN_POINT ( 'NONE',  ( 13.43411237798105340, 15.58196800326374998, 12.81628187352647963 ) ) ;
#83350 = FACE_OUTER_BOUND ( 'NONE', #14198, .T. ) ;
#83351 = CARTESIAN_POINT ( 'NONE',  ( 7.361572987183170547, 57.05059781766744464, 9.846743663894590881 ) ) ;
#83352 = DIRECTION ( 'NONE',  ( 0.000000000000000000, 1.000000000000000000, 0.000000000000000000 ) ) ;
#83353 = CARTESIAN_POINT ( 'NONE',  ( -3.949999999999997069, 99.99999999999998579, 8.000000000000000000 ) ) ;
#83354 = CARTESIAN_POINT ( 'NONE',  ( 22.26659068614895176, 4.720415501580633943, -7.082119434687042414 ) ) ;
#83355 = B_SPLINE_CURVE_WITH_KNOTS ( 'NONE', 3,
 ( #65584, #19607, #2298, #4127, #13085, #74074 ),
 .UNSPECIFIED., .F., .F.,
 ( 4, 2, 4 ),
 ( 3.409110551361852929E-05, 0.0004400426677354470398, 0.0008459942299572755300 ),
 .UNSPECIFIED. ) ;
#83356 = CARTESIAN_POINT ( 'NONE',  ( 5.076628168052704559, 30.17559781766745175, -8.527530157486179263 ) ) ;
#83357 = DIRECTION ( 'NONE',  ( 1.000000000000000000, -5.818595309480553908E-17, 0.000000000000000000 ) ) ;
#83358 = CARTESIAN_POINT ( 'NONE',  ( 24.16423886937409904, 39.09541550158062506, 3.795296366450317205 ) ) ;
#83359 = PRODUCT_DEFINITION_SHAPE ( 'NONE', 'NONE',  #48898 ) ;
#83360 = CARTESIAN_POINT ( 'NONE',  ( 10.00000000000000178, 2.258931151000784787, 9.846743663894594434 ) ) ;
#83362 = CARTESIAN_POINT ( 'NONE',  ( -0.1503990784575328643, 35.12777174578612716, 6.262539305110068177 ) ) ;
#83361 = CARTESIAN_POINT ( 'NONE',  ( 26.00000000000000355, 35.99999999999997158, -10.00000000000000000 ) ) ;
#83363 = CARTESIAN_POINT ( 'NONE',  ( 4.559911319644449179, 32.23035201082150536, -9.422509992056141925 ) ) ;
#83364 = CARTESIAN_POINT ( 'NONE',  ( 16.40814093676323893, 55.79030133659708923, 11.09922568453595026 ) ) ;
#83365 = CARTESIAN_POINT ( 'NONE',  ( 0.5774900079438607392, 3.480352010821504027, 5.440088680355550821 ) ) ;
#83367 = VERTEX_POINT ( 'NONE', #97237 ) ;
#83366 = CARTESIAN_POINT ( 'NONE',  ( 6.565887622018943937, 33.08196800326374643, -12.81628187352647608 ) ) ;
#83368 = VERTEX_POINT ( 'NONE', #81700 ) ;
#83369 = LINE ( 'NONE', #14391, #3981 ) ;
#83370 = LINE ( 'NONE', #37393, #38295 ) ;
#83371 = CARTESIAN_POINT ( 'NONE',  ( 17.08211943468705130, 43.47041550158063927, 12.26659068614894998 ) ) ;
#83372 = CARTESIAN_POINT ( 'NONE',  ( 2.917880565312948704, 17.63708216824730357, 12.26659068614894643 ) ) ;
#83373 = CARTESIAN_POINT ( 'NONE',  ( 17.96484262340118221, 11.18868534415483929, -7.964842623401177768 ) ) ;
#83374 = CARTESIAN_POINT ( 'NONE',  ( 20.88017736071110519, 40.56368534415484106, 2.639326808657452039E-16 ) ) ;
#83375 = CARTESIAN_POINT ( 'NONE',  ( 0.000000000000000000, 14.49999999999999822, 0.000000000000000000 ) ) ;
#83376 = DIRECTION ( 'NONE',  ( 0.5547001962252290364, 0.8320502943378437211, 0.000000000000000000 ) ) ;
#83377 = CARTESIAN_POINT ( 'NONE',  ( 4.559911319644449179, 57.23035201082150536, -9.422509992056141925 ) ) ;
#83378 = CARTESIAN_POINT ( 'NONE',  ( 15.44008868035555260, 64.73035201082151957, 9.422509992056143702 ) ) ;
#83379 = CARTESIAN_POINT ( 'NONE',  ( 22.81628187352647785, 21.62363466993041783, 6.195893100308588602E-16 ) ) ;
#83380 = CARTESIAN_POINT ( 'NONE',  ( -5.815488105659849083, 0.2301500539507708720, 13.76235181012714293 ) ) ;
#83381 = CARTESIAN_POINT ( 'NONE',  ( 20.03743638938523119, 26.75197528031018734, 6.399506433553979079 ) ) ;
#83382 = CARTESIAN_POINT ( 'NONE',  ( 12.63842701281683034, 42.46726448433412315, 9.846743663894596210 ) ) ;
#83383 = EDGE_CURVE ( 'NONE', #935, #75686, #8044, .T. ) ;
#83384 = B_SPLINE_CURVE_WITH_KNOTS ( 'NONE', 3,
 ( #84081, #15596, #45081, #37106, #66605, #89601 ),
 .UNSPECIFIED., .F., .F.,
 ( 4, 2, 4 ),
 ( 0.000000000000000000, 0.0002701661927229330050, 0.0005403323854458660100 ),
 .UNSPECIFIED. ) ;
#83385 = UNCERTAINTY_MEASURE_WITH_UNIT (LENGTH_MEASURE( 1.000000000000000082E-05 ), #5455, 'distance_accuracy_value', 'NONE');
#83386 = VECTOR ( 'NONE', #36059, 1000.000000000000114 ) ;
#83387 = CARTESIAN_POINT ( 'NONE',  ( 3.591859063236761518, 19.95696800326375353, 11.09922568453594849 ) ) ;
#83388 = FACE_OUTER_BOUND ( 'NONE', #20627, .T. ) ;
#83389 = CARTESIAN_POINT ( 'NONE',  ( 19.42250999205614193, 5.147018677488171434, 5.440088680355555262 ) ) ;
#83390 = CARTESIAN_POINT ( 'NONE',  ( 7.361572987183170547, 42.05059781766745886, 9.846743663894590881 ) ) ;
#83391 = CARTESIAN_POINT ( 'NONE',  ( 34.56412365047463453, 13.99999999999999645, -9.500000000000000000 ) ) ;
#83392 = CARTESIAN_POINT ( 'NONE',  ( 5.076628168052704559, 15.17559781766745175, -8.527530157486179263 ) ) ;
#83393 = CARTESIAN_POINT ( 'NONE',  ( 13.79529636645031943, 5.345415501580634832, -14.16423886937409904 ) ) ;
#83394 = DIRECTION ( 'NONE',  ( 0.8070303256584299145, -0.5905099943842175847, 0.000000000000000000 ) ) ;
#83395 = CARTESIAN_POINT ( 'NONE',  ( 4.559911319644449179, 32.23035201082150536, -9.422509992056141925 ) ) ;
#83397 = CARTESIAN_POINT ( 'NONE',  ( 10.00000000000000000, 30.55374883491397142, -14.16423886937410082 ) ) ;
#83396 = CARTESIAN_POINT ( 'NONE',  ( 4.559911319644449179, 2.230352010821504471, -9.422509992056141925 ) ) ;
#83398 = ADVANCED_FACE ( 'NONE', ( #80230 ), #28211, .F. ) ;
#83399 = CARTESIAN_POINT ( 'NONE',  ( -0.8801773607111009756, 33.06368534415484106, 1.068504757029289695E-15 ) ) ;
#83400 = CARTESIAN_POINT ( 'NONE',  ( -0.8801773607110991993, 22.85535201082150181, -2.915334737309923874 ) ) ;
#83401 = EDGE_LOOP ( 'NONE', ( #62699, #89064, #47218, #39701, #42286, #87592 ) ) ;
#83402 = CARTESIAN_POINT ( 'NONE',  ( 10.00000000000000000, 31.81368534415483751, -10.88017736071110342 ) ) ;
#83403 = CARTESIAN_POINT ( 'NONE',  ( 6.565887622018943937, 43.08196800326374643, -12.81628187352647608 ) ) ;
#83404 = CARTESIAN_POINT ( 'NONE',  ( 2.035157376598824452, 43.68868534415484106, 7.964842623401179544 ) ) ;
#83406 = CARTESIAN_POINT ( 'NONE',  ( 19.42250999205614193, 50.14701867748817676, 5.440088680355555262 ) ) ;
#83405 = CARTESIAN_POINT ( 'NONE',  ( -5.999999999999994671, 43.00000000000000000, -4.250000000000000000 ) ) ;
#83407 = CIRCLE ( 'NONE', #40298, 19.43999999999999773 ) ;
#83408 = ORIENTED_EDGE ( 'NONE', *, *, #97546, .T. ) ;
#83409 = CARTESIAN_POINT ( 'NONE',  ( 12.91533473730992121, 34.52201867748817676, 10.88017736071110164 ) ) ;
#83410 = CARTESIAN_POINT ( 'NONE',  ( 6.575338752097509065, -50.90849809615561838, 3.999999999999999556 ) ) ;
#83411 = CARTESIAN_POINT ( 'NONE',  ( -14.47650479471820439, 14.63606881343827126, -3.928206833722228453 ) ) ;
#83412 = CARTESIAN_POINT ( 'NONE',  ( 13.79529636645030344, 48.26208216824728936, 14.16423886937410614 ) ) ;
#83413 = CARTESIAN_POINT ( 'NONE',  ( 14.92337183194729633, 2.675597817667451750, 8.527530157486181039 ) ) ;
#83414 =( LENGTH_UNIT ( ) NAMED_UNIT ( * ) SI_UNIT ( .MILLI., .METRE. ) );
#83415 = CARTESIAN_POINT ( 'NONE',  ( 14.92337183194729633, 57.67559781766745886, 8.527530157486181039 ) ) ;
#83416 = VECTOR ( 'NONE', #52581, 1000.000000000000000 ) ;
#83417 = CARTESIAN_POINT ( 'NONE',  ( -14.93875075227017213, 14.76984974223857172, 0.2365588874158334465 ) ) ;
#83418 = CARTESIAN_POINT ( 'NONE',  ( 0.1532563361054082862, 36.21726448433410894, 2.638427012816831674 ) ) ;
#83419 = EDGE_LOOP ( 'NONE', ( #41335, #27084, #52043, #59847 ) ) ;
#83420 = AXIS2_PLACEMENT_3D ( 'NONE', #41117, #10116, #71113 ) ;
#83421 = CARTESIAN_POINT ( 'NONE',  ( 1.472469842513823179, 35.59226448433412315, -4.923371831947296329 ) ) ;
#83422 = CARTESIAN_POINT ( 'NONE',  ( 9.382169495545415572, -17.75136533006957862, -9.382169495545422677 ) ) ;
#83423 = AXIS2_PLACEMENT_3D ( 'NONE', #88890, #66374, #96908 ) ;
#83424 = CARTESIAN_POINT ( 'NONE',  ( 17.96484262340118221, 29.93868534415484106, 7.964842623401181321 ) ) ;
#83425 = CARTESIAN_POINT ( 'NONE',  ( 17.20831665107776587, 37.88393115100078745, 7.208316651077764980 ) ) ;
#83427 = CARTESIAN_POINT ( 'NONE',  ( 20.88017736071110519, 60.56368534415484106, 2.639326808657452039E-16 ) ) ;
#83426 = CARTESIAN_POINT ( 'NONE',  ( 19.72487221294571569, 25.71833443783938478, -6.499999999999989342 ) ) ;
#83429 = CARTESIAN_POINT ( 'NONE',  ( -1.099225684535947600, 64.54030133659709634, 6.408140936763237150 ) ) ;
#83428 = CARTESIAN_POINT ( 'NONE',  ( -0.8801773607111008646, 28.27201867748817321, 2.915334737309923430 ) ) ;
#83430 = CARTESIAN_POINT ( 'NONE',  ( 13.79529636645031943, 40.34541550158063217, -14.16423886937409904 ) ) ;
#83431 = EDGE_CURVE ( 'NONE', #62035, #89063, #39443, .T. ) ;
#83432 = CARTESIAN_POINT ( 'NONE',  ( -13.11254139118232231, 91.00000000000000000, 8.000000000000000000 ) ) ;
#83433 = ADVANCED_FACE ( 'NONE', ( #43210 ), #19729, .F. ) ;
#83434 = ORIENTED_EDGE ( 'NONE', *, *, #75522, .F. ) ;
#83435 = CARTESIAN_POINT ( 'NONE',  ( 0.6178305044545838731, 9.748634669930416052, 9.382169495545420901 ) ) ;
#83436 = CARTESIAN_POINT ( 'NONE',  ( -0.8801773607110991993, 12.85535201082150358, -2.915334737309923874 ) ) ;
#83437 = CARTESIAN_POINT ( 'NONE',  ( 10.00000000000000000, 46.81368534415484106, -10.88017736071110342 ) ) ;
#83438 = LINE ( 'NONE', #51457, #31372 ) ;
#83439 = ORIENTED_EDGE ( 'NONE', *, *, #25771, .F. ) ;
#83440 = CARTESIAN_POINT ( 'NONE',  ( 20.88017736071110875, 60.77201867748817676, -2.915334737309920765 ) ) ;
#83441 = CARTESIAN_POINT ( 'NONE',  ( 17.20831665107776587, 37.88393115100078745, 7.208316651077764980 ) ) ;
#83442 = CARTESIAN_POINT ( 'NONE',  ( 1.472469842513823179, 20.59226448433411960, -4.923371831947296329 ) ) ;
#83443 = CARTESIAN_POINT ( 'NONE',  ( 14.92337183194729633, 17.67559781766745175, 8.527530157486181039 ) ) ;
#83444 = CARTESIAN_POINT ( 'NONE',  ( 14.43100913237647731, 15.00000000000000000, -1.412789942450803027 ) ) ;
#83445 = CYLINDRICAL_SURFACE ( 'NONE', #21287, 0.5000000000000004441 ) ;
#83447 = LINE ( 'NONE', #82954, #96225 ) ;
#83446 = CARTESIAN_POINT ( 'NONE',  ( 1.472469842513823179, 10.59226448433411782, -4.923371831947296329 ) ) ;
#83448 = CARTESIAN_POINT ( 'NONE',  ( 4.630000000000002558, 0.09071050906739661079, -4.000000000000000000 ) ) ;
#83450 = VERTEX_POINT ( 'NONE', #42733 ) ;
#83449 = CARTESIAN_POINT ( 'NONE',  ( 5.076628168052703671, 26.84226448433411960, 8.527530157486179263 ) ) ;
#83451 =( BOUNDED_SURFACE ( )  B_SPLINE_SURFACE ( 1, 2, ( 
 ( #29240, #59738, #37754, #45737, #30712, #7751, #68251, #68736, #90233, #38730, #91727, #90731, #38245, #29728, #52245, #21766, #23249, #82739, #44737, #37265, #84240, #46231, #69230, #22257, #76717, #14762, #75733, #62688, #56672, #48179, #17708, #77695, #87161, #32185, #10689, #71682, #24715, #2224, #55700, #25703, #9207, #25219, #54692, #39720, #86196, #56193, #24225, #86687, #17219, #2721, #3192, #63667, #32684, #26181, #48672, #18686, #18191, #49171, #33174, #79173, #31700, #94172, #47191, #63177, #41202, #78691, #55187, #33658, #79673, #64153, #1731, #10202, #9703, #94672, #40695, #11170, #71197, #69718, #62191, #47698, #1244, #93686, #85214, #92701, #70212, #93188, #85703, #78190, #16718, #40199, #70707, #66640, #51137, #12152, #12641, #65637, #42659, #51641, #65141, #72159, #64642, #97164, #80153, #73631, #27147, #11665, #43633, #95662, #49646, #81627, #20145, #96659, #28632, #59120, #89629, #95152, #26662, #21140, #28139, #58639, #73134, #3687, #88638, #50651, #82122, #43138, #89138, #35136, #42178, #41689, #34645, #80658, #34148, #66130, #57156, #19167, #81139, #20648, #87654, #72642, #5156, #4175, #57649, #88145, #35643, #19657, #13134, #74118, #36130, #50148, #4675, #96160, #5654, #27643, #58127, #15630, #83619, #53110, #14646, #38130, #15135, #45611, #91610, #14139, #61586, #92097, #84114, #36642, #52128, #23126, #22134, #31091, #38611, #90610, #83116, #67126, #29605, #75615, #29116, #60609, #53599, #91103, #68127, #52616, #54089, #98655, #76109, #30595, #75119, #45108, #7125, #37630, #7640, #68618, #30101, #147, #61100, #46113, #76599, #44624, #23628, #13632, #8115, #97654, #82625, #69108, #22631, #44115, #642, #74625, #6139, #59619, #60109, #90117, #21644, #6626, #37140, #67634, #98144, #24603, #26069, #70585, #25100, #2606, #47077, #93074, #17100, #9583, #33059, #63067, #70094, #63555, #41078, #94064, #16600, #40084, #55069, #17592, #2111, #78574, #32570, #64038, #77089, #32065, #71080, #47585, #39109, #46591, #54577, #77575, #9090, #62075, #18076, #86081, #92583, #10570, #25586, #85587, #55585, #93567, #78079, #94552, #39606, #16105, #8599, #71576, #24106, #48059, #1617, #85091, #86572, #62569, #10083, #56077, #40583, #48554, #3086, #33543, #84604, #69599, #1120, #31582, #79055, #12532, #27034, #18565, #4555, #35020, #13018, #58018, #43032, #50037, #64529, #43517, #49533, #95546, #49057, #81026, #79561, #34033, #96043, #35524, #87054, #26545, #27528, #11060, #41579, #95036, #65521, #72047, #50531, #5041, #51020, #87544, #34523, #74012, #58517, #19055, #88527, #89025, #57040, #96543, #20029, #73513, #5540 ),
 ( #11546, #88029, #42538, #66019, #80039, #12038, #3577, #42065, #73022, #28019, #72526, #20536, #4060, #81512, #36017, #66520, #19542, #97048, #56560, #65017, #57533, #80541, #61849, #84861, #89520, #92356, #6030, #23388, #6512, #90491, #36529, #82511, #28523, #31839, #29489, #16367, #53873, #14027, #8369, #77343, #90006, #67019, #46848, #69864, #84383, #21029, #31349, #75007, #85347, #77835, #38877, #97539, #16859, #44507, #59998, #29000, #15883, #46367, #23883, #76856, #47334, #54347, #59511, #8854, #39369, #13524, #69368, #1385, #62336, #888, #9347, #92844, #24371, #39851, #54834, #70356, #59015, #51521, #82013, #21526, #44006, #74508, #52020, #37018, #67517, #98034, #26309, #2365, #18333, #57298, #1875, #41830, #87791, #42307, #10340, #56333, #3326, #48813, #40838, #71819, #32331, #72296, #33791, #93827, #71339, #32821, #55339, #19306, #2857, #62836, #93336, #40351, #86827, #33311, #94807, #49306, #95299, #63318, #78830, #49794, #3827, #25356, #64296, #34282, #56809, #41350, #63805, #87306, #18825, #79807, #11310, #55841, #80301, #11800, #64782, #24856, #70852, #26802, #94312, #85846, #17359, #25837, #79320, #47829, #17839, #10830, #78329, #9851, #86335, #48322, #28282, #12782, #14286, #58776, #13279, #89767, #35282, #81284, #5305, #96805, #21283, #51281, #58269, #51778, #29265, #82262, #4809, #89281, #43281, #5789, #20792, #66777, #81767, #52268, #65278, #20295, #59265, #35782, #27286, #34789, #42801, #65778, #96307, #50281, #6278, #74260, #80797, #97804, #13778, #73776, #43770, #36280, #66271, #82764, #27783, #4316, #95808, #59761, #12293, #97298, #88785, #73285, #74770, #50793, #28770, #44264, #36784, #67275, #90255, #21788, #72780, #57786, #88292, #19792, #31227, #775, #15281, #6775, #91750, #23270, #1267, #46252, #61723, #38267, #52756, #31721, #37778, #83757, #37285, #69255, #67775, #22282, #84264, #23765, #75262, #14788, #15765, #98295, #29751, #83263, #53746, #60260, #54228, #53252, #62218, #69741, #22772, #45762, #90754, #60746, #7773, #45258, #76737, #84743, #8253, #291, #76256, #85237, #30737, #38754, #92239, #7276, #68760, #61243, #16247, #46730, #77228, #30242, #8733, #92724, #39251, #75755, #24249, #54716, #44759, #68275, #98795, #91247, #95173, #9231, #63201, #3215, #48201, #70235, #77718, #85726, #47717, #40223, #93210, #49190, #18215, #24733, #41710, #26200, #86216, #86710, #40714, #17728, #26680, #70733, #47217, #39740, #72180, #55211, #48694, #2247, #17239, #18706, #32705, #78212, #56692, #94192, #71701, #3710, #34170, #64660, #1754, #32209, #57175, #33677, #64174, #78714, #62710, #63689, #25722 ) ),
 .UNSPECIFIED., .F., .F., .F. ) 
 B_SPLINE_SURFACE_WITH_KNOTS ( ( 2, 2 ),
 ( 3, 2, 2, 2, 2, 2, 2, 2, 2, 2, 2, 2, 2, 2, 2, 2, 2, 2, 2, 2, 2, 2, 2, 2, 2, 2, 2, 2, 2, 2, 2, 2, 2, 2, 2, 2, 2, 2, 2, 2, 2, 2, 2, 2, 2, 2, 2, 2, 2, 2, 2, 2, 2, 2, 2, 2, 2, 2, 2, 2, 2, 2, 2, 2, 2, 2, 2, 2, 2, 2, 2, 2, 2, 2, 2, 2, 2, 2, 2, 2, 2, 2, 2, 2, 2, 2, 2, 2, 2, 2, 2, 2, 2, 2, 2, 2, 2, 2, 2, 2, 2, 2, 2, 2, 2, 2, 2, 2, 2, 2, 2, 2, 2, 2, 2, 2, 2, 2, 2, 2, 2, 2, 2, 2, 2, 2, 2, 2, 2, 2, 2, 2, 2, 2, 2, 2, 2, 2, 2, 2, 2, 2, 2, 2, 2, 2, 2, 2, 2, 2, 2, 2, 2, 2, 2, 2, 2, 2, 2, 2, 2, 2, 3 ),
 ( 0.000000000000000000, 1.000000000000000000 ),
 ( 0.000000000000000000, 0.005952380952380952051, 0.01190476190476190410, 0.01785714285714285615, 0.02380952380952380820, 0.02976190476190476025, 0.03571428571428571230, 0.04166666666666666435, 0.04761904761904761640, 0.05357142857142856845, 0.05952380952380952051, 0.06547619047619047949, 0.07142857142857142461, 0.07738095238095238360, 0.08333333333333332871, 0.08928571428571428770, 0.09523809523809523281, 0.1011904761904761918, 0.1071428571428571369, 0.1130952380952380959, 0.1190476190476190410, 0.1250000000000000000, 0.1309523809523809590, 0.1369047619047619180, 0.1428571428571428492, 0.1488095238095238082, 0.1547619047619047672, 0.1607142857142857262, 0.1666666666666666574, 0.1726190476190476164, 0.1785714285714285754, 0.1845238095238095344, 0.1904761904761904656, 0.1964285714285714246, 0.2023809523809523836, 0.2083333333333333426, 0.2142857142857142738, 0.2202380952380952328, 0.2261904761904761918, 0.2321428571428571508, 0.2380952380952380820, 0.2440476190476190410, 0.2500000000000000000, 0.2559523809523809312, 0.2619047619047619180, 0.2678571428571428492, 0.2738095238095238360, 0.2797619047619047672, 0.2857142857142856984, 0.2916666666666666852, 0.2976190476190476164, 0.3035714285714285476, 0.3095238095238095344, 0.3154761904761904656, 0.3214285714285714524, 0.3273809523809523836, 0.3333333333333333148, 0.3392857142857143016, 0.3452380952380952328, 0.3511904761904761640, 0.3571428571428571508, 0.3630952380952380820, 0.3690476190476190688, 0.3750000000000000000, 0.3809523809523809312, 0.3869047619047619180, 0.3928571428571428492, 0.3988095238095238360, 0.4047619047619047672, 0.4107142857142856984, 0.4166666666666666852, 0.4226190476190476164, 0.4285714285714285476, 0.4345238095238095344, 0.4404761904761904656, 0.4464285714285714524, 0.4523809523809523836, 0.4583333333333333148, 0.4642857142857143016, 0.4702380952380952328, 0.4761904761904761640, 0.4821428571428571508, 0.4880952380952380820, 0.4940476190476190688, 0.5000000000000000000, 0.5059523809523809312, 0.5119047619047618625, 0.5178571428571429047, 0.5238095238095238360, 0.5297619047619047672, 0.5357142857142856984, 0.5416666666666666297, 0.5476190476190476719, 0.5535714285714286031, 0.5595238095238095344, 0.5654761904761904656, 0.5714285714285713969, 0.5773809523809523281, 0.5833333333333333703, 0.5892857142857143016, 0.5952380952380952328, 0.6011904761904761640, 0.6071428571428570953, 0.6130952380952381375, 0.6190476190476190688, 0.6250000000000000000, 0.6309523809523809312, 0.6369047619047618625, 0.6428571428571429047, 0.6488095238095238360, 0.6547619047619047672, 0.6607142857142856984, 0.6666666666666666297, 0.6726190476190476719, 0.6785714285714286031, 0.6845238095238095344, 0.6904761904761904656, 0.6964285714285713969, 0.7023809523809523281, 0.7083333333333333703, 0.7142857142857143016, 0.7202380952380952328, 0.7261904761904761640, 0.7321428571428570953, 0.7380952380952381375, 0.7440476190476190688, 0.7500000000000000000, 0.7559523809523809312, 0.7619047619047618625, 0.7678571428571429047, 0.7738095238095238360, 0.7797619047619047672, 0.7857142857142856984, 0.7916666666666666297, 0.7976190476190476719, 0.8035714285714286031, 0.8095238095238095344, 0.8154761904761904656, 0.8214285714285713969, 0.8273809523809523281, 0.8333333333333333703, 0.8392857142857143016, 0.8452380952380952328, 0.8511904761904761640, 0.8571428571428570953, 0.8630952380952381375, 0.8690476190476190688, 0.8750000000000000000, 0.8809523809523809312, 0.8869047619047618625, 0.8928571428571429047, 0.8988095238095238360, 0.9047619047619047672, 0.9107142857142856984, 0.9166666666666666297, 0.9226190476190476719, 0.9285714285714286031, 0.9345238095238095344, 0.9404761904761904656, 0.9464285714285713969, 0.9523809523809523281, 0.9583333333333333703, 0.9642857142857143016 ),
 .UNSPECIFIED. ) 
 GEOMETRIC_REPRESENTATION_ITEM ( )  RATIONAL_B_SPLINE_SURFACE ( (
 ( 1.000000000000000000, 0.9659258262890683122, 1.000000000000000000, 0.9659258262890683122, 1.000000000000000000, 0.9659258262890683122, 1.000000000000000000, 0.9659258262890683122, 1.000000000000000000, 0.9659258262890683122, 1.000000000000000000, 0.9659258262890683122, 1.000000000000000000, 0.9659258262890683122, 1.000000000000000000, 0.9659258262890683122, 1.000000000000000000, 0.9659258262890683122, 1.000000000000000000, 0.9659258262890683122, 1.000000000000000000, 0.9659258262890683122, 1.000000000000000000, 0.9659258262890683122, 1.000000000000000000, 0.9659258262890683122, 1.000000000000000000, 0.9659258262890683122, 1.000000000000000000, 0.9659258262890683122, 1.000000000000000000, 0.9659258262890683122, 1.000000000000000000, 0.9659258262890683122, 1.000000000000000000, 0.9659258262890683122, 1.000000000000000000, 0.9659258262890683122, 1.000000000000000000, 0.9659258262890683122, 1.000000000000000000, 0.9659258262890683122, 1.000000000000000000, 0.9659258262890683122, 1.000000000000000000, 0.9659258262890683122, 1.000000000000000000, 0.9659258262890683122, 1.000000000000000000, 0.9659258262890683122, 1.000000000000000000, 0.9659258262890683122, 1.000000000000000000, 0.9659258262890683122, 1.000000000000000000, 0.9659258262890683122, 1.000000000000000000, 0.9659258262890683122, 1.000000000000000000, 0.9659258262890683122, 1.000000000000000000, 0.9659258262890683122, 1.000000000000000000, 0.9659258262890683122, 1.000000000000000000, 0.9659258262890683122, 1.000000000000000000, 0.9659258262890683122, 1.000000000000000000, 0.9659258262890683122, 1.000000000000000000, 0.9659258262890683122, 1.000000000000000000, 0.9659258262890683122, 1.000000000000000000, 0.9659258262890683122, 1.000000000000000000, 0.9659258262890683122, 1.000000000000000000, 0.9659258262890683122, 1.000000000000000000, 0.9659258262890683122, 1.000000000000000000, 0.9659258262890683122, 1.000000000000000000, 0.9659258262890683122, 1.000000000000000000, 0.9659258262890683122, 1.000000000000000000, 0.9659258262890683122, 1.000000000000000000, 0.9659258262890683122, 1.000000000000000000, 0.9659258262890683122, 1.000000000000000000, 0.9659258262890683122, 1.000000000000000000, 0.9659258262890683122, 1.000000000000000000, 0.9659258262890683122, 1.000000000000000000, 0.9659258262890683122, 1.000000000000000000, 0.9659258262890683122, 1.000000000000000000, 0.9659258262890683122, 1.000000000000000000, 0.9659258262890683122, 1.000000000000000000, 0.9659258262890683122, 1.000000000000000000, 0.9659258262890683122, 1.000000000000000000, 0.9659258262890683122, 1.000000000000000000, 0.9659258262890683122, 1.000000000000000000, 0.9659258262890683122, 1.000000000000000000, 0.9659258262890683122, 1.000000000000000000, 0.9659258262890683122, 1.000000000000000000, 0.9659258262890683122, 1.000000000000000000, 0.9659258262890683122, 1.000000000000000000, 0.9659258262890683122, 1.000000000000000000, 0.9659258262890683122, 1.000000000000000000, 0.9659258262890683122, 1.000000000000000000, 0.9659258262890683122, 1.000000000000000000, 0.9659258262890683122, 1.000000000000000000, 0.9659258262890683122, 1.000000000000000000, 0.9659258262890683122, 1.000000000000000000, 0.9659258262890683122, 1.000000000000000000, 0.9659258262890683122, 1.000000000000000000, 0.9659258262890683122, 1.000000000000000000, 0.9659258262890683122, 1.000000000000000000, 0.9659258262890683122, 1.000000000000000000, 0.9659258262890683122, 1.000000000000000000, 0.9659258262890683122, 1.000000000000000000, 0.9659258262890683122, 1.000000000000000000, 0.9659258262890683122, 1.000000000000000000, 0.9659258262890683122, 1.000000000000000000, 0.9659258262890683122, 1.000000000000000000, 0.9659258262890683122, 1.000000000000000000, 0.9659258262890683122, 1.000000000000000000, 0.9659258262890683122, 1.000000000000000000, 0.9659258262890683122, 1.000000000000000000, 0.9659258262890683122, 1.000000000000000000, 0.9659258262890683122, 1.000000000000000000, 0.9659258262890683122, 1.000000000000000000, 0.9659258262890683122, 1.000000000000000000, 0.9659258262890683122, 1.000000000000000000, 0.9659258262890683122, 1.000000000000000000, 0.9659258262890683122, 1.000000000000000000, 0.9659258262890683122, 1.000000000000000000, 0.9659258262890683122, 1.000000000000000000, 0.9659258262890683122, 1.000000000000000000, 0.9659258262890683122, 1.000000000000000000, 0.9659258262890683122, 1.000000000000000000, 0.9659258262890683122, 1.000000000000000000, 0.9659258262890683122, 1.000000000000000000, 0.9659258262890683122, 1.000000000000000000, 0.9659258262890683122, 1.000000000000000000, 0.9659258262890683122, 1.000000000000000000, 0.9659258262890683122, 1.000000000000000000, 0.9659258262890683122, 1.000000000000000000, 0.9659258262890683122, 1.000000000000000000, 0.9659258262890683122, 1.000000000000000000, 0.9659258262890683122, 1.000000000000000000, 0.9659258262890683122, 1.000000000000000000, 0.9659258262890683122, 1.000000000000000000, 0.9659258262890683122, 1.000000000000000000, 0.9659258262890683122, 1.000000000000000000, 0.9659258262890683122, 1.000000000000000000, 0.9659258262890683122, 1.000000000000000000, 0.9659258262890683122, 1.000000000000000000, 0.9659258262890683122, 1.000000000000000000, 0.9659258262890683122, 1.000000000000000000, 0.9659258262890683122, 1.000000000000000000, 0.9659258262890683122, 1.000000000000000000, 0.9659258262890683122, 1.000000000000000000, 0.9659258262890683122, 1.000000000000000000, 0.9659258262890683122, 1.000000000000000000, 0.9659258262890683122, 1.000000000000000000, 0.9659258262890683122, 1.000000000000000000, 0.9659258262890683122, 1.000000000000000000, 0.9659258262890683122, 1.000000000000000000, 0.9659258262890683122, 1.000000000000000000, 0.9659258262890683122, 1.000000000000000000, 0.9659258262890683122, 1.000000000000000000, 0.9659258262890683122, 1.000000000000000000, 0.9659258262890683122, 1.000000000000000000, 0.9659258262890683122, 1.000000000000000000, 0.9659258262890683122, 1.000000000000000000, 0.9659258262890683122, 1.000000000000000000, 0.9659258262890683122, 1.000000000000000000, 0.9659258262890683122, 1.000000000000000000, 0.9659258262890683122, 1.000000000000000000, 0.9659258262890683122, 1.000000000000000000, 0.9659258262890683122, 1.000000000000000000, 0.9659258262890683122, 1.000000000000000000, 0.9659258262890683122, 1.000000000000000000, 0.9659258262890683122, 1.000000000000000000, 0.9659258262890683122, 1.000000000000000000, 0.9659258262890683122, 1.000000000000000000, 0.9659258262890683122, 1.000000000000000000, 0.9659258262890683122, 1.000000000000000000, 0.9659258262890683122, 1.000000000000000000, 0.9659258262890683122, 1.000000000000000000, 0.9659258262890683122, 1.000000000000000000, 0.9659258262890683122, 1.000000000000000000, 0.9659258262890683122, 1.000000000000000000, 0.9659258262890683122, 1.000000000000000000, 0.9659258262890683122, 1.000000000000000000, 0.9659258262890683122, 1.000000000000000000, 0.9659258262890683122, 1.000000000000000000, 0.9659258262890683122, 1.000000000000000000, 0.9659258262890683122, 1.000000000000000000, 0.9659258262890683122, 1.000000000000000000, 0.9659258262890683122, 1.000000000000000000, 0.9659258262890683122, 1.000000000000000000, 0.9659258262890683122, 1.000000000000000000, 0.9659258262890683122, 1.000000000000000000, 0.9659258262890683122, 1.000000000000000000),
 ( 1.000000000000000000, 0.9659258262890683122, 1.000000000000000000, 0.9659258262890683122, 1.000000000000000000, 0.9659258262890683122, 1.000000000000000000, 0.9659258262890683122, 1.000000000000000000, 0.9659258262890683122, 1.000000000000000000, 0.9659258262890683122, 1.000000000000000000, 0.9659258262890683122, 1.000000000000000000, 0.9659258262890683122, 1.000000000000000000, 0.9659258262890683122, 1.000000000000000000, 0.9659258262890683122, 1.000000000000000000, 0.9659258262890683122, 1.000000000000000000, 0.9659258262890683122, 1.000000000000000000, 0.9659258262890683122, 1.000000000000000000, 0.9659258262890683122, 1.000000000000000000, 0.9659258262890683122, 1.000000000000000000, 0.9659258262890683122, 1.000000000000000000, 0.9659258262890683122, 1.000000000000000000, 0.9659258262890683122, 1.000000000000000000, 0.9659258262890683122, 1.000000000000000000, 0.9659258262890683122, 1.000000000000000000, 0.9659258262890683122, 1.000000000000000000, 0.9659258262890683122, 1.000000000000000000, 0.9659258262890683122, 1.000000000000000000, 0.9659258262890683122, 1.000000000000000000, 0.9659258262890683122, 1.000000000000000000, 0.9659258262890683122, 1.000000000000000000, 0.9659258262890683122, 1.000000000000000000, 0.9659258262890683122, 1.000000000000000000, 0.9659258262890683122, 1.000000000000000000, 0.9659258262890683122, 1.000000000000000000, 0.9659258262890683122, 1.000000000000000000, 0.9659258262890683122, 1.000000000000000000, 0.9659258262890683122, 1.000000000000000000, 0.9659258262890683122, 1.000000000000000000, 0.9659258262890683122, 1.000000000000000000, 0.9659258262890683122, 1.000000000000000000, 0.9659258262890683122, 1.000000000000000000, 0.9659258262890683122, 1.000000000000000000, 0.9659258262890683122, 1.000000000000000000, 0.9659258262890683122, 1.000000000000000000, 0.9659258262890683122, 1.000000000000000000, 0.9659258262890683122, 1.000000000000000000, 0.9659258262890683122, 1.000000000000000000, 0.9659258262890683122, 1.000000000000000000, 0.9659258262890683122, 1.000000000000000000, 0.9659258262890683122, 1.000000000000000000, 0.9659258262890683122, 1.000000000000000000, 0.9659258262890683122, 1.000000000000000000, 0.9659258262890683122, 1.000000000000000000, 0.9659258262890683122, 1.000000000000000000, 0.9659258262890683122, 1.000000000000000000, 0.9659258262890683122, 1.000000000000000000, 0.9659258262890683122, 1.000000000000000000, 0.9659258262890683122, 1.000000000000000000, 0.9659258262890683122, 1.000000000000000000, 0.9659258262890683122, 1.000000000000000000, 0.9659258262890683122, 1.000000000000000000, 0.9659258262890683122, 1.000000000000000000, 0.9659258262890683122, 1.000000000000000000, 0.9659258262890683122, 1.000000000000000000, 0.9659258262890683122, 1.000000000000000000, 0.9659258262890683122, 1.000000000000000000, 0.9659258262890683122, 1.000000000000000000, 0.9659258262890683122, 1.000000000000000000, 0.9659258262890683122, 1.000000000000000000, 0.9659258262890683122, 1.000000000000000000, 0.9659258262890683122, 1.000000000000000000, 0.9659258262890683122, 1.000000000000000000, 0.9659258262890683122, 1.000000000000000000, 0.9659258262890683122, 1.000000000000000000, 0.9659258262890683122, 1.000000000000000000, 0.9659258262890683122, 1.000000000000000000, 0.9659258262890683122, 1.000000000000000000, 0.9659258262890683122, 1.000000000000000000, 0.9659258262890683122, 1.000000000000000000, 0.9659258262890683122, 1.000000000000000000, 0.9659258262890683122, 1.000000000000000000, 0.9659258262890683122, 1.000000000000000000, 0.9659258262890683122, 1.000000000000000000, 0.9659258262890683122, 1.000000000000000000, 0.9659258262890683122, 1.000000000000000000, 0.9659258262890683122, 1.000000000000000000, 0.9659258262890683122, 1.000000000000000000, 0.9659258262890683122, 1.000000000000000000, 0.9659258262890683122, 1.000000000000000000, 0.9659258262890683122, 1.000000000000000000, 0.9659258262890683122, 1.000000000000000000, 0.9659258262890683122, 1.000000000000000000, 0.9659258262890683122, 1.000000000000000000, 0.9659258262890683122, 1.000000000000000000, 0.9659258262890683122, 1.000000000000000000, 0.9659258262890683122, 1.000000000000000000, 0.9659258262890683122, 1.000000000000000000, 0.9659258262890683122, 1.000000000000000000, 0.9659258262890683122, 1.000000000000000000, 0.9659258262890683122, 1.000000000000000000, 0.9659258262890683122, 1.000000000000000000, 0.9659258262890683122, 1.000000000000000000, 0.9659258262890683122, 1.000000000000000000, 0.9659258262890683122, 1.000000000000000000, 0.9659258262890683122, 1.000000000000000000, 0.9659258262890683122, 1.000000000000000000, 0.9659258262890683122, 1.000000000000000000, 0.9659258262890683122, 1.000000000000000000, 0.9659258262890683122, 1.000000000000000000, 0.9659258262890683122, 1.000000000000000000, 0.9659258262890683122, 1.000000000000000000, 0.9659258262890683122, 1.000000000000000000, 0.9659258262890683122, 1.000000000000000000, 0.9659258262890683122, 1.000000000000000000, 0.9659258262890683122, 1.000000000000000000, 0.9659258262890683122, 1.000000000000000000, 0.9659258262890683122, 1.000000000000000000, 0.9659258262890683122, 1.000000000000000000, 0.9659258262890683122, 1.000000000000000000, 0.9659258262890683122, 1.000000000000000000, 0.9659258262890683122, 1.000000000000000000, 0.9659258262890683122, 1.000000000000000000, 0.9659258262890683122, 1.000000000000000000, 0.9659258262890683122, 1.000000000000000000, 0.9659258262890683122, 1.000000000000000000, 0.9659258262890683122, 1.000000000000000000, 0.9659258262890683122, 1.000000000000000000, 0.9659258262890683122, 1.000000000000000000, 0.9659258262890683122, 1.000000000000000000, 0.9659258262890683122, 1.000000000000000000, 0.9659258262890683122, 1.000000000000000000, 0.9659258262890683122, 1.000000000000000000, 0.9659258262890683122, 1.000000000000000000, 0.9659258262890683122, 1.000000000000000000, 0.9659258262890683122, 1.000000000000000000, 0.9659258262890683122, 1.000000000000000000, 0.9659258262890683122, 1.000000000000000000, 0.9659258262890683122, 1.000000000000000000, 0.9659258262890683122, 1.000000000000000000, 0.9659258262890683122, 1.000000000000000000, 0.9659258262890683122, 1.000000000000000000, 0.9659258262890683122, 1.000000000000000000, 0.9659258262890683122, 1.000000000000000000, 0.9659258262890683122, 1.000000000000000000, 0.9659258262890683122, 1.000000000000000000, 0.9659258262890683122, 1.000000000000000000, 0.9659258262890683122, 1.000000000000000000, 0.9659258262890683122, 1.000000000000000000, 0.9659258262890683122, 1.000000000000000000, 0.9659258262890683122, 1.000000000000000000, 0.9659258262890683122, 1.000000000000000000, 0.9659258262890683122, 1.000000000000000000, 0.9659258262890683122, 1.000000000000000000, 0.9659258262890683122, 1.000000000000000000, 0.9659258262890683122, 1.000000000000000000, 0.9659258262890683122, 1.000000000000000000, 0.9659258262890683122, 1.000000000000000000, 0.9659258262890683122, 1.000000000000000000, 0.9659258262890683122, 1.000000000000000000, 0.9659258262890683122, 1.000000000000000000, 0.9659258262890683122, 1.000000000000000000, 0.9659258262890683122, 1.000000000000000000, 0.9659258262890683122, 1.000000000000000000, 0.9659258262890683122, 1.000000000000000000, 0.9659258262890683122, 1.000000000000000000, 0.9659258262890683122, 1.000000000000000000) ) ) 
 REPRESENTATION_ITEM ( '' )  SURFACE ( )  );
#83452 = AXIS2_PLACEMENT_3D ( 'NONE', #66323, #29311, #28818 ) ;
#83453 = CARTESIAN_POINT ( 'NONE',  ( 22.81628187352648496, 16.83196800326374998, -3.434112377981050290 ) ) ;
#83454 = CARTESIAN_POINT ( 'NONE',  ( 7.084665262690076126, 57.02201867748817676, -10.88017736071110164 ) ) ;
#83455 = CARTESIAN_POINT ( 'NONE',  ( 22.26659068614895176, 29.72041550158063572, -7.082119434687042414 ) ) ;
#83456 = UNCERTAINTY_MEASURE_WITH_UNIT (LENGTH_MEASURE( 1.000000000000000082E-05 ), #22558, 'distance_accuracy_value', 'NONE');
#83457 = CARTESIAN_POINT ( 'NONE',  ( -10.91371419741111204, 89.69638457836138912, 6.151049038645131084 ) ) ;
#83458 = EDGE_CURVE ( 'NONE', #7455, #37030, #27717, .T. ) ;
#83459 = CARTESIAN_POINT ( 'NONE',  ( 22.26659068614895176, 34.72041550158063927, -7.082119434687042414 ) ) ;
#83460 = CARTESIAN_POINT ( 'NONE',  ( 13.79529636645031943, 40.34541550158063217, -14.16423886937409904 ) ) ;
#83461 = CARTESIAN_POINT ( 'NONE',  ( -4.164238869374098151, 11.59541550158063217, -3.795296366450310543 ) ) ;
#83463 = DIRECTION ( 'NONE',  ( 1.000000000000000000, -0.000000000000000000, -0.000000000000000000 ) ) ;
#83462 = CARTESIAN_POINT ( 'NONE',  ( -2.266590686148945544, 32.22041550158063927, 7.082119434687048631 ) ) ;
#83464 = CARTESIAN_POINT ( 'NONE',  ( 4.559911319644449179, 52.23035201082151247, -9.422509992056141925 ) ) ;
#83465 = CARTESIAN_POINT ( 'NONE',  ( 6.004190426492125532, -34.81345361117713111, -2.750000000000000000 ) ) ;
#83466 = CARTESIAN_POINT ( 'NONE',  ( 10.00000000000000178, 32.25893115100078745, 9.846743663894594434 ) ) ;
#83468 = CARTESIAN_POINT ( 'NONE',  ( 19.84674366389459266, 48.71726448433413026, -2.638427012816827677 ) ) ;
#83467 = CARTESIAN_POINT ( 'NONE',  ( 0.5774900079438607392, 63.48035201082149825, 5.440088680355550821 ) ) ;
#83469 = CARTESIAN_POINT ( 'NONE',  ( -0.8801773607111009756, 28.06368534415484106, 1.068504757029289695E-15 ) ) ;
#83470 = CARTESIAN_POINT ( 'NONE',  ( -2.816281873526471635, 53.91530133659709634, -3.434112377981056508 ) ) ;
#83471 = CARTESIAN_POINT ( 'NONE',  ( 14.92337183194729988, 59.34226448433412315, -8.527530157486177487 ) ) ;
#83472 = CARTESIAN_POINT ( 'NONE',  ( -9.876730923139158236, 14.63595249122788999, -11.28938378619077376 ) ) ;
#83473 = CARTESIAN_POINT ( 'NONE',  ( 0.1532563361054083140, 26.00893115100078745, 1.131784320476157264E-15 ) ) ;
#83474 = CARTESIAN_POINT ( 'NONE',  ( 19.38216949554541557, 62.24863466993041072, -9.382169495545420901 ) ) ;
#83475 = CARTESIAN_POINT ( 'NONE',  ( 10.36894250292378850, -20.07125116508603213, -10.36894250292379027 ) ) ;
#83476 = CIRCLE ( 'NONE', #22815, 14.49999999999999822 ) ;
#83477 = CARTESIAN_POINT ( 'NONE',  ( 19.42250999205614548, 45.98035201082150536, -5.440088680355545492 ) ) ;
#83478 = CARTESIAN_POINT ( 'NONE',  ( 5.076628168052704559, 55.17559781766745175, -8.527530157486179263 ) ) ;
#83479 = CARTESIAN_POINT ( 'NONE',  ( 22.26659068614895176, 34.72041550158063927, -7.082119434687042414 ) ) ;
#83480 = ORIENTED_EDGE ( 'NONE', *, *, #55648, .T. ) ;
#83481 = DIRECTION ( 'NONE',  ( -0.000000000000000000, -0.000000000000000000, -1.000000000000000000 ) ) ;
#83482 = CARTESIAN_POINT ( 'NONE',  ( 10.00000000000000000, 66.81368534415484817, -10.88017736071110342 ) ) ;
#83483 = DIRECTION ( 'NONE',  ( -0.000000000000000000, -1.000000000000000000, -0.000000000000000000 ) ) ;
#83485 = AXIS2_PLACEMENT_3D ( 'NONE', #80733, #57233, #56747 ) ;
#83484 = CARTESIAN_POINT ( 'NONE',  ( 17.08211943468705130, 58.47041550158063927, 12.26659068614894998 ) ) ;
#83486 = CARTESIAN_POINT ( 'NONE',  ( 21.09922568453595559, 12.04030133659708746, -6.408140936763230044 ) ) ;
#83487 = AXIS2_PLACEMENT_3D ( 'NONE', #21488, #98000, #51985 ) ;
#83488 = LINE ( 'NONE', #45984, #49674 ) ;
#83489 = CARTESIAN_POINT ( 'NONE',  ( -0.8801773607111008646, 48.27201867748816966, 2.915334737309923430 ) ) ;
#83490 = MECHANICAL_DESIGN_GEOMETRIC_PRESENTATION_REPRESENTATION (  '', ( #96270 ), #24408 ) ;
#83491 = CARTESIAN_POINT ( 'NONE',  ( -0.3289641300568009741, 27.24545670184114243, -5.963430220938281678 ) ) ;
#83492 = FACE_OUTER_BOUND ( 'NONE', #14068, .T. ) ;
#83493 = CARTESIAN_POINT ( 'NONE',  ( 17.08211943468705130, 43.47041550158063927, 12.26659068614894998 ) ) ;
#83494 = CARTESIAN_POINT ( 'NONE',  ( -5.440088680355547268, 28.89701867748817321, 9.422509992056143702 ) ) ;
#83495 = CARTESIAN_POINT ( 'NONE',  ( 10.00000000000000178, 14.31368534415483751, 10.88017736071110342 ) ) ;
#83497 = CIRCLE ( 'NONE', #81824, 15.00000000000000000 ) ;
#83496 = CARTESIAN_POINT ( 'NONE',  ( 10.00000000000000178, 19.31368534415484106, 10.88017736071110342 ) ) ;
#83498 = CARTESIAN_POINT ( 'NONE',  ( 0.1532563361054082862, 51.21726448433412315, 2.638427012816831674 ) ) ;
#83499 = CARTESIAN_POINT ( 'NONE',  ( 21.09922568453594849, 56.20696800326375353, 6.408140936763242479 ) ) ;
#83500 = CARTESIAN_POINT ( 'NONE',  ( 1.707155281725178941, 42.90189080397286148, 6.499999999999955591 ) ) ;
#83501 = ORIENTED_EDGE ( 'NONE', *, *, #90416, .F. ) ;
#83502 = CARTESIAN_POINT ( 'NONE',  ( 4.559911319644449179, 18.89701867748817321, 9.422509992056141925 ) ) ;
#83503 = ADVANCED_FACE ( 'NONE', ( #88714 ), #5238, .T. ) ;
#83504 = CARTESIAN_POINT ( 'NONE',  ( 0.6178305044545838731, 19.74863466993042138, 9.382169495545420901 ) ) ;
#83505 = DIRECTION ( 'NONE',  ( 0.000000000000000000, 0.000000000000000000, 1.000000000000000000 ) ) ;
#83506 = CARTESIAN_POINT ( 'NONE',  ( 5.076628168052704559, 50.17559781766745886, -8.527530157486179263 ) ) ;
#83507 = CARTESIAN_POINT ( 'NONE',  ( 20.88017736071110519, 30.56368534415484106, 2.639326808657452039E-16 ) ) ;
#83508 = CARTESIAN_POINT ( 'NONE',  ( 3.591859063236761518, 24.95696800326375353, 11.09922568453594849 ) ) ;
#83510 = DIRECTION ( 'NONE',  ( 0.000000000000000000, 0.000000000000000000, -1.000000000000000000 ) ) ;
#83509 = CARTESIAN_POINT ( 'NONE',  ( -0.8801773607111008646, 48.27201867748816966, 2.915334737309923430 ) ) ;
#83511 = CARTESIAN_POINT ( 'NONE',  ( 18.61655166652077753, 54.87718327197430312, 6.499999999999981348 ) ) ;
#83512 = CARTESIAN_POINT ( 'NONE',  ( 6.565887622018943937, 50.16530133659708213, 12.81628187352647430 ) ) ;
#83513 = VERTEX_POINT ( 'NONE', #51215 ) ;
#83514 = CARTESIAN_POINT ( 'NONE',  ( 15.44008868035555260, 54.73035201082150536, 9.422509992056143702 ) ) ;
#83515 = CARTESIAN_POINT ( 'NONE',  ( 3.591859063236761518, 34.95696800326375353, 11.09922568453594849 ) ) ;
#83516 = CARTESIAN_POINT ( 'NONE',  ( 18.52753015748617571, 8.092264484334117824, 4.923371831947298993 ) ) ;
#83517 = CARTESIAN_POINT ( 'NONE',  ( 19.42250999205614193, 50.14701867748817676, 5.440088680355555262 ) ) ;
#83518 = CARTESIAN_POINT ( 'NONE',  ( 17.08211943468705130, 43.47041550158063927, 12.26659068614894998 ) ) ;
#83519 = PRESENTATION_LAYER_ASSIGNMENT (  '', '', ( #61161 ) ) ;
#83520 = DIRECTION ( 'NONE',  ( 0.000000000000000000, 1.000000000000000000, -0.000000000000000000 ) ) ;
#83521 = CARTESIAN_POINT ( 'NONE',  ( 1.472469842513823179, 11.42559781766745175, 4.923371831947296329 ) ) ;
#83522 = CARTESIAN_POINT ( 'NONE',  ( 17.20831665107776587, 7.883931151000784787, 7.208316651077764980 ) ) ;
#83523 = DIRECTION ( 'NONE',  ( 0.000000000000000000, 0.000000000000000000, 1.000000000000000000 ) ) ;
#83524 = CARTESIAN_POINT ( 'NONE',  ( 10.00000000000000000, 45.55374883491397497, -14.16423886937410082 ) ) ;
#83525 = AXIS2_PLACEMENT_3D ( 'NONE', #34143, #3681, #49640 ) ;
#83526 = CARTESIAN_POINT ( 'NONE',  ( 4.559911319644449179, 3.897018677488170990, 9.422509992056141925 ) ) ;
#83527 = CARTESIAN_POINT ( 'NONE',  ( -7.330124059959834071, -69.53998168068577002, -3.999999999999999112 ) ) ;
#83528 = ORIENTED_EDGE ( 'NONE', *, *, #56902, .T. ) ;
#83529 = AXIS2_PLACEMENT_3D ( 'NONE', #14717, #46663, #90686 ) ;
#83530 = CARTESIAN_POINT ( 'NONE',  ( 2.035157376598824452, 13.68868534415483751, 7.964842623401179544 ) ) ;
#83531 = CARTESIAN_POINT ( 'NONE',  ( -0.3689425029237881626, 57.42874883491397497, 10.36894250292379027 ) ) ;
#83532 = CARTESIAN_POINT ( 'NONE',  ( 19.84674366389459266, 48.71726448433413026, -2.638427012816827677 ) ) ;
#83533 = CARTESIAN_POINT ( 'NONE',  ( 21.09922568453594849, 41.20696800326375353, 6.408140936763242479 ) ) ;
#83534 = CYLINDRICAL_SURFACE ( 'NONE', #87451, 7.000000000000006217 ) ;
#83536 = CARTESIAN_POINT ( 'NONE',  ( 6.204703633549690345, 7.845415501580634832, 14.16423886937410082 ) ) ;
#83535 = CARTESIAN_POINT ( 'NONE',  ( 3.836325488036079534, 14.63606917487430970, 14.50112432709429378 ) ) ;
#83537 = CARTESIAN_POINT ( 'NONE',  ( -0.8801773607110991993, 17.85535201082150536, -2.915334737309923874 ) ) ;
#83538 = CARTESIAN_POINT ( 'NONE',  ( 10.00000000000000000, 1.813685344154838175, -10.88017736071110342 ) ) ;
#83539 = CARTESIAN_POINT ( 'NONE',  ( 1.472469842513823179, 40.59226448433411605, -4.923371831947296329 ) ) ;
#83540 = CARTESIAN_POINT ( 'NONE',  ( 12.03829478939427666, 15.00000000000000888, -8.307695547791400514 ) ) ;
#83541 = CARTESIAN_POINT ( 'NONE',  ( 10.00000000000000000, 24.75893115100078745, -9.846743663894594434 ) ) ;
#83542 = DIRECTION ( 'NONE',  ( 0.000000000000000000, 0.000000000000000000, 1.000000000000000000 ) ) ;
#83543 = CARTESIAN_POINT ( 'NONE',  ( 4.923371831947301658, 12.67559781766745886, 8.527530157486175710 ) ) ;
#83544 = ORIENTED_EDGE ( 'NONE', *, *, #34284, .T. ) ;
#83545 = ORIENTED_EDGE ( 'NONE', *, *, #98535, .F. ) ;
#83547 = EDGE_CURVE ( 'NONE', #87897, #91043, #65204, .T. ) ;
#83546 = CARTESIAN_POINT ( 'NONE',  ( 0.04758788293972446987, 0.000000000000000000, -5.453031268574422441 ) ) ;
#83548 = EDGE_LOOP ( 'NONE', ( #28869, #92520 ) ) ;
#83549 = CARTESIAN_POINT ( 'NONE',  ( 12.63842701281683034, 57.46726448433411605, 9.846743663894596210 ) ) ;
#83551 = CARTESIAN_POINT ( 'NONE',  ( 4.559911319644449179, 37.23035201082150536, -9.422509992056141925 ) ) ;
#83550 = CARTESIAN_POINT ( 'NONE',  ( 12.91533473730992121, 39.52201867748817676, 10.88017736071110164 ) ) ;
#83553 = CARTESIAN_POINT ( 'NONE',  ( 21.09922568453594849, 36.20696800326375353, 6.408140936763242479 ) ) ;
#83552 = CARTESIAN_POINT ( 'NONE',  ( 3.969999999999999751, 10.00000000000000000, -2.750000000000000000 ) ) ;
#83554 = CARTESIAN_POINT ( 'NONE',  ( 20.36894250292379382, 3.678748834913967869, 10.36894250292379205 ) ) ;
#83555 = ADVANCED_FACE ( 'NONE', ( #58710 ), #88296, .T. ) ;
#83556 = EDGE_CURVE ( 'NONE', #88170, #56402, #21212, .T. ) ;
#83557 = CARTESIAN_POINT ( 'NONE',  ( 19.38216949554541202, 45.99863466993041072, 9.382169495545424454 ) ) ;
#83558 = EDGE_CURVE ( 'NONE', #22423, #91046, #79580, .T. ) ;
#83559 = ORIENTED_EDGE ( 'NONE', *, *, #70129, .T. ) ;
#83560 = CARTESIAN_POINT ( 'NONE',  ( 5.076628168052703671, 41.84226448433411605, 8.527530157486179263 ) ) ;
#83561 = CARTESIAN_POINT ( 'NONE',  ( 4.559911319644449179, 8.897018677488173211, 9.422509992056141925 ) ) ;
#83562 = VERTEX_POINT ( 'NONE', #19239 ) ;
#83563 = PLANE ( 'NONE',  #62284 ) ;
#83564 = AXIS2_PLACEMENT_3D ( 'NONE', #85086, #39599, #94058 ) ;
#83565 = CARTESIAN_POINT ( 'NONE',  ( 10.00000000000000000, 21.81368534415484106, -10.88017736071110342 ) ) ;
#83566 = ORIENTED_EDGE ( 'NONE', *, *, #60962, .F. ) ;
#83567 = CARTESIAN_POINT ( 'NONE',  ( 2.035157376598824452, 58.68868534415482685, 7.964842623401179544 ) ) ;
#83568 = CARTESIAN_POINT ( 'NONE',  ( 20.88017736071110875, 55.77201867748816966, -2.915334737309920765 ) ) ;
#83569 = CARTESIAN_POINT ( 'NONE',  ( 20.88017736071110875, 65.77201867748817676, -2.915334737309920765 ) ) ;
#83570 = VECTOR ( 'NONE', #36841, 1000.000000000000000 ) ;
#83571 = CARTESIAN_POINT ( 'NONE',  ( 7.084665262690076126, 57.02201867748817676, -10.88017736071110164 ) ) ;
#83572 = DIRECTION ( 'NONE',  ( 0.000000000000000000, 0.000000000000000000, -1.000000000000000000 ) ) ;
#83574 = VERTEX_POINT ( 'NONE', #89701 ) ;
#83573 = CARTESIAN_POINT ( 'NONE',  ( 10.93144397355366770, -92.98246991212813839, 4.000000000000000000 ) ) ;
#83575 = CARTESIAN_POINT ( 'NONE',  ( 19.84674366389459621, 48.50893115100078745, 7.409399052514197653E-17 ) ) ;
#83576 = ORIENTED_EDGE ( 'NONE', *, *, #33865, .T. ) ;
#83577 = CARTESIAN_POINT ( 'NONE',  ( 19.80832241502127644, 19.75868815902069642, 6.499999999999986677 ) ) ;
#83578 = EDGE_CURVE ( 'NONE', #48651, #91690, #74704, .T. ) ;
#83579 = CARTESIAN_POINT ( 'NONE',  ( -2.266590686148945544, 1.387082168247301128, -7.082119434687050408 ) ) ;
#83580 = ORIENTED_EDGE ( 'NONE', *, *, #11165, .F. ) ;
#83581 = DIRECTION ( 'NONE',  ( 0.6246950475544238435, 0.7808688094430307203, 0.000000000000000000 ) ) ;
#83582 = CARTESIAN_POINT ( 'NONE',  ( 18.72515096720583827, 30.05509018479937566, 6.499999999999810818 ) ) ;
#83583 = CARTESIAN_POINT ( 'NONE',  ( 7.084665262690076126, 2.022018677488171434, -10.88017736071110164 ) ) ;
#83584 = CARTESIAN_POINT ( 'NONE',  ( 0.1532563361054100626, 65.80059781766745175, -2.638427012816831230 ) ) ;
#83586 = EDGE_LOOP ( 'NONE', ( #39033, #77481, #22197, #50713 ) ) ;
#83585 = CARTESIAN_POINT ( 'NONE',  ( 21.09922568453595559, 47.04030133659708923, -6.408140936763230044 ) ) ;
#83587 = FACE_OUTER_BOUND ( 'NONE', #34494, .T. ) ;
#83588 = CARTESIAN_POINT ( 'NONE',  ( 18.52753015748618282, 48.92559781766745886, -4.923371831947291888 ) ) ;
#83589 = CARTESIAN_POINT ( 'NONE',  ( 14.92337183194729988, 4.342264484334117824, -8.527530157486177487 ) ) ;
#83591 = COLOUR_RGB ( '', 0.72549020, 0.75294118, 0.79215686) ;
#83590 = CARTESIAN_POINT ( 'NONE',  ( 3.591859063236763294, 13.29030133659708746, -11.09922568453595026 ) ) ;
#83592 = CARTESIAN_POINT ( 'NONE',  ( 17.20831665107776587, 22.88393115100078745, 7.208316651077764980 ) ) ;
#83593 = DIRECTION ( 'NONE',  ( 0.000000000000000000, 0.000000000000000000, -1.000000000000000000 ) ) ;
#83594 = CARTESIAN_POINT ( 'NONE',  ( 22.81628187352648496, 1.831968003263753753, -3.434112377981050290 ) ) ;
#83595 = ADVANCED_FACE ( 'NONE', ( #57227 ), #77090, .T. ) ;
#83596 = LINE ( 'NONE', #67612, #509 ) ;
#83597 = VECTOR ( 'NONE', #95876, 1000.000000000000000 ) ;
#83598 = VERTEX_POINT ( 'NONE', #4248 ) ;
#83599 = B_SPLINE_CURVE_WITH_KNOTS ( 'NONE', 3,
 ( #42617, #36094, #73592, #51101 ),
 .UNSPECIFIED., .F., .F.,
 ( 4, 4 ),
 ( 5.284504157781969479E-17, 0.002562518741975523297 ),
 .UNSPECIFIED. ) ;
#83600 = VERTEX_POINT ( 'NONE', #91682 ) ;
#83601 = CARTESIAN_POINT ( 'NONE',  ( 17.96484262340118221, 26.18868534415483396, -7.964842623401177768 ) ) ;
#83602 = CARTESIAN_POINT ( 'NONE',  ( 24.16423886937410614, 14.30374883491396787, 8.672049930838204340E-16 ) ) ;
#83603 = CARTESIAN_POINT ( 'NONE',  ( 10.00000000000000000, 24.75893115100078745, -9.846743663894594434 ) ) ;
#83604 = CARTESIAN_POINT ( 'NONE',  ( 1.472469842513823179, 0.5922644843341181575, -4.923371831947296329 ) ) ;
#83606 = CARTESIAN_POINT ( 'NONE',  ( -6.000000000000000000, 78.07179676972447169, 4.250000000000000000 ) ) ;
#83605 = CARTESIAN_POINT ( 'NONE',  ( -2.816281873526473856, 34.12363466993042493, 9.499525473075851096E-16 ) ) ;
#83607 = CARTESIAN_POINT ( 'NONE',  ( -0.8801773607111009756, 13.06368534415483929, 1.068504757029289695E-15 ) ) ;
#83608 = CARTESIAN_POINT ( 'NONE',  ( -9.997910040112463648, 15.00000000000000000, -10.50199004140731773 ) ) ;
#83609 = CARTESIAN_POINT ( 'NONE',  ( 21.09922568453595559, 12.04030133659708746, -6.408140936763230044 ) ) ;
#83610 = CARTESIAN_POINT ( 'NONE',  ( 22.81628187352647785, 6.415301336597088344, 3.434112377981063169 ) ) ;
#83611 = CARTESIAN_POINT ( 'NONE',  ( 17.20831665107776587, 24.13393115100078035, -7.208316651077762316 ) ) ;
#83612 = CARTESIAN_POINT ( 'NONE',  ( -2.915334737309934532, -17.97798132251182324, -10.88017736071109987 ) ) ;
#83613 = CARTESIAN_POINT ( 'NONE',  ( -1.099225684535947600, 29.54030133659708923, 6.408140936763237150 ) ) ;
#83614 = DIRECTION ( 'NONE',  ( 0.000000000000000000, 0.000000000000000000, -1.000000000000000000 ) ) ;
#83616 = CARTESIAN_POINT ( 'NONE',  ( 14.43100913236846772, 15.00000000000000000, 1.412789942453269054 ) ) ;
#83615 = CARTESIAN_POINT ( 'NONE',  ( 0.5774900079438607392, 43.48035201082151247, 5.440088680355550821 ) ) ;
#83617 = CARTESIAN_POINT ( 'NONE',  ( -14.62617646268082972, 0.5000000000000004441, -3.327906561567078647 ) ) ;
#83618 = DIRECTION ( 'NONE',  ( 0.000000000000000000, 1.000000000000000000, 0.000000000000000000 ) ) ;
#83619 = CARTESIAN_POINT ( 'NONE',  ( 10.00000000000000178, 34.31368534415484106, 10.88017736071110342 ) ) ;
#83620 = CARTESIAN_POINT ( 'NONE',  ( 20.88017736071110519, 45.56368534415484106, 2.639326808657452039E-16 ) ) ;
#83621 = CARTESIAN_POINT ( 'NONE',  ( 10.00000000000000000, 64.75893115100078035, -9.846743663894594434 ) ) ;
#83622 = CARTESIAN_POINT ( 'NONE',  ( 17.96484262340118221, 66.18868534415483396, -7.964842623401177768 ) ) ;
#83623 = COLOUR_RGB ( '', 0.08235294, 0.09019608, 0.10196078) ;
#83624 = CARTESIAN_POINT ( 'NONE',  ( 5.076628168052703671, 46.84226448433412315, 8.527530157486179263 ) ) ;
#83626 = CARTESIAN_POINT ( 'NONE',  ( -9.876730923139378504, 0.5000000000000004441, 11.28938378619056415 ) ) ;
#83625 = CARTESIAN_POINT ( 'NONE',  ( -0.8801773607111008646, 8.272018677488171434, 2.915334737309923430 ) ) ;
#83627 = CARTESIAN_POINT ( 'NONE',  ( 22.81628187352647785, 6.623634669930420493, 6.195893100308588602E-16 ) ) ;
#83628 = ORIENTED_EDGE ( 'NONE', *, *, #64347, .F. ) ;
#83629 = CARTESIAN_POINT ( 'NONE',  ( 7.084665262690076126, 37.02201867748817676, -10.88017736071110164 ) ) ;
#83630 = VECTOR ( 'NONE', #85934, 1000.000000000000000 ) ;
#83632 = PLANE ( 'NONE',  #76454 ) ;
#83631 = CARTESIAN_POINT ( 'NONE',  ( -2.816281873526473856, -0.6680319967362464695, 3.434112377981055619 ) ) ;
#83633 = CARTESIAN_POINT ( 'NONE',  ( 4.559911319644449179, 27.23035201082150536, -9.422509992056141925 ) ) ;
#83634 = CARTESIAN_POINT ( 'NONE',  ( -4.164238869374099927, 37.01208216824731068, 3.795296366450308767 ) ) ;
#83635 = CARTESIAN_POINT ( 'NONE',  ( 10.00000000000000178, 32.25893115100078745, 9.846743663894594434 ) ) ;
#83636 = CARTESIAN_POINT ( 'NONE',  ( 17.96484262340118221, 51.18868534415483396, -7.964842623401177768 ) ) ;
#83637 = DIRECTION ( 'NONE',  ( 0.6755902076156493630, 0.000000000000000000, 0.7372773368101340763 ) ) ;
#83638 = CARTESIAN_POINT ( 'NONE',  ( 24.16423886937410614, 9.512082168247301794, -3.795296366450302550 ) ) ;
#83639 = EDGE_CURVE ( 'NONE', #76841, #27600, #61177, .T. ) ;
#83640 =( NAMED_UNIT ( * ) PLANE_ANGLE_UNIT ( ) SI_UNIT ( $, .RADIAN. ) );
#83641 = CARTESIAN_POINT ( 'NONE',  ( 0.1532563361054082862, 56.21726448433411605, 2.638427012816831674 ) ) ;
#83642 = ORIENTED_EDGE ( 'NONE', *, *, #17668, .T. ) ;
#83643 = ORIENTED_EDGE ( 'NONE', *, *, #7626, .F. ) ;
#83644 = CARTESIAN_POINT ( 'NONE',  ( 6.204703633549690345, 37.84541550158063927, 14.16423886937410082 ) ) ;
#83645 = CARTESIAN_POINT ( 'NONE',  ( 6.204703633549690345, 22.84541550158062861, 14.16423886937410082 ) ) ;
#83646 = CARTESIAN_POINT ( 'NONE',  ( 7.084665262690076126, 69.10535201082151957, 10.88017736071109987 ) ) ;
#83647 = CARTESIAN_POINT ( 'NONE',  ( -0.8801773607110991993, 2.855352010821504471, -2.915334737309923874 ) ) ;
#83648 = CARTESIAN_POINT ( 'NONE',  ( 5.076628168052704559, 50.17559781766745886, -8.527530157486179263 ) ) ;
#83649 = CARTESIAN_POINT ( 'NONE',  ( -11.16005593731603618, -52.90553718811315775, 3.750000000000000000 ) ) ;
#83651 = CARTESIAN_POINT ( 'NONE',  ( 16.40814093676323893, 20.79030133659708923, 11.09922568453595026 ) ) ;
#83650 = CARTESIAN_POINT ( 'NONE',  ( 0.5774900079438607392, 43.48035201082151247, 5.440088680355550821 ) ) ;
#83652 = CARTESIAN_POINT ( 'NONE',  ( 24.16423886937410614, 14.30374883491396787, 8.672049930838204340E-16 ) ) ;
#83653 = CARTESIAN_POINT ( 'NONE',  ( 10.00000000000000178, 14.31368534415483929, 10.88017736071110342 ) ) ;
#83654 = CARTESIAN_POINT ( 'NONE',  ( -0.8801773607111009756, 33.06368534415484106, 1.068504757029289695E-15 ) ) ;
#83655 = CARTESIAN_POINT ( 'NONE',  ( -6.689969769699040114, 15.00000000000000000, 12.58200319823965785 ) ) ;
#83656 = CARTESIAN_POINT ( 'NONE',  ( -0.8801773607111008646, 58.27201867748816966, 2.915334737309923430 ) ) ;
#83657 = CARTESIAN_POINT ( 'NONE',  ( 9.846743663894590881, -26.69940218233254470, 2.638427012816828565 ) ) ;
#83658 = ORIENTED_EDGE ( 'NONE', *, *, #90304, .T. ) ;
#83659 = DIRECTION ( 'NONE',  ( -0.2503800040544453820, 0.000000000000000000, 0.9681476403781066331 ) ) ;
#83660 = DIRECTION ( 'NONE',  ( -1.000000000000000000, 0.000000000000000000, 0.000000000000000000 ) ) ;
#83661 = DIRECTION ( 'NONE',  ( 0.000000000000000000, 1.000000000000000000, 0.000000000000000000 ) ) ;
#83662 = ORIENTED_EDGE ( 'NONE', *, *, #63448, .T. ) ;
#83663 = CYLINDRICAL_SURFACE ( 'NONE', #21742, 0.2500000000000002220 ) ;
#83665 = CARTESIAN_POINT ( 'NONE',  ( 22.26659068614895176, 59.72041550158063927, -7.082119434687042414 ) ) ;
#83664 = CARTESIAN_POINT ( 'NONE',  ( 24.16423886937409904, 64.09541550158064638, 3.795296366450317205 ) ) ;
#83667 = CARTESIAN_POINT ( 'NONE',  ( 0.1532563361054082862, 56.21726448433411605, 2.638427012816831674 ) ) ;
#83666 = CARTESIAN_POINT ( 'NONE',  ( 1.472469842513823179, 26.42559781766745175, 4.923371831947296329 ) ) ;
#83668 = FACE_OUTER_BOUND ( 'NONE', #78741, .T. ) ;
#83669 = CARTESIAN_POINT ( 'NONE',  ( 19.72487221294571569, 49.78217586085237656, 6.499999999999993783 ) ) ;
#83670 = CARTESIAN_POINT ( 'NONE',  ( 12.63842701281683922, 9.550597817667449974, -9.846743663894590881 ) ) ;
#83671 = EDGE_CURVE ( 'NONE', #34469, #48237, #92665, .T. ) ;
#83672 = CARTESIAN_POINT ( 'NONE',  ( -12.81628187352647963, 23.91530133659708213, -3.434112377981046293 ) ) ;
#83673 = EDGE_CURVE ( 'NONE', #36015, #69849, #46186, .T. ) ;
#83674 = VERTEX_POINT ( 'NONE', #92173 ) ;
#83675 = CARTESIAN_POINT ( 'NONE',  ( 10.00000000000000000, 30.55374883491397142, -14.16423886937410082 ) ) ;
#83676 = CARTESIAN_POINT ( 'NONE',  ( 13.79529636645031943, 40.34541550158063217, -14.16423886937409904 ) ) ;
#83677 = ORIENTED_EDGE ( 'NONE', *, *, #58135, .T. ) ;
#83678 = CARTESIAN_POINT ( 'NONE',  ( -2.816281873526473856, 54.12363466993041783, 9.499525473075851096E-16 ) ) ;
#83679 = CARTESIAN_POINT ( 'NONE',  ( 0.5774900079438590739, 27.64701867748817676, -5.440088680355550821 ) ) ;
#83680 = CARTESIAN_POINT ( 'NONE',  ( 7.361572987183169658, 49.96726448433410894, -9.846743663894592657 ) ) ;
#83681 = CARTESIAN_POINT ( 'NONE',  ( 17.96484262340118221, 24.93868534415484461, 7.964842623401181321 ) ) ;
#83682 = CARTESIAN_POINT ( 'NONE',  ( 21.09922568453594849, 61.20696800326376064, 6.408140936763242479 ) ) ;
#83683 = DIRECTION ( 'NONE',  ( 0.000000000000000000, 1.000000000000000000, 0.000000000000000000 ) ) ;
#83684 = CARTESIAN_POINT ( 'NONE',  ( 18.52753015748617571, 58.09226448433411605, 4.923371831947298993 ) ) ;
#83685 = CARTESIAN_POINT ( 'NONE',  ( 17.20831665107776587, 49.13393115100078745, -7.208316651077762316 ) ) ;
#83687 = ORIENTED_EDGE ( 'NONE', *, *, #48244, .F. ) ;
#83686 = CARTESIAN_POINT ( 'NONE',  ( 3.469446951953614189E-15, 3.912123368507817833, 11.92686044187656513 ) ) ;
#83688 = CARTESIAN_POINT ( 'NONE',  ( 3.969999999999999751, 10.25000000000000000, -4.000000000000000000 ) ) ;
#83689 = VECTOR ( 'NONE', #33684, 1000.000000000000000 ) ;
#83690 = CARTESIAN_POINT ( 'NONE',  ( 17.20831665107776587, 2.883931151000785231, 7.208316651077764980 ) ) ;
#83691 = EDGE_LOOP ( 'NONE', ( #26081, #820, #96116, #16533, #58908, #28490 ) ) ;
#83692 = CARTESIAN_POINT ( 'NONE',  ( -0.1298530154764001854, 80.39370036920264795, 9.500000000000000000 ) ) ;
#83693 = CARTESIAN_POINT ( 'NONE',  ( 0.1532563361054082862, 36.21726448433410894, 2.638427012816831674 ) ) ;
#83694 = DIRECTION ( 'NONE',  ( 0.000000000000000000, 0.000000000000000000, 1.000000000000000000 ) ) ;
#83695 = CARTESIAN_POINT ( 'NONE',  ( 10.00000000000000000, 32.87363466993042493, -12.81628187352647608 ) ) ;
#83697 = DIRECTION ( 'NONE',  ( 0.000000000000000000, 0.000000000000000000, 1.000000000000000000 ) ) ;
#83696 = AXIS2_PLACEMENT_3D ( 'NONE', #44725, #53218, #8221 ) ;
#83698 = EDGE_CURVE ( 'NONE', #51739, #94197, #796, .T. ) ;
#83699 = CARTESIAN_POINT ( 'NONE',  ( -10.64017930668218881, 14.49999999999999112, 10.57291749337211151 ) ) ;
#83700 = CARTESIAN_POINT ( 'NONE',  ( -5.451370222425315326, 0.000000000000000000, 0.1427491530889740401 ) ) ;
#83701 = DIRECTION ( 'NONE',  ( 0.000000000000000000, 1.000000000000000000, 0.000000000000000000 ) ) ;
#83702 = CARTESIAN_POINT ( 'NONE',  ( 5.076628168052703671, 41.84226448433411605, 8.527530157486179263 ) ) ;
#83703 = CARTESIAN_POINT ( 'NONE',  ( -4.164238869374099039, 31.80374883491396432, 8.674139862899312516E-16 ) ) ;
#83704 = CARTESIAN_POINT ( 'NONE',  ( 0.1532563361054082862, 66.21726448433413736, 2.638427012816831674 ) ) ;
#83705 = PLANE ( 'NONE',  #52759 ) ;
#83706 = CARTESIAN_POINT ( 'NONE',  ( 14.92337183194729633, 7.675597817667451750, 8.527530157486181039 ) ) ;
#83707 = CARTESIAN_POINT ( 'NONE',  ( 6.204703633549690345, 0.7620821682473009062, -14.16423886937410259 ) ) ;
#83708 = CARTESIAN_POINT ( 'NONE',  ( 5.076628168052704559, 45.17559781766745175, -8.527530157486179263 ) ) ;
#83709 = CARTESIAN_POINT ( 'NONE',  ( 20.88017736071110519, 55.56368534415484817, 2.639326808657452039E-16 ) ) ;
#83710 = CARTESIAN_POINT ( 'NONE',  ( 19.84674366389459266, 43.71726448433410894, -2.638427012816827677 ) ) ;
#83711 = DIRECTION ( 'NONE',  ( 0.9170600743851238246, 0.000000000000000000, -0.3987490689252466414 ) ) ;
#83712 = CARTESIAN_POINT ( 'NONE',  ( -0.8801773607111008646, 48.27201867748816966, 2.915334737309923430 ) ) ;
#83713 = ORIENTED_EDGE ( 'NONE', *, *, #74478, .F. ) ;
#83714 = CARTESIAN_POINT ( 'NONE',  ( 0.9408516040111469803, 22.46693863883976050, -6.499999999999953815 ) ) ;
#83715 = CARTESIAN_POINT ( 'NONE',  ( 19.42250999205614193, 35.14701867748816966, 5.440088680355555262 ) ) ;
#83717 = CARTESIAN_POINT ( 'NONE',  ( -0.8801773607111008646, 63.27201867748817676, 2.915334737309923430 ) ) ;
#83716 = CARTESIAN_POINT ( 'NONE',  ( -2.816281873526471635, 3.915301336597087456, -3.434112377981056508 ) ) ;
#83718 = DIRECTION ( 'NONE',  ( 0.5519369853120560387, 0.000000000000000000, 0.8338858220671695465 ) ) ;
#83719 = CARTESIAN_POINT ( 'NONE',  ( 19.72487221294570858, 4.782175860852374782, 6.500000000000002665 ) ) ;
#83720 = LINE ( 'NONE', #6734, #29365 ) ;
#83722 = CARTESIAN_POINT ( 'NONE',  ( 20.00000000000001066, 95.39111596594167963, -4.637569772578755689 ) ) ;
#83721 = CARTESIAN_POINT ( 'NONE',  ( 20.88017736071110875, 45.77201867748816966, -2.915334737309920765 ) ) ;
#83723 = CARTESIAN_POINT ( 'NONE',  ( 10.00000000000000178, 12.25893115100078568, 9.846743663894594434 ) ) ;
#83724 = CARTESIAN_POINT ( 'NONE',  ( 19.84674366389459621, 33.50893115100078745, 7.409399052514197653E-17 ) ) ;
#83725 = CARTESIAN_POINT ( 'NONE',  ( 20.15039907845753220, 57.62777174578613426, -6.262539305110077947 ) ) ;
#83726 =( BOUNDED_CURVE ( )  B_SPLINE_CURVE ( 2, ( #71514, #63972, #4490, #86988, #87479, #18992, #34462, #78995, #10501 ),
 .UNSPECIFIED., .F., .T. ) 
 B_SPLINE_CURVE_WITH_KNOTS ( ( 3, 2, 2, 2, 3 ),
 ( 0.7615695083688026612, 0.7619047619047618625, 0.7678571428571429047, 0.7738095238095238360, 0.7741447773454829262 ),
 .UNSPECIFIED. ) 
 CURVE ( )  GEOMETRIC_REPRESENTATION_ITEM ( )  RATIONAL_B_SPLINE_CURVE ( ( 0.9963778908391753841, 0.9980808541467917072, 1.000000000000000000, 0.9659258262890683122, 1.000000000000000000, 0.9659258262890683122, 1.000000000000000000, 0.9980808541467922623, 0.9963778908391764944 ) ) 
 REPRESENTATION_ITEM ( '' )  );
#83727 = CARTESIAN_POINT ( 'NONE',  ( -12.26659068614895354, 16.38708216824731068, -7.082119434687038861 ) ) ;
#83728 = CARTESIAN_POINT ( 'NONE',  ( 13.43411237798105340, 0.5819680032637533085, 12.81628187352647963 ) ) ;
#83729 = CARTESIAN_POINT ( 'NONE',  ( 12.91533473730992121, 4.522018677488170546, 10.88017736071110164 ) ) ;
#83730 = DIRECTION ( 'NONE',  ( 0.8070303256584298035, -0.5905099943842175847, 0.000000000000000000 ) ) ;
#83731 = VECTOR ( 'NONE', #30748, 1000.000000000000227 ) ;
#83732 = CARTESIAN_POINT ( 'NONE',  ( 22.26659068614895176, 19.72041550158063572, -7.082119434687042414 ) ) ;
#83733 = CARTESIAN_POINT ( 'NONE',  ( 10.00000000000000178, 53.05374883491396787, 14.16423886937410082 ) ) ;
#83734 = CARTESIAN_POINT ( 'NONE',  ( 18.52753015748617571, 23.09226448433411960, 4.923371831947298993 ) ) ;
#83735 =( NAMED_UNIT ( * ) PLANE_ANGLE_UNIT ( ) SI_UNIT ( $, .RADIAN. ) );
#83736 = ORIENTED_EDGE ( 'NONE', *, *, #21475, .F. ) ;
#83737 = CARTESIAN_POINT ( 'NONE',  ( 0.1532563361054083140, 26.00893115100078745, 1.131784320476157264E-15 ) ) ;
#83738 = CARTESIAN_POINT ( 'NONE',  ( 10.00000000000000000, 31.81368534415483751, -10.88017736071110342 ) ) ;
#83739 = CARTESIAN_POINT ( 'NONE',  ( 10.00000000000000000, 49.75893115100078745, -9.846743663894594434 ) ) ;
#83740 = CARTESIAN_POINT ( 'NONE',  ( 20.36894250292379382, 13.67874883491396965, 10.36894250292379205 ) ) ;
#83741 = FACE_OUTER_BOUND ( 'NONE', #47883, .T. ) ;
#83742 = CARTESIAN_POINT ( 'NONE',  ( 2.791683348922240793, 11.63393115100078568, 7.208316651077764092 ) ) ;
#83743 = CARTESIAN_POINT ( 'NONE',  ( 0.6178305044545838731, 39.74863466993041072, 9.382169495545420901 ) ) ;
#83744 = B_SPLINE_CURVE_WITH_KNOTS ( 'NONE', 3,
 ( #98251, #29709, #83714, #60217 ),
 .UNSPECIFIED., .F., .F.,
 ( 4, 4 ),
 ( 0.000000000000000000, 0.001036303429213395648 ),
 .UNSPECIFIED. ) ;
#83745 = CARTESIAN_POINT ( 'NONE',  ( 1.472469842513823179, 45.59226448433412315, -4.923371831947296329 ) ) ;
#83746 = ORIENTED_EDGE ( 'NONE', *, *, #76871, .F. ) ;
#83747 = CARTESIAN_POINT ( 'NONE',  ( 7.361572987183170547, 27.05059781766745175, 9.846743663894590881 ) ) ;
#83748 = CARTESIAN_POINT ( 'NONE',  ( 11.10657215103663553, -52.67603735984217650, -3.750000000001792788 ) ) ;
#83749 = LINE ( 'NONE', #44256, #1193 ) ;
#83750 = CARTESIAN_POINT ( 'NONE',  ( 22.26659068614894466, 58.88708216824729647, 7.082119434687054849 ) ) ;
#83751 = CARTESIAN_POINT ( 'NONE',  ( -0.8801773607111008646, 43.27201867748817676, 2.915334737309923430 ) ) ;
#83752 = CARTESIAN_POINT ( 'NONE',  ( -0.1503990784575247319, 32.22266099184917465, -6.262539305110083276 ) ) ;
#83753 = DIRECTION ( 'NONE',  ( 0.000000000000000000, 1.000000000000000000, 0.000000000000000000 ) ) ;
#83754 = CARTESIAN_POINT ( 'NONE',  ( 19.84674366389459621, 33.50893115100078745, 7.409399052514197653E-17 ) ) ;
#83755 = CARTESIAN_POINT ( 'NONE',  ( 0.1532563361054100626, 40.80059781766745886, -2.638427012816831230 ) ) ;
#83756 = DIRECTION ( 'NONE',  ( 0.000000000000000000, 1.000000000000000000, 0.000000000000000000 ) ) ;
#83757 = CARTESIAN_POINT ( 'NONE',  ( 7.361572987183170547, 47.05059781766745175, 9.846743663894590881 ) ) ;
#83758 = EDGE_CURVE ( 'NONE', #63180, #91314, #80303, .T. ) ;
#83759 = CARTESIAN_POINT ( 'NONE',  ( 12.91533473730992121, 54.52201867748816255, 10.88017736071110164 ) ) ;
#83760 = B_SPLINE_CURVE_WITH_KNOTS ( 'NONE', 3,
 ( #29520, #44539, #76024, #37551, #7555, #83039 ),
 .UNSPECIFIED., .F., .F.,
 ( 4, 2, 4 ),
 ( 3.409110551494652110E-05, 0.0004400426677367922637, 0.0008459942299586379385 ),
 .UNSPECIFIED. ) ;
#83761 = ORIENTED_EDGE ( 'NONE', *, *, #39371, .T. ) ;
#83762 = EDGE_LOOP ( 'NONE', ( #85366, #6211, #35089, #56031 ) ) ;
#83763 = CARTESIAN_POINT ( 'NONE',  ( 16.40814093676324603, 57.45696800326375353, -11.09922568453594671 ) ) ;
#83764 = COLOUR_RGB ( '', 0.08235294, 0.09019608, 0.10196078) ;
#83765 = CARTESIAN_POINT ( 'NONE',  ( 19.84674366389459621, 13.50893115100078568, 7.409399052514197653E-17 ) ) ;
#83766 = CARTESIAN_POINT ( 'NONE',  ( 21.09922568453594849, 56.20696800326375353, 6.408140936763242479 ) ) ;
#83768 = CARTESIAN_POINT ( 'NONE',  ( 17.20831665107776587, 47.88393115100078745, 7.208316651077764980 ) ) ;
#83767 = CARTESIAN_POINT ( 'NONE',  ( 19.42250999205614548, 5.980352010821504471, -5.440088680355545492 ) ) ;
#83769 = CARTESIAN_POINT ( 'NONE',  ( 20.00000000000000711, 85.01043265490480394, 4.826711383682784628 ) ) ;
#83770 = CARTESIAN_POINT ( 'NONE',  ( 22.26659068614894466, 28.88708216824730357, 7.082119434687054849 ) ) ;
#83771 = CARTESIAN_POINT ( 'NONE',  ( 2.917880565312950480, 55.97041550158063217, -12.26659068614894821 ) ) ;
#83772 = CARTESIAN_POINT ( 'NONE',  ( 0.1532563361054083140, 61.00893115100078745, 1.131784320476157264E-15 ) ) ;
#83773 = CARTESIAN_POINT ( 'NONE',  ( 10.00000000000000000, 51.81368534415484106, -10.88017736071110342 ) ) ;
#83774 = CIRCLE ( 'NONE', #45426, 1.000000000000000888 ) ;
#83775 = CARTESIAN_POINT ( 'NONE',  ( 10.00000000000000000, 66.81368534415484817, -10.88017736071110342 ) ) ;
#83776 = FILL_AREA_STYLE_COLOUR ( '', #57335 ) ;
#83777 = ORIENTED_EDGE ( 'NONE', *, *, #71070, .T. ) ;
#83778 = CARTESIAN_POINT ( 'NONE',  ( 22.81628187352648496, 56.83196800326374643, -3.434112377981050290 ) ) ;
#83779 = ORIENTED_EDGE ( 'NONE', *, *, #3166, .F. ) ;
#83780 = CARTESIAN_POINT ( 'NONE',  ( 12.63842701281683034, 12.46726448433411782, 9.846743663894596210 ) ) ;
#83781 = ORIENTED_EDGE ( 'NONE', *, *, #95894, .F. ) ;
#83782 = CARTESIAN_POINT ( 'NONE',  ( 13.79529636645030344, 18.26208216824730002, 14.16423886937410614 ) ) ;
#83783 = CARTESIAN_POINT ( 'NONE',  ( 17.20831665107776587, 17.88393115100078745, 7.208316651077764980 ) ) ;
#83784 = CARTESIAN_POINT ( 'NONE',  ( 10.00000000000000178, 29.31368534415483751, 10.88017736071110342 ) ) ;
#83785 = CARTESIAN_POINT ( 'NONE',  ( 3.897244926436223444, 15.00000000000000000, -13.96644127841327787 ) ) ;
#83786 = ORIENTED_EDGE ( 'NONE', *, *, #66402, .T. ) ;
#83787 = CARTESIAN_POINT ( 'NONE',  ( 17.96484262340118221, 26.18868534415483396, -7.964842623401177768 ) ) ;
#83788 = EDGE_CURVE ( 'NONE', #87349, #88123, #27620, .T. ) ;
#83789 = COLOUR_RGB ( '', 0.66274510, 0.83137255, 0.94901961) ;
#83790 = B_SPLINE_CURVE_WITH_KNOTS ( 'NONE', 3,
 ( #63135, #47143, #56144, #25172, #9157, #25651 ),
 .UNSPECIFIED., .F., .F.,
 ( 4, 2, 4 ),
 ( 3.252606517456513784E-19, 0.0004056965545342626793, 0.0008113931090685250333 ),
 .UNSPECIFIED. ) ;
#83791 = EDGE_CURVE ( 'NONE', #54718, #88041, #37220, .T. ) ;
#83792 = EDGE_LOOP ( 'NONE', ( #64741, #2170, #42566, #70423, #49149, #11180 ) ) ;
#83793 = CARTESIAN_POINT ( 'NONE',  ( 0.5774900079438607392, 38.48035201082150536, 5.440088680355550821 ) ) ;
#83794 = DIRECTION ( 'NONE',  ( 0.000000000000000000, 1.000000000000000000, 0.000000000000000000 ) ) ;
#83795 = ORIENTED_EDGE ( 'NONE', *, *, #93272, .T. ) ;
#83796 = EDGE_LOOP ( 'NONE', ( #43495, #2996, #25268, #72936 ) ) ;
#83797 = CARTESIAN_POINT ( 'NONE',  ( 13.43411237798106583, 17.66530133659708923, -12.81628187352647252 ) ) ;
#83798 = SURFACE_SIDE_STYLE ('',( #77757 ) ) ;
#83799 = CARTESIAN_POINT ( 'NONE',  ( 7.361572987183169658, 14.96726448433411960, -9.846743663894592657 ) ) ;
#83800 = LINE ( 'NONE', #68312, #14343 ) ;
#83801 = CARTESIAN_POINT ( 'NONE',  ( 7.361572987183170547, 12.05059781766744997, 9.846743663894590881 ) ) ;
#83802 = CARTESIAN_POINT ( 'NONE',  ( 0.5774900079438590739, 32.64701867748816966, -5.440088680355550821 ) ) ;
#83803 = AXIS2_PLACEMENT_3D ( 'NONE', #30642, #75169, #6679 ) ;
#83804 = ORIENTED_EDGE ( 'NONE', *, *, #79517, .F. ) ;
#83805 = CARTESIAN_POINT ( 'NONE',  ( -7.154372922009654800, -0.03417435944610275333, 14.30707323420372035 ) ) ;
#83806 = CARTESIAN_POINT ( 'NONE',  ( -0.8801773607110991993, 62.85535201082150536, -2.915334737309923874 ) ) ;
#83807 = CARTESIAN_POINT ( 'NONE',  ( -0.1503990784575247319, 22.22266099184918886, -6.262539305110083276 ) ) ;
#83808 = CARTESIAN_POINT ( 'NONE',  ( 21.09922568453595559, 57.04030133659708923, -6.408140936763230044 ) ) ;
#83809 = CARTESIAN_POINT ( 'NONE',  ( 2.035157376598822676, 62.43868534415483396, -7.964842623401177768 ) ) ;
#83810 = CARTESIAN_POINT ( 'NONE',  ( 10.00000000000000178, 0.3736346699304200492, 12.81628187352647608 ) ) ;
#83811 = SURFACE_STYLE_USAGE ( .BOTH. , #90807 ) ;
#83812 = CARTESIAN_POINT ( 'NONE',  ( 0.1532563361054082862, 26.21726448433411605, 2.638427012816831674 ) ) ;
#83813 = CARTESIAN_POINT ( 'NONE',  ( 13.43411237798105340, 55.58196800326374643, 12.81628187352647963 ) ) ;
#83814 = DIRECTION ( 'NONE',  ( 1.000000000000000000, 0.000000000000000000, 0.000000000000000000 ) ) ;
#83815 = CARTESIAN_POINT ( 'NONE',  ( 17.20831665107776587, 4.133931151000785675, -7.208316651077762316 ) ) ;
#83816 = CARTESIAN_POINT ( 'NONE',  ( -2.816281873526473856, 24.12363466993042138, 9.499525473075851096E-16 ) ) ;
#83818 = DIRECTION ( 'NONE',  ( -6.608470384673550777E-17, -1.000000000000000000, 0.000000000000000000 ) ) ;
#83817 = CARTESIAN_POINT ( 'NONE',  ( -16.94000000000001194, 92.00000000000000000, -10.09898361729590199 ) ) ;
#83819 = CARTESIAN_POINT ( 'NONE',  ( -0.8801773607110991993, 32.85535201082151247, -2.915334737309923874 ) ) ;
#83820 = CARTESIAN_POINT ( 'NONE',  ( -2.816281873526473856, -0.8763653300695799508, 9.499525473075851096E-16 ) ) ;
#83821 = CARTESIAN_POINT ( 'NONE',  ( 7.551349515323100725, -0.03417435944610275333, 12.08468537022911349 ) ) ;
#83822 = EDGE_CURVE ( 'NONE', #32106, #93746, #73874, .T. ) ;
#83823 = CARTESIAN_POINT ( 'NONE',  ( 14.92337183194729633, 7.675597817667451750, 8.527530157486181039 ) ) ;
#83825 = VERTEX_POINT ( 'NONE', #6703 ) ;
#83824 = CARTESIAN_POINT ( 'NONE',  ( 13.43411237798105340, 10.58196800326375353, 12.81628187352647963 ) ) ;
#83826 = CARTESIAN_POINT ( 'NONE',  ( 19.84674366389459621, 63.50893115100078745, 7.409399052514197653E-17 ) ) ;
#83827 = VECTOR ( 'NONE', #43836, 1000.000000000000000 ) ;
#83828 = CARTESIAN_POINT ( 'NONE',  ( 12.91533473730993009, 6.605352010821504471, -10.88017736071109987 ) ) ;
#83829 = CARTESIAN_POINT ( 'NONE',  ( 14.92337183194729633, 42.67559781766745886, 8.527530157486181039 ) ) ;
#83830 = AXIS2_PLACEMENT_3D ( 'NONE', #20360, #73842, #97859 ) ;
#83831 =( BOUNDED_CURVE ( )  B_SPLINE_CURVE ( 2, ( #33909, #12410, #72909, #64897, #88415, #20419, #49917, #80428, #50905 ),
 .UNSPECIFIED., .F., .F. ) 
 B_SPLINE_CURVE_WITH_KNOTS ( ( 3, 2, 2, 2, 3 ),
 ( 0.01057180293546599974, 0.01190476190476190410, 0.01785714285714285615, 0.02380952380952380820, 0.02514248277882003349 ),
 .UNSPECIFIED. ) 
 CURVE ( )  GEOMETRIC_REPRESENTATION_ITEM ( )  RATIONAL_B_SPLINE_CURVE ( ( 0.9881565478350764486, 0.9923695281211519781, 1.000000000000000000, 0.9659258262890683122, 1.000000000000000000, 0.9659258262890683122, 1.000000000000000000, 0.9923695281211502017, 0.9881565478350745613 ) ) 
 REPRESENTATION_ITEM ( '' )  );
#83832 = DIRECTION ( 'NONE',  ( -0.000000000000000000, 1.000000000000000000, -0.000000000000000000 ) ) ;
#83833 = CARTESIAN_POINT ( 'NONE',  ( 10.00000000000000178, 9.313685344154839285, 10.88017736071110342 ) ) ;
#83834 = DIRECTION ( 'NONE',  ( -0.000000000000000000, 0.000000000000000000, -1.000000000000000000 ) ) ;
#83835 = CARTESIAN_POINT ( 'NONE',  ( 15.44008868035555793, 31.39701867748817676, -9.422509992056140149 ) ) ;
#83837 = FACE_OUTER_BOUND ( 'NONE', #12941, .T. ) ;
#83836 = CARTESIAN_POINT ( 'NONE',  ( -4.164238869374099039, 61.80374883491397497, 8.674139862899312516E-16 ) ) ;
#83838 = CARTESIAN_POINT ( 'NONE',  ( 10.00000000000000178, 7.258931151000785675, 9.846743663894594434 ) ) ;
#83839 = CARTESIAN_POINT ( 'NONE',  ( 17.20831665107776587, 19.13393115100078035, -7.208316651077762316 ) ) ;
#83840 = CARTESIAN_POINT ( 'NONE',  ( 16.40814093676323893, 15.79030133659708746, 11.09922568453595026 ) ) ;
#83841 = CARTESIAN_POINT ( 'NONE',  ( -46.94000000000001194, 103.2691844435154422, 6.361973263950303270 ) ) ;
#83842 = DIRECTION ( 'NONE',  ( 0.4305110968083047940, 0.000000000000000000, -0.9025852843498560762 ) ) ;
#83843 = CARTESIAN_POINT ( 'NONE',  ( 5.076628168052704559, 65.17559781766745175, -8.527530157486179263 ) ) ;
#83844 = CARTESIAN_POINT ( 'NONE',  ( 0.000000000000000000, 0.000000000000000000, 0.000000000000000000 ) ) ;
#83845 = SURFACE_SIDE_STYLE ('',( #76825 ) ) ;
#83846 = CARTESIAN_POINT ( 'NONE',  ( -4.164238869374099927, 7.012082168247302683, 3.795296366450308767 ) ) ;
#83847 = CARTESIAN_POINT ( 'NONE',  ( 1.472469842513823179, 31.42559781766745530, 4.923371831947296329 ) ) ;
#83848 = ORIENTED_EDGE ( 'NONE', *, *, #85350, .T. ) ;
#83849 = CIRCLE ( 'NONE', #35949, 0.5000000000000000000 ) ;
#83850 = CARTESIAN_POINT ( 'NONE',  ( 22.26659068614895176, 59.72041550158063927, -7.082119434687042414 ) ) ;
#83851 = CARTESIAN_POINT ( 'NONE',  ( 10.00000000000000000, 9.758931151000785675, -9.846743663894594434 ) ) ;
#83853 = CARTESIAN_POINT ( 'NONE',  ( 4.265659168453209915, 14.95077488074853456, 14.12268572233453590 ) ) ;
#83852 = FILL_AREA_STYLE_COLOUR ( '', #93044 ) ;
#83854 = CARTESIAN_POINT ( 'NONE',  ( 12.91533473730993009, 36.60535201082151247, -10.88017736071109987 ) ) ;
#83855 = CARTESIAN_POINT ( 'NONE',  ( 19.38216949554541202, 45.99863466993041072, 9.382169495545424454 ) ) ;
#83856 = CARTESIAN_POINT ( 'NONE',  ( 15.44008868035555793, 16.39701867748817321, -9.422509992056140149 ) ) ;
#83857 = CARTESIAN_POINT ( 'NONE',  ( 21.09922568453594849, 36.20696800326375353, 6.408140936763242479 ) ) ;
#83858 = CARTESIAN_POINT ( 'NONE',  ( 5.076628168052704559, 65.17559781766745175, -8.527530157486179263 ) ) ;
#83859 = CARTESIAN_POINT ( 'NONE',  ( 10.00000000000000000, 4.758931151000784787, -9.846743663894594434 ) ) ;
#83860 = EDGE_LOOP ( 'NONE', ( #53061, #15558, #88101, #50799 ) ) ;
#83861 = SURFACE_STYLE_USAGE ( .BOTH. , #43872 ) ;
#83862 = CARTESIAN_POINT ( 'NONE',  ( -11.29222593019763288, 14.76930270348881535, -9.783848334571407790 ) ) ;
#83863 = CARTESIAN_POINT ( 'NONE',  ( 13.79529636645030344, 38.26208216824729647, 14.16423886937410614 ) ) ;
#83864 = CARTESIAN_POINT ( 'NONE',  ( 13.79529636645031943, 20.34541550158063572, -14.16423886937409904 ) ) ;
#83865 = CARTESIAN_POINT ( 'NONE',  ( 15.44008868035555793, 11.39701867748817143, -9.422509992056140149 ) ) ;
#83866 = CARTESIAN_POINT ( 'NONE',  ( 12.91533473730992121, 34.52201867748817676, 10.88017736071110164 ) ) ;
#83867 = DIRECTION ( 'NONE',  ( -1.000000000000000000, -0.000000000000000000, -0.000000000000000000 ) ) ;
#83868 = CARTESIAN_POINT ( 'NONE',  ( 14.61046065509105674, -2.732951804315999255E-15, -0.6655452423542743690 ) ) ;
#83869 = CARTESIAN_POINT ( 'NONE',  ( 12.91533473730993009, 66.60535201082150536, -10.88017736071109987 ) ) ;
#83870 = CARTESIAN_POINT ( 'NONE',  ( 19.42250999205614548, 60.98035201082151247, -5.440088680355545492 ) ) ;
#83871 = CARTESIAN_POINT ( 'NONE',  ( 21.09922568453595559, 32.04030133659708923, -6.408140936763230044 ) ) ;
#83872 = CARTESIAN_POINT ( 'NONE',  ( 5.419894505350628222, 14.49999999999999112, -13.98659156302463735 ) ) ;
#83873 = CARTESIAN_POINT ( 'NONE',  ( -11.92686044187656513, 2.662123368507809840, 3.903127820947815962E-15 ) ) ;
#83874 = CARTESIAN_POINT ( 'NONE',  ( 14.92337183194729988, 39.34226448433412315, -8.527530157486177487 ) ) ;
#83875 = VECTOR ( 'NONE', #76814, 1000.000000000000000 ) ;
#83876 = EDGE_CURVE ( 'NONE', #26706, #82021, #53183, .T. ) ;
#83877 = CARTESIAN_POINT ( 'NONE',  ( 7.084665262690076126, 19.10535201082150181, 10.88017736071109987 ) ) ;
#83878 = CARTESIAN_POINT ( 'NONE',  ( 6.565887622018943937, 13.08196800326374998, -12.81628187352647608 ) ) ;
#83879 = CIRCLE ( 'NONE', #8859, 0.2500000000000002220 ) ;
#83880 = CARTESIAN_POINT ( 'NONE',  ( 10.00000000000000000, 14.75893115100078568, -9.846743663894594434 ) ) ;
#83881 = CARTESIAN_POINT ( 'NONE',  ( -0.8801773607111008646, 3.272018677488171434, 2.915334737309923430 ) ) ;
#83882 = CARTESIAN_POINT ( 'NONE',  ( 2.791683348922240793, 36.63393115100078035, 7.208316651077764092 ) ) ;
#83883 = CARTESIAN_POINT ( 'NONE',  ( -2.816281873526471635, 58.91530133659707502, -3.434112377981056508 ) ) ;
#83884 = CARTESIAN_POINT ( 'NONE',  ( 17.20831665107776587, 12.88393115100078390, 7.208316651077764980 ) ) ;
#83885 = CARTESIAN_POINT ( 'NONE',  ( -0.3689425029237898834, 6.178748834913968757, -10.36894250292378850 ) ) ;
#83886 = CARTESIAN_POINT ( 'NONE',  ( -13.78891971893199830, 0.5000000000000004441, -5.904717858191724567 ) ) ;
#83887 = CARTESIAN_POINT ( 'NONE',  ( 2.035157376598822676, 27.43868534415483396, -7.964842623401177768 ) ) ;
#83889 = CARTESIAN_POINT ( 'NONE',  ( 10.00000000000000178, 48.05374883491396787, 14.16423886937410082 ) ) ;
#83888 = CARTESIAN_POINT ( 'NONE',  ( 2.035157376598822676, 12.43868534415483751, -7.964842623401177768 ) ) ;
#83890 = CARTESIAN_POINT ( 'NONE',  ( 20.88017736071110164, 35.35535201082150536, 2.915334737309930979 ) ) ;
#83891 = CARTESIAN_POINT ( 'NONE',  ( 15.44008868035555260, 19.73035201082150536, 9.422509992056143702 ) ) ;
#83892 = ORIENTED_EDGE ( 'NONE', *, *, #1615, .T. ) ;
#83893 = CARTESIAN_POINT ( 'NONE',  ( 12.91533473730993009, 36.60535201082151247, -10.88017736071109987 ) ) ;
#83894 = CARTESIAN_POINT ( 'NONE',  ( 16.40814093676323893, 50.79030133659708923, 11.09922568453595026 ) ) ;
#83895 = CARTESIAN_POINT ( 'NONE',  ( 15.44008868035555260, 49.73035201082150536, 9.422509992056143702 ) ) ;
#83896 = CARTESIAN_POINT ( 'NONE',  ( 10.00000000000000178, 54.31368534415484106, 10.88017736071110342 ) ) ;
#83897 = CIRCLE ( 'NONE', #40791, 14.49999999999999822 ) ;
#83898 = EDGE_LOOP ( 'NONE', ( #8062, #38774, #2879, #42567 ) ) ;
#83899 = CARTESIAN_POINT ( 'NONE',  ( 15.44008868035555793, 56.39701867748817676, -9.422509992056140149 ) ) ;
#83900 = CARTESIAN_POINT ( 'NONE',  ( 6.034747819232443078, -36.07388523689489546, 3.750000000000000000 ) ) ;
#83901 = ADVANCED_FACE ( 'NONE', ( #52690 ), #30176, .T. ) ;
#83902 = FACE_OUTER_BOUND ( 'NONE', #22176, .T. ) ;
#83903 = CARTESIAN_POINT ( 'NONE',  ( 13.79529636645031943, 50.34541550158064638, -14.16423886937409904 ) ) ;
#83904 = CARTESIAN_POINT ( 'NONE',  ( 10.00000000000000178, 69.31368534415484817, 10.88017736071110342 ) ) ;
#83905 = FILL_AREA_STYLE ('',( #90400 ) ) ;
#83906 = CARTESIAN_POINT ( 'NONE',  ( -4.139423687100487470, -8.271184049145455575, -4.000000000000000000 ) ) ;
#83907 = CARTESIAN_POINT ( 'NONE',  ( 12.63842701281683034, 62.46726448433410894, 9.846743663894596210 ) ) ;
#83908 = DIRECTION ( 'NONE',  ( -5.240252676230738871E-14, 0.000000000000000000, 1.000000000000000000 ) ) ;
#83909 = CARTESIAN_POINT ( 'NONE',  ( 1.472469842513823179, 36.42559781766745175, 4.923371831947296329 ) ) ;
#83910 = VERTEX_POINT ( 'NONE', #82697 ) ;
#83911 = CARTESIAN_POINT ( 'NONE',  ( 18.52753015748617571, 33.09226448433411605, 4.923371831947298993 ) ) ;
#83912 = CARTESIAN_POINT ( 'NONE',  ( -11.09922568453594316, -0.4596986634029104346, 6.408140936763246920 ) ) ;
#83913 = CARTESIAN_POINT ( 'NONE',  ( 17.96484262340118221, 31.18868534415483751, -7.964842623401177768 ) ) ;
#83914 = CARTESIAN_POINT ( 'NONE',  ( 18.52753015748617571, 43.09226448433412315, 4.923371831947298993 ) ) ;
#83915 = CARTESIAN_POINT ( 'NONE',  ( -0.8801773607111009756, 68.06368534415484817, 1.068504757029289695E-15 ) ) ;
#83917 = CARTESIAN_POINT ( 'NONE',  ( 20.88017736071110519, 5.563685344154837509, 2.639326808657452039E-16 ) ) ;
#83916 = CARTESIAN_POINT ( 'NONE',  ( 19.42250999205614193, 50.14701867748817676, 5.440088680355555262 ) ) ;
#83918 = CARTESIAN_POINT ( 'NONE',  ( 20.36894250292379738, 54.92874883491396076, -10.36894250292379027 ) ) ;
#83919 = CIRCLE ( 'NONE', #96717, 0.2500000000000002220 ) ;
#83920 = CARTESIAN_POINT ( 'NONE',  ( -1.099225684535947600, 28.70696800326375353, -6.408140936763238038 ) ) ;
#83921 = CARTESIAN_POINT ( 'NONE',  ( 2.897438467171757030E-16, 23.03999999999999915, 0.000000000000000000 ) ) ;
#83922 = ORIENTED_EDGE ( 'NONE', *, *, #66971, .F. ) ;
#83923 = CARTESIAN_POINT ( 'NONE',  ( -2.816281873526473856, 9.331968003263753531, 3.434112377981055619 ) ) ;
#83924 = CARTESIAN_POINT ( 'NONE',  ( 0.5774900079438590739, 22.64701867748817321, -5.440088680355550821 ) ) ;
#83925 = CARTESIAN_POINT ( 'NONE',  ( 4.559911319644449179, 53.89701867748817676, 9.422509992056141925 ) ) ;
#83926 = EDGE_LOOP ( 'NONE', ( #328, #56695, #88684, #84517 ) ) ;
#83927 = EDGE_CURVE ( 'NONE', #94683, #31369, #91427, .T. ) ;
#83928 = CARTESIAN_POINT ( 'NONE',  ( -0.8801773607111008646, 53.27201867748816966, 2.915334737309923430 ) ) ;
#83929 = CARTESIAN_POINT ( 'NONE',  ( 5.076628168052704559, 55.17559781766745175, -8.527530157486179263 ) ) ;
#83930 = CARTESIAN_POINT ( 'NONE',  ( 17.20831665107776587, 29.13393115100078390, -7.208316651077762316 ) ) ;
#83931 = CARTESIAN_POINT ( 'NONE',  ( 0.1532563361054100626, 30.80059781766744820, -2.638427012816831230 ) ) ;
#83932 = DIRECTION ( 'NONE',  ( 0.000000000000000000, 0.000000000000000000, 1.000000000000000000 ) ) ;
#83933 = VECTOR ( 'NONE', #82227, 1000.000000000000114 ) ;
#83935 = CARTESIAN_POINT ( 'NONE',  ( -2.816281873526473856, 34.33196800326376064, 3.434112377981055619 ) ) ;
#83934 = CYLINDRICAL_SURFACE ( 'NONE', #69183, 0.1000000000000001166 ) ;
#83936 = ADVANCED_FACE ( 'NONE', ( #38685 ), #60190, .F. ) ;
#83938 = DIRECTION ( 'NONE',  ( -0.000000000000000000, -0.000000000000000000, -1.000000000000000000 ) ) ;
#83937 = CARTESIAN_POINT ( 'NONE',  ( 19.84674366389459621, 18.50893115100078745, 7.409399052514197653E-17 ) ) ;
#83939 = FACE_OUTER_BOUND ( 'NONE', #8301, .T. ) ;
#83941 = ORIENTED_EDGE ( 'NONE', *, *, #65715, .F. ) ;
#83940 = CARTESIAN_POINT ( 'NONE',  ( 17.20831665107776587, 39.13393115100079456, -7.208316651077762316 ) ) ;
#83942 = CARTESIAN_POINT ( 'NONE',  ( 22.81628187352648496, 61.83196800326376774, -3.434112377981050290 ) ) ;
#83943 = CARTESIAN_POINT ( 'NONE',  ( 11.42945456197617915, 15.00000000000000711, -9.127207413380702405 ) ) ;
#83944 = CARTESIAN_POINT ( 'NONE',  ( 13.43411237798106583, 17.66530133659708923, -12.81628187352647252 ) ) ;
#83945 = CIRCLE ( 'NONE', #40843, 14.49999999999999822 ) ;
#83946 = CARTESIAN_POINT ( 'NONE',  ( -0.8801773607111008646, 53.27201867748816966, 2.915334737309923430 ) ) ;
#83947 = CARTESIAN_POINT ( 'NONE',  ( -4.164238869374098151, 31.59541550158063927, -3.795296366450310543 ) ) ;
#83948 = CARTESIAN_POINT ( 'NONE',  ( 11.42945456197613119, 1.694065894508600678E-16, 9.127207413380800105 ) ) ;
#83949 = CARTESIAN_POINT ( 'NONE',  ( 6.204703633549690345, 27.84541550158063217, 14.16423886937410082 ) ) ;
#83950 = CARTESIAN_POINT ( 'NONE',  ( 2.917880565312948704, 57.63708216824731068, 12.26659068614894643 ) ) ;
#83951 = CARTESIAN_POINT ( 'NONE',  ( 10.00000000000000178, 13.05374883491396787, 14.16423886937410082 ) ) ;
#83953 = DIRECTION ( 'NONE',  ( -1.000000000000000000, 0.000000000000000000, 0.000000000000000000 ) ) ;
#83952 = CARTESIAN_POINT ( 'NONE',  ( 24.16423886937410614, 29.30374883491396787, 8.672049930838204340E-16 ) ) ;
#83954 = CARTESIAN_POINT ( 'NONE',  ( 4.559911319644449179, 48.89701867748817676, 9.422509992056141925 ) ) ;
#83955 = CARTESIAN_POINT ( 'NONE',  ( 6.673414917871782315, -55.62670566514463388, -2.750000000000000000 ) ) ;
#83957 = CARTESIAN_POINT ( 'NONE',  ( 1.472469842513823179, 45.59226448433412315, -4.923371831947296329 ) ) ;
#83956 = CARTESIAN_POINT ( 'NONE',  ( 7.084665262690076126, 64.10535201082150536, 10.88017736071109987 ) ) ;
#83958 = CARTESIAN_POINT ( 'NONE',  ( 19.42250999205614548, 25.98035201082150891, -5.440088680355545492 ) ) ;
#83959 = DIRECTION ( 'NONE',  ( -0.5372996083468194461, 0.000000000000000000, -0.8433914458128884961 ) ) ;
#83960 = CARTESIAN_POINT ( 'NONE',  ( 5.076628168052704559, 60.17559781766745175, -8.527530157486179263 ) ) ;
#83961 = CARTESIAN_POINT ( 'NONE',  ( 14.37564666802075131, -2.797749824780953231E-15, -2.692451322017675786 ) ) ;
#83962 = CARTESIAN_POINT ( 'NONE',  ( 6.565887622018943937, 58.08196800326376064, -12.81628187352647608 ) ) ;
#83964 = PRESENTATION_LAYER_ASSIGNMENT (  '', '', ( #20080 ) ) ;
#83963 = CARTESIAN_POINT ( 'NONE',  ( 3.795296366450314540, -6.737917831752698206, 14.16423886937410082 ) ) ;
#83965 = CARTESIAN_POINT ( 'NONE',  ( 17.20831665107776587, 44.13393115100078745, -7.208316651077762316 ) ) ;
#83966 = CARTESIAN_POINT ( 'NONE',  ( 5.076628168052703671, 51.84226448433412315, 8.527530157486179263 ) ) ;
#83967 = CIRCLE ( 'NONE', #61607, 14.49999999999999822 ) ;
#83968 = VECTOR ( 'NONE', #97875, 1000.000000000000000 ) ;
#83969 = CARTESIAN_POINT ( 'NONE',  ( 24.16423886937410614, 34.51208216824731068, -3.795296366450302550 ) ) ;
#83970 = EDGE_LOOP ( 'NONE', ( #66295, #76086, #71640, #81797 ) ) ;
#83971 = CARTESIAN_POINT ( 'NONE',  ( 6.204703633549690345, 17.84541550158063217, 14.16423886937410082 ) ) ;
#83972 = AXIS2_PLACEMENT_3D ( 'NONE', #35914, #96943, #66411 ) ;
#83973 = CARTESIAN_POINT ( 'NONE',  ( 12.91533473730993009, 66.60535201082150536, -10.88017736071109987 ) ) ;
#83974 = SURFACE_STYLE_FILL_AREA ( #47442 ) ;
#83975 = CARTESIAN_POINT ( 'NONE',  ( 2.917880565312948704, 57.63708216824731068, 12.26659068614894643 ) ) ;
#83976 = CARTESIAN_POINT ( 'NONE',  ( -2.816281873526471635, 13.91530133659708746, -3.434112377981056508 ) ) ;
#83977 = CARTESIAN_POINT ( 'NONE',  ( 2.863771337576428433, 14.95037103301162063, 14.47259902956231770 ) ) ;
#83978 = CARTESIAN_POINT ( 'NONE',  ( 0.1532563361054082862, 1.217264484334117824, 2.638427012816831674 ) ) ;
#83979 = DIRECTION ( 'NONE',  ( -0.000000000000000000, 1.000000000000000000, -0.000000000000000000 ) ) ;
#83980 = DIRECTION ( 'NONE',  ( 0.000000000000000000, 1.000000000000000000, 0.000000000000000000 ) ) ;
#83981 = CARTESIAN_POINT ( 'NONE',  ( -1.099225684535947600, 33.70696800326375353, -6.408140936763238038 ) ) ;
#83982 = CARTESIAN_POINT ( 'NONE',  ( -0.8801773607110991993, 2.855352010821504471, -2.915334737309923874 ) ) ;
#83983 = CARTESIAN_POINT ( 'NONE',  ( -9.422509992056136596, 28.48035201082149825, 5.440088680355559703 ) ) ;
#83984 = CARTESIAN_POINT ( 'NONE',  ( 4.559911319644449179, 13.89701867748817143, 9.422509992056141925 ) ) ;
#83985 = CARTESIAN_POINT ( 'NONE',  ( 2.035157376598822676, 27.43868534415483396, -7.964842623401177768 ) ) ;
#83986 = CARTESIAN_POINT ( 'NONE',  ( 10.00000000000000000, 59.75893115100078745, -9.846743663894594434 ) ) ;
#83987 = CARTESIAN_POINT ( 'NONE',  ( 17.20831665107776587, 47.88393115100078745, 7.208316651077764980 ) ) ;
#83988 = CARTESIAN_POINT ( 'NONE',  ( 6.565887622018943937, 48.08196800326375353, -12.81628187352647608 ) ) ;
#83989 = CARTESIAN_POINT ( 'NONE',  ( 0.1532563361054083140, 1.008931151000784787, 1.131784320476157264E-15 ) ) ;
#83990 = VERTEX_POINT ( 'NONE', #62144 ) ;
#83991 = CARTESIAN_POINT ( 'NONE',  ( -0.8801773607111009756, 13.06368534415483929, 1.068504757029289695E-15 ) ) ;
#83992 = ADVANCED_FACE ( 'NONE', ( #77647 ), #59597, .T. ) ;
#83993 = CARTESIAN_POINT ( 'NONE',  ( 10.00000000000000178, 20.37363466993042138, 12.81628187352647608 ) ) ;
#83994 = CARTESIAN_POINT ( 'NONE',  ( 19.80832241502127289, 39.75868815902069997, 6.499999999999984901 ) ) ;
#83995 = AXIS2_PLACEMENT_3D ( 'NONE', #21132, #51632, #82112 ) ;
#83996 = CARTESIAN_POINT ( 'NONE',  ( 2.791683348922240793, 46.63393115100077324, 7.208316651077764092 ) ) ;
#83997 = ADVANCED_FACE ( 'NONE', ( #1197 ), #24519, .T. ) ;
#83998 = CARTESIAN_POINT ( 'NONE',  ( 2.035157376598824452, 53.68868534415484817, 7.964842623401179544 ) ) ;
#83999 = CARTESIAN_POINT ( 'NONE',  ( -1.099225684535947600, 23.70696800326375708, -6.408140936763238038 ) ) ;
#84001 = CARTESIAN_POINT ( 'NONE',  ( 64.56412365047461321, 44.99999999999998579, 0.000000000000000000 ) ) ;
#84000 = CARTESIAN_POINT ( 'NONE',  ( 0.5774900079438607392, 53.48035201082151247, 5.440088680355550821 ) ) ;
#84002 = CARTESIAN_POINT ( 'NONE',  ( 0.000000000000000000, 15.00000000000000000, 14.25000000000000000 ) ) ;
#84003 = CARTESIAN_POINT ( 'NONE',  ( 10.00000000000000178, 55.37363466993042493, 12.81628187352647608 ) ) ;
#84004 = ORIENTED_EDGE ( 'NONE', *, *, #49763, .F. ) ;
#84005 = CARTESIAN_POINT ( 'NONE',  ( 18.52753015748617571, 58.09226448433411605, 4.923371831947298993 ) ) ;
#84006 = CARTESIAN_POINT ( 'NONE',  ( -0.1503990784575328643, 70.00000000000000000, -6.262539305110068177 ) ) ;
#84007 = CARTESIAN_POINT ( 'NONE',  ( 4.559911319644449179, 52.23035201082151247, -9.422509992056141925 ) ) ;
#84009 = CARTESIAN_POINT ( 'NONE',  ( -0.3689425029237898834, 11.17874883491396787, -10.36894250292378850 ) ) ;
#84008 = CARTESIAN_POINT ( 'NONE',  ( 19.38216949554541557, 47.24863466993041783, -9.382169495545420901 ) ) ;
#84010 = CARTESIAN_POINT ( 'NONE',  ( 1.472469842513823179, 6.425597817667451750, 4.923371831947296329 ) ) ;
#84011 = CARTESIAN_POINT ( 'NONE',  ( -6.349999999999995204, -97.00000000000000000, 3.750000000000000000 ) ) ;
#84012 = CARTESIAN_POINT ( 'NONE',  ( 5.076628168052703671, 11.84226448433411960, 8.527530157486179263 ) ) ;
#84013 = CARTESIAN_POINT ( 'NONE',  ( 5.076628168052703671, 6.842264484334118713, 8.527530157486179263 ) ) ;
#84014 = B_SPLINE_CURVE_WITH_KNOTS ( 'NONE', 3,
 ( #8563, #83577, #60067, #53555, #84072, #14095 ),
 .UNSPECIFIED., .F., .F.,
 ( 4, 2, 4 ),
 ( 0.000000000000000000, 0.0002565770811490952221, 0.0005131541622981904442 ),
 .UNSPECIFIED. ) ;
#84015 = DIRECTION ( 'NONE',  ( 0.9981347984218670311, 0.000000000000000000, -0.06104853953485662316 ) ) ;
#84016 = CARTESIAN_POINT ( 'NONE',  ( -4.164238869374099039, 41.80374883491397497, 8.674139862899312516E-16 ) ) ;
#84017 = VECTOR ( 'NONE', #67147, 999.9999999999998863 ) ;
#84018 = CARTESIAN_POINT ( 'NONE',  ( 1.046131998950050379, 55.73810908735726599, 6.499999999999992006 ) ) ;
#84019 = CARTESIAN_POINT ( 'NONE',  ( 4.559911319644449179, 13.89701867748817143, 9.422509992056141925 ) ) ;
#84020 = LINE ( 'NONE', #31000, #37651 ) ;
#84021 = ORIENTED_EDGE ( 'NONE', *, *, #95734, .F. ) ;
#84022 = CARTESIAN_POINT ( 'NONE',  ( 12.91533473730992121, 14.52201867748817143, 10.88017736071110164 ) ) ;
#84023 = CARTESIAN_POINT ( 'NONE',  ( 17.96484262340118221, 4.938685344154837509, 7.964842623401181321 ) ) ;
#84024 = CARTESIAN_POINT ( 'NONE',  ( 7.361572987183169658, 44.96726448433412315, -9.846743663894592657 ) ) ;
#84025 = EDGE_CURVE ( 'NONE', #61288, #14585, #62808, .T. ) ;
#84026 = CARTESIAN_POINT ( 'NONE',  ( 0.6178305044545838731, 34.74863466993042493, 9.382169495545420901 ) ) ;
#84027 =( NAMED_UNIT ( * ) SI_UNIT ( $, .STERADIAN. ) SOLID_ANGLE_UNIT ( ) );
#84029 = CARTESIAN_POINT ( 'NONE',  ( 24.16423886937410614, 9.512082168247301794, -3.795296366450302550 ) ) ;
#84028 = DIRECTION ( 'NONE',  ( 0.000000000000000000, 0.000000000000000000, 1.000000000000000000 ) ) ;
#84030 = CARTESIAN_POINT ( 'NONE',  ( 17.96484262340118221, 21.18868534415483396, -7.964842623401177768 ) ) ;
#84031 = CARTESIAN_POINT ( 'NONE',  ( 0.5774900079438590739, 2.647018677488171434, -5.440088680355550821 ) ) ;
#84032 = CARTESIAN_POINT ( 'NONE',  ( 0.1532563361054100626, 35.80059781766745175, -2.638427012816831230 ) ) ;
#84033 = CARTESIAN_POINT ( 'NONE',  ( 66.76470751278411342, 40.99999999999997868, 10.00000000000000000 ) ) ;
#84034 = CARTESIAN_POINT ( 'NONE',  ( 0.1532563361054082862, 21.21726448433412315, 2.638427012816831674 ) ) ;
#84035 = EDGE_CURVE ( 'NONE', #14939, #69916, #2677, .T. ) ;
#84036 = CARTESIAN_POINT ( 'NONE',  ( -4.923371831947292776, 31.84226448433413736, 8.527530157486181039 ) ) ;
#84037 = ORIENTED_EDGE ( 'NONE', *, *, #79922, .F. ) ;
#84038 = DIRECTION ( 'NONE',  ( 0.000000000000000000, 1.000000000000000000, 0.000000000000000000 ) ) ;
#84039 = ORIENTED_EDGE ( 'NONE', *, *, #62192, .T. ) ;
#84040 = CARTESIAN_POINT ( 'NONE',  ( 5.076628168052704559, 55.17559781766745175, -8.527530157486179263 ) ) ;
#84042 = CARTESIAN_POINT ( 'NONE',  ( 15.44008868035555260, 39.73035201082150536, 9.422509992056143702 ) ) ;
#84041 = CARTESIAN_POINT ( 'NONE',  ( 0.5774900079438607392, 28.48035201082150891, 5.440088680355550821 ) ) ;
#84044 = CARTESIAN_POINT ( 'NONE',  ( -1.099225684535947600, 24.54030133659708923, 6.408140936763237150 ) ) ;
#84043 = PRESENTATION_STYLE_ASSIGNMENT (( #75052 ) ) ;
#84045 = AXIS2_PLACEMENT_3D ( 'NONE', #70204, #61695, #63171 ) ;
#84046 = CARTESIAN_POINT ( 'NONE',  ( 17.08211943468705840, 15.13708216824730179, -12.26659068614894466 ) ) ;
#84047 = AXIS2_PLACEMENT_3D ( 'NONE', #66420, #11948, #42452 ) ;
#84048 = VECTOR ( 'NONE', #98821, 1000.000000000000000 ) ;
#84050 = CARTESIAN_POINT ( 'NONE',  ( 6.565887622018943937, 50.16530133659708213, 12.81628187352647430 ) ) ;
#84049 = COLOUR_RGB ( '', 0.31764706, 0.68627451, 0.89019608) ;
#84051 = EDGE_LOOP ( 'NONE', ( #82181, #23855, #28678, #74068 ) ) ;
#84052 = CARTESIAN_POINT ( 'NONE',  ( 19.84674366389459266, 38.30059781766745175, 2.638427012816836559 ) ) ;
#84053 = CARTESIAN_POINT ( 'NONE',  ( 17.96484262340118221, 9.938685344154839285, 7.964842623401181321 ) ) ;
#84054 = ORIENTED_EDGE ( 'NONE', *, *, #9865, .F. ) ;
#84055 = CARTESIAN_POINT ( 'NONE',  ( 4.559911319644449179, 22.23035201082150536, -9.422509992056141925 ) ) ;
#84056 = VERTEX_POINT ( 'NONE', #48135 ) ;
#84057 = CARTESIAN_POINT ( 'NONE',  ( 17.96484262340118221, 59.93868534415484106, 7.964842623401181321 ) ) ;
#84058 = CARTESIAN_POINT ( 'NONE',  ( 19.42250999205614193, 60.14701867748817676, 5.440088680355555262 ) ) ;
#84059 = CARTESIAN_POINT ( 'NONE',  ( 0.5774900079438607392, 58.48035201082151247, 5.440088680355550821 ) ) ;
#84060 = DIRECTION ( 'NONE',  ( 0.000000000000000000, 0.000000000000000000, 1.000000000000000000 ) ) ;
#84061 = CARTESIAN_POINT ( 'NONE',  ( 2.035157376598822676, 57.43868534415484106, -7.964842623401177768 ) ) ;
#84062 = CARTESIAN_POINT ( 'NONE',  ( -0.2418659066527716062, 52.23410085661203794, -6.114288769123046308 ) ) ;
#84063 = EDGE_CURVE ( 'NONE', #45054, #52174, #16516, .T. ) ;
#84065 = CARTESIAN_POINT ( 'NONE',  ( -46.94000000000001194, 101.2919103424992358, 7.700697297268528807 ) ) ;
#84064 = CIRCLE ( 'NONE', #56927, 0.5000000000000004441 ) ;
#84067 = ORIENTED_EDGE ( 'NONE', *, *, #20131, .F. ) ;
#84066 = CARTESIAN_POINT ( 'NONE',  ( 10.47195283030799651, -40.28639508432959815, 4.000000000000001776 ) ) ;
#84068 = PRESENTATION_LAYER_ASSIGNMENT (  '', '', ( #80921 ) ) ;
#84069 = AXIS2_PLACEMENT_3D ( 'NONE', #46805, #73106, #72615 ) ;
#84070 = CARTESIAN_POINT ( 'NONE',  ( 17.20831665107776587, 37.88393115100078745, 7.208316651077764980 ) ) ;
#84071 = EDGE_LOOP ( 'NONE', ( #55562, #39584, #74036, #34104, #46156, #32238 ) ) ;
#84072 = CARTESIAN_POINT ( 'NONE',  ( 20.10493008474206533, 19.71697413083879269, 6.336235997365759154 ) ) ;
#84073 = CARTESIAN_POINT ( 'NONE',  ( 20.36894250292379382, 18.67874883491397142, 10.36894250292379205 ) ) ;
#84074 = LINE ( 'NONE', #46074, #10664 ) ;
#84076 = CARTESIAN_POINT ( 'NONE',  ( 12.91533473730992121, 64.52201867748817676, 10.88017736071110164 ) ) ;
#84075 = LINE ( 'NONE', #53561, #84914 ) ;
#84077 = CARTESIAN_POINT ( 'NONE',  ( 4.559911319644449179, 3.897018677488171434, 9.422509992056141925 ) ) ;
#84078 = CARTESIAN_POINT ( 'NONE',  ( -8.209432707284690878, 0.5000000000000004441, -12.55409154915497183 ) ) ;
#84080 = VERTEX_POINT ( 'NONE', #17173 ) ;
#84079 = CARTESIAN_POINT ( 'NONE',  ( 0.6178305044545838731, 39.74863466993041072, 9.382169495545420901 ) ) ;
#84081 = CARTESIAN_POINT ( 'NONE',  ( 19.72487221294571924, 62.80223176428831522, -6.499999999999984901 ) ) ;
#84082 = CARTESIAN_POINT ( 'NONE',  ( 2.791683348922240793, 1.633931151000784565, 7.208316651077764092 ) ) ;
#84083 = CARTESIAN_POINT ( 'NONE',  ( -2.816281873526471635, 33.91530133659708213, -3.434112377981056508 ) ) ;
#84084 = CARTESIAN_POINT ( 'NONE',  ( 12.63842701281683034, 17.46726448433411250, 9.846743663894596210 ) ) ;
#84085 = FACE_OUTER_BOUND ( 'NONE', #64973, .T. ) ;
#84086 = CARTESIAN_POINT ( 'NONE',  ( 5.076628168052703671, 16.84226448433411960, 8.527530157486179263 ) ) ;
#84087 = CARTESIAN_POINT ( 'NONE',  ( 21.09922568453594849, 16.20696800326375353, 6.408140936763242479 ) ) ;
#84088 = CARTESIAN_POINT ( 'NONE',  ( 19.89103541497709315, 40.66234555792571825, -6.479102184480824533 ) ) ;
#84089 = CIRCLE ( 'NONE', #98539, 2.999999999999997780 ) ;
#84090 = CARTESIAN_POINT ( 'NONE',  ( 12.63842701281683922, 4.550597817667451750, -9.846743663894590881 ) ) ;
#84091 = ORIENTED_EDGE ( 'NONE', *, *, #52539, .T. ) ;
#84092 = EDGE_LOOP ( 'NONE', ( #88569, #77988, #67679, #67564, #37755, #47532 ) ) ;
#84093 = CARTESIAN_POINT ( 'NONE',  ( 10.00000000000000000, 26.81368534415484106, -10.88017736071110342 ) ) ;
#84094 = CARTESIAN_POINT ( 'NONE',  ( 13.79529636645030344, 18.26208216824730002, 14.16423886937410614 ) ) ;
#84095 = CARTESIAN_POINT ( 'NONE',  ( 19.84674366389459621, 38.50893115100078745, 7.409399052514197653E-17 ) ) ;
#84096 = ADVANCED_FACE ( 'NONE', ( #10640 ), #39437, .F. ) ;
#84097 = CARTESIAN_POINT ( 'NONE',  ( 2.035157376598822676, 62.43868534415483396, -7.964842623401177768 ) ) ;
#84099 = DIRECTION ( 'NONE',  ( 0.000000000000000000, 0.000000000000000000, 1.000000000000000000 ) ) ;
#84098 = CARTESIAN_POINT ( 'NONE',  ( 19.38216949554541202, 45.99863466993041072, 9.382169495545424454 ) ) ;
#84100 = CARTESIAN_POINT ( 'NONE',  ( 15.44008868035555260, 9.730352010821505360, 9.422509992056143702 ) ) ;
#84101 = CARTESIAN_POINT ( 'NONE',  ( -14.29484424893239414, 0.2301500622783318739, -4.345072767107323486 ) ) ;
#84102 = CARTESIAN_POINT ( 'NONE',  ( 3.591859063236763294, 8.290301336597087456, -11.09922568453595026 ) ) ;
#84103 = CARTESIAN_POINT ( 'NONE',  ( -1.099225684535947600, 3.706968003263753531, -6.408140936763238038 ) ) ;
#84104 = CARTESIAN_POINT ( 'NONE',  ( 19.84674366389459621, 33.50893115100078745, 7.409399052514197653E-17 ) ) ;
#84105 = CARTESIAN_POINT ( 'NONE',  ( 9.422509992056141925, -9.852981322511819684, 5.440088680355547268 ) ) ;
#84106 = CARTESIAN_POINT ( 'NONE',  ( 10.00000000000000178, 35.37363466993042493, 12.81628187352647608 ) ) ;
#84107 = CARTESIAN_POINT ( 'NONE',  ( 13.50171220565087182, -3.186537947570676692E-15, -5.622479820943826034 ) ) ;
#84109 = CARTESIAN_POINT ( 'NONE',  ( 0.9408516040111470913, 62.46693863883975695, -6.499999999999953815 ) ) ;
#84108 = CARTESIAN_POINT ( 'NONE',  ( 12.91533473730993009, 56.60535201082151247, -10.88017736071109987 ) ) ;
#84110 = DIRECTION ( 'NONE',  ( 0.3665012267243071276, 0.000000000000000000, -0.9304175679820205769 ) ) ;
#84111 = AXIS2_PLACEMENT_3D ( 'NONE', #87758, #19273, #35249 ) ;
#84112 = CARTESIAN_POINT ( 'NONE',  ( -14.97687855664615064, 14.49999999999999112, 0.8325315005899805998 ) ) ;
#84113 =( BOUNDED_CURVE ( )  B_SPLINE_CURVE ( 2, ( #22593, #37593, #52577, #14608, #76068, #83081, #38575, #16068, #60071 ),
 .UNSPECIFIED., .F., .F. ) 
 B_SPLINE_CURVE_WITH_KNOTS ( ( 3, 2, 2, 2, 3 ),
 ( 0.8687123655116599785, 0.8690476190476190688, 0.8750000000000000000, 0.8809523809523809312, 0.8812876344883400215 ),
 .UNSPECIFIED. ) 
 CURVE ( )  GEOMETRIC_REPRESENTATION_ITEM ( )  RATIONAL_B_SPLINE_CURVE ( ( 0.9963778908391764944, 0.9980808541467923733, 1.000000000000000000, 0.9659258262890682012, 1.000000000000000000, 0.9659258262890682012, 1.000000000000000000, 0.9980808541467922623, 0.9963778908391764944 ) ) 
 REPRESENTATION_ITEM ( '' )  );
#84114 = CARTESIAN_POINT ( 'NONE',  ( 15.44008868035555793, 36.39701867748816966, -9.422509992056140149 ) ) ;
#84115 = CARTESIAN_POINT ( 'NONE',  ( 15.44008868035555793, 46.39701867748817676, -9.422509992056140149 ) ) ;
#84116 = DIRECTION ( 'NONE',  ( -0.000000000000000000, -0.000000000000000000, -1.000000000000000000 ) ) ;
#84117 = CARTESIAN_POINT ( 'NONE',  ( -0.8801773607111008646, 68.27201867748817676, 2.915334737309923430 ) ) ;
#84118 = EDGE_CURVE ( 'NONE', #3611, #89098, #81854, .T. ) ;
#84119 = AXIS2_PLACEMENT_3D ( 'NONE', #79138, #48144, #78158 ) ;
#84120 = EDGE_CURVE ( 'NONE', #68783, #89049, #93142, .T. ) ;
#84121 =( BOUNDED_SURFACE ( )  B_SPLINE_SURFACE ( 1, 2, ( 
 ( #88391, #19403, #3918, #65379, #89860, #81861, #5879, #66365, #74353, #27388, #57879, #36375, #96902, #19890, #41928, #89373, #66870, #28854, #14377, #60349, #83354, #6865, #23360, #76826, #21879, #67364, #14878, #44360, #82356, #7371, #90842, #83846, #37870, #52359, #45853, #31321, #68366, #45347, #82860, #75851, #61821, #13877, #44845, #75351, #37376, #29350, #84354, #53337, #59854, #98883, #862, #385, #92328, #30833, #30334, #52846, #74862, #6361, #36873, #8341, #51873, #91843, #38847, #60840, #15854, #67866, #97891, #53843, #76343, #22371, #90343, #91339, #22866, #68852, #98388, #15372, #7860, #29844, #46339, #69337, #38358, #61331, #55308, #16338, #54317, #78302, #62807, #55815, #9820, #92814, #17813, #3298, #40321, #17332, #24344, #85817, #33762, #84831, #54806, #85318, #47305, #1359, #56306, #25330, #31810, #70825, #71793, #71312, #64269, #2830, #2339, #24830, #46821, #77312, #8826, #48785, #62306, #32794, #63290, #86309, #93799, #48294, #69835, #39341, #78801, #10311, #10803, #79293, #23851, #16830, #47802, #77805, #40813, #33286, #63777, #32302, #86803, #9320, #93306, #39824, #94286, #70329, #18302, #1844, #25808, #41321, #56781, #50253, #13256, #81740, #95269, #57270, #96279, #65252, #58750, #42774, #26772, #27756, #88758, #50767, #5767, #80770, #34256, #5281, #12264, #87765, #73749, #89255, #72271, #58239, #87277, #19279, #64758, #20270, #65752, #81259, #35757, #11282, #49764, #49282, #72755, #18797, #80274, #66245, #4289, #79781, #41800, #11775, #51254, #3801, #73257, #88263, #12757, #57759, #42283, #4782, #43748, #43255, #27260, #19767, #35255, #96779, #28255, #36255, #20766, #26281, #74233, #94781, #34762, #95780, #29727, #52244, #45233, #15256, #36758, #52730, #37264, #82738, #90729, #59240, #68250, #14257, #74742, #84237, #30218, #97774, #91219, #67751, #67250, #7248, #45734, #60235, #22256, #46228, #23245, #60723, #29239, #22746, #53229, #51755, #83237, #98769, #28749, #53720, #6255, #89739, #66751, #30709, #97276, #44239, #37753, #75732, #83733, #59737, #90232, #21765, #14760, #68734, #15744, #44736, #98271, #76234, #7748, #76714, #21258, #38243, #8233, #82240, #75236, #263, #61221, #6746, #91725, #13753, #17706, #40693, #752, #9700, #47187, #39225, #92214, #56190, #86194, #9205, #46704, #54202, #32183, #38727, #31697, #62188, #55697, #17217, #71194, #92698, #31204, #2717, #48176, #1728, #47695, #25700, #8709, #79170, #77691, #61699, #69227, #39718, #69714, #78688, #23740, #16222, #32682, #2222, #86684, #77204, #84718, #24222, #1241, #70209, #54688, #10199, #85210, #16715, #63175, #93683, #18188 ),
 ( #85700, #48669, #25216, #62685, #93186, #24712, #40196, #33171, #55183, #63664, #78187, #70703, #94169, #97042, #37010, #74007, #96539, #89514, #59501, #79670, #28517, #81508, #28014, #36013, #3189, #13517, #58511, #18682, #29480, #74500, #41686, #36519, #13013, #11167, #51513, #89999, #5533, #66515, #90482, #67506, #6023, #72156, #67011, #97532, #94668, #59011, #43998, #71679, #98026, #49168, #33655, #10685, #75000, #41199, #87157, #82005, #21024, #28991, #5034, #35520, #66012, #21515, #14019, #59989, #89020, #43510, #52012, #82501, #22019, #64150, #44499, #52493, #26178, #20529, #6502, #56669, #51014, #46957, #996, #61959, #84965, #44987, #53974, #91486, #83496, #37511, #1490, #31457, #53475, #90977, #98530, #76481, #83000, #75986, #7515, #92458, #61467, #16481, #38006, #75494, #77451, #23986, #45992, #91974, #69971, #52982, #24482, #23007, #7006, #22510, #23503, #84483, #15984, #46471, #76967, #29983, #68004, #8479, #38985, #31943, #39481, #62444, #14518, #83985, #60488, #69477, #15510, #7995, #38493, #8965, #68499, #68988, #15015, #54457, #92947, #45484, #26, #30473, #523, #60974, #30970, #72409, #41946, #55459, #17471, #56445, #25472, #18939, #2968, #85962, #86931, #48926, #10936, #64894, #10449, #93449, #64414, #40957, #47938, #33906, #49416, #32450, #18444, #47454, #78444, #24974, #79438, #25943, #41460, #94920, #70462, #9959, #9460, #32937, #77953, #40465, #26419, #63438, #39961, #1984, #70964, #34405, #56920, #79917, #86454, #87422, #2483, #62946, #11426, #71928, #93945, #95422, #71454, #94428, #3449, #55954, #17952, #48438, #78939, #3936, #54945, #33418, #63917, #85462, #16974, #57415, #81397, #65894, #58896, #12899, #95927, #20910, #6382, #43396, #20416, #27407, #88905, #36898, #87908, #57898, #88412, #50403, #4439, #59380, #28401, #34905, #73894, #74884, #74377, #67386, #5904, #5425, #27898, #19422, #49914, #80425, #51896, #35895, #66390, #89394, #96923, #51399, #72906, #11921, #81886, #13398, #13900, #82378, #26918, #42425, #58387, #65401, #43881, #50902, #36399, #35401, #89884, #80913, #96425, #19912, #66892, #12407, #21402, #42914, #97411, #28878, #73395, #44385, #4923, #84856, #98411, #60369, #408, #68386, #61846, #45880, #29867, #30860, #91866, #53869, #8851, #53363, #37401, #8365, #83870, #90866, #76851, #92352, #75373, #61357, #90365, #22396, #67889, #23384, #68878, #84379, #38873, #14399, #52872, #52379, #75875, #21902, #83378, #69364, #7396, #82883, #44870, #14900, #77339, #885, #23879, #30357, #31345, #45371, #6888, #54343, #15879, #37894, #39365, #15394, #38377, #46363, #98906, #60865, #91365 ) ),
 .UNSPECIFIED., .F., .F., .F. ) 
 B_SPLINE_SURFACE_WITH_KNOTS ( ( 2, 2 ),
 ( 3, 2, 2, 2, 2, 2, 2, 2, 2, 2, 2, 2, 2, 2, 2, 2, 2, 2, 2, 2, 2, 2, 2, 2, 2, 2, 2, 2, 2, 2, 2, 2, 2, 2, 2, 2, 2, 2, 2, 2, 2, 2, 2, 2, 2, 2, 2, 2, 2, 2, 2, 2, 2, 2, 2, 2, 2, 2, 2, 2, 2, 2, 2, 2, 2, 2, 2, 2, 2, 2, 2, 2, 2, 2, 2, 2, 2, 2, 2, 2, 2, 2, 2, 2, 2, 2, 2, 2, 2, 2, 2, 2, 2, 2, 2, 2, 2, 2, 2, 2, 2, 2, 2, 2, 2, 2, 2, 2, 2, 2, 2, 2, 2, 2, 2, 2, 2, 2, 2, 2, 2, 2, 2, 2, 2, 2, 2, 2, 2, 2, 2, 2, 2, 2, 2, 2, 2, 2, 2, 2, 2, 2, 2, 2, 2, 2, 2, 2, 2, 2, 2, 2, 2, 2, 2, 2, 2, 2, 2, 2, 2, 2, 3 ),
 ( 0.000000000000000000, 1.000000000000000000 ),
 ( 0.000000000000000000, 0.005952380952380952051, 0.01190476190476190410, 0.01785714285714285615, 0.02380952380952380820, 0.02976190476190476025, 0.03571428571428571230, 0.04166666666666666435, 0.04761904761904761640, 0.05357142857142856845, 0.05952380952380952051, 0.06547619047619047949, 0.07142857142857142461, 0.07738095238095238360, 0.08333333333333332871, 0.08928571428571428770, 0.09523809523809523281, 0.1011904761904761918, 0.1071428571428571369, 0.1130952380952380959, 0.1190476190476190410, 0.1250000000000000000, 0.1309523809523809590, 0.1369047619047619180, 0.1428571428571428492, 0.1488095238095238082, 0.1547619047619047672, 0.1607142857142857262, 0.1666666666666666574, 0.1726190476190476164, 0.1785714285714285754, 0.1845238095238095344, 0.1904761904761904656, 0.1964285714285714246, 0.2023809523809523836, 0.2083333333333333426, 0.2142857142857142738, 0.2202380952380952328, 0.2261904761904761918, 0.2321428571428571508, 0.2380952380952380820, 0.2440476190476190410, 0.2500000000000000000, 0.2559523809523809312, 0.2619047619047619180, 0.2678571428571428492, 0.2738095238095238360, 0.2797619047619047672, 0.2857142857142856984, 0.2916666666666666852, 0.2976190476190476164, 0.3035714285714285476, 0.3095238095238095344, 0.3154761904761904656, 0.3214285714285714524, 0.3273809523809523836, 0.3333333333333333148, 0.3392857142857143016, 0.3452380952380952328, 0.3511904761904761640, 0.3571428571428571508, 0.3630952380952380820, 0.3690476190476190688, 0.3750000000000000000, 0.3809523809523809312, 0.3869047619047619180, 0.3928571428571428492, 0.3988095238095238360, 0.4047619047619047672, 0.4107142857142856984, 0.4166666666666666852, 0.4226190476190476164, 0.4285714285714285476, 0.4345238095238095344, 0.4404761904761904656, 0.4464285714285714524, 0.4523809523809523836, 0.4583333333333333148, 0.4642857142857143016, 0.4702380952380952328, 0.4761904761904761640, 0.4821428571428571508, 0.4880952380952380820, 0.4940476190476190688, 0.5000000000000000000, 0.5059523809523809312, 0.5119047619047618625, 0.5178571428571429047, 0.5238095238095238360, 0.5297619047619047672, 0.5357142857142856984, 0.5416666666666666297, 0.5476190476190476719, 0.5535714285714286031, 0.5595238095238095344, 0.5654761904761904656, 0.5714285714285713969, 0.5773809523809523281, 0.5833333333333333703, 0.5892857142857143016, 0.5952380952380952328, 0.6011904761904761640, 0.6071428571428570953, 0.6130952380952381375, 0.6190476190476190688, 0.6250000000000000000, 0.6309523809523809312, 0.6369047619047618625, 0.6428571428571429047, 0.6488095238095238360, 0.6547619047619047672, 0.6607142857142856984, 0.6666666666666666297, 0.6726190476190476719, 0.6785714285714286031, 0.6845238095238095344, 0.6904761904761904656, 0.6964285714285713969, 0.7023809523809523281, 0.7083333333333333703, 0.7142857142857143016, 0.7202380952380952328, 0.7261904761904761640, 0.7321428571428570953, 0.7380952380952381375, 0.7440476190476190688, 0.7500000000000000000, 0.7559523809523809312, 0.7619047619047618625, 0.7678571428571429047, 0.7738095238095238360, 0.7797619047619047672, 0.7857142857142856984, 0.7916666666666666297, 0.7976190476190476719, 0.8035714285714286031, 0.8095238095238095344, 0.8154761904761904656, 0.8214285714285713969, 0.8273809523809523281, 0.8333333333333333703, 0.8392857142857143016, 0.8452380952380952328, 0.8511904761904761640, 0.8571428571428570953, 0.8630952380952381375, 0.8690476190476190688, 0.8750000000000000000, 0.8809523809523809312, 0.8869047619047618625, 0.8928571428571429047, 0.8988095238095238360, 0.9047619047619047672, 0.9107142857142856984, 0.9166666666666666297, 0.9226190476190476719, 0.9285714285714286031, 0.9345238095238095344, 0.9404761904761904656, 0.9464285714285713969, 0.9523809523809523281, 0.9583333333333333703, 0.9642857142857143016 ),
 .UNSPECIFIED. ) 
 GEOMETRIC_REPRESENTATION_ITEM ( )  RATIONAL_B_SPLINE_SURFACE ( (
 ( 1.000000000000000000, 0.9659258262890683122, 1.000000000000000000, 0.9659258262890683122, 1.000000000000000000, 0.9659258262890683122, 1.000000000000000000, 0.9659258262890683122, 1.000000000000000000, 0.9659258262890683122, 1.000000000000000000, 0.9659258262890683122, 1.000000000000000000, 0.9659258262890683122, 1.000000000000000000, 0.9659258262890683122, 1.000000000000000000, 0.9659258262890683122, 1.000000000000000000, 0.9659258262890683122, 1.000000000000000000, 0.9659258262890683122, 1.000000000000000000, 0.9659258262890683122, 1.000000000000000000, 0.9659258262890683122, 1.000000000000000000, 0.9659258262890683122, 1.000000000000000000, 0.9659258262890683122, 1.000000000000000000, 0.9659258262890683122, 1.000000000000000000, 0.9659258262890683122, 1.000000000000000000, 0.9659258262890683122, 1.000000000000000000, 0.9659258262890683122, 1.000000000000000000, 0.9659258262890683122, 1.000000000000000000, 0.9659258262890683122, 1.000000000000000000, 0.9659258262890683122, 1.000000000000000000, 0.9659258262890683122, 1.000000000000000000, 0.9659258262890683122, 1.000000000000000000, 0.9659258262890683122, 1.000000000000000000, 0.9659258262890683122, 1.000000000000000000, 0.9659258262890683122, 1.000000000000000000, 0.9659258262890683122, 1.000000000000000000, 0.9659258262890683122, 1.000000000000000000, 0.9659258262890683122, 1.000000000000000000, 0.9659258262890683122, 1.000000000000000000, 0.9659258262890683122, 1.000000000000000000, 0.9659258262890683122, 1.000000000000000000, 0.9659258262890683122, 1.000000000000000000, 0.9659258262890683122, 1.000000000000000000, 0.9659258262890683122, 1.000000000000000000, 0.9659258262890683122, 1.000000000000000000, 0.9659258262890683122, 1.000000000000000000, 0.9659258262890683122, 1.000000000000000000, 0.9659258262890683122, 1.000000000000000000, 0.9659258262890683122, 1.000000000000000000, 0.9659258262890683122, 1.000000000000000000, 0.9659258262890683122, 1.000000000000000000, 0.9659258262890683122, 1.000000000000000000, 0.9659258262890683122, 1.000000000000000000, 0.9659258262890683122, 1.000000000000000000, 0.9659258262890683122, 1.000000000000000000, 0.9659258262890683122, 1.000000000000000000, 0.9659258262890683122, 1.000000000000000000, 0.9659258262890683122, 1.000000000000000000, 0.9659258262890683122, 1.000000000000000000, 0.9659258262890683122, 1.000000000000000000, 0.9659258262890683122, 1.000000000000000000, 0.9659258262890683122, 1.000000000000000000, 0.9659258262890683122, 1.000000000000000000, 0.9659258262890683122, 1.000000000000000000, 0.9659258262890683122, 1.000000000000000000, 0.9659258262890683122, 1.000000000000000000, 0.9659258262890683122, 1.000000000000000000, 0.9659258262890683122, 1.000000000000000000, 0.9659258262890683122, 1.000000000000000000, 0.9659258262890683122, 1.000000000000000000, 0.9659258262890683122, 1.000000000000000000, 0.9659258262890683122, 1.000000000000000000, 0.9659258262890683122, 1.000000000000000000, 0.9659258262890683122, 1.000000000000000000, 0.9659258262890683122, 1.000000000000000000, 0.9659258262890683122, 1.000000000000000000, 0.9659258262890683122, 1.000000000000000000, 0.9659258262890683122, 1.000000000000000000, 0.9659258262890683122, 1.000000000000000000, 0.9659258262890683122, 1.000000000000000000, 0.9659258262890683122, 1.000000000000000000, 0.9659258262890683122, 1.000000000000000000, 0.9659258262890683122, 1.000000000000000000, 0.9659258262890683122, 1.000000000000000000, 0.9659258262890683122, 1.000000000000000000, 0.9659258262890683122, 1.000000000000000000, 0.9659258262890683122, 1.000000000000000000, 0.9659258262890683122, 1.000000000000000000, 0.9659258262890683122, 1.000000000000000000, 0.9659258262890683122, 1.000000000000000000, 0.9659258262890683122, 1.000000000000000000, 0.9659258262890683122, 1.000000000000000000, 0.9659258262890683122, 1.000000000000000000, 0.9659258262890683122, 1.000000000000000000, 0.9659258262890683122, 1.000000000000000000, 0.9659258262890683122, 1.000000000000000000, 0.9659258262890683122, 1.000000000000000000, 0.9659258262890683122, 1.000000000000000000, 0.9659258262890683122, 1.000000000000000000, 0.9659258262890683122, 1.000000000000000000, 0.9659258262890683122, 1.000000000000000000, 0.9659258262890683122, 1.000000000000000000, 0.9659258262890683122, 1.000000000000000000, 0.9659258262890683122, 1.000000000000000000, 0.9659258262890683122, 1.000000000000000000, 0.9659258262890683122, 1.000000000000000000, 0.9659258262890683122, 1.000000000000000000, 0.9659258262890683122, 1.000000000000000000, 0.9659258262890683122, 1.000000000000000000, 0.9659258262890683122, 1.000000000000000000, 0.9659258262890683122, 1.000000000000000000, 0.9659258262890683122, 1.000000000000000000, 0.9659258262890683122, 1.000000000000000000, 0.9659258262890683122, 1.000000000000000000, 0.9659258262890683122, 1.000000000000000000, 0.9659258262890683122, 1.000000000000000000, 0.9659258262890683122, 1.000000000000000000, 0.9659258262890683122, 1.000000000000000000, 0.9659258262890683122, 1.000000000000000000, 0.9659258262890683122, 1.000000000000000000, 0.9659258262890683122, 1.000000000000000000, 0.9659258262890683122, 1.000000000000000000, 0.9659258262890683122, 1.000000000000000000, 0.9659258262890683122, 1.000000000000000000, 0.9659258262890683122, 1.000000000000000000, 0.9659258262890683122, 1.000000000000000000, 0.9659258262890683122, 1.000000000000000000, 0.9659258262890683122, 1.000000000000000000, 0.9659258262890683122, 1.000000000000000000, 0.9659258262890683122, 1.000000000000000000, 0.9659258262890683122, 1.000000000000000000, 0.9659258262890683122, 1.000000000000000000, 0.9659258262890683122, 1.000000000000000000, 0.9659258262890683122, 1.000000000000000000, 0.9659258262890683122, 1.000000000000000000, 0.9659258262890683122, 1.000000000000000000, 0.9659258262890683122, 1.000000000000000000, 0.9659258262890683122, 1.000000000000000000, 0.9659258262890683122, 1.000000000000000000, 0.9659258262890683122, 1.000000000000000000, 0.9659258262890683122, 1.000000000000000000, 0.9659258262890683122, 1.000000000000000000, 0.9659258262890683122, 1.000000000000000000, 0.9659258262890683122, 1.000000000000000000, 0.9659258262890683122, 1.000000000000000000, 0.9659258262890683122, 1.000000000000000000, 0.9659258262890683122, 1.000000000000000000, 0.9659258262890683122, 1.000000000000000000, 0.9659258262890683122, 1.000000000000000000, 0.9659258262890683122, 1.000000000000000000, 0.9659258262890683122, 1.000000000000000000, 0.9659258262890683122, 1.000000000000000000, 0.9659258262890683122, 1.000000000000000000, 0.9659258262890683122, 1.000000000000000000, 0.9659258262890683122, 1.000000000000000000, 0.9659258262890683122, 1.000000000000000000, 0.9659258262890683122, 1.000000000000000000, 0.9659258262890683122, 1.000000000000000000, 0.9659258262890683122, 1.000000000000000000, 0.9659258262890683122, 1.000000000000000000, 0.9659258262890683122, 1.000000000000000000, 0.9659258262890683122, 1.000000000000000000, 0.9659258262890683122, 1.000000000000000000, 0.9659258262890683122, 1.000000000000000000, 0.9659258262890683122, 1.000000000000000000, 0.9659258262890683122, 1.000000000000000000, 0.9659258262890683122, 1.000000000000000000, 0.9659258262890683122, 1.000000000000000000, 0.9659258262890683122, 1.000000000000000000, 0.9659258262890683122, 1.000000000000000000),
 ( 1.000000000000000000, 0.9659258262890683122, 1.000000000000000000, 0.9659258262890683122, 1.000000000000000000, 0.9659258262890683122, 1.000000000000000000, 0.9659258262890683122, 1.000000000000000000, 0.9659258262890683122, 1.000000000000000000, 0.9659258262890683122, 1.000000000000000000, 0.9659258262890683122, 1.000000000000000000, 0.9659258262890683122, 1.000000000000000000, 0.9659258262890683122, 1.000000000000000000, 0.9659258262890683122, 1.000000000000000000, 0.9659258262890683122, 1.000000000000000000, 0.9659258262890683122, 1.000000000000000000, 0.9659258262890683122, 1.000000000000000000, 0.9659258262890683122, 1.000000000000000000, 0.9659258262890683122, 1.000000000000000000, 0.9659258262890683122, 1.000000000000000000, 0.9659258262890683122, 1.000000000000000000, 0.9659258262890683122, 1.000000000000000000, 0.9659258262890683122, 1.000000000000000000, 0.9659258262890683122, 1.000000000000000000, 0.9659258262890683122, 1.000000000000000000, 0.9659258262890683122, 1.000000000000000000, 0.9659258262890683122, 1.000000000000000000, 0.9659258262890683122, 1.000000000000000000, 0.9659258262890683122, 1.000000000000000000, 0.9659258262890683122, 1.000000000000000000, 0.9659258262890683122, 1.000000000000000000, 0.9659258262890683122, 1.000000000000000000, 0.9659258262890683122, 1.000000000000000000, 0.9659258262890683122, 1.000000000000000000, 0.9659258262890683122, 1.000000000000000000, 0.9659258262890683122, 1.000000000000000000, 0.9659258262890683122, 1.000000000000000000, 0.9659258262890683122, 1.000000000000000000, 0.9659258262890683122, 1.000000000000000000, 0.9659258262890683122, 1.000000000000000000, 0.9659258262890683122, 1.000000000000000000, 0.9659258262890683122, 1.000000000000000000, 0.9659258262890683122, 1.000000000000000000, 0.9659258262890683122, 1.000000000000000000, 0.9659258262890683122, 1.000000000000000000, 0.9659258262890683122, 1.000000000000000000, 0.9659258262890683122, 1.000000000000000000, 0.9659258262890683122, 1.000000000000000000, 0.9659258262890683122, 1.000000000000000000, 0.9659258262890683122, 1.000000000000000000, 0.9659258262890683122, 1.000000000000000000, 0.9659258262890683122, 1.000000000000000000, 0.9659258262890683122, 1.000000000000000000, 0.9659258262890683122, 1.000000000000000000, 0.9659258262890683122, 1.000000000000000000, 0.9659258262890683122, 1.000000000000000000, 0.9659258262890683122, 1.000000000000000000, 0.9659258262890683122, 1.000000000000000000, 0.9659258262890683122, 1.000000000000000000, 0.9659258262890683122, 1.000000000000000000, 0.9659258262890683122, 1.000000000000000000, 0.9659258262890683122, 1.000000000000000000, 0.9659258262890683122, 1.000000000000000000, 0.9659258262890683122, 1.000000000000000000, 0.9659258262890683122, 1.000000000000000000, 0.9659258262890683122, 1.000000000000000000, 0.9659258262890683122, 1.000000000000000000, 0.9659258262890683122, 1.000000000000000000, 0.9659258262890683122, 1.000000000000000000, 0.9659258262890683122, 1.000000000000000000, 0.9659258262890683122, 1.000000000000000000, 0.9659258262890683122, 1.000000000000000000, 0.9659258262890683122, 1.000000000000000000, 0.9659258262890683122, 1.000000000000000000, 0.9659258262890683122, 1.000000000000000000, 0.9659258262890683122, 1.000000000000000000, 0.9659258262890683122, 1.000000000000000000, 0.9659258262890683122, 1.000000000000000000, 0.9659258262890683122, 1.000000000000000000, 0.9659258262890683122, 1.000000000000000000, 0.9659258262890683122, 1.000000000000000000, 0.9659258262890683122, 1.000000000000000000, 0.9659258262890683122, 1.000000000000000000, 0.9659258262890683122, 1.000000000000000000, 0.9659258262890683122, 1.000000000000000000, 0.9659258262890683122, 1.000000000000000000, 0.9659258262890683122, 1.000000000000000000, 0.9659258262890683122, 1.000000000000000000, 0.9659258262890683122, 1.000000000000000000, 0.9659258262890683122, 1.000000000000000000, 0.9659258262890683122, 1.000000000000000000, 0.9659258262890683122, 1.000000000000000000, 0.9659258262890683122, 1.000000000000000000, 0.9659258262890683122, 1.000000000000000000, 0.9659258262890683122, 1.000000000000000000, 0.9659258262890683122, 1.000000000000000000, 0.9659258262890683122, 1.000000000000000000, 0.9659258262890683122, 1.000000000000000000, 0.9659258262890683122, 1.000000000000000000, 0.9659258262890683122, 1.000000000000000000, 0.9659258262890683122, 1.000000000000000000, 0.9659258262890683122, 1.000000000000000000, 0.9659258262890683122, 1.000000000000000000, 0.9659258262890683122, 1.000000000000000000, 0.9659258262890683122, 1.000000000000000000, 0.9659258262890683122, 1.000000000000000000, 0.9659258262890683122, 1.000000000000000000, 0.9659258262890683122, 1.000000000000000000, 0.9659258262890683122, 1.000000000000000000, 0.9659258262890683122, 1.000000000000000000, 0.9659258262890683122, 1.000000000000000000, 0.9659258262890683122, 1.000000000000000000, 0.9659258262890683122, 1.000000000000000000, 0.9659258262890683122, 1.000000000000000000, 0.9659258262890683122, 1.000000000000000000, 0.9659258262890683122, 1.000000000000000000, 0.9659258262890683122, 1.000000000000000000, 0.9659258262890683122, 1.000000000000000000, 0.9659258262890683122, 1.000000000000000000, 0.9659258262890683122, 1.000000000000000000, 0.9659258262890683122, 1.000000000000000000, 0.9659258262890683122, 1.000000000000000000, 0.9659258262890683122, 1.000000000000000000, 0.9659258262890683122, 1.000000000000000000, 0.9659258262890683122, 1.000000000000000000, 0.9659258262890683122, 1.000000000000000000, 0.9659258262890683122, 1.000000000000000000, 0.9659258262890683122, 1.000000000000000000, 0.9659258262890683122, 1.000000000000000000, 0.9659258262890683122, 1.000000000000000000, 0.9659258262890683122, 1.000000000000000000, 0.9659258262890683122, 1.000000000000000000, 0.9659258262890683122, 1.000000000000000000, 0.9659258262890683122, 1.000000000000000000, 0.9659258262890683122, 1.000000000000000000, 0.9659258262890683122, 1.000000000000000000, 0.9659258262890683122, 1.000000000000000000, 0.9659258262890683122, 1.000000000000000000, 0.9659258262890683122, 1.000000000000000000, 0.9659258262890683122, 1.000000000000000000, 0.9659258262890683122, 1.000000000000000000, 0.9659258262890683122, 1.000000000000000000, 0.9659258262890683122, 1.000000000000000000, 0.9659258262890683122, 1.000000000000000000, 0.9659258262890683122, 1.000000000000000000, 0.9659258262890683122, 1.000000000000000000, 0.9659258262890683122, 1.000000000000000000, 0.9659258262890683122, 1.000000000000000000, 0.9659258262890683122, 1.000000000000000000, 0.9659258262890683122, 1.000000000000000000, 0.9659258262890683122, 1.000000000000000000, 0.9659258262890683122, 1.000000000000000000, 0.9659258262890683122, 1.000000000000000000, 0.9659258262890683122, 1.000000000000000000, 0.9659258262890683122, 1.000000000000000000, 0.9659258262890683122, 1.000000000000000000, 0.9659258262890683122, 1.000000000000000000, 0.9659258262890683122, 1.000000000000000000, 0.9659258262890683122, 1.000000000000000000, 0.9659258262890683122, 1.000000000000000000, 0.9659258262890683122, 1.000000000000000000, 0.9659258262890683122, 1.000000000000000000, 0.9659258262890683122, 1.000000000000000000, 0.9659258262890683122, 1.000000000000000000, 0.9659258262890683122, 1.000000000000000000, 0.9659258262890683122, 1.000000000000000000) ) ) 
 REPRESENTATION_ITEM ( '' )  SURFACE ( )  );
#84122 = CARTESIAN_POINT ( 'NONE',  ( 18.52753015748618282, 48.92559781766745886, -4.923371831947291888 ) ) ;
#84124 = CARTESIAN_POINT ( 'NONE',  ( -0.2838433074297238012, 13.12729635533385597, -10.00000000000000000 ) ) ;
#84123 = CARTESIAN_POINT ( 'NONE',  ( 0.5774900079438607392, 3.480352010821504027, 5.440088680355550821 ) ) ;
#84125 = CARTESIAN_POINT ( 'NONE',  ( 13.43411237798105340, 5.581968003263753531, 12.81628187352647963 ) ) ;
#84126 = VERTEX_POINT ( 'NONE', #44449 ) ;
#84127 = AXIS2_PLACEMENT_3D ( 'NONE', #78056, #77067, #24083 ) ;
#84128 = CARTESIAN_POINT ( 'NONE',  ( 10.00000000000000178, 34.31368534415484106, 10.88017736071110342 ) ) ;
#84130 = CARTESIAN_POINT ( 'NONE',  ( 15.41943733314631793, -0.03417435944610275333, -4.256565371896342320 ) ) ;
#84129 = CARTESIAN_POINT ( 'NONE',  ( 14.92337183194729633, 57.67559781766745886, 8.527530157486181039 ) ) ;
#84131 = CARTESIAN_POINT ( 'NONE',  ( 2.035157376598824452, 8.688685344154839285, 7.964842623401179544 ) ) ;
#84132 = CARTESIAN_POINT ( 'NONE',  ( 4.559911319644449179, 32.23035201082150536, -9.422509992056141925 ) ) ;
#84133 = CARTESIAN_POINT ( 'NONE',  ( 24.16423886937409904, 39.09541550158062506, 3.795296366450317205 ) ) ;
#84134 = CARTESIAN_POINT ( 'NONE',  ( 0.1532563361054082862, 31.21726448433412315, 2.638427012816831674 ) ) ;
#84135 = CARTESIAN_POINT ( 'NONE',  ( 20.88017736071110164, 50.35535201082151247, 2.915334737309930979 ) ) ;
#84136 = CARTESIAN_POINT ( 'NONE',  ( 24.35999999999999233, 44.49999999999997158, 9.500000000000000000 ) ) ;
#84137 = PRESENTATION_STYLE_ASSIGNMENT (( #46131 ) ) ;
#84138 =( GEOMETRIC_REPRESENTATION_CONTEXT ( 3 ) GLOBAL_UNCERTAINTY_ASSIGNED_CONTEXT ( ( #44121 ) ) GLOBAL_UNIT_ASSIGNED_CONTEXT ( ( #52749, #46248, #39246 ) ) REPRESENTATION_CONTEXT ( 'NONE', 'WORKASPACE' ) );
#84139 = AXIS2_PLACEMENT_3D ( 'NONE', #70942, #54922, #86908 ) ;
#84140 = UNCERTAINTY_MEASURE_WITH_UNIT (LENGTH_MEASURE( 1.000000000000000082E-05 ), #21266, 'distance_accuracy_value', 'NONE');
#84141 = CARTESIAN_POINT ( 'NONE',  ( -1.114591949025130369, 3.902037737440774503E-16, 14.45709807627963706 ) ) ;
#84142 = CARTESIAN_POINT ( 'NONE',  ( 14.92337183194729633, 57.67559781766745886, 8.527530157486181039 ) ) ;
#84143 = AXIS2_PLACEMENT_3D ( 'NONE', #11081, #64549, #42085 ) ;
#84144 = VERTEX_POINT ( 'NONE', #52449 ) ;
#84145 = ORIENTED_EDGE ( 'NONE', *, *, #13820, .F. ) ;
#84146 = CARTESIAN_POINT ( 'NONE',  ( 10.00000000000000000, 35.55374883491396787, -14.16423886937410082 ) ) ;
#84148 = VECTOR ( 'NONE', #95011, 1000.000000000000000 ) ;
#84147 = CARTESIAN_POINT ( 'NONE',  ( 2.917880565312950480, 20.97041550158063217, -12.26659068614894821 ) ) ;
#84149 = CARTESIAN_POINT ( 'NONE',  ( 2.791683348922240793, 6.633931151000785675, 7.208316651077764092 ) ) ;
#84150 = EDGE_CURVE ( 'NONE', #29028, #156, #94725, .T. ) ;
#84151 = CARTESIAN_POINT ( 'NONE',  ( 6.565887622018943937, 8.081968003263751754, -12.81628187352647608 ) ) ;
#84152 = CARTESIAN_POINT ( 'NONE',  ( 0.000000000000000000, 14.49999999999999822, 0.000000000000000000 ) ) ;
#84153 = CARTESIAN_POINT ( 'NONE',  ( -8.330954874177404434, -7.272562134471185047, 3.750000000000000000 ) ) ;
#84155 = CARTESIAN_POINT ( 'NONE',  ( 21.09922568453595559, 22.04030133659708923, -6.408140936763230044 ) ) ;
#84154 = CARTESIAN_POINT ( 'NONE',  ( 20.88017736071110875, 60.77201867748817676, -2.915334737309920765 ) ) ;
#84156 = CARTESIAN_POINT ( 'NONE',  ( 2.917880565312950480, 35.97041550158063217, -12.26659068614894821 ) ) ;
#84157 = CARTESIAN_POINT ( 'NONE',  ( 4.559911319644449179, 12.23035201082150714, -9.422509992056141925 ) ) ;
#84158 = CARTESIAN_POINT ( 'NONE',  ( 15.44008868035555793, 36.39701867748816966, -9.422509992056140149 ) ) ;
#84159 = DIRECTION ( 'NONE',  ( 0.000000000000000000, 0.000000000000000000, 1.000000000000000000 ) ) ;
#84160 = CARTESIAN_POINT ( 'NONE',  ( 7.084665262690076126, 57.02201867748817676, -10.88017736071110164 ) ) ;
#84161 = EDGE_CURVE ( 'NONE', #1168, #92445, #35963, .T. ) ;
#84162 = CARTESIAN_POINT ( 'NONE',  ( 10.00000000000000000, 47.87363466993042493, -12.81628187352647608 ) ) ;
#84163 = CARTESIAN_POINT ( 'NONE',  ( -9.846743663894596210, -29.19940218233254470, -2.638427012816824124 ) ) ;
#84164 = ORIENTED_EDGE ( 'NONE', *, *, #492, .T. ) ;
#84165 = CARTESIAN_POINT ( 'NONE',  ( 19.90229974777923161, 0.3225724651664713671, 6.500000000000000000 ) ) ;
#84166 = VERTEX_POINT ( 'NONE', #28470 ) ;
#84167 = CARTESIAN_POINT ( 'NONE',  ( 8.979999999999991545, 0.000000000000000000, 2.900000000000000355 ) ) ;
#84168 = ORIENTED_EDGE ( 'NONE', *, *, #71634, .F. ) ;
#84169 = FILL_AREA_STYLE ('',( #57818 ) ) ;
#84171 = CARTESIAN_POINT ( 'NONE',  ( 13.79529636645031943, 60.34541550158063927, -14.16423886937409904 ) ) ;
#84170 = CARTESIAN_POINT ( 'NONE',  ( -0.3689425029237881626, 57.42874883491397497, 10.36894250292379027 ) ) ;
#84173 = CARTESIAN_POINT ( 'NONE',  ( 17.20831665107776587, 64.13393115100079456, -7.208316651077762316 ) ) ;
#84172 = CARTESIAN_POINT ( 'NONE',  ( 17.20831665107776587, 24.13393115100078035, -7.208316651077762316 ) ) ;
#84174 = CARTESIAN_POINT ( 'NONE',  ( -2.361121941889217979, 14.76984946027100243, 14.75287579053847509 ) ) ;
#84175 = CARTESIAN_POINT ( 'NONE',  ( 22.81628187352647785, 1.623634669930420271, 6.195893100308588602E-16 ) ) ;
#84176 = CARTESIAN_POINT ( 'NONE',  ( -3.434112377981047626, 15.16530133659708390, 12.81628187352647963 ) ) ;
#84177 = ORIENTED_EDGE ( 'NONE', *, *, #39298, .F. ) ;
#84178 = CARTESIAN_POINT ( 'NONE',  ( -2.266590686148945544, 36.38708216824730357, -7.082119434687050408 ) ) ;
#84179 = CARTESIAN_POINT ( 'NONE',  ( 24.16423886937409904, 49.09541550158063217, 3.795296366450317205 ) ) ;
#84180 = VERTEX_POINT ( 'NONE', #43460 ) ;
#84181 = CARTESIAN_POINT ( 'NONE',  ( 0.6178305044545818747, 58.49863466993042493, -9.382169495545419124 ) ) ;
#84182 = CARTESIAN_POINT ( 'NONE',  ( 12.63842701281683922, 44.55059781766745175, -9.846743663894590881 ) ) ;
#84183 = CARTESIAN_POINT ( 'NONE',  ( 19.42250999205614548, 20.98035201082150891, -5.440088680355545492 ) ) ;
#84184 = CARTESIAN_POINT ( 'NONE',  ( 17.20831665107776587, 59.13393115100078745, -7.208316651077762316 ) ) ;
#84185 = CARTESIAN_POINT ( 'NONE',  ( 10.00000000000000178, 52.25893115100078745, 9.846743663894594434 ) ) ;
#84186 = CARTESIAN_POINT ( 'NONE',  ( -2.816281873526473856, 29.12363466993041783, 9.499525473075851096E-16 ) ) ;
#84188 = ORIENTED_EDGE ( 'NONE', *, *, #74422, .T. ) ;
#84187 = CARTESIAN_POINT ( 'NONE',  ( 0.000000000000000000, 15.00000000000000000, 0.000000000000000000 ) ) ;
#84189 = DIRECTION ( 'NONE',  ( 0.000000000000000000, 1.000000000000000000, 0.000000000000000000 ) ) ;
#84190 = CARTESIAN_POINT ( 'NONE',  ( 2.791683348922237240, 0.3839311510007847872, -7.208316651077763204 ) ) ;
#84191 = DIRECTION ( 'NONE',  ( 0.000000000000000000, -0.000000000000000000, -1.000000000000000000 ) ) ;
#84192 = ORIENTED_EDGE ( 'NONE', *, *, #22725, .F. ) ;
#84193 = COLOUR_RGB ( '', 0.08235294, 0.09019608, 0.10196078) ;
#84194 = CARTESIAN_POINT ( 'NONE',  ( 8.880000000000000782, 1.019547802438459216, 4.000000000000000000 ) ) ;
#84195 = CARTESIAN_POINT ( 'NONE',  ( 1.472469842513823179, 26.42559781766745175, 4.923371831947296329 ) ) ;
#84196 = CARTESIAN_POINT ( 'NONE',  ( -7.598395483715266452E-32, -2.710505431213761085E-16, 0.000000000000000000 ) ) ;
#84197 = CARTESIAN_POINT ( 'NONE',  ( 3.591859063236761518, 34.95696800326375353, 11.09922568453594849 ) ) ;
#84198 = CARTESIAN_POINT ( 'NONE',  ( -3.500000000000000444, 1.019547802438453887, 3.750000000000000444 ) ) ;
#84199 = CIRCLE ( 'NONE', #49074, 1.499999999999999112 ) ;
#84200 = ORIENTED_EDGE ( 'NONE', *, *, #68363, .F. ) ;
#84201 = CARTESIAN_POINT ( 'NONE',  ( -9.000000000000001776, 83.99999999999994316, -2.900000000000000799 ) ) ;
#84202 = CARTESIAN_POINT ( 'NONE',  ( -0.7375392941516176748, 15.00000000000000000, -14.98185688723471820 ) ) ;
#84203 = CARTESIAN_POINT ( 'NONE',  ( 19.84674366389459621, 58.50893115100078745, 7.409399052514197653E-17 ) ) ;
#84204 = CARTESIAN_POINT ( 'NONE',  ( 20.36894250292379382, 38.67874883491396076, 10.36894250292379205 ) ) ;
#84205 = CARTESIAN_POINT ( 'NONE',  ( 1.472469842513823179, 56.42559781766745886, 4.923371831947296329 ) ) ;
#84206 = B_SPLINE_CURVE_WITH_KNOTS ( 'NONE', 3,
 ( #96542, #74011, #35019, #27526, #88526, #81025 ),
 .UNSPECIFIED., .F., .F.,
 ( 4, 2, 4 ),
 ( 4.336808689942017736E-18, 0.0002605067024380912301, 0.0005210134048761781234 ),
 .UNSPECIFIED. ) ;
#84207 = CARTESIAN_POINT ( 'NONE',  ( -4.391347328463997002, 14.76984910450705257, 14.28069739540189254 ) ) ;
#84208 = CARTESIAN_POINT ( 'NONE',  ( 0.1532563361054083140, 6.008931151000784787, 1.131784320476157264E-15 ) ) ;
#84209 =( GEOMETRIC_REPRESENTATION_CONTEXT ( 3 ) GLOBAL_UNCERTAINTY_ASSIGNED_CONTEXT ( ( #93459 ) ) GLOBAL_UNIT_ASSIGNED_CONTEXT ( ( #2289, #87225, #20588 ) ) REPRESENTATION_CONTEXT ( 'NONE', 'WORKASPACE' ) );
#84210 = CARTESIAN_POINT ( 'NONE',  ( 6.565887622018943937, 48.08196800326375353, -12.81628187352647608 ) ) ;
#84211 = CARTESIAN_POINT ( 'NONE',  ( -4.164238869374099927, 2.012082168247300906, 3.795296366450308767 ) ) ;
#84212 = EDGE_CURVE ( 'NONE', #16145, #42399, #89128, .T. ) ;
#84213 = CARTESIAN_POINT ( 'NONE',  ( 19.84674366389459621, 43.50893115100078745, 7.409399052514197653E-17 ) ) ;
#84214 = CARTESIAN_POINT ( 'NONE',  ( 10.00000000000000178, 49.31368534415484106, 10.88017736071110342 ) ) ;
#84215 = AXIS2_PLACEMENT_3D ( 'NONE', #41414, #32889, #48872 ) ;
#84216 = CARTESIAN_POINT ( 'NONE',  ( 18.52753015748617571, 48.09226448433412315, 4.923371831947298993 ) ) ;
#84217 = AXIS2_PLACEMENT_3D ( 'NONE', #69997, #61985, #15041 ) ;
#84218 = CARTESIAN_POINT ( 'NONE',  ( -3.195792623639539531, 6.620456701841148650, -11.92686044187656513 ) ) ;
#84219 = ORIENTED_EDGE ( 'NONE', *, *, #85560, .T. ) ;
#84220 = CARTESIAN_POINT ( 'NONE',  ( 1.274849032794294290, 53.57228050351032067, 6.499999999999979572 ) ) ;
#84221 = CARTESIAN_POINT ( 'NONE',  ( 12.91533473730993009, 26.60535201082150536, -10.88017736071109987 ) ) ;
#84223 = CARTESIAN_POINT ( 'NONE',  ( 20.88017736071110875, 50.77201867748817676, -2.915334737309920765 ) ) ;
#84222 = CARTESIAN_POINT ( 'NONE',  ( 0.6178305044545838731, 4.748634669930420493, 9.382169495545420901 ) ) ;
#84224 = SURFACE_SIDE_STYLE ('',( #82723 ) ) ;
#84225 = CARTESIAN_POINT ( 'NONE',  ( -7.684764310694977674, 0.3639308364404307827, 12.88194075009933393 ) ) ;
#84227 = DIRECTION ( 'NONE',  ( 1.000000000000000000, -0.000000000000000000, 0.000000000000000000 ) ) ;
#84226 = CARTESIAN_POINT ( 'NONE',  ( 7.084665262690076126, 42.02201867748816966, -10.88017736071110164 ) ) ;
#84228 = CARTESIAN_POINT ( 'NONE',  ( 12.63842701281683922, 9.550597817667449974, -9.846743663894590881 ) ) ;
#84229 = CARTESIAN_POINT ( 'NONE',  ( 0.1532563361054082862, 36.21726448433410894, 2.638427012816831674 ) ) ;
#84230 = DIRECTION ( 'NONE',  ( -1.000000000000000000, 0.000000000000000000, 0.000000000000000000 ) ) ;
#84231 = CARTESIAN_POINT ( 'NONE',  ( 7.082119434687054849, 23.47041550158063217, 12.26659068614894288 ) ) ;
#84232 = CARTESIAN_POINT ( 'NONE',  ( 12.63842701281683034, 62.46726448433410894, 9.846743663894596210 ) ) ;
#84233 = EDGE_CURVE ( 'NONE', #30157, #42828, #66460, .T. ) ;
#84234 = CARTESIAN_POINT ( 'NONE',  ( 10.00000000000000000, 1.813685344154838175, -10.88017736071110342 ) ) ;
#84235 = CARTESIAN_POINT ( 'NONE',  ( 2.261421327065715303, 0.000000000000000000, 4.962236210031257144 ) ) ;
#84236 = CARTESIAN_POINT ( 'NONE',  ( 6.204703633549690345, 20.76208216824730357, -14.16423886937410259 ) ) ;
#84237 = CARTESIAN_POINT ( 'NONE',  ( -4.164238869374099927, 47.01208216824729647, 3.795296366450308767 ) ) ;
#84238 = CARTESIAN_POINT ( 'NONE',  ( 18.52753015748617571, 33.09226448433411605, 4.923371831947298993 ) ) ;
#84239 = CARTESIAN_POINT ( 'NONE',  ( 19.84674366389459266, 18.71726448433411960, -2.638427012816827677 ) ) ;
#84240 = CARTESIAN_POINT ( 'NONE',  ( 19.42250999205614548, 5.980352010821504471, -5.440088680355545492 ) ) ;
#84241 = EDGE_CURVE ( 'NONE', #61376, #7648, #61668, .T. ) ;
#84242 = ORIENTED_EDGE ( 'NONE', *, *, #24656, .F. ) ;
#84243 = CARTESIAN_POINT ( 'NONE',  ( 0.1532563361054083140, 31.00893115100078390, 1.131784320476157264E-15 ) ) ;
#84244 = CARTESIAN_POINT ( 'NONE',  ( 17.96484262340118221, 31.18868534415483751, -7.964842623401177768 ) ) ;
#84245 = CARTESIAN_POINT ( 'NONE',  ( 19.84674366389459621, 58.50893115100078745, 7.409399052514197653E-17 ) ) ;
#84247 = CARTESIAN_POINT ( 'NONE',  ( 14.71525861348287734, 0.5000000000000004441, 2.908807992686682109 ) ) ;
#84246 = CARTESIAN_POINT ( 'NONE',  ( 10.00000000000000178, 8.053748834913967869, 14.16423886937410082 ) ) ;
#84248 = DIRECTION ( 'NONE',  ( 0.9961946980917461003, -0.08715574274765139351, 0.000000000000000000 ) ) ;
#84249 = EDGE_CURVE ( 'NONE', #89076, #34917, #54807, .T. ) ;
#84250 = COLOUR_RGB ( '', 0.72549020, 0.75294118, 0.79215686) ;
#84251 = CARTESIAN_POINT ( 'NONE',  ( 19.84674366389459266, 13.30059781766745353, 2.638427012816836559 ) ) ;
#84252 = CARTESIAN_POINT ( 'NONE',  ( 21.09922568453595559, 42.04030133659708213, -6.408140936763230044 ) ) ;
#84253 = CARTESIAN_POINT ( 'NONE',  ( 10.00000000000000178, 47.25893115100078745, 9.846743663894594434 ) ) ;
#84254 = ORIENTED_EDGE ( 'NONE', *, *, #65117, .F. ) ;
#84255 = CARTESIAN_POINT ( 'NONE',  ( 2.791683348922237240, 25.38393115100078390, -7.208316651077763204 ) ) ;
#84256 = CARTESIAN_POINT ( 'NONE',  ( 10.79855660033419262, -95.56318652451196272, -4.000000000000000000 ) ) ;
#84257 = CARTESIAN_POINT ( 'NONE',  ( 6.204703633549690345, 57.84541550158063927, 14.16423886937410082 ) ) ;
#84258 = CARTESIAN_POINT ( 'NONE',  ( 2.035157376598824452, 48.68868534415483396, 7.964842623401179544 ) ) ;
#84259 = CARTESIAN_POINT ( 'NONE',  ( -0.3689425029237898834, 1.178748834913967869, -10.36894250292378850 ) ) ;
#84260 = CARTESIAN_POINT ( 'NONE',  ( -3.750000000000000000, 36.75000000000000000, -3.750000000000000000 ) ) ;
#84261 = CARTESIAN_POINT ( 'NONE',  ( 14.92337183194729633, 42.67559781766745886, 8.527530157486181039 ) ) ;
#84262 = CARTESIAN_POINT ( 'NONE',  ( 10.00000000000000000, 11.81368534415483751, -10.88017736071110342 ) ) ;
#84263 = CARTESIAN_POINT ( 'NONE',  ( 5.806645064956438063, 8.233160247311797324E-16, 13.42464971017000330 ) ) ;
#84264 = CARTESIAN_POINT ( 'NONE',  ( 18.52753015748617571, 48.09226448433412315, 4.923371831947298993 ) ) ;
#84265 = CARTESIAN_POINT ( 'NONE',  ( 20.88017736071110164, 50.35535201082151247, 2.915334737309930979 ) ) ;
#84266 = SURFACE_STYLE_FILL_AREA ( #70734 ) ;
#84267 = CIRCLE ( 'NONE', #36348, 1.249999999999987121 ) ;
#84268 = ORIENTED_EDGE ( 'NONE', *, *, #43796, .F. ) ;
#84269 = ORIENTED_EDGE ( 'NONE', *, *, #97258, .F. ) ;
#84270 = LINE ( 'NONE', #15770, #90036 ) ;
#84271 = DIRECTION ( 'NONE',  ( -8.673617379884027583E-16, -1.000000000000000000, 0.000000000000000000 ) ) ;
#84272 = EDGE_CURVE ( 'NONE', #55236, #47721, #40500, .T. ) ;
#84273 = CARTESIAN_POINT ( 'NONE',  ( 18.52753015748618282, 3.925597817667451306, -4.923371831947291888 ) ) ;
#84274 = CARTESIAN_POINT ( 'NONE',  ( 0.6178305044545838731, 59.74863466993041783, 9.382169495545420901 ) ) ;
#84276 = CARTESIAN_POINT ( 'NONE',  ( 1.472469842513823179, 46.42559781766745175, 4.923371831947296329 ) ) ;
#84275 = CARTESIAN_POINT ( 'NONE',  ( 2.917880565312948704, 67.63708216824730357, 12.26659068614894643 ) ) ;
#84277 = CARTESIAN_POINT ( 'NONE',  ( 14.35840480524198171, 14.63595249122788999, 4.340070442838947606 ) ) ;
#84278 = CARTESIAN_POINT ( 'NONE',  ( 22.26659068614895176, 59.72041550158063927, -7.082119434687042414 ) ) ;
#84279 = CARTESIAN_POINT ( 'NONE',  ( 12.63842701281683034, 52.46726448433413026, 9.846743663894596210 ) ) ;
#84280 = CARTESIAN_POINT ( 'NONE',  ( 18.00000000000000355, 77.66934307245642799, 4.068269658013480949 ) ) ;
#84281 = CARTESIAN_POINT ( 'NONE',  ( 19.42250999205614193, 45.14701867748817676, 5.440088680355555262 ) ) ;
#84282 = ADVANCED_FACE ( 'NONE', ( #7462 ), #76920, .F. ) ;
#84283 = CARTESIAN_POINT ( 'NONE',  ( 19.42250999205614548, 65.98035201082151957, -5.440088680355545492 ) ) ;
#84284 = CARTESIAN_POINT ( 'NONE',  ( 3.969999999999999751, 36.75000000000000000, -2.750000000000000000 ) ) ;
#84285 = ORIENTED_EDGE ( 'NONE', *, *, #85831, .F. ) ;
#84286 = CARTESIAN_POINT ( 'NONE',  ( -2.816281873526471635, 58.91530133659707502, -3.434112377981056508 ) ) ;
#84287 = ORIENTED_EDGE ( 'NONE', *, *, #6093, .T. ) ;
#84288 = VECTOR ( 'NONE', #74351, 1000.000000000000000 ) ;
#84289 = CARTESIAN_POINT ( 'NONE',  ( 5.076628168052703671, 11.84226448433411960, 8.527530157486179263 ) ) ;
#84290 = ORIENTED_EDGE ( 'NONE', *, *, #61910, .F. ) ;
#84291 = CARTESIAN_POINT ( 'NONE',  ( 13.79529636645030344, 13.26208216824729824, 14.16423886937410614 ) ) ;
#84292 = CARTESIAN_POINT ( 'NONE',  ( 1.472469842513823179, 25.59226448433412315, -4.923371831947296329 ) ) ;
#84293 = CARTESIAN_POINT ( 'NONE',  ( 15.44008868035555793, 31.39701867748817676, -9.422509992056140149 ) ) ;
#84294 = VECTOR ( 'NONE', #98257, 1000.000000000000000 ) ;
#84295 = FACE_OUTER_BOUND ( 'NONE', #13317, .T. ) ;
#84296 = ORIENTED_EDGE ( 'NONE', *, *, #89313, .T. ) ;
#84297 = VECTOR ( 'NONE', #85625, 1000.000000000000000 ) ;
#84298 = CARTESIAN_POINT ( 'NONE',  ( 2.035157376598822676, 32.43868534415483396, -7.964842623401177768 ) ) ;
#84299 = EDGE_LOOP ( 'NONE', ( #80500, #92534, #21167, #48583 ) ) ;
#84300 = CARTESIAN_POINT ( 'NONE',  ( -0.8801773607111009756, 38.06368534415484106, 1.068504757029289695E-15 ) ) ;
#84301 = CARTESIAN_POINT ( 'NONE',  ( 20.10421743870887568, 55.60736173766201773, -6.337391062633416894 ) ) ;
#84302 = ORIENTED_EDGE ( 'NONE', *, *, #18604, .F. ) ;
#84303 = ORIENTED_EDGE ( 'NONE', *, *, #74271, .F. ) ;
#84304 = CARTESIAN_POINT ( 'NONE',  ( 21.09922568453595559, 17.04030133659708923, -6.408140936763230044 ) ) ;
#84305 = CARTESIAN_POINT ( 'NONE',  ( 0.1532563361054082862, 11.21726448433411605, 2.638427012816831674 ) ) ;
#84306 =( NAMED_UNIT ( * ) PLANE_ANGLE_UNIT ( ) SI_UNIT ( $, .RADIAN. ) );
#84307 = CARTESIAN_POINT ( 'NONE',  ( 0.000000000000000000, 0.5000000000000004441, 0.000000000000000000 ) ) ;
#84308 = CARTESIAN_POINT ( 'NONE',  ( 2.791683348922240793, 16.63393115100078745, 7.208316651077764092 ) ) ;
#84309 = CARTESIAN_POINT ( 'NONE',  ( 20.88017736071110164, 25.35535201082150891, 2.915334737309930979 ) ) ;
#84310 = ORIENTED_EDGE ( 'NONE', *, *, #12967, .T. ) ;
#84311 = ORIENTED_EDGE ( 'NONE', *, *, #7626, .T. ) ;
#84312 = CARTESIAN_POINT ( 'NONE',  ( 0.6178305044545838731, 64.74863466993043914, 9.382169495545420901 ) ) ;
#84313 = CARTESIAN_POINT ( 'NONE',  ( 0.5774900079438607392, 53.48035201082151247, 5.440088680355550821 ) ) ;
#84314 = CARTESIAN_POINT ( 'NONE',  ( -3.949999999999997069, 99.99999999999998579, 8.000000000000000000 ) ) ;
#84315 = CARTESIAN_POINT ( 'NONE',  ( 6.565887622018943937, 50.16530133659708213, 12.81628187352647430 ) ) ;
#84316 = CARTESIAN_POINT ( 'NONE',  ( 20.88017736071110875, 55.77201867748816966, -2.915334737309920765 ) ) ;
#84317 = CARTESIAN_POINT ( 'NONE',  ( -2.816281873526473856, 4.123634669930420493, 9.499525473075851096E-16 ) ) ;
#84318 = CARTESIAN_POINT ( 'NONE',  ( 17.20831665107776587, 32.88393115100078745, 7.208316651077764980 ) ) ;
#84319 = CARTESIAN_POINT ( 'NONE',  ( 16.40814093676323893, 50.79030133659708923, 11.09922568453595026 ) ) ;
#84320 = CARTESIAN_POINT ( 'NONE',  ( 6.000000000000000000, 11.50000000000000000, -6.000000000000000000 ) ) ;
#84321 = CARTESIAN_POINT ( 'NONE',  ( 10.00000000000000000, 24.75893115100078745, -9.846743663894594434 ) ) ;
#84322 = CARTESIAN_POINT ( 'NONE',  ( -2.816281873526473856, 19.33196800326375708, 3.434112377981055619 ) ) ;
#84324 = CARTESIAN_POINT ( 'NONE',  ( 0.000000000000000000, 15.00000000000000000, 0.000000000000000000 ) ) ;
#84323 = CARTESIAN_POINT ( 'NONE',  ( 2.393480905993150998, 15.00000000000000000, -14.80781041047751323 ) ) ;
#84325 = CARTESIAN_POINT ( 'NONE',  ( 17.96484262340118221, 34.93868534415482685, 7.964842623401181321 ) ) ;
#84326 = CARTESIAN_POINT ( 'NONE',  ( 6.565887622018943937, -1.918031996736246692, -12.81628187352647608 ) ) ;
#84327 = CARTESIAN_POINT ( 'NONE',  ( 7.684764310694801814, 14.49999999999999112, 12.88194075009947248 ) ) ;
#84328 = ADVANCED_FACE ( 'NONE', ( #60928 ), #83445, .T. ) ;
#84329 = CARTESIAN_POINT ( 'NONE',  ( 14.92337183194729633, 22.67559781766745175, 8.527530157486181039 ) ) ;
#84330 = CARTESIAN_POINT ( 'NONE',  ( 19.84674366389459266, 13.30059781766745353, 2.638427012816836559 ) ) ;
#84331 = CARTESIAN_POINT ( 'NONE',  ( -0.8801773607111008646, 18.27201867748817321, 2.915334737309923430 ) ) ;
#84332 = CARTESIAN_POINT ( 'NONE',  ( 10.00000000000000178, 10.37363466993041961, 12.81628187352647608 ) ) ;
#84333 = CARTESIAN_POINT ( 'NONE',  ( -0.8801773607110991993, 2.855352010821504471, -2.915334737309923874 ) ) ;
#84334 = SHAPE_REPRESENTATION_RELATIONSHIP ( 'NONE' , 'NONE' ,  #53719, #30996 ) ;
#84335 = CARTESIAN_POINT ( 'NONE',  ( 18.52753015748617571, 63.09226448433412315, 4.923371831947298993 ) ) ;
#84336 = CARTESIAN_POINT ( 'NONE',  ( 4.395712687241005945, -0.8323168403886667122, -2.750000000000000444 ) ) ;
#84337 = CARTESIAN_POINT ( 'NONE',  ( -0.3689425029237898834, 66.17874883491396076, -10.36894250292378850 ) ) ;
#84338 = CARTESIAN_POINT ( 'NONE',  ( 18.52753015748618282, 38.92559781766745175, -4.923371831947291888 ) ) ;
#84339 = SURFACE_STYLE_FILL_AREA ( #23838 ) ;
#84340 = CARTESIAN_POINT ( 'NONE',  ( 12.91533473730992121, 19.52201867748816611, 10.88017736071110164 ) ) ;
#84341 = CARTESIAN_POINT ( 'NONE',  ( 1.274849032794305170, 12.55509018479935968, -6.499999999999995559 ) ) ;
#84342 = CARTESIAN_POINT ( 'NONE',  ( 4.559911319644449179, 27.23035201082150536, -9.422509992056141925 ) ) ;
#84343 = CIRCLE ( 'NONE', #12454, 14.49999999999999822 ) ;
#84345 = DIRECTION ( 'NONE',  ( 0.000000000000000000, 0.000000000000000000, 1.000000000000000000 ) ) ;
#84344 = CARTESIAN_POINT ( 'NONE',  ( -0.3689425029237881626, 62.42874883491396787, 10.36894250292379027 ) ) ;
#84346 = FILL_AREA_STYLE_COLOUR ( '', #54769 ) ;
#84347 = CARTESIAN_POINT ( 'NONE',  ( 14.92337183194729988, 24.34226448433411960, -8.527530157486177487 ) ) ;
#84348 = CARTESIAN_POINT ( 'NONE',  ( 10.00000000000000000, 7.873634669930421381, -12.81628187352647608 ) ) ;
#84349 = CARTESIAN_POINT ( 'NONE',  ( 10.00000000000000178, 62.25893115100078745, 9.846743663894594434 ) ) ;
#84351 = CARTESIAN_POINT ( 'NONE',  ( -12.60874940350938189, 3.923185800807110140E-16, -7.160268045227207168 ) ) ;
#84350 = AXIS2_PLACEMENT_3D ( 'NONE', #96315, #49797, #5311 ) ;
#84352 = AXIS2_PLACEMENT_3D ( 'NONE', #36056, #44545, #89554 ) ;
#84353 = CARTESIAN_POINT ( 'NONE',  ( -10.54707717934878275, -44.61285707881522455, -3.999999999999998224 ) ) ;
#84354 = CARTESIAN_POINT ( 'NONE',  ( 17.08211943468705840, 10.13708216824730179, -12.26659068614894466 ) ) ;
#84355 = CARTESIAN_POINT ( 'NONE',  ( 19.84674366389459621, 43.50893115100078745, 7.409399052514197653E-17 ) ) ;
#84356 = ADVANCED_FACE ( 'NONE', ( #1444 ), #89937, .T. ) ;
#84357 = CARTESIAN_POINT ( 'NONE',  ( -2.266590686148945544, 56.38708216824731068, -7.082119434687050408 ) ) ;
#84358 = CARTESIAN_POINT ( 'NONE',  ( 5.076628168052704559, 25.17559781766745175, -8.527530157486179263 ) ) ;
#84360 = CARTESIAN_POINT ( 'NONE',  ( 11.36220558718857276, 15.00000000000000000, 9.008345252845320061 ) ) ;
#84359 = DIRECTION ( 'NONE',  ( 1.000000000000000000, 0.000000000000000000, 0.000000000000000000 ) ) ;
#84361 = CARTESIAN_POINT ( 'NONE',  ( 20.88017736071110164, 50.35535201082151247, 2.915334737309930979 ) ) ;
#84362 = CARTESIAN_POINT ( 'NONE',  ( 6.565887622018943937, 53.08196800326374643, -12.81628187352647608 ) ) ;
#84363 = ORIENTED_EDGE ( 'NONE', *, *, #77882, .T. ) ;
#84364 = EDGE_CURVE ( 'NONE', #25626, #98330, #46822, .T. ) ;
#84365 = CARTESIAN_POINT ( 'NONE',  ( -0.8801773607111009756, 23.06368534415484106, 1.068504757029289695E-15 ) ) ;
#84366 = CARTESIAN_POINT ( 'NONE',  ( 21.09922568453595559, 42.04030133659708213, -6.408140936763230044 ) ) ;
#84367 = CARTESIAN_POINT ( 'NONE',  ( 0.1532563361054100626, 65.80059781766745175, -2.638427012816831230 ) ) ;
#84368 = CARTESIAN_POINT ( 'NONE',  ( 2.791683348922237240, 0.3839311510007847872, -7.208316651077763204 ) ) ;
#84369 = ORIENTED_EDGE ( 'NONE', *, *, #3440, .F. ) ;
#84370 = CARTESIAN_POINT ( 'NONE',  ( 13.78891971893204271, 0.5000000000000004441, 5.904717858191622426 ) ) ;
#84371 = CARTESIAN_POINT ( 'NONE',  ( 11.94720539484406707, 14.76930270348881535, 8.972309510150243028 ) ) ;
#84372 = CARTESIAN_POINT ( 'NONE',  ( 22.26659068614894466, 38.88708216824731068, 7.082119434687054849 ) ) ;
#84373 = CARTESIAN_POINT ( 'NONE',  ( 10.00000000000000178, 8.053748834913967869, 14.16423886937410082 ) ) ;
#84374 = CARTESIAN_POINT ( 'NONE',  ( 20.88017736071110875, 15.77201867748817143, -2.915334737309920765 ) ) ;
#84375 = CARTESIAN_POINT ( 'NONE',  ( 10.00000000000000000, 36.81368534415484106, -10.88017736071110342 ) ) ;
#84376 = DIRECTION ( 'NONE',  ( 0.000000000000000000, 0.000000000000000000, 1.000000000000000000 ) ) ;
#84377 = DIRECTION ( 'NONE',  ( -0.000000000000000000, -1.000000000000000000, -0.000000000000000000 ) ) ;
#84378 = CARTESIAN_POINT ( 'NONE',  ( 17.96484262340118221, 66.18868534415483396, -7.964842623401177768 ) ) ;
#84379 = CARTESIAN_POINT ( 'NONE',  ( -0.8801773607111008646, 63.27201867748817676, 2.915334737309923430 ) ) ;
#84380 = CARTESIAN_POINT ( 'NONE',  ( 13.43411237798106583, 27.66530133659708568, -12.81628187352647252 ) ) ;
#84381 = CARTESIAN_POINT ( 'NONE',  ( 5.147851794455788443, -2.778691583467731473E-15, 13.68970903997130328 ) ) ;
#84382 = DIRECTION ( 'NONE',  ( -0.3007057995042635157, 0.000000000000000000, -0.9537169507482300412 ) ) ;
#84383 = CARTESIAN_POINT ( 'NONE',  ( 18.52753015748618282, 8.925597817667451750, -4.923371831947291888 ) ) ;
#84384 = CARTESIAN_POINT ( 'NONE',  ( 5.076628168052703671, 41.84226448433411605, 8.527530157486179263 ) ) ;
#84385 = PRODUCT_RELATED_PRODUCT_CATEGORY ( 'part', '', ( #6128 ) ) ;
#84386 = CARTESIAN_POINT ( 'NONE',  ( 12.91533473730993009, 11.60535201082150536, -10.88017736071109987 ) ) ;
#84387 = CARTESIAN_POINT ( 'NONE',  ( 10.00000000000000000, 37.87363466993041783, -12.81628187352647608 ) ) ;
#84388 = CARTESIAN_POINT ( 'NONE',  ( 17.20831665107776587, 14.13393115100078568, -7.208316651077762316 ) ) ;
#84389 = CARTESIAN_POINT ( 'NONE',  ( 0.5774900079438607392, 13.48035201082150358, 5.440088680355550821 ) ) ;
#84390 = CARTESIAN_POINT ( 'NONE',  ( 7.361572987183169658, 39.96726448433411605, -9.846743663894592657 ) ) ;
#84391 = CARTESIAN_POINT ( 'NONE',  ( 19.84674366389459266, 28.71726448433411960, -2.638427012816827677 ) ) ;
#84392 = CARTESIAN_POINT ( 'NONE',  ( 2.917880565312950480, 20.97041550158063217, -12.26659068614894821 ) ) ;
#84393 = CARTESIAN_POINT ( 'NONE',  ( 20.88017736071110875, 35.77201867748816966, -2.915334737309920765 ) ) ;
#84394 = CARTESIAN_POINT ( 'NONE',  ( 4.559911319644449179, 7.230352010821504471, -9.422509992056141925 ) ) ;
#84395 = CARTESIAN_POINT ( 'NONE',  ( 17.96484262340118221, 36.18868534415484106, -7.964842623401177768 ) ) ;
#84396 = CARTESIAN_POINT ( 'NONE',  ( -0.8801773607110991993, 32.85535201082151247, -2.915334737309923874 ) ) ;
#84397 = EDGE_LOOP ( 'NONE', ( #71126, #75030, #66996, #92874 ) ) ;
#84398 = CARTESIAN_POINT ( 'NONE',  ( 19.42250999205614548, 40.98035201082150536, -5.440088680355545492 ) ) ;
#84399 = CARTESIAN_POINT ( 'NONE',  ( 6.565887622018943937, 58.08196800326376064, -12.81628187352647608 ) ) ;
#84400 = CARTESIAN_POINT ( 'NONE',  ( -0.8801773607111008646, 43.27201867748817676, 2.915334737309923430 ) ) ;
#84401 = CARTESIAN_POINT ( 'NONE',  ( 10.00000000000000000, 51.81368534415484106, -10.88017736071110342 ) ) ;
#84402 = AXIS2_PLACEMENT_3D ( 'NONE', #96459, #6417, #36930 ) ;
#84403 = VERTEX_POINT ( 'NONE', #91434 ) ;
#84404 = CARTESIAN_POINT ( 'NONE',  ( 17.96484262340118221, 51.18868534415483396, -7.964842623401177768 ) ) ;
#84405 = CARTESIAN_POINT ( 'NONE',  ( 5.115475850186006923, -17.53855045867880591, 3.750000000001609823 ) ) ;
#84406 = CARTESIAN_POINT ( 'NONE',  ( 4.431036607602466759, 0.5000000000000004441, 14.33059365769913818 ) ) ;
#84407 = CARTESIAN_POINT ( 'NONE',  ( -4.164238869374098151, 66.59541550158060375, -3.795296366450310543 ) ) ;
#84408 = CARTESIAN_POINT ( 'NONE',  ( 7.084665262690076126, 69.10535201082151957, 10.88017736071109987 ) ) ;
#84409 = FACE_OUTER_BOUND ( 'NONE', #89468, .T. ) ;
#84410 = CARTESIAN_POINT ( 'NONE',  ( -14.62617646268096827, 14.49999999999999112, 3.327906561566773558 ) ) ;
#84411 = CARTESIAN_POINT ( 'NONE',  ( -10.88853822400146676, 46.97908644289115898, 2.899999999999999467 ) ) ;
#84412 = CARTESIAN_POINT ( 'NONE',  ( 14.92337183194729988, 39.34226448433412315, -8.527530157486177487 ) ) ;
#84413 = ORIENTED_EDGE ( 'NONE', *, *, #36828, .T. ) ;
#84414 = CARTESIAN_POINT ( 'NONE',  ( 17.20831665107776587, 34.13393115100078745, -7.208316651077762316 ) ) ;
#84415 = COLOUR_RGB ( '', 0.66274510, 0.83137255, 0.94901961) ;
#84416 = CARTESIAN_POINT ( 'NONE',  ( 12.91533473730992121, 39.52201867748817676, 10.88017736071110164 ) ) ;
#84417 = CARTESIAN_POINT ( 'NONE',  ( 19.84674366389459266, 33.30059781766744464, 2.638427012816836559 ) ) ;
#84418 = CARTESIAN_POINT ( 'NONE',  ( 0.6178305044545838731, 24.74863466993042493, 9.382169495545420901 ) ) ;
#84420 = CARTESIAN_POINT ( 'NONE',  ( 19.42250999205614193, 60.14701867748817676, 5.440088680355555262 ) ) ;
#84419 = CARTESIAN_POINT ( 'NONE',  ( 10.00000000000000178, 69.31368534415484817, 10.88017736071110342 ) ) ;
#84422 = CARTESIAN_POINT ( 'NONE',  ( 12.91533473730993009, 6.605352010821504471, -10.88017736071109987 ) ) ;
#84421 = CARTESIAN_POINT ( 'NONE',  ( 4.559911319644449179, 48.89701867748817676, 9.422509992056141925 ) ) ;
#84423 = CARTESIAN_POINT ( 'NONE',  ( 10.00000000000000178, 63.05374883491396076, 14.16423886937410082 ) ) ;
#84424 = AXIS2_PLACEMENT_3D ( 'NONE', #86268, #56269, #86761 ) ;
#84425 = CARTESIAN_POINT ( 'NONE',  ( -2.816281873526471635, 18.91530133659708213, -3.434112377981056508 ) ) ;
#84426 = DIRECTION ( 'NONE',  ( 1.000000000000000000, -0.000000000000000000, 0.000000000000000000 ) ) ;
#84427 = ORIENTED_EDGE ( 'NONE', *, *, #51919, .F. ) ;
#84428 = CARTESIAN_POINT ( 'NONE',  ( 22.81628187352647785, 16.41530133659708923, 3.434112377981063169 ) ) ;
#84429 = CARTESIAN_POINT ( 'NONE',  ( 12.91533473730992121, 24.52201867748816966, 10.88017736071110164 ) ) ;
#84430 = CARTESIAN_POINT ( 'NONE',  ( 15.44008868035555260, 54.73035201082150536, 9.422509992056143702 ) ) ;
#84431 = ORIENTED_EDGE ( 'NONE', *, *, #77720, .T. ) ;
#84432 = TOROIDAL_SURFACE ( 'NONE', #41344, 1.499999999999996669, 0.5000000000000000000 ) ;
#84433 = CARTESIAN_POINT ( 'NONE',  ( 5.076628168052704559, 5.175597817667451750, -8.527530157486179263 ) ) ;
#84434 = CARTESIAN_POINT ( 'NONE',  ( 5.076628168052703671, 51.84226448433412315, 8.527530157486179263 ) ) ;
#84435 = CARTESIAN_POINT ( 'NONE',  ( 19.84674366389459621, 33.50893115100078745, 7.409399052514197653E-17 ) ) ;
#84436 = CARTESIAN_POINT ( 'NONE',  ( -1.099225684535947600, 63.70696800326376774, -6.408140936763238038 ) ) ;
#84437 = CARTESIAN_POINT ( 'NONE',  ( 5.129999999999995453, 43.00000000000000711, 6.500000000000000888 ) ) ;
#84438 = CARTESIAN_POINT ( 'NONE',  ( -2.999999999999999556, 21.83999999999999986, 0.000000000000000000 ) ) ;
#84439 = ADVANCED_FACE ( 'NONE', ( #15936 ), #37289, .T. ) ;
#84441 = CARTESIAN_POINT ( 'NONE',  ( 0.2751277870542911952, 33.21833443783938122, 6.499999999999992006 ) ) ;
#84440 = CARTESIAN_POINT ( 'NONE',  ( 0.1532563361054083140, 11.00893115100078568, 1.131784320476157264E-15 ) ) ;
#84442 = LINE ( 'NONE', #37469, #63274 ) ;
#84444 = EDGE_LOOP ( 'NONE', ( #91083, #46913, #30247, #35307 ) ) ;
#84443 = CARTESIAN_POINT ( 'NONE',  ( 19.84674366389459621, 48.50893115100078745, 7.409399052514197653E-17 ) ) ;
#84445 = DIRECTION ( 'NONE',  ( 0.9636304532086229502, 0.000000000000000000, -0.2672383760782571227 ) ) ;
#84446 = CARTESIAN_POINT ( 'NONE',  ( 3.591859063236763294, 13.29030133659708746, -11.09922568453595026 ) ) ;
#84447 = CARTESIAN_POINT ( 'NONE',  ( 20.88017736071110164, 55.35535201082149825, 2.915334737309930979 ) ) ;
#84448 = CARTESIAN_POINT ( 'NONE',  ( 13.79529636645030344, 38.26208216824729647, 14.16423886937410614 ) ) ;
#84449 = CARTESIAN_POINT ( 'NONE',  ( 20.00000000000138911, 90.62861641165379467, 5.317662825071818311 ) ) ;
#84450 = CARTESIAN_POINT ( 'NONE',  ( 2.917880565312948704, 47.63708216824730357, 12.26659068614894643 ) ) ;
#84451 = CARTESIAN_POINT ( 'NONE',  ( 20.36894250292379382, 53.67874883491397497, 10.36894250292379205 ) ) ;
#84452 = CARTESIAN_POINT ( 'NONE',  ( 24.16423886937410614, 29.51208216824729647, -3.795296366450302550 ) ) ;
#84454 = DIRECTION ( 'NONE',  ( -1.000000000000000000, 0.000000000000000000, -0.000000000000000000 ) ) ;
#84453 = CARTESIAN_POINT ( 'NONE',  ( -0.3689425029237881626, 27.42874883491397142, 10.36894250292379027 ) ) ;
#84455 = CARTESIAN_POINT ( 'NONE',  ( -0.03743638938522369369, 29.25197528031018379, -6.399506433553970197 ) ) ;
#84456 = CIRCLE ( 'NONE', #86025, 15.00000000000000000 ) ;
#84458 = CARTESIAN_POINT ( 'NONE',  ( 12.63842701281683034, 37.46726448433411605, 9.846743663894596210 ) ) ;
#84457 = PLANE ( 'NONE',  #14979 ) ;
#84459 = CARTESIAN_POINT ( 'NONE',  ( 17.96484262340118221, 24.93868534415484461, 7.964842623401181321 ) ) ;
#84460 = DIRECTION ( 'NONE',  ( 0.9366721892484018985, 0.000000000000000000, -0.3502073812594559410 ) ) ;
#84461 = CARTESIAN_POINT ( 'NONE',  ( 12.63842701281683034, 57.46726448433411605, 9.846743663894596210 ) ) ;
#84462 = DIRECTION ( 'NONE',  ( -0.000000000000000000, -1.000000000000000000, -0.000000000000000000 ) ) ;
#84463 = CARTESIAN_POINT ( 'NONE',  ( 2.791683348922237240, 45.38393115100079456, -7.208316651077763204 ) ) ;
#84464 = CARTESIAN_POINT ( 'NONE',  ( -2.816281873526473856, 54.12363466993041783, 9.499525473075851096E-16 ) ) ;
#84465 = CARTESIAN_POINT ( 'NONE',  ( 12.26659068614894821, -11.11291783175269465, 7.082119434687044190 ) ) ;
#84466 = CARTESIAN_POINT ( 'NONE',  ( 2.791683348922237240, 45.38393115100079456, -7.208316651077763204 ) ) ;
#84467 = CARTESIAN_POINT ( 'NONE',  ( 7.361572987183170547, 57.05059781766744464, 9.846743663894590881 ) ) ;
#84468 = CARTESIAN_POINT ( 'NONE',  ( -4.164238869374099039, 41.80374883491397497, 8.674139862899312516E-16 ) ) ;
#84469 = EDGE_CURVE ( 'NONE', #80952, #66014, #1937, .T. ) ;
#84470 = ORIENTED_EDGE ( 'NONE', *, *, #63163, .T. ) ;
#84471 = CARTESIAN_POINT ( 'NONE',  ( -4.164238869374099039, 16.80374883491396787, 8.674139862899312516E-16 ) ) ;
#84472 = CARTESIAN_POINT ( 'NONE',  ( -0.8801773607110991993, 57.85535201082149825, -2.915334737309923874 ) ) ;
#84473 = CARTESIAN_POINT ( 'NONE',  ( 1.796787675079331459, 0.2301501525782880253, -14.83218748772976525 ) ) ;
#84474 = CARTESIAN_POINT ( 'NONE',  ( 10.00000000000000000, 6.813685344154838397, -10.88017736071110342 ) ) ;
#84475 = CARTESIAN_POINT ( 'NONE',  ( 6.565887622018943937, 18.08196800326375708, -12.81628187352647608 ) ) ;
#84476 = CARTESIAN_POINT ( 'NONE',  ( -7.750000000000000000, 41.24999999999999289, -6.250000000000000000 ) ) ;
#84477 = CARTESIAN_POINT ( 'NONE',  ( -0.8801773607111009756, 68.06368534415484817, 1.068504757029289695E-15 ) ) ;
#84478 = CARTESIAN_POINT ( 'NONE',  ( 21.92686044187657046, 42.39664270246084499, -3.195792623639524432 ) ) ;
#84479 = DIRECTION ( 'NONE',  ( 0.9762960071199360268, 0.000000000000000000, -0.2164396139380907191 ) ) ;
#84480 = CARTESIAN_POINT ( 'NONE',  ( 22.26659068614894466, 63.88708216824730357, 7.082119434687054849 ) ) ;
#84481 = LINE ( 'NONE', #70460, #4911 ) ;
#84482 = CARTESIAN_POINT ( 'NONE',  ( -0.8801773607111008646, 33.27201867748817676, 2.915334737309923430 ) ) ;
#84483 = CARTESIAN_POINT ( 'NONE',  ( 17.96484262340118221, 24.93868534415484461, 7.964842623401181321 ) ) ;
#84484 = CARTESIAN_POINT ( 'NONE',  ( 19.84674366389459266, 58.71726448433411605, -2.638427012816827677 ) ) ;
#84485 = CARTESIAN_POINT ( 'NONE',  ( 19.84674366389459266, 53.71726448433411605, -2.638427012816827677 ) ) ;
#84486 = CARTESIAN_POINT ( 'NONE',  ( 22.81628187352647785, 46.62363466993041783, 6.195893100308588602E-16 ) ) ;
#84487 = LINE ( 'NONE', #77455, #88679 ) ;
#84488 = EDGE_LOOP ( 'NONE', ( #35580, #70188, #23789, #13320 ) ) ;
#84489 = CARTESIAN_POINT ( 'NONE',  ( 20.88017736071110875, 15.77201867748817143, -2.915334737309920765 ) ) ;
#84490 = CARTESIAN_POINT ( 'NONE',  ( -1.099225684535947600, 14.54030133659708568, 6.408140936763237150 ) ) ;
#84491 = CARTESIAN_POINT ( 'NONE',  ( 13.03370038005726705, -0.03417435944610275333, -9.273621236547697322 ) ) ;
#84492 = AXIS2_PLACEMENT_3D ( 'NONE', #37224, #67709, #98222 ) ;
#84493 = CARTESIAN_POINT ( 'NONE',  ( 10.00000000000000000, 44.75893115100078745, -9.846743663894594434 ) ) ;
#84494 = CARTESIAN_POINT ( 'NONE',  ( 4.559911319644449179, 47.23035201082150536, -9.422509992056141925 ) ) ;
#84495 = CARTESIAN_POINT ( 'NONE',  ( -2.816281873526473856, 24.12363466993042138, 9.499525473075851096E-16 ) ) ;
#84497 = CARTESIAN_POINT ( 'NONE',  ( 13.07661834287487501, -3.129363223631011419E-15, -6.550615570651680208 ) ) ;
#84496 = CARTESIAN_POINT ( 'NONE',  ( 2.035157376598824452, 68.68868534415484817, 7.964842623401179544 ) ) ;
#84498 = DIRECTION ( 'NONE',  ( 0.000000000000000000, 0.000000000000000000, 1.000000000000000000 ) ) ;
#84499 = CARTESIAN_POINT ( 'NONE',  ( -2.816281873526471635, 58.91530133659707502, -3.434112377981056508 ) ) ;
#84500 = VERTEX_POINT ( 'NONE', #54408 ) ;
#84501 = PLANE ( 'NONE',  #64405 ) ;
#84502 = CARTESIAN_POINT ( 'NONE',  ( 17.96484262340118221, 46.18868534415484106, -7.964842623401177768 ) ) ;
#84504 = CARTESIAN_POINT ( 'NONE',  ( 24.16423886937409904, 14.09541550158063217, 3.795296366450317205 ) ) ;
#84503 = CARTESIAN_POINT ( 'NONE',  ( 3.591859063236761518, 44.95696800326376064, 11.09922568453594849 ) ) ;
#84505 = CARTESIAN_POINT ( 'NONE',  ( 7.361572987183170547, 7.050597817667451750, 9.846743663894590881 ) ) ;
#84506 = DIRECTION ( 'NONE',  ( -0.000000000000000000, -1.000000000000000000, -0.000000000000000000 ) ) ;
#84507 = ADVANCED_FACE ( 'NONE', ( #93399 ), #83934, .T. ) ;
#84508 = CARTESIAN_POINT ( 'NONE',  ( 1.472469842513823179, 20.59226448433411960, -4.923371831947296329 ) ) ;
#84509 = DIRECTION ( 'NONE',  ( 0.000000000000000000, 0.000000000000000000, 1.000000000000000000 ) ) ;
#84510 = CARTESIAN_POINT ( 'NONE',  ( 6.204703633549690345, 40.76208216824731778, -14.16423886937410259 ) ) ;
#84511 = CARTESIAN_POINT ( 'NONE',  ( 7.084665262690076126, 2.022018677488170990, -10.88017736071110164 ) ) ;
#84512 = EDGE_CURVE ( 'NONE', #7091, #87189, #29268, .T. ) ;
#84513 = VECTOR ( 'NONE', #86257, 1000.000000000000000 ) ;
#84514 = CARTESIAN_POINT ( 'NONE',  ( 15.44008868035555793, 6.397018677488170546, -9.422509992056140149 ) ) ;
#84515 = CARTESIAN_POINT ( 'NONE',  ( -7.121448108906508700, -73.25984652122873797, -3.750000000000000888 ) ) ;
#84516 = ORIENTED_EDGE ( 'NONE', *, *, #58859, .T. ) ;
#84517 = ORIENTED_EDGE ( 'NONE', *, *, #72493, .F. ) ;
#84518 = CARTESIAN_POINT ( 'NONE',  ( 2.035157376598824452, 8.688685344154839285, 7.964842623401179544 ) ) ;
#84519 = CARTESIAN_POINT ( 'NONE',  ( -0.8801773607111009756, 8.063685344154837509, 1.068504757029289695E-15 ) ) ;
#84520 = CARTESIAN_POINT ( 'NONE',  ( 12.63842701281683922, 44.55059781766745175, -9.846743663894590881 ) ) ;
#84521 = CARTESIAN_POINT ( 'NONE',  ( 16.40814093676324603, 32.45696800326375353, -11.09922568453594671 ) ) ;
#84522 = CYLINDRICAL_SURFACE ( 'NONE', #10804, 0.5000000000000004441 ) ;
#84524 = CARTESIAN_POINT ( 'NONE',  ( 22.26659068614894466, 8.887082168247300018, 7.082119434687054849 ) ) ;
#84523 = CARTESIAN_POINT ( 'NONE',  ( 0.2751277870542969683, 2.282175860852373894, -6.500000000000000888 ) ) ;
#84525 = CARTESIAN_POINT ( 'NONE',  ( 20.88017736071110875, 30.77201867748816966, -2.915334737309920765 ) ) ;
#84526 = CARTESIAN_POINT ( 'NONE',  ( -0.8801773607110991993, 7.855352010821506248, -2.915334737309923874 ) ) ;
#84527 = CARTESIAN_POINT ( 'NONE',  ( 2.791683348922240793, 36.63393115100078035, 7.208316651077764092 ) ) ;
#84528 = CARTESIAN_POINT ( 'NONE',  ( -25.69000000000001194, 93.50000000000000000, -10.09898361729590199 ) ) ;
#84529 = CARTESIAN_POINT ( 'NONE',  ( 17.20831665107776587, 27.88393115100078390, 7.208316651077764980 ) ) ;
#84530 = DIRECTION ( 'NONE',  ( -0.000000000000000000, 1.000000000000000000, -0.000000000000000000 ) ) ;
#84531 = CARTESIAN_POINT ( 'NONE',  ( 3.434112377981060948, -39.41803199673623936, 12.81628187352647430 ) ) ;
#84532 = VERTEX_POINT ( 'NONE', #84438 ) ;
#84533 = AXIS2_PLACEMENT_3D ( 'NONE', #28487, #36488, #96511 ) ;
#84534 = PRESENTATION_STYLE_ASSIGNMENT (( #8534 ) ) ;
#84535 = VERTEX_POINT ( 'NONE', #46426 ) ;
#84536 = CARTESIAN_POINT ( 'NONE',  ( 19.84674366389459266, 53.71726448433411605, -2.638427012816827677 ) ) ;
#84538 = CARTESIAN_POINT ( 'NONE',  ( 2.035157376598822676, 42.43868534415483396, -7.964842623401177768 ) ) ;
#84537 = CARTESIAN_POINT ( 'NONE',  ( 17.96484262340118221, 36.18868534415484106, -7.964842623401177768 ) ) ;
#84540 = CARTESIAN_POINT ( 'NONE',  ( -2.816281873526473856, 29.33196800326376064, 3.434112377981055619 ) ) ;
#84539 = CARTESIAN_POINT ( 'NONE',  ( 10.00000000000000178, 4.313685344154837509, 10.88017736071110342 ) ) ;
#84541 = CARTESIAN_POINT ( 'NONE',  ( 20.36894250292379382, 18.67874883491397142, 10.36894250292379205 ) ) ;
#84542 = CARTESIAN_POINT ( 'NONE',  ( 0.6178305044545818747, 43.49863466993042493, -9.382169495545419124 ) ) ;
#84543 = ORIENTED_EDGE ( 'NONE', *, *, #50576, .T. ) ;
#84544 = CARTESIAN_POINT ( 'NONE',  ( 1.472469842513823179, 51.42559781766745886, 4.923371831947296329 ) ) ;
#84545 = CARTESIAN_POINT ( 'NONE',  ( 20.88017736071110519, 50.56368534415484106, 2.639326808657452039E-16 ) ) ;
#84546 = CARTESIAN_POINT ( 'NONE',  ( 0.5774900079438607392, 18.48035201082150536, 5.440088680355550821 ) ) ;
#84547 = ORIENTED_EDGE ( 'NONE', *, *, #72228, .T. ) ;
#84548 = CARTESIAN_POINT ( 'NONE',  ( 20.88017736071110519, 20.56368534415484106, 2.639326808657452039E-16 ) ) ;
#84549 = ORIENTED_EDGE ( 'NONE', *, *, #83264, .F. ) ;
#84550 = CARTESIAN_POINT ( 'NONE',  ( 2.035157376598822676, 57.43868534415484106, -7.964842623401177768 ) ) ;
#84551 = CYLINDRICAL_SURFACE ( 'NONE', #72637, 11.92686044187656513 ) ;
#84552 = CARTESIAN_POINT ( 'NONE',  ( 20.88017736071110519, 60.56368534415484106, 2.639326808657452039E-16 ) ) ;
#84553 = CARTESIAN_POINT ( 'NONE',  ( 2.791683348922237240, 5.383931151000785675, -7.208316651077763204 ) ) ;
#84554 = CARTESIAN_POINT ( 'NONE',  ( -0.8801773607111008646, 63.27201867748817676, 2.915334737309923430 ) ) ;
#84555 = CARTESIAN_POINT ( 'NONE',  ( -4.265659168453410643, 0.04922511925147263212, 14.12268572233449149 ) ) ;
#84556 = EDGE_CURVE ( 'NONE', #49843, #31069, #23939, .T. ) ;
#84557 = CARTESIAN_POINT ( 'NONE',  ( -46.75138744620058873, 100.8579332310653598, 9.074091037931069081 ) ) ;
#84558 = CARTESIAN_POINT ( 'NONE',  ( 12.63842701281683034, 2.467264484334118269, 9.846743663894596210 ) ) ;
#84559 = CARTESIAN_POINT ( 'NONE',  ( 0.1532563361054083140, 46.00893115100079456, 1.131784320476157264E-15 ) ) ;
#84560 = ORIENTED_EDGE ( 'NONE', *, *, #3280, .T. ) ;
#84561 = EDGE_LOOP ( 'NONE', ( #54719, #82838, #81993, #82168 ) ) ;
#84562 = CYLINDRICAL_SURFACE ( 'NONE', #36232, 0.5000000000000004441 ) ;
#84563 = DIRECTION ( 'NONE',  ( 0.000000000000000000, -1.000000000000000000, -0.000000000000000000 ) ) ;
#84564 = CARTESIAN_POINT ( 'NONE',  ( 2.603489959281591659, 10.43575266056827644, -6.500000000000006217 ) ) ;
#84565 = AXIS2_PLACEMENT_3D ( 'NONE', #82375, #28875, #59377 ) ;
#84566 = CARTESIAN_POINT ( 'NONE',  ( 17.08211943468705130, 23.47041550158063572, 12.26659068614894998 ) ) ;
#84567 = CYLINDRICAL_SURFACE ( 'NONE', #20307, 11.92686044187656513 ) ;
#84569 = CARTESIAN_POINT ( 'NONE',  ( -0.8801773607111009756, 58.06368534415484106, 1.068504757029289695E-15 ) ) ;
#84568 = FACE_OUTER_BOUND ( 'NONE', #30758, .T. ) ;
#84570 = CARTESIAN_POINT ( 'NONE',  ( 19.42250999205614548, 20.98035201082150891, -5.440088680355545492 ) ) ;
#84571 = CARTESIAN_POINT ( 'NONE',  ( 0.1532563361054083140, 66.00893115100079456, 1.131784320476157264E-15 ) ) ;
#84572 = ORIENTED_EDGE ( 'NONE', *, *, #76963, .F. ) ;
#84573 = CARTESIAN_POINT ( 'NONE',  ( 2.791683348922240793, 6.633931151000785675, 7.208316651077764092 ) ) ;
#84574 = CARTESIAN_POINT ( 'NONE',  ( 18.52753015748618282, 3.925597817667451306, -4.923371831947291888 ) ) ;
#84575 = CARTESIAN_POINT ( 'NONE',  ( 22.81628187352647785, 31.41530133659709279, 3.434112377981063169 ) ) ;
#84576 = CARTESIAN_POINT ( 'NONE',  ( 0.1532563361054100626, 25.80059781766744820, -2.638427012816831230 ) ) ;
#84577 = AXIS2_PLACEMENT_3D ( 'NONE', #7025, #62464, #83018 ) ;
#84578 = DIRECTION ( 'NONE',  ( 0.000000000000000000, 1.000000000000000000, 0.000000000000000000 ) ) ;
#84579 = CARTESIAN_POINT ( 'NONE',  ( 10.00000000000000178, 10.37363466993041961, 12.81628187352647608 ) ) ;
#84580 = DIRECTION ( 'NONE',  ( 1.000000000000000000, 6.938893903907221278E-15, 0.000000000000000000 ) ) ;
#84581 = CARTESIAN_POINT ( 'NONE',  ( 0.1532563361054100626, 5.800597817667452638, -2.638427012816831230 ) ) ;
#84582 = EDGE_CURVE ( 'NONE', #55236, #20156, #34034, .T. ) ;
#84583 = ORIENTED_EDGE ( 'NONE', *, *, #20763, .F. ) ;
#84584 = ORIENTED_EDGE ( 'NONE', *, *, #78452, .F. ) ;
#84585 = ORIENTED_EDGE ( 'NONE', *, *, #13094, .T. ) ;
#84586 = CARTESIAN_POINT ( 'NONE',  ( 20.88017736071110875, 20.77201867748816611, -2.915334737309920765 ) ) ;
#84587 = CARTESIAN_POINT ( 'NONE',  ( -2.266590686148945544, 16.38708216824730357, -7.082119434687050408 ) ) ;
#84588 = CARTESIAN_POINT ( 'NONE',  ( 18.52753015748618282, 38.92559781766745175, -4.923371831947291888 ) ) ;
#84589 = CARTESIAN_POINT ( 'NONE',  ( 0.1532563361054100626, 0.8005978176674514168, -2.638427012816831230 ) ) ;
#84591 = CARTESIAN_POINT ( 'NONE',  ( 9.402796353261127393, 0.5000000000000004441, -11.68706210897757103 ) ) ;
#84590 = CARTESIAN_POINT ( 'NONE',  ( 21.09922568453594849, 56.20696800326375353, 6.408140936763242479 ) ) ;
#84592 = CARTESIAN_POINT ( 'NONE',  ( 4.559911319644449179, 28.89701867748817321, 9.422509992056141925 ) ) ;
#84593 = EDGE_CURVE ( 'NONE', #61703, #67320, #31408, .T. ) ;
#84594 = PLANE ( 'NONE',  #59778 ) ;
#84595 = VECTOR ( 'NONE', #90836, 1000.000000000000114 ) ;
#84596 = CARTESIAN_POINT ( 'NONE',  ( 13.43411237798105340, 15.58196800326374998, 12.81628187352647963 ) ) ;
#84597 = CARTESIAN_POINT ( 'NONE',  ( 16.40814093676323893, 10.79030133659708923, 11.09922568453595026 ) ) ;
#84598 = CARTESIAN_POINT ( 'NONE',  ( 18.52753015748617571, 43.09226448433412315, 4.923371831947298993 ) ) ;
#84599 = CARTESIAN_POINT ( 'NONE',  ( 10.88017736071109987, -4.227981322511823237, -2.915334737309928315 ) ) ;
#84600 = CARTESIAN_POINT ( 'NONE',  ( 0.6178305044545838731, 54.74863466993042493, 9.382169495545420901 ) ) ;
#84602 = DIRECTION ( 'NONE',  ( 5.818595309480553908E-17, 1.000000000000000000, -0.000000000000000000 ) ) ;
#84601 = CARTESIAN_POINT ( 'NONE',  ( -0.8801773607111009756, 48.06368534415484817, 1.068504757029289695E-15 ) ) ;
#84603 = CARTESIAN_POINT ( 'NONE',  ( 8.375939845167756914, -0.03417435944610275333, -11.52849216984298941 ) ) ;
#84604 = CARTESIAN_POINT ( 'NONE',  ( 15.44008868035555260, 59.73035201082151247, 9.422509992056143702 ) ) ;
#84605 = CARTESIAN_POINT ( 'NONE',  ( 12.91533473730992121, 44.52201867748816966, 10.88017736071110164 ) ) ;
#84606 = CARTESIAN_POINT ( 'NONE',  ( 0.000000000000000000, 15.00000000000000000, 0.000000000000000000 ) ) ;
#84607 = CARTESIAN_POINT ( 'NONE',  ( 7.084665262690076126, 64.10535201082150536, 10.88017736071109987 ) ) ;
#84608 = CARTESIAN_POINT ( 'NONE',  ( 12.63842701281683922, 49.55059781766744464, -9.846743663894590881 ) ) ;
#84610 = FACE_OUTER_BOUND ( 'NONE', #61063, .T. ) ;
#84609 = CARTESIAN_POINT ( 'NONE',  ( -0.8801773607111008646, 3.272018677488171434, 2.915334737309923430 ) ) ;
#84611 = CARTESIAN_POINT ( 'NONE',  ( 13.43411237798106583, 22.66530133659708923, -12.81628187352647252 ) ) ;
#84612 = ORIENTED_EDGE ( 'NONE', *, *, #73376, .T. ) ;
#84613 = CARTESIAN_POINT ( 'NONE',  ( 7.084665262690076126, 32.02201867748816966, -10.88017736071110164 ) ) ;
#84614 = CARTESIAN_POINT ( 'NONE',  ( -2.816281873526473856, 4.123634669930420493, 9.499525473075851096E-16 ) ) ;
#84615 = CARTESIAN_POINT ( 'NONE',  ( 12.91533473730993009, 16.60535201082150891, -10.88017736071109987 ) ) ;
#84616 = CARTESIAN_POINT ( 'NONE',  ( -0.8801773607111008646, 33.27201867748817676, 2.915334737309923430 ) ) ;
#84617 = CARTESIAN_POINT ( 'NONE',  ( 2.917880565312948704, 37.63708216824731068, 12.26659068614894643 ) ) ;
#84618 = CARTESIAN_POINT ( 'NONE',  ( 7.361572987183169658, 24.96726448433412315, -9.846743663894592657 ) ) ;
#84619 = CARTESIAN_POINT ( 'NONE',  ( 19.42250999205614548, 55.98035201082150536, -5.440088680355545492 ) ) ;
#84620 = CARTESIAN_POINT ( 'NONE',  ( 0.6076426042653103599, 32.37576471608601025, -6.499999999999992006 ) ) ;
#84621 = CARTESIAN_POINT ( 'NONE',  ( -0.3689425029237898834, 6.178748834913968757, -10.36894250292378850 ) ) ;
#84622 = ADVANCED_FACE ( 'NONE', ( #91927 ), #85413, .T. ) ;
#84623 = PRESENTATION_STYLE_ASSIGNMENT (( #69619 ) ) ;
#84624 = CARTESIAN_POINT ( 'NONE',  ( 18.52753015748618282, 63.92559781766745886, -4.923371831947291888 ) ) ;
#84625 = EDGE_LOOP ( 'NONE', ( #1297, #11381, #16510, #21317, #88719, #57924 ) ) ;
#84626 = ORIENTED_EDGE ( 'NONE', *, *, #21144, .F. ) ;
#84627 = CARTESIAN_POINT ( 'NONE',  ( 24.16423886937409904, 34.09541550158064638, 3.795296366450317205 ) ) ;
#84628 = CARTESIAN_POINT ( 'NONE',  ( 17.08211943468705130, 43.47041550158063927, 12.26659068614894998 ) ) ;
#84629 = CARTESIAN_POINT ( 'NONE',  ( 1.472469842513823179, 1.425597817667451528, 4.923371831947296329 ) ) ;
#84630 = CARTESIAN_POINT ( 'NONE',  ( 16.40814093676324603, 7.456968003263754419, -11.09922568453594671 ) ) ;
#84631 = CARTESIAN_POINT ( 'NONE',  ( 10.00000000000000178, 62.25893115100078745, 9.846743663894594434 ) ) ;
#84632 = CARTESIAN_POINT ( 'NONE',  ( -11.62541523589044168, -75.76371818141878123, 3.999999999998198330 ) ) ;
#84634 = CARTESIAN_POINT ( 'NONE',  ( 6.565887622018943937, 13.08196800326374998, -12.81628187352647608 ) ) ;
#84633 = CARTESIAN_POINT ( 'NONE',  ( 20.88017736071110519, 55.56368534415484817, 2.639326808657452039E-16 ) ) ;
#84635 = CARTESIAN_POINT ( 'NONE',  ( 13.79529636645030344, 28.26208216824729647, 14.16423886937410614 ) ) ;
#84636 = CARTESIAN_POINT ( 'NONE',  ( 17.96484262340118221, 34.93868534415482685, 7.964842623401181321 ) ) ;
#84637 = DIRECTION ( 'NONE',  ( 0.5547001962252290364, 0.8320502943378437211, 0.000000000000000000 ) ) ;
#84638 = CARTESIAN_POINT ( 'NONE',  ( 19.42250999205614193, 60.14701867748817676, 5.440088680355555262 ) ) ;
#84639 = AXIS2_PLACEMENT_3D ( 'NONE', #32578, #25110, #15142 ) ;
#84640 = CARTESIAN_POINT ( 'NONE',  ( 2.638427012816829897, -5.449402182332544697, -9.846743663894592657 ) ) ;
#84641 = VERTEX_POINT ( 'NONE', #38444 ) ;
#84642 = CARTESIAN_POINT ( 'NONE',  ( -9.898881779040587858, -0.03417435944610275333, -10.25059215482589714 ) ) ;
#84643 = ORIENTED_EDGE ( 'NONE', *, *, #54416, .F. ) ;
#84644 = AXIS2_PLACEMENT_3D ( 'NONE', #73328, #88340, #20835 ) ;
#84645 = ORIENTED_EDGE ( 'NONE', *, *, #63155, .T. ) ;
#84646 = CARTESIAN_POINT ( 'NONE',  ( -0.3689425029237898834, 6.178748834913968757, -10.36894250292378850 ) ) ;
#84648 = CARTESIAN_POINT ( 'NONE',  ( 22.26659068614894466, 58.88708216824729647, 7.082119434687054849 ) ) ;
#84647 = CARTESIAN_POINT ( 'NONE',  ( 24.16423886937409904, 59.09541550158063217, 3.795296366450317205 ) ) ;
#84650 = CARTESIAN_POINT ( 'NONE',  ( 19.84674366389459266, 63.71726448433412315, -2.638427012816827677 ) ) ;
#84649 = CARTESIAN_POINT ( 'NONE',  ( 19.84674366389459266, 33.30059781766744464, 2.638427012816836559 ) ) ;
#84651 = CARTESIAN_POINT ( 'NONE',  ( -13.61464873478165138, 14.49999999999999112, -6.296136897218031159 ) ) ;
#84652 = CARTESIAN_POINT ( 'NONE',  ( -2.816281873526473856, 4.123634669930420493, 9.499525473075851096E-16 ) ) ;
#84653 = VERTEX_POINT ( 'NONE', #22961 ) ;
#84654 = CARTESIAN_POINT ( 'NONE',  ( 10.00000000000000000, 50.55374883491396787, -14.16423886937410082 ) ) ;
#84655 = VERTEX_POINT ( 'NONE', #23453 ) ;
#84656 = CARTESIAN_POINT ( 'NONE',  ( -4.164238869374099039, 41.80374883491397497, 8.674139862899312516E-16 ) ) ;
#84657 = ORIENTED_EDGE ( 'NONE', *, *, #71364, .F. ) ;
#84658 = CARTESIAN_POINT ( 'NONE',  ( 22.81628187352648496, 51.83196800326376064, -3.434112377981050290 ) ) ;
#84659 = VECTOR ( 'NONE', #88253, 1000.000000000000000 ) ;
#84660 = CARTESIAN_POINT ( 'NONE',  ( -0.8801773607110991993, 22.85535201082150181, -2.915334737309923874 ) ) ;
#84661 = CARTESIAN_POINT ( 'NONE',  ( 12.63842701281683034, 52.46726448433413026, 9.846743663894596210 ) ) ;
#84662 = CARTESIAN_POINT ( 'NONE',  ( 4.559911319644449179, 28.89701867748817321, 9.422509992056141925 ) ) ;
#84663 = CARTESIAN_POINT ( 'NONE',  ( 10.27191093752554529, 15.00000000000000888, 10.41278984915632400 ) ) ;
#84664 = CARTESIAN_POINT ( 'NONE',  ( 2.791683348922240793, 56.63393115100078035, 7.208316651077764092 ) ) ;
#84665 = FACE_OUTER_BOUND ( 'NONE', #2678, .T. ) ;
#84666 = ADVANCED_FACE ( 'NONE', ( #84920 ), #45436, .F. ) ;
#84668 = ORIENTED_EDGE ( 'NONE', *, *, #29623, .T. ) ;
#84667 = CYLINDRICAL_SURFACE ( 'NONE', #34484, 15.00000000000000000 ) ;
#84669 = CARTESIAN_POINT ( 'NONE',  ( 0.000000000000000000, 0.5000000000000004441, 0.000000000000000000 ) ) ;
#84670 = CARTESIAN_POINT ( 'NONE',  ( 0.1532563361054100626, 0.8005978176674514168, -2.638427012816831230 ) ) ;
#84671 = CARTESIAN_POINT ( 'NONE',  ( 15.00000000000000000, 77.07179676972447169, 4.000000000000000000 ) ) ;
#84672 = ORIENTED_EDGE ( 'NONE', *, *, #42248, .F. ) ;
#84673 = EDGE_CURVE ( 'NONE', #36587, #96742, #93893, .T. ) ;
#84674 = CARTESIAN_POINT ( 'NONE',  ( 8.650320195874050100, -1.048895414467672094, 4.000000000000000000 ) ) ;
#84675 = CARTESIAN_POINT ( 'NONE',  ( 19.84674366389459621, 28.50893115100078745, 7.409399052514197653E-17 ) ) ;
#84676 = EDGE_CURVE ( 'NONE', #20694, #9403, #37797, .T. ) ;
#84677 = CARTESIAN_POINT ( 'NONE',  ( 17.99999999999999645, 99.99999999999998579, 8.000000000000000000 ) ) ;
#84678 = FACE_OUTER_BOUND ( 'NONE', #78481, .T. ) ;
#84679 = DIRECTION ( 'NONE',  ( -0.000000000000000000, -0.000000000000000000, -1.000000000000000000 ) ) ;
#84680 = VERTEX_POINT ( 'NONE', #17905 ) ;
#84681 = DIRECTION ( 'NONE',  ( -0.000000000000000000, -1.000000000000000000, -0.000000000000000000 ) ) ;
#84682 = CARTESIAN_POINT ( 'NONE',  ( 19.84674366389459266, 53.71726448433411605, -2.638427012816827677 ) ) ;
#84683 = CARTESIAN_POINT ( 'NONE',  ( 22.26659068614895176, 39.72041550158063217, -7.082119434687042414 ) ) ;
#84684 = CARTESIAN_POINT ( 'NONE',  ( 18.52753015748617571, 58.09226448433411605, 4.923371831947298993 ) ) ;
#84685 =( NAMED_UNIT ( * ) SI_UNIT ( $, .STERADIAN. ) SOLID_ANGLE_UNIT ( ) );
#84686 = CARTESIAN_POINT ( 'NONE',  ( 7.361572987183170547, 17.05059781766745530, 9.846743663894590881 ) ) ;
#84687 = CARTESIAN_POINT ( 'NONE',  ( -2.816281873526473856, 49.33196800326374643, 3.434112377981055619 ) ) ;
#84688 = CARTESIAN_POINT ( 'NONE',  ( -4.164238869374099039, 1.803748834913967647, 8.674139862899312516E-16 ) ) ;
#84689 = CARTESIAN_POINT ( 'NONE',  ( 3.591859063236763294, -1.709698663402913210, -11.09922568453595026 ) ) ;
#84690 = CARTESIAN_POINT ( 'NONE',  ( 10.00000000000000178, 59.31368534415484106, 10.88017736071110342 ) ) ;
#84691 = CARTESIAN_POINT ( 'NONE',  ( 19.84674366389459621, 43.50893115100078745, 7.409399052514197653E-17 ) ) ;
#84692 =( BOUNDED_SURFACE ( )  B_SPLINE_SURFACE ( 1, 2, ( 
 ( #14413, #5918, #7413, #44883, #75385, #6903, #96940, #29880, #81901, #44396, #22408, #37909, #68397, #14913, #60382, #90880, #13410, #21414, #20923, #74896, #43896, #89407, #52883, #83393, #66905, #51909, #45383, #83885, #98918, #91377, #29387, #30373, #97424, #74395, #60877, #22905, #6394, #7897, #53375, #15414, #45896, #28890, #36909, #59888, #82394, #76382, #66408, #36412, #59395, #28414, #58909, #89898, #13918, #67401, #70370, #92852, #8381, #32346, #17852, #24380, #39864, #78344, #86349, #1888, #423, #38889, #69377, #61861, #16378, #70865, #2381, #85859, #54847, #48338, #17371, #78841, #23402, #8864, #93842, #23892, #62849, #30874, #899, #31361, #92366, #38392, #68895, #55354, #61370, #62347, #39380, #31850, #93347, #25369, #55854, #91880, #53886, #69875, #84392, #24872, #1395, #85361, #46861, #32835, #54358, #15891, #47841, #16873, #47348, #77353, #63337, #84869, #77850, #46376, #9360, #9866, #76865, #40364, #71831, #3340, #79334, #50808, #26324, #88800, #34804, #56346, #12307, #79821, #73299, #57309, #10843, #57801, #64309, #65293, #34298, #64796, #48823, #19806, #95314, #19322, #49806, #40851, #42321, #94329, #87320, #95820, #50296, #80809, #88308, #87801, #27300, #25849, #94820, #63818, #18837, #86841, #33323, #42815, #4334, #41364, #56821, #4823, #27797, #35297, #65790, #41842, #96324, #33802, #18345, #58282, #20310, #49317, #10352, #26816, #80314, #71355, #11323, #72308, #3839, #11814, #2874, #72795, #51294, #96820, #13794, #73788, #12794, #36795, #21298, #14300, #67289, #81780, #75276, #60761, #97817, #82780, #22295, #30258, #44771, #43294, #13295, #43781, #5802, #59282, #14802, #45274, #29764, #29278, #91261, #60272, #22787, #66285, #51790, #37791, #66791, #6787, #5319, #74274, #36294, #97311, #81299, #35798, #98310, #28296, #6293, #82277, #74784, #37301, #68288, #98809, #58789, #89296, #44280, #59774, #89781, #75769, #28784, #90267, #20807, #52282, #21801, #67788, #90771, #52769, #83277, #7290, #93723, #69269, #32720, #77734, #306, #55229, #23779, #17256, #1285, #53763, #1769, #8270, #9245, #77242, #8749, #91763, #62726, #39268, #62234, #92741, #83771, #85250, #38281, #31242, #39755, #93226, #24752, #32225, #31739, #70254, #68776, #38767, #7786, #61738, #30750, #76269, #85744, #47230, #84278, #789, #47731, #70751, #78228, #9741, #84757, #40241, #15778, #61257, #2265, #63219, #92256, #53265, #69757, #24265, #15295, #46267, #54245, #16263, #46746, #45777, #23285, #76751, #54729, #16756, #17743, #55741, #79709, #64192, #57192, #11208, #94210, #19205, #4714, #41727, #26697, #65179, #73175, #87690, #86232 ),
 ( #42213, #80192, #64681, #48219, #25740, #63707, #49687, #40732, #35176, #56232, #95702, #78729, #4216, #94711, #72197, #18725, #26217, #72680, #3726, #57688, #18229, #10239, #27185, #34686, #87201, #34187, #12189, #56710, #71234, #41241, #86727, #48711, #79213, #65677, #71718, #25256, #11703, #2759, #88183, #49205, #19697, #95189, #10724, #50184, #3229, #80695, #42698, #33212, #33694, #6665, #82160, #6175, #36679, #27683, #29154, #81182, #74157, #52167, #37182, #67674, #44660, #44156, #21681, #12682, #51181, #50689, #5691, #43181, #20187, #82660, #90151, #96702, #81663, #14176, #14680, #98184, #22170, #28670, #29641, #28180, #73669, #60148, #75155, #36177, #37667, #13673, #67167, #90645, #58676, #66678, #59163, #13175, #52652, #83155, #66168, #5197, #89668, #88680, #58168, #51681, #97202, #59660, #74665, #89175, #45148, #75653, #97692, #7164, #96200, #35684, #20688, #43671, #21180, #38164, #180, #23163, #54610, #24142, #1158, #674, #9125, #69634, #39640, #22669, #15664, #47112, #61136, #46625, #30136, #76148, #68650, #7673, #1652, #68167, #31619, #70132, #69147, #76633, #38645, #39144, #98687, #60642, #91143, #53146, #31124, #30628, #85127, #61620, #92138, #23662, #83654, #46147, #54124, #91645, #62109, #15170, #92619, #16637, #77124, #84636, #8635, #8152, #77613, #53640, #45651, #16139, #84158, #44482, #51997, #52477, #21500, #82487, #66498, #14004, #29466, #89983, #74984, #6487, #59973, #36994, #58995, #82982, #6006, #67491, #14502, #90467, #59483, #74484, #98012, #60471, #22002, #28501, #44972, #28979, #36501, #66993, #75478, #97516, #90960, #37990, #81990, #6992, #97024, #37496, #67985, #89497, #98512, #29965, #22492, #52965, #68482, #14998, #83477, #21008, #45468, #75969, #43492, #7497, #9, #20512, #58495, #51495, #50997, #89005, #81492, #12995, #35996, #73992, #5518, #13501, #43981, #41548, #20503, #56531, #64501, #72995, #12501, #50989, #4525, #33511, #72013, #3543, #95007, #49504, #5010, #35494, #20000, #57504, #81483, #50501, #12987, #87020, #42037, #27989, #57012, #65492, #64008, #34004, #26515, #87514, #71547, #3057, #88497, #94521, #95514, #72501, #64987, #27497, #58484, #88997, #26040, #18532, #4033, #49023, #57991, #34496, #27007, #80009, #65989, #19027, #11514, #79529, #11029, #88000, #96012, #80998, #19513, #50010, #43000, #80513, #73483, #96516, #12012, #42511, #34988, #66487, #83467, #37487, #82476, #83956, #29456, #82973, #60462, #5998, #51988, #74973, #97505, #14988, #68473, #13492, #58985, #6478, #35985, #73984, #98003, #13996, #75467, #59964, #43971, #91456, #28492, #36492, #44963, #45459, #22982 ) ),
 .UNSPECIFIED., .F., .F., .T. ) 
 B_SPLINE_SURFACE_WITH_KNOTS ( ( 2, 2 ),
 ( 3, 2, 2, 2, 2, 2, 2, 2, 2, 2, 2, 2, 2, 2, 2, 2, 2, 2, 2, 2, 2, 2, 2, 2, 2, 2, 2, 2, 2, 2, 2, 2, 2, 2, 2, 2, 2, 2, 2, 2, 2, 2, 2, 2, 2, 2, 2, 2, 2, 2, 2, 2, 2, 2, 2, 2, 2, 2, 2, 2, 2, 2, 2, 2, 2, 2, 2, 2, 2, 2, 2, 2, 2, 2, 2, 2, 2, 2, 2, 2, 2, 2, 2, 2, 2, 2, 2, 2, 2, 2, 2, 2, 2, 2, 2, 2, 2, 2, 2, 2, 2, 2, 2, 2, 2, 2, 2, 2, 2, 2, 2, 2, 2, 2, 2, 2, 2, 2, 2, 2, 2, 2, 2, 2, 2, 2, 2, 2, 2, 2, 2, 2, 2, 2, 2, 2, 2, 2, 2, 2, 2, 2, 2, 2, 2, 2, 2, 2, 2, 2, 2, 2, 2, 2, 2, 2, 2, 2, 2, 2, 2, 2, 3 ),
 ( 0.000000000000000000, 1.000000000000000000 ),
 ( 0.000000000000000000, 0.005952380952380952051, 0.01190476190476190410, 0.01785714285714285615, 0.02380952380952380820, 0.02976190476190476025, 0.03571428571428571230, 0.04166666666666666435, 0.04761904761904761640, 0.05357142857142856845, 0.05952380952380952051, 0.06547619047619047949, 0.07142857142857142461, 0.07738095238095238360, 0.08333333333333332871, 0.08928571428571428770, 0.09523809523809523281, 0.1011904761904761918, 0.1071428571428571369, 0.1130952380952380959, 0.1190476190476190410, 0.1250000000000000000, 0.1309523809523809590, 0.1369047619047619180, 0.1428571428571428492, 0.1488095238095238082, 0.1547619047619047672, 0.1607142857142857262, 0.1666666666666666574, 0.1726190476190476164, 0.1785714285714285754, 0.1845238095238095344, 0.1904761904761904656, 0.1964285714285714246, 0.2023809523809523836, 0.2083333333333333426, 0.2142857142857142738, 0.2202380952380952328, 0.2261904761904761918, 0.2321428571428571508, 0.2380952380952380820, 0.2440476190476190410, 0.2500000000000000000, 0.2559523809523809312, 0.2619047619047619180, 0.2678571428571428492, 0.2738095238095238360, 0.2797619047619047672, 0.2857142857142856984, 0.2916666666666666852, 0.2976190476190476164, 0.3035714285714285476, 0.3095238095238095344, 0.3154761904761904656, 0.3214285714285714524, 0.3273809523809523836, 0.3333333333333333148, 0.3392857142857143016, 0.3452380952380952328, 0.3511904761904761640, 0.3571428571428571508, 0.3630952380952380820, 0.3690476190476190688, 0.3750000000000000000, 0.3809523809523809312, 0.3869047619047619180, 0.3928571428571428492, 0.3988095238095238360, 0.4047619047619047672, 0.4107142857142856984, 0.4166666666666666852, 0.4226190476190476164, 0.4285714285714285476, 0.4345238095238095344, 0.4404761904761904656, 0.4464285714285714524, 0.4523809523809523836, 0.4583333333333333148, 0.4642857142857143016, 0.4702380952380952328, 0.4761904761904761640, 0.4821428571428571508, 0.4880952380952380820, 0.4940476190476190688, 0.5000000000000000000, 0.5059523809523809312, 0.5119047619047618625, 0.5178571428571429047, 0.5238095238095238360, 0.5297619047619047672, 0.5357142857142856984, 0.5416666666666666297, 0.5476190476190476719, 0.5535714285714286031, 0.5595238095238095344, 0.5654761904761904656, 0.5714285714285713969, 0.5773809523809523281, 0.5833333333333333703, 0.5892857142857143016, 0.5952380952380952328, 0.6011904761904761640, 0.6071428571428570953, 0.6130952380952381375, 0.6190476190476190688, 0.6250000000000000000, 0.6309523809523809312, 0.6369047619047618625, 0.6428571428571429047, 0.6488095238095238360, 0.6547619047619047672, 0.6607142857142856984, 0.6666666666666666297, 0.6726190476190476719, 0.6785714285714286031, 0.6845238095238095344, 0.6904761904761904656, 0.6964285714285713969, 0.7023809523809523281, 0.7083333333333333703, 0.7142857142857143016, 0.7202380952380952328, 0.7261904761904761640, 0.7321428571428570953, 0.7380952380952381375, 0.7440476190476190688, 0.7500000000000000000, 0.7559523809523809312, 0.7619047619047618625, 0.7678571428571429047, 0.7738095238095238360, 0.7797619047619047672, 0.7857142857142856984, 0.7916666666666666297, 0.7976190476190476719, 0.8035714285714286031, 0.8095238095238095344, 0.8154761904761904656, 0.8214285714285713969, 0.8273809523809523281, 0.8333333333333333703, 0.8392857142857143016, 0.8452380952380952328, 0.8511904761904761640, 0.8571428571428570953, 0.8630952380952381375, 0.8690476190476190688, 0.8750000000000000000, 0.8809523809523809312, 0.8869047619047618625, 0.8928571428571429047, 0.8988095238095238360, 0.9047619047619047672, 0.9107142857142856984, 0.9166666666666666297, 0.9226190476190476719, 0.9285714285714286031, 0.9345238095238095344, 0.9404761904761904656, 0.9464285714285713969, 0.9523809523809523281, 0.9583333333333333703, 0.9642857142857143016 ),
 .UNSPECIFIED. ) 
 GEOMETRIC_REPRESENTATION_ITEM ( )  RATIONAL_B_SPLINE_SURFACE ( (
 ( 1.000000000000000000, 0.9659258262890683122, 1.000000000000000000, 0.9659258262890683122, 1.000000000000000000, 0.9659258262890683122, 1.000000000000000000, 0.9659258262890683122, 1.000000000000000000, 0.9659258262890683122, 1.000000000000000000, 0.9659258262890683122, 1.000000000000000000, 0.9659258262890683122, 1.000000000000000000, 0.9659258262890683122, 1.000000000000000000, 0.9659258262890683122, 1.000000000000000000, 0.9659258262890683122, 1.000000000000000000, 0.9659258262890683122, 1.000000000000000000, 0.9659258262890683122, 1.000000000000000000, 0.9659258262890683122, 1.000000000000000000, 0.9659258262890683122, 1.000000000000000000, 0.9659258262890683122, 1.000000000000000000, 0.9659258262890683122, 1.000000000000000000, 0.9659258262890683122, 1.000000000000000000, 0.9659258262890683122, 1.000000000000000000, 0.9659258262890683122, 1.000000000000000000, 0.9659258262890683122, 1.000000000000000000, 0.9659258262890683122, 1.000000000000000000, 0.9659258262890683122, 1.000000000000000000, 0.9659258262890683122, 1.000000000000000000, 0.9659258262890683122, 1.000000000000000000, 0.9659258262890683122, 1.000000000000000000, 0.9659258262890683122, 1.000000000000000000, 0.9659258262890683122, 1.000000000000000000, 0.9659258262890683122, 1.000000000000000000, 0.9659258262890683122, 1.000000000000000000, 0.9659258262890683122, 1.000000000000000000, 0.9659258262890683122, 1.000000000000000000, 0.9659258262890683122, 1.000000000000000000, 0.9659258262890683122, 1.000000000000000000, 0.9659258262890683122, 1.000000000000000000, 0.9659258262890683122, 1.000000000000000000, 0.9659258262890683122, 1.000000000000000000, 0.9659258262890683122, 1.000000000000000000, 0.9659258262890683122, 1.000000000000000000, 0.9659258262890683122, 1.000000000000000000, 0.9659258262890683122, 1.000000000000000000, 0.9659258262890683122, 1.000000000000000000, 0.9659258262890683122, 1.000000000000000000, 0.9659258262890683122, 1.000000000000000000, 0.9659258262890683122, 1.000000000000000000, 0.9659258262890683122, 1.000000000000000000, 0.9659258262890683122, 1.000000000000000000, 0.9659258262890683122, 1.000000000000000000, 0.9659258262890683122, 1.000000000000000000, 0.9659258262890683122, 1.000000000000000000, 0.9659258262890683122, 1.000000000000000000, 0.9659258262890683122, 1.000000000000000000, 0.9659258262890683122, 1.000000000000000000, 0.9659258262890683122, 1.000000000000000000, 0.9659258262890683122, 1.000000000000000000, 0.9659258262890683122, 1.000000000000000000, 0.9659258262890683122, 1.000000000000000000, 0.9659258262890683122, 1.000000000000000000, 0.9659258262890683122, 1.000000000000000000, 0.9659258262890683122, 1.000000000000000000, 0.9659258262890683122, 1.000000000000000000, 0.9659258262890683122, 1.000000000000000000, 0.9659258262890683122, 1.000000000000000000, 0.9659258262890683122, 1.000000000000000000, 0.9659258262890683122, 1.000000000000000000, 0.9659258262890683122, 1.000000000000000000, 0.9659258262890683122, 1.000000000000000000, 0.9659258262890683122, 1.000000000000000000, 0.9659258262890683122, 1.000000000000000000, 0.9659258262890683122, 1.000000000000000000, 0.9659258262890683122, 1.000000000000000000, 0.9659258262890683122, 1.000000000000000000, 0.9659258262890683122, 1.000000000000000000, 0.9659258262890683122, 1.000000000000000000, 0.9659258262890683122, 1.000000000000000000, 0.9659258262890683122, 1.000000000000000000, 0.9659258262890683122, 1.000000000000000000, 0.9659258262890683122, 1.000000000000000000, 0.9659258262890683122, 1.000000000000000000, 0.9659258262890683122, 1.000000000000000000, 0.9659258262890683122, 1.000000000000000000, 0.9659258262890683122, 1.000000000000000000, 0.9659258262890683122, 1.000000000000000000, 0.9659258262890683122, 1.000000000000000000, 0.9659258262890683122, 1.000000000000000000, 0.9659258262890683122, 1.000000000000000000, 0.9659258262890683122, 1.000000000000000000, 0.9659258262890683122, 1.000000000000000000, 0.9659258262890683122, 1.000000000000000000, 0.9659258262890683122, 1.000000000000000000, 0.9659258262890683122, 1.000000000000000000, 0.9659258262890683122, 1.000000000000000000, 0.9659258262890683122, 1.000000000000000000, 0.9659258262890683122, 1.000000000000000000, 0.9659258262890683122, 1.000000000000000000, 0.9659258262890683122, 1.000000000000000000, 0.9659258262890683122, 1.000000000000000000, 0.9659258262890683122, 1.000000000000000000, 0.9659258262890683122, 1.000000000000000000, 0.9659258262890683122, 1.000000000000000000, 0.9659258262890683122, 1.000000000000000000, 0.9659258262890683122, 1.000000000000000000, 0.9659258262890683122, 1.000000000000000000, 0.9659258262890683122, 1.000000000000000000, 0.9659258262890683122, 1.000000000000000000, 0.9659258262890683122, 1.000000000000000000, 0.9659258262890683122, 1.000000000000000000, 0.9659258262890683122, 1.000000000000000000, 0.9659258262890683122, 1.000000000000000000, 0.9659258262890683122, 1.000000000000000000, 0.9659258262890683122, 1.000000000000000000, 0.9659258262890683122, 1.000000000000000000, 0.9659258262890683122, 1.000000000000000000, 0.9659258262890683122, 1.000000000000000000, 0.9659258262890683122, 1.000000000000000000, 0.9659258262890683122, 1.000000000000000000, 0.9659258262890683122, 1.000000000000000000, 0.9659258262890683122, 1.000000000000000000, 0.9659258262890683122, 1.000000000000000000, 0.9659258262890683122, 1.000000000000000000, 0.9659258262890683122, 1.000000000000000000, 0.9659258262890683122, 1.000000000000000000, 0.9659258262890683122, 1.000000000000000000, 0.9659258262890683122, 1.000000000000000000, 0.9659258262890683122, 1.000000000000000000, 0.9659258262890683122, 1.000000000000000000, 0.9659258262890683122, 1.000000000000000000, 0.9659258262890683122, 1.000000000000000000, 0.9659258262890683122, 1.000000000000000000, 0.9659258262890683122, 1.000000000000000000, 0.9659258262890683122, 1.000000000000000000, 0.9659258262890683122, 1.000000000000000000, 0.9659258262890683122, 1.000000000000000000, 0.9659258262890683122, 1.000000000000000000, 0.9659258262890683122, 1.000000000000000000, 0.9659258262890683122, 1.000000000000000000, 0.9659258262890683122, 1.000000000000000000, 0.9659258262890683122, 1.000000000000000000, 0.9659258262890683122, 1.000000000000000000, 0.9659258262890683122, 1.000000000000000000, 0.9659258262890683122, 1.000000000000000000, 0.9659258262890683122, 1.000000000000000000, 0.9659258262890683122, 1.000000000000000000, 0.9659258262890683122, 1.000000000000000000, 0.9659258262890683122, 1.000000000000000000, 0.9659258262890683122, 1.000000000000000000, 0.9659258262890683122, 1.000000000000000000, 0.9659258262890683122, 1.000000000000000000, 0.9659258262890683122, 1.000000000000000000, 0.9659258262890683122, 1.000000000000000000, 0.9659258262890683122, 1.000000000000000000, 0.9659258262890683122, 1.000000000000000000, 0.9659258262890683122, 1.000000000000000000, 0.9659258262890683122, 1.000000000000000000, 0.9659258262890683122, 1.000000000000000000, 0.9659258262890683122, 1.000000000000000000, 0.9659258262890683122, 1.000000000000000000, 0.9659258262890683122, 1.000000000000000000, 0.9659258262890683122, 1.000000000000000000, 0.9659258262890683122, 1.000000000000000000, 0.9659258262890683122, 1.000000000000000000, 0.9659258262890683122, 1.000000000000000000, 0.9659258262890683122, 1.000000000000000000),
 ( 1.000000000000000000, 0.9659258262890683122, 1.000000000000000000, 0.9659258262890683122, 1.000000000000000000, 0.9659258262890683122, 1.000000000000000000, 0.9659258262890683122, 1.000000000000000000, 0.9659258262890683122, 1.000000000000000000, 0.9659258262890683122, 1.000000000000000000, 0.9659258262890683122, 1.000000000000000000, 0.9659258262890683122, 1.000000000000000000, 0.9659258262890683122, 1.000000000000000000, 0.9659258262890683122, 1.000000000000000000, 0.9659258262890683122, 1.000000000000000000, 0.9659258262890683122, 1.000000000000000000, 0.9659258262890683122, 1.000000000000000000, 0.9659258262890683122, 1.000000000000000000, 0.9659258262890683122, 1.000000000000000000, 0.9659258262890683122, 1.000000000000000000, 0.9659258262890683122, 1.000000000000000000, 0.9659258262890683122, 1.000000000000000000, 0.9659258262890683122, 1.000000000000000000, 0.9659258262890683122, 1.000000000000000000, 0.9659258262890683122, 1.000000000000000000, 0.9659258262890683122, 1.000000000000000000, 0.9659258262890683122, 1.000000000000000000, 0.9659258262890683122, 1.000000000000000000, 0.9659258262890683122, 1.000000000000000000, 0.9659258262890683122, 1.000000000000000000, 0.9659258262890683122, 1.000000000000000000, 0.9659258262890683122, 1.000000000000000000, 0.9659258262890683122, 1.000000000000000000, 0.9659258262890683122, 1.000000000000000000, 0.9659258262890683122, 1.000000000000000000, 0.9659258262890683122, 1.000000000000000000, 0.9659258262890683122, 1.000000000000000000, 0.9659258262890683122, 1.000000000000000000, 0.9659258262890683122, 1.000000000000000000, 0.9659258262890683122, 1.000000000000000000, 0.9659258262890683122, 1.000000000000000000, 0.9659258262890683122, 1.000000000000000000, 0.9659258262890683122, 1.000000000000000000, 0.9659258262890683122, 1.000000000000000000, 0.9659258262890683122, 1.000000000000000000, 0.9659258262890683122, 1.000000000000000000, 0.9659258262890683122, 1.000000000000000000, 0.9659258262890683122, 1.000000000000000000, 0.9659258262890683122, 1.000000000000000000, 0.9659258262890683122, 1.000000000000000000, 0.9659258262890683122, 1.000000000000000000, 0.9659258262890683122, 1.000000000000000000, 0.9659258262890683122, 1.000000000000000000, 0.9659258262890683122, 1.000000000000000000, 0.9659258262890683122, 1.000000000000000000, 0.9659258262890683122, 1.000000000000000000, 0.9659258262890683122, 1.000000000000000000, 0.9659258262890683122, 1.000000000000000000, 0.9659258262890683122, 1.000000000000000000, 0.9659258262890683122, 1.000000000000000000, 0.9659258262890683122, 1.000000000000000000, 0.9659258262890683122, 1.000000000000000000, 0.9659258262890683122, 1.000000000000000000, 0.9659258262890683122, 1.000000000000000000, 0.9659258262890683122, 1.000000000000000000, 0.9659258262890683122, 1.000000000000000000, 0.9659258262890683122, 1.000000000000000000, 0.9659258262890683122, 1.000000000000000000, 0.9659258262890683122, 1.000000000000000000, 0.9659258262890683122, 1.000000000000000000, 0.9659258262890683122, 1.000000000000000000, 0.9659258262890683122, 1.000000000000000000, 0.9659258262890683122, 1.000000000000000000, 0.9659258262890683122, 1.000000000000000000, 0.9659258262890683122, 1.000000000000000000, 0.9659258262890683122, 1.000000000000000000, 0.9659258262890683122, 1.000000000000000000, 0.9659258262890683122, 1.000000000000000000, 0.9659258262890683122, 1.000000000000000000, 0.9659258262890683122, 1.000000000000000000, 0.9659258262890683122, 1.000000000000000000, 0.9659258262890683122, 1.000000000000000000, 0.9659258262890683122, 1.000000000000000000, 0.9659258262890683122, 1.000000000000000000, 0.9659258262890683122, 1.000000000000000000, 0.9659258262890683122, 1.000000000000000000, 0.9659258262890683122, 1.000000000000000000, 0.9659258262890683122, 1.000000000000000000, 0.9659258262890683122, 1.000000000000000000, 0.9659258262890683122, 1.000000000000000000, 0.9659258262890683122, 1.000000000000000000, 0.9659258262890683122, 1.000000000000000000, 0.9659258262890683122, 1.000000000000000000, 0.9659258262890683122, 1.000000000000000000, 0.9659258262890683122, 1.000000000000000000, 0.9659258262890683122, 1.000000000000000000, 0.9659258262890683122, 1.000000000000000000, 0.9659258262890683122, 1.000000000000000000, 0.9659258262890683122, 1.000000000000000000, 0.9659258262890683122, 1.000000000000000000, 0.9659258262890683122, 1.000000000000000000, 0.9659258262890683122, 1.000000000000000000, 0.9659258262890683122, 1.000000000000000000, 0.9659258262890683122, 1.000000000000000000, 0.9659258262890683122, 1.000000000000000000, 0.9659258262890683122, 1.000000000000000000, 0.9659258262890683122, 1.000000000000000000, 0.9659258262890683122, 1.000000000000000000, 0.9659258262890683122, 1.000000000000000000, 0.9659258262890683122, 1.000000000000000000, 0.9659258262890683122, 1.000000000000000000, 0.9659258262890683122, 1.000000000000000000, 0.9659258262890683122, 1.000000000000000000, 0.9659258262890683122, 1.000000000000000000, 0.9659258262890683122, 1.000000000000000000, 0.9659258262890683122, 1.000000000000000000, 0.9659258262890683122, 1.000000000000000000, 0.9659258262890683122, 1.000000000000000000, 0.9659258262890683122, 1.000000000000000000, 0.9659258262890683122, 1.000000000000000000, 0.9659258262890683122, 1.000000000000000000, 0.9659258262890683122, 1.000000000000000000, 0.9659258262890683122, 1.000000000000000000, 0.9659258262890683122, 1.000000000000000000, 0.9659258262890683122, 1.000000000000000000, 0.9659258262890683122, 1.000000000000000000, 0.9659258262890683122, 1.000000000000000000, 0.9659258262890683122, 1.000000000000000000, 0.9659258262890683122, 1.000000000000000000, 0.9659258262890683122, 1.000000000000000000, 0.9659258262890683122, 1.000000000000000000, 0.9659258262890683122, 1.000000000000000000, 0.9659258262890683122, 1.000000000000000000, 0.9659258262890683122, 1.000000000000000000, 0.9659258262890683122, 1.000000000000000000, 0.9659258262890683122, 1.000000000000000000, 0.9659258262890683122, 1.000000000000000000, 0.9659258262890683122, 1.000000000000000000, 0.9659258262890683122, 1.000000000000000000, 0.9659258262890683122, 1.000000000000000000, 0.9659258262890683122, 1.000000000000000000, 0.9659258262890683122, 1.000000000000000000, 0.9659258262890683122, 1.000000000000000000, 0.9659258262890683122, 1.000000000000000000, 0.9659258262890683122, 1.000000000000000000, 0.9659258262890683122, 1.000000000000000000, 0.9659258262890683122, 1.000000000000000000, 0.9659258262890683122, 1.000000000000000000, 0.9659258262890683122, 1.000000000000000000, 0.9659258262890683122, 1.000000000000000000, 0.9659258262890683122, 1.000000000000000000, 0.9659258262890683122, 1.000000000000000000, 0.9659258262890683122, 1.000000000000000000, 0.9659258262890683122, 1.000000000000000000, 0.9659258262890683122, 1.000000000000000000, 0.9659258262890683122, 1.000000000000000000, 0.9659258262890683122, 1.000000000000000000, 0.9659258262890683122, 1.000000000000000000, 0.9659258262890683122, 1.000000000000000000, 0.9659258262890683122, 1.000000000000000000, 0.9659258262890683122, 1.000000000000000000, 0.9659258262890683122, 1.000000000000000000, 0.9659258262890683122, 1.000000000000000000, 0.9659258262890683122, 1.000000000000000000, 0.9659258262890683122, 1.000000000000000000, 0.9659258262890683122, 1.000000000000000000) ) ) 
 REPRESENTATION_ITEM ( '' )  SURFACE ( )  );
#84693 = CARTESIAN_POINT ( 'NONE',  ( 12.58781651029199189, 15.00000000000000533, 7.446837378630806192 ) ) ;
#84694 = VECTOR ( 'NONE', #49189, 1000.000000000000114 ) ;
#84695 = EDGE_CURVE ( 'NONE', #39693, #23152, #87374, .T. ) ;
#84696 = CARTESIAN_POINT ( 'NONE',  ( -0.8801773607110991993, 57.85535201082149825, -2.915334737309923874 ) ) ;
#84697 = ORIENTED_EDGE ( 'NONE', *, *, #93272, .F. ) ;
#84698 = CARTESIAN_POINT ( 'NONE',  ( 14.49999999999999822, 11.50000000000000000, 5.000000000000000000 ) ) ;
#84699 = CARTESIAN_POINT ( 'NONE',  ( 2.035157376598824452, 28.68868534415484106, 7.964842623401179544 ) ) ;
#84700 = AXIS2_PLACEMENT_3D ( 'NONE', #34903, #27405, #26916 ) ;
#84702 = CARTESIAN_POINT ( 'NONE',  ( 7.084665262690076126, 59.10535201082150536, 10.88017736071109987 ) ) ;
#84701 = CARTESIAN_POINT ( 'NONE',  ( 7.361572987183169658, 64.96726448433412315, -9.846743663894592657 ) ) ;
#84703 = CARTESIAN_POINT ( 'NONE',  ( -1.926860441876564023, 62.87045670184114243, 3.195792623639529761 ) ) ;
#84704 = EDGE_CURVE ( 'NONE', #71742, #55464, #34357, .T. ) ;
#84705 = CARTESIAN_POINT ( 'NONE',  ( 8.630000000000000782, 1.019547802438458550, 4.000000000000000000 ) ) ;
#84707 = AXIS2_PLACEMENT_3D ( 'NONE', #17969, #48455, #78953 ) ;
#84706 = CARTESIAN_POINT ( 'NONE',  ( 5.963430220938287007, 4.328790035174473694, 10.32896413005679825 ) ) ;
#84709 = FACE_OUTER_BOUND ( 'NONE', #3382, .T. ) ;
#84708 = CARTESIAN_POINT ( 'NONE',  ( 10.00000000000000178, 34.31368534415484106, 10.88017736071110342 ) ) ;
#84710 = CARTESIAN_POINT ( 'NONE',  ( 12.63842701281683922, 34.55059781766745886, -9.846743663894590881 ) ) ;
#84711 = FACE_OUTER_BOUND ( 'NONE', #79540, .T. ) ;
#84712 = CARTESIAN_POINT ( 'NONE',  ( -5.204170427930421283E-15, 25.55374883491398563, -14.16423886937410082 ) ) ;
#84713 = CARTESIAN_POINT ( 'NONE',  ( 19.38216949554541557, 2.248634669930420049, -9.382169495545420901 ) ) ;
#84714 = AXIS2_PLACEMENT_3D ( 'NONE', #6696, #14709, #28698 ) ;
#84715 = CARTESIAN_POINT ( 'NONE',  ( 7.084665262690076126, 17.02201867748817676, -10.88017736071110164 ) ) ;
#84716 = LINE ( 'NONE', #14253, #5371 ) ;
#84717 = CARTESIAN_POINT ( 'NONE',  ( 20.36894250292379738, 24.92874883491396787, -10.36894250292379027 ) ) ;
#84718 = CARTESIAN_POINT ( 'NONE',  ( 2.917880565312950480, 65.97041550158063217, -12.26659068614894821 ) ) ;
#84719 = CARTESIAN_POINT ( 'NONE',  ( 7.361572987183169658, 29.96726448433411960, -9.846743663894592657 ) ) ;
#84720 = CARTESIAN_POINT ( 'NONE',  ( 2.791683348922240793, 21.63393115100078745, 7.208316651077764092 ) ) ;
#84721 = FACE_OUTER_BOUND ( 'NONE', #52560, .T. ) ;
#84722 = VERTEX_POINT ( 'NONE', #95367 ) ;
#84723 = CARTESIAN_POINT ( 'NONE',  ( 14.92337183194729633, 27.67559781766745530, 8.527530157486181039 ) ) ;
#84724 = CARTESIAN_POINT ( 'NONE',  ( 20.88017736071110875, 25.77201867748816966, -2.915334737309920765 ) ) ;
#84725 = CARTESIAN_POINT ( 'NONE',  ( 2.791683348922237240, 60.38393115100078745, -7.208316651077763204 ) ) ;
#84727 = CARTESIAN_POINT ( 'NONE',  ( 5.500000000000000000, 11.50000000000000000, -6.500000000000000888 ) ) ;
#84726 = CARTESIAN_POINT ( 'NONE',  ( 6.204703633549690345, 7.845415501580634832, 14.16423886937410082 ) ) ;
#84728 = CARTESIAN_POINT ( 'NONE',  ( -18.89999999999999147, 91.00000000000000000, -7.750000000000000000 ) ) ;
#84729 = CARTESIAN_POINT ( 'NONE',  ( 2.791683348922240793, 6.633931151000785675, 7.208316651077764092 ) ) ;
#84730 = CARTESIAN_POINT ( 'NONE',  ( 10.00000000000000000, 32.87363466993042493, -12.81628187352647608 ) ) ;
#84731 = CARTESIAN_POINT ( 'NONE',  ( 14.92337183194729633, 42.67559781766745886, 8.527530157486181039 ) ) ;
#84732 = ORIENTED_EDGE ( 'NONE', *, *, #26876, .T. ) ;
#84733 = CARTESIAN_POINT ( 'NONE',  ( 1.472469842513823179, 15.59226448433411960, -4.923371831947296329 ) ) ;
#84734 = DIRECTION ( 'NONE',  ( -0.000000000000000000, 1.000000000000000000, -0.000000000000000000 ) ) ;
#84735 = CARTESIAN_POINT ( 'NONE',  ( 14.36383853300408475, 14.95037103067321915, -3.367113227848937740 ) ) ;
#84736 = CARTESIAN_POINT ( 'NONE',  ( 20.36894250292379382, 48.67874883491396076, 10.36894250292379205 ) ) ;
#84737 = CARTESIAN_POINT ( 'NONE',  ( -0.8801773607111008646, 58.27201867748816966, 2.915334737309923430 ) ) ;
#84738 = AXIS2_PLACEMENT_3D ( 'NONE', #27140, #34142, #41195 ) ;
#84739 = CARTESIAN_POINT ( 'NONE',  ( 15.44008868035555260, 59.73035201082151247, 9.422509992056143702 ) ) ;
#84740 = CARTESIAN_POINT ( 'NONE',  ( 1.472469842513823179, 41.42559781766745886, 4.923371831947296329 ) ) ;
#84741 = CARTESIAN_POINT ( 'NONE',  ( 2.035157376598822676, 22.43868534415483396, -7.964842623401177768 ) ) ;
#84742 = FACE_OUTER_BOUND ( 'NONE', #61546, .T. ) ;
#84743 = CARTESIAN_POINT ( 'NONE',  ( 12.63842701281683034, 52.46726448433413026, 9.846743663894596210 ) ) ;
#84744 = AXIS2_PLACEMENT_3D ( 'NONE', #17088, #630, #84099 ) ;
#84745 = CARTESIAN_POINT ( 'NONE',  ( 17.96484262340118221, 51.18868534415483396, -7.964842623401177768 ) ) ;
#84746 = EDGE_CURVE ( 'NONE', #6373, #35739, #70826, .T. ) ;
#84747 = ORIENTED_EDGE ( 'NONE', *, *, #6143, .F. ) ;
#84748 = VERTEX_POINT ( 'NONE', #48388 ) ;
#84749 = LINE ( 'NONE', #16254, #35714 ) ;
#84750 =( LENGTH_UNIT ( ) NAMED_UNIT ( * ) SI_UNIT ( .MILLI., .METRE. ) );
#84751 = CARTESIAN_POINT ( 'NONE',  ( 19.84674366389459266, 43.71726448433410894, -2.638427012816827677 ) ) ;
#84752 = CARTESIAN_POINT ( 'NONE',  ( 0.1532563361054082862, 16.21726448433411960, 2.638427012816831674 ) ) ;
#84753 = CARTESIAN_POINT ( 'NONE',  ( 16.40814093676324603, 52.45696800326375353, -11.09922568453594671 ) ) ;
#84755 = CARTESIAN_POINT ( 'NONE',  ( 1.472469842513823179, 51.42559781766745886, 4.923371831947296329 ) ) ;
#84754 = CARTESIAN_POINT ( 'NONE',  ( 2.035157376598822676, 22.43868534415483396, -7.964842623401177768 ) ) ;
#84756 = CARTESIAN_POINT ( 'NONE',  ( 13.79529636645031943, 30.34541550158063927, -14.16423886937409904 ) ) ;
#84757 = CARTESIAN_POINT ( 'NONE',  ( 2.917880565312950480, 60.97041550158063927, -12.26659068614894821 ) ) ;
#84758 = CARTESIAN_POINT ( 'NONE',  ( 0.1532563361054083140, 56.00893115100078745, 1.131784320476157264E-15 ) ) ;
#84759 = CARTESIAN_POINT ( 'NONE',  ( 18.00000000000000000, 78.06026162106516608, 3.869897288748200825 ) ) ;
#84760 = CARTESIAN_POINT ( 'NONE',  ( 19.42250999205614193, 50.14701867748817676, 5.440088680355555262 ) ) ;
#84761 = CARTESIAN_POINT ( 'NONE',  ( 10.00000000000000000, 19.75893115100078390, -9.846743663894594434 ) ) ;
#84762 = CARTESIAN_POINT ( 'NONE',  ( -7.072388532689616980, -84.40601219567531643, 4.000000000000805578 ) ) ;
#84763 = ORIENTED_EDGE ( 'NONE', *, *, #83031, .F. ) ;
#84764 = CARTESIAN_POINT ( 'NONE',  ( -14.26295192185813221, 14.95077488074853456, 3.770186020344923339 ) ) ;
#84765 = EDGE_LOOP ( 'NONE', ( #71545, #53626, #86437, #42336 ) ) ;
#84766 = CARTESIAN_POINT ( 'NONE',  ( 0.1532563361054100626, 5.800597817667452638, -2.638427012816831230 ) ) ;
#84767 = ORIENTED_EDGE ( 'NONE', *, *, #48860, .T. ) ;
#84768 = CARTESIAN_POINT ( 'NONE',  ( 2.917880565312950480, 25.97041550158063572, -12.26659068614894821 ) ) ;
#84769 = CARTESIAN_POINT ( 'NONE',  ( 1.472469842513823179, 15.59226448433411960, -4.923371831947296329 ) ) ;
#84770 = CARTESIAN_POINT ( 'NONE',  ( -0.8801773607110991993, 42.85535201082150536, -2.915334737309923874 ) ) ;
#84771 = SURFACE_STYLE_FILL_AREA ( #31258 ) ;
#84772 = VERTEX_POINT ( 'NONE', #34852 ) ;
#84773 = AXIS2_PLACEMENT_3D ( 'NONE', #48653, #10667, #64621 ) ;
#84774 = CARTESIAN_POINT ( 'NONE',  ( 19.42250999205614548, 25.98035201082150891, -5.440088680355545492 ) ) ;
#84775 = EDGE_LOOP ( 'NONE', ( #8043, #19553, #43072, #52897 ) ) ;
#84776 = PRESENTATION_LAYER_ASSIGNMENT (  '', '', ( #59201 ) ) ;
#84777 = CARTESIAN_POINT ( 'NONE',  ( 10.00000000000000178, 8.053748834913967869, 14.16423886937410082 ) ) ;
#84778 = ORIENTED_EDGE ( 'NONE', *, *, #46018, .T. ) ;
#84779 = CIRCLE ( 'NONE', #14564, 14.49999999999999822 ) ;
#84780 = ORIENTED_EDGE ( 'NONE', *, *, #45124, .T. ) ;
#84781 = CARTESIAN_POINT ( 'NONE',  ( -2.816281873526473856, 14.33196800326375531, 3.434112377981055619 ) ) ;
#84782 = CARTESIAN_POINT ( 'NONE',  ( 0.1532563361054100626, 5.800597817667452638, -2.638427012816831230 ) ) ;
#84783 = EDGE_CURVE ( 'NONE', #27291, #18983, #26866, .T. ) ;
#84784 = CARTESIAN_POINT ( 'NONE',  ( -0.1503990784575328643, 70.00000000000000000, 6.262539305110068177 ) ) ;
#84785 = CARTESIAN_POINT ( 'NONE',  ( 14.92337183194729633, 22.67559781766745175, 8.527530157486181039 ) ) ;
#84786 = CARTESIAN_POINT ( 'NONE',  ( 15.44008868035555793, 36.39701867748816966, -9.422509992056140149 ) ) ;
#84787 = EDGE_CURVE ( 'NONE', #9539, #94683, #11567, .T. ) ;
#84788 = ORIENTED_EDGE ( 'NONE', *, *, #89192, .T. ) ;
#84789 = DIRECTION ( 'NONE',  ( -0.000000000000000000, -1.000000000000000000, -0.000000000000000000 ) ) ;
#84790 = CARTESIAN_POINT ( 'NONE',  ( 20.88017736071110519, 55.56368534415484817, 2.639326808657452039E-16 ) ) ;
#84791 = CARTESIAN_POINT ( 'NONE',  ( -46.94000000000001194, 102.9999999999993889, -5.997726559847341932 ) ) ;
#84792 = CARTESIAN_POINT ( 'NONE',  ( 19.67858290521088804, 89.00000000000000000, -5.461713021790605360 ) ) ;
#84793 = CARTESIAN_POINT ( 'NONE',  ( 10.00000000000000000, 61.81368534415484106, -10.88017736071110342 ) ) ;
#84794 = EDGE_CURVE ( 'NONE', #3863, #18606, #49860, .T. ) ;
#84795 = CARTESIAN_POINT ( 'NONE',  ( 5.076628168052704559, 65.17559781766745175, -8.527530157486179263 ) ) ;
#84796 = CARTESIAN_POINT ( 'NONE',  ( 9.742785792574936821, 12.20136696231599061, 5.624999999999996447 ) ) ;
#84797 = CARTESIAN_POINT ( 'NONE',  ( 12.63842701281683034, 27.46726448433411250, 9.846743663894596210 ) ) ;
#84798 = CARTESIAN_POINT ( 'NONE',  ( 13.43411237798106583, 52.66530133659708213, -12.81628187352647252 ) ) ;
#84799 = DIRECTION ( 'NONE',  ( 0.1650476058606741014, 0.000000000000000000, 0.9862856015372319929 ) ) ;
#84800 = CARTESIAN_POINT ( 'NONE',  ( 0.1532563361054083140, 26.00893115100078745, 1.131784320476157264E-15 ) ) ;
#84801 = CARTESIAN_POINT ( 'NONE',  ( 13.43411237798106583, 22.66530133659708923, -12.81628187352647252 ) ) ;
#84802 = CYLINDRICAL_SURFACE ( 'NONE', #51353, 0.5000000000000004441 ) ;
#84803 = CARTESIAN_POINT ( 'NONE',  ( 0.5774900079438590739, 42.64701867748816966, -5.440088680355550821 ) ) ;
#84804 = CARTESIAN_POINT ( 'NONE',  ( 0.1532563361054100626, 60.80059781766744464, -2.638427012816831230 ) ) ;
#84805 = CIRCLE ( 'NONE', #49668, 2.000000000000001776 ) ;
#84806 = ADVANCED_FACE ( 'NONE', ( #49370 ), #32891, .F. ) ;
#84807 = AXIS2_PLACEMENT_3D ( 'NONE', #93303, #41798, #47302 ) ;
#84808 = DIRECTION ( 'NONE',  ( 0.000000000000000000, 1.000000000000000000, 0.000000000000000000 ) ) ;
#84809 = CARTESIAN_POINT ( 'NONE',  ( 19.84674366389459266, 28.30059781766745886, 2.638427012816836559 ) ) ;
#84810 = CARTESIAN_POINT ( 'NONE',  ( 5.076628168052703671, 21.84226448433411960, 8.527530157486179263 ) ) ;
#84811 = CARTESIAN_POINT ( 'NONE',  ( 4.559911319644449179, 7.230352010821504471, -9.422509992056141925 ) ) ;
#84812 = CARTESIAN_POINT ( 'NONE',  ( 22.81628187352647785, 16.41530133659708923, 3.434112377981063169 ) ) ;
#84813 = CARTESIAN_POINT ( 'NONE',  ( -10.28286150160520762, 89.18763609516977908, 5.839555419999288510 ) ) ;
#84814 = AXIS2_PLACEMENT_3D ( 'NONE', #38487, #13510, #43992 ) ;
#84815 = CARTESIAN_POINT ( 'NONE',  ( 6.507545146409696279, -58.30914921458864342, -2.500000000000000000 ) ) ;
#84816 = CARTESIAN_POINT ( 'NONE',  ( 12.91533473730992121, 24.52201867748816966, 10.88017736071110164 ) ) ;
#84817 = SURFACE_SIDE_STYLE ('',( #84339 ) ) ;
#84818 = CARTESIAN_POINT ( 'NONE',  ( 4.559911319644449179, 22.23035201082150536, -9.422509992056141925 ) ) ;
#84819 = CARTESIAN_POINT ( 'NONE',  ( 0.8952175423694853640, 12.60160829253885950, -5.990408912944323205 ) ) ;
#84820 = EDGE_CURVE ( 'NONE', #25555, #39153, #2922, .T. ) ;
#84821 = CARTESIAN_POINT ( 'NONE',  ( 15.44008868035555260, 34.73035201082151247, 9.422509992056143702 ) ) ;
#84823 = CARTESIAN_POINT ( 'NONE',  ( 9.641087339108837639, 14.95077488074853456, 11.16671550067055385 ) ) ;
#84822 = CARTESIAN_POINT ( 'NONE',  ( 17.08211943468705840, 60.13708216824729647, -12.26659068614894466 ) ) ;
#84824 = CARTESIAN_POINT ( 'NONE',  ( 18.72515096720570327, 6.072280503510315341, -6.499999999999985789 ) ) ;
#84825 = CARTESIAN_POINT ( 'NONE',  ( 12.63842701281683922, 24.55059781766745175, -9.846743663894590881 ) ) ;
#84826 = CARTESIAN_POINT ( 'NONE',  ( -16.60833333333331652, 99.75000000000000000, -8.000000000000000000 ) ) ;
#84827 = CARTESIAN_POINT ( 'NONE',  ( 2.603489959281584998, 6.582109641433292246, 6.499999999999998224 ) ) ;
#84828 = CARTESIAN_POINT ( 'NONE',  ( 17.20831665107776587, 62.88393115100078745, 7.208316651077764980 ) ) ;
#84829 = CYLINDRICAL_SURFACE ( 'NONE', #93829, 0.1000000000000001166 ) ;
#84830 = CARTESIAN_POINT ( 'NONE',  ( -10.79676793866758011, -44.60032227172015240, -4.000000000003602452 ) ) ;
#84831 = CARTESIAN_POINT ( 'NONE',  ( 6.204703633549690345, 20.76208216824730357, -14.16423886937410259 ) ) ;
#84832 = TOROIDAL_SURFACE ( 'NONE', #60841, 14.49999999999999822, 0.5000000000000000000 ) ;
#84833 = CARTESIAN_POINT ( 'NONE',  ( 10.00000000000000000, 39.75893115100078745, -9.846743663894594434 ) ) ;
#84834 = VERTEX_POINT ( 'NONE', #57362 ) ;
#84835 = CARTESIAN_POINT ( 'NONE',  ( -0.3689425029237898834, 51.17874883491397497, -10.36894250292378850 ) ) ;
#84836 = CARTESIAN_POINT ( 'NONE',  ( 19.84674366389459266, 18.30059781766745175, 2.638427012816836559 ) ) ;
#84838 = DIRECTION ( 'NONE',  ( 0.000000000000000000, 0.000000000000000000, 1.000000000000000000 ) ) ;
#84837 = DIRECTION ( 'NONE',  ( 0.8320502943378436100, -0.5547001962252291474, 0.000000000000000000 ) ) ;
#84839 = CARTESIAN_POINT ( 'NONE',  ( 20.88017736071110519, 50.56368534415484106, 2.639326808657452039E-16 ) ) ;
#84840 = CARTESIAN_POINT ( 'NONE',  ( 13.43411237798106583, 47.66530133659709634, -12.81628187352647252 ) ) ;
#84841 = CARTESIAN_POINT ( 'NONE',  ( 0.5774900079438590739, 12.64701867748817143, -5.440088680355550821 ) ) ;
#84843 = ORIENTED_EDGE ( 'NONE', *, *, #29798, .F. ) ;
#84842 = CARTESIAN_POINT ( 'NONE',  ( 22.81628187352648496, 51.83196800326376064, -3.434112377981050290 ) ) ;
#84844 = CARTESIAN_POINT ( 'NONE',  ( 14.92337183194729988, 64.34226448433412315, -8.527530157486177487 ) ) ;
#84845 = CARTESIAN_POINT ( 'NONE',  ( 7.361572987183170547, 7.050597817667451750, 9.846743663894590881 ) ) ;
#84846 = ORIENTED_EDGE ( 'NONE', *, *, #93932, .F. ) ;
#84847 = DIRECTION ( 'NONE',  ( 0.4617486132350345773, 0.000000000000000000, 0.8870108331782213806 ) ) ;
#84848 = CARTESIAN_POINT ( 'NONE',  ( 1.697696962861934722, 1.866248959293451470, -6.500000000000000888 ) ) ;
#84849 = CARTESIAN_POINT ( 'NONE',  ( -2.266590686148945544, 56.38708216824731068, -7.082119434687050408 ) ) ;
#84850 = CARTESIAN_POINT ( 'NONE',  ( 24.16423886937409904, 19.09541550158063927, 3.795296366450317205 ) ) ;
#84851 = CARTESIAN_POINT ( 'NONE',  ( 20.88017736071110164, 20.35535201082150891, 2.915334737309930979 ) ) ;
#84852 = CARTESIAN_POINT ( 'NONE',  ( 4.559911319644449179, 42.23035201082151247, -9.422509992056141925 ) ) ;
#84853 = CARTESIAN_POINT ( 'NONE',  ( 9.641450013144471143, 14.95037107666755638, -11.16690429682349439 ) ) ;
#84854 = DIRECTION ( 'NONE',  ( -1.000000000000000000, -2.569960705150834273E-16, 0.000000000000000000 ) ) ;
#84855 = CARTESIAN_POINT ( 'NONE',  ( 10.00000000000000000, 61.81368534415484106, -10.88017736071110342 ) ) ;
#84856 = CARTESIAN_POINT ( 'NONE',  ( -0.8801773607110991993, 57.85535201082149825, -2.915334737309923874 ) ) ;
#84857 = CARTESIAN_POINT ( 'NONE',  ( 7.361572987183169658, 14.96726448433411960, -9.846743663894592657 ) ) ;
#84858 = CARTESIAN_POINT ( 'NONE',  ( 18.39792806157250382, 19.52224192338640663, 6.499999999999979572 ) ) ;
#84859 = VECTOR ( 'NONE', #13158, 1000.000000000000000 ) ;
#84860 =( NAMED_UNIT ( * ) PLANE_ANGLE_UNIT ( ) SI_UNIT ( $, .RADIAN. ) );
#84861 = CARTESIAN_POINT ( 'NONE',  ( 12.63842701281683922, 4.550597817667451750, -9.846743663894590881 ) ) ;
#84862 = CARTESIAN_POINT ( 'NONE',  ( 10.00000000000000178, 32.25893115100078745, 9.846743663894594434 ) ) ;
#84863 = CARTESIAN_POINT ( 'NONE',  ( 20.88017736071110519, 20.56368534415484106, 2.639326808657452039E-16 ) ) ;
#84864 = CARTESIAN_POINT ( 'NONE',  ( -2.816281873526473856, 34.33196800326376064, 3.434112377981055619 ) ) ;
#84865 = CARTESIAN_POINT ( 'NONE',  ( 19.84674366389459266, 8.717264484334116048, -2.638427012816827677 ) ) ;
#84866 = CARTESIAN_POINT ( 'NONE',  ( -13.34343830728394309, 0.5000000000000004441, -6.852200678592783589 ) ) ;
#84867 = CARTESIAN_POINT ( 'NONE',  ( 7.361572987183170547, 47.05059781766745175, 9.846743663894590881 ) ) ;
#84868 = CARTESIAN_POINT ( 'NONE',  ( 7.361572987183169658, 34.96726448433411605, -9.846743663894592657 ) ) ;
#84869 = CARTESIAN_POINT ( 'NONE',  ( 20.36894250292379382, 23.67874883491397142, 10.36894250292379205 ) ) ;
#84870 = CARTESIAN_POINT ( 'NONE',  ( 17.96484262340118221, 31.18868534415483751, -7.964842623401177768 ) ) ;
#84871 = CARTESIAN_POINT ( 'NONE',  ( 20.88017736071110875, 15.77201867748817143, -2.915334737309920765 ) ) ;
#84872 = CARTESIAN_POINT ( 'NONE',  ( 19.42250999205614548, 50.98035201082151247, -5.440088680355545492 ) ) ;
#84873 = EDGE_CURVE ( 'NONE', #3878, #75561, #72357, .T. ) ;
#84874 = CARTESIAN_POINT ( 'NONE',  ( 2.035157376598824452, 33.68868534415484106, 7.964842623401179544 ) ) ;
#84875 = ORIENTED_EDGE ( 'NONE', *, *, #94690, .F. ) ;
#84876 = CARTESIAN_POINT ( 'NONE',  ( 13.43411237798106583, 37.66530133659708923, -12.81628187352647252 ) ) ;
#84877 = CARTESIAN_POINT ( 'NONE',  ( 7.084665262690076126, 34.10535201082151247, 10.88017736071109987 ) ) ;
#84878 = VECTOR ( 'NONE', #39821, 999.9999999999998863 ) ;
#84879 = EDGE_LOOP ( 'NONE', ( #72085, #36686, #29624, #30975, #66955, #42217 ) ) ;
#84880 = ADVANCED_FACE ( 'NONE', ( #33371 ), #26362, .T. ) ;
#84881 = CARTESIAN_POINT ( 'NONE',  ( 22.81628187352647785, 56.41530133659708213, 3.434112377981063169 ) ) ;
#84882 = CARTESIAN_POINT ( 'NONE',  ( 17.96484262340118221, 54.93868534415484106, 7.964842623401181321 ) ) ;
#84883 = VERTEX_POINT ( 'NONE', #3890 ) ;
#84884 = CARTESIAN_POINT ( 'NONE',  ( 7.084665262690076126, 52.02201867748816255, -10.88017736071110164 ) ) ;
#84885 = PLANE ( 'NONE',  #80113 ) ;
#84886 = COLOUR_RGB ( '', 0.31764706, 0.68627451, 0.89019608) ;
#84887 = CARTESIAN_POINT ( 'NONE',  ( 19.42250999205614548, 40.98035201082150536, -5.440088680355545492 ) ) ;
#84888 = CARTESIAN_POINT ( 'NONE',  ( -0.2418659066527799606, 25.11633188102327097, 6.114288769123030320 ) ) ;
#84889 = CARTESIAN_POINT ( 'NONE',  ( 20.36894250292379738, 59.92874883491397497, -10.36894250292379027 ) ) ;
#84890 = CARTESIAN_POINT ( 'NONE',  ( 20.88017736071110164, 65.35535201082150536, 2.915334737309930979 ) ) ;
#84891 = CARTESIAN_POINT ( 'NONE',  ( -14.35840480524209894, 14.49999999999999112, 4.340070442838745102 ) ) ;
#84892 = LINE ( 'NONE', #60900, #23768 ) ;
#84893 = CARTESIAN_POINT ( 'NONE',  ( -13.75801628063875803, 4.618045246005505222E-16, -4.578972376164643698 ) ) ;
#84894 = CARTESIAN_POINT ( 'NONE',  ( 7.361572987183170547, 27.05059781766745175, 9.846743663894590881 ) ) ;
#84895 = EDGE_LOOP ( 'NONE', ( #27807, #36317, #49362, #94184 ) ) ;
#84896 = CARTESIAN_POINT ( 'NONE',  ( 0.1532563361054100626, 30.80059781766744820, -2.638427012816831230 ) ) ;
#84897 = CARTESIAN_POINT ( 'NONE',  ( 12.91533473730992121, 34.52201867748817676, 10.88017736071110164 ) ) ;
#84898 = CARTESIAN_POINT ( 'NONE',  ( 19.84674366389459621, 38.50893115100078745, 7.409399052514197653E-17 ) ) ;
#84900 = CARTESIAN_POINT ( 'NONE',  ( 4.559911319644449179, 68.89701867748817676, 9.422509992056141925 ) ) ;
#84899 = DIRECTION ( 'NONE',  ( 0.000000000000000000, 0.000000000000000000, 1.000000000000000000 ) ) ;
#84901 = CARTESIAN_POINT ( 'NONE',  ( 0.5774900079438607392, 48.48035201082150536, 5.440088680355550821 ) ) ;
#84902 = CARTESIAN_POINT ( 'NONE',  ( 22.26659068614894466, 58.88708216824729647, 7.082119434687054849 ) ) ;
#84903 = VECTOR ( 'NONE', #63553, 1000.000000000000000 ) ;
#84904 = EDGE_CURVE ( 'NONE', #42454, #56421, #18393, .T. ) ;
#84905 = CARTESIAN_POINT ( 'NONE',  ( 22.81628187352647785, 16.62363466993042138, 6.195893100308588602E-16 ) ) ;
#84906 = CARTESIAN_POINT ( 'NONE',  ( 7.595945211628325922, 15.00000000000000000, -12.35117874301639240 ) ) ;
#84907 = ORIENTED_EDGE ( 'NONE', *, *, #62317, .T. ) ;
#84908 = CARTESIAN_POINT ( 'NONE',  ( 16.40814093676324603, 27.45696800326375708, -11.09922568453594671 ) ) ;
#84909 = CARTESIAN_POINT ( 'NONE',  ( 17.96484262340118221, 26.18868534415483396, -7.964842623401177768 ) ) ;
#84910 = EDGE_CURVE ( 'NONE', #42957, #18747, #25157, .T. ) ;
#84911 = VECTOR ( 'NONE', #32852, 1000.000000000000000 ) ;
#84912 = ORIENTED_EDGE ( 'NONE', *, *, #34448, .T. ) ;
#84913 = CARTESIAN_POINT ( 'NONE',  ( 2.791683348922240793, 6.633931151000785675, 7.208316651077764092 ) ) ;
#84914 = VECTOR ( 'NONE', #9056, 1000.000000000000000 ) ;
#84915 = CARTESIAN_POINT ( 'NONE',  ( 18.52753015748618282, 43.92559781766745175, -4.923371831947291888 ) ) ;
#84916 = CARTESIAN_POINT ( 'NONE',  ( 5.076628168052703671, 41.84226448433411605, 8.527530157486179263 ) ) ;
#84917 = CARTESIAN_POINT ( 'NONE',  ( 0.6178305044545838731, 64.74863466993043914, 9.382169495545420901 ) ) ;
#84918 = CARTESIAN_POINT ( 'NONE',  ( 19.84674366389459266, 33.30059781766744464, 2.638427012816836559 ) ) ;
#84919 = CARTESIAN_POINT ( 'NONE',  ( 20.32896413005680714, 57.60497603579418069, -5.963430220938276349 ) ) ;
#84920 = FACE_OUTER_BOUND ( 'NONE', #4000, .T. ) ;
#84922 = CARTESIAN_POINT ( 'NONE',  ( 1.274849032794231007, 33.57228050351031357, 6.499999999999895195 ) ) ;
#84921 = CARTESIAN_POINT ( 'NONE',  ( 19.84674366389459266, 18.71726448433411960, -2.638427012816827677 ) ) ;
#84923 = CARTESIAN_POINT ( 'NONE',  ( -6.000000000000009770, 40.74999999999999289, 4.250000000000000000 ) ) ;
#84925 = ORIENTED_EDGE ( 'NONE', *, *, #70198, .T. ) ;
#84924 = CARTESIAN_POINT ( 'NONE',  ( 12.63842701281683034, 42.46726448433412315, 9.846743663894596210 ) ) ;
#84926 = CARTESIAN_POINT ( 'NONE',  ( 2.913501739333757889, 3.989000423594319145E-16, -14.20427779279535230 ) ) ;
#84927 = CARTESIAN_POINT ( 'NONE',  ( 13.43411237798105340, 10.58196800326375353, 12.81628187352647963 ) ) ;
#84928 = EDGE_CURVE ( 'NONE', #1559, #13075, #63389, .T. ) ;
#84929 = CARTESIAN_POINT ( 'NONE',  ( 12.91533473730992121, 49.52201867748817676, 10.88017736071110164 ) ) ;
#84930 = CARTESIAN_POINT ( 'NONE',  ( -4.164238869374099927, 42.01208216824728936, 3.795296366450308767 ) ) ;
#84931 = CARTESIAN_POINT ( 'NONE',  ( 19.54721792061764418, 97.02882860391893871, 5.000000000000000888 ) ) ;
#84932 = CARTESIAN_POINT ( 'NONE',  ( 10.00000000000000000, 40.55374883491397497, -14.16423886937410082 ) ) ;
#84933 = EDGE_CURVE ( 'NONE', #95526, #68087, #43919, .T. ) ;
#84934 = CARTESIAN_POINT ( 'NONE',  ( 6.204703633549690345, 60.76208216824730357, -14.16423886937410259 ) ) ;
#84935 = CARTESIAN_POINT ( 'NONE',  ( 24.16423886937409904, 19.09541550158063927, 3.795296366450317205 ) ) ;
#84937 = CARTESIAN_POINT ( 'NONE',  ( -2.815433093576920509, 14.63606915880330206, -14.73340885523757748 ) ) ;
#84936 = CARTESIAN_POINT ( 'NONE',  ( -4.164238869374099039, 26.80374883491397142, 8.674139862899312516E-16 ) ) ;
#84938 = CARTESIAN_POINT ( 'NONE',  ( 4.474002695404426966, -3.767820133606233579, -2.750000000000000000 ) ) ;
#84940 = CARTESIAN_POINT ( 'NONE',  ( 18.52753015748618282, 43.92559781766745175, -4.923371831947291888 ) ) ;
#84939 = CARTESIAN_POINT ( 'NONE',  ( 4.395712687241356775, -0.8323168404091368933, 2.750000000000000000 ) ) ;
#84941 = CARTESIAN_POINT ( 'NONE',  ( 20.88017736071110164, 35.35535201082150536, 2.915334737309930979 ) ) ;
#84942 = CARTESIAN_POINT ( 'NONE',  ( -1.909764518474394990, 0.000000000000000000, -5.107897229450617971 ) ) ;
#84943 = CARTESIAN_POINT ( 'NONE',  ( 5.076628168052703671, 66.84226448433412315, 8.527530157486179263 ) ) ;
#84944 = CARTESIAN_POINT ( 'NONE',  ( 19.67370888310397703, 87.37213813211816671, -5.438836974231106680 ) ) ;
#84945 = CARTESIAN_POINT ( 'NONE',  ( 2.791683348922237240, 35.38393115100079456, -7.208316651077763204 ) ) ;
#84946 = CARTESIAN_POINT ( 'NONE',  ( 19.38216949554541202, 55.99863466993041072, 9.382169495545424454 ) ) ;
#84947 = CARTESIAN_POINT ( 'NONE',  ( -5.204170427930421283E-15, -9.446251165086030355, -14.16423886937410082 ) ) ;
#84948 = CARTESIAN_POINT ( 'NONE',  ( 0.1532563361054100626, 45.80059781766745886, -2.638427012816831230 ) ) ;
#84949 = CARTESIAN_POINT ( 'NONE',  ( 19.84674366389459266, 58.71726448433411605, -2.638427012816827677 ) ) ;
#84950 = COLOUR_RGB ( '', 0.31764706, 0.68627451, 0.89019608) ;
#84951 = CARTESIAN_POINT ( 'NONE',  ( 10.00000000000000000, 35.55374883491396787, -14.16423886937410082 ) ) ;
#84952 = EDGE_LOOP ( 'NONE', ( #48227, #72664, #59520, #341 ) ) ;
#84953 = CARTESIAN_POINT ( 'NONE',  ( 2.917880565312950480, 15.97041550158063217, -12.26659068614894821 ) ) ;
#84954 = DIRECTION ( 'NONE',  ( 0.9990482215818573541, 0.000000000000000000, 0.04361938736534638067 ) ) ;
#84955 = CARTESIAN_POINT ( 'NONE',  ( 0.000000000000000000, 15.00000000000000000, 0.000000000000000000 ) ) ;
#84956 = CARTESIAN_POINT ( 'NONE',  ( 2.035157376598824452, 3.688685344154837953, 7.964842623401179544 ) ) ;
#84957 = CARTESIAN_POINT ( 'NONE',  ( 10.00000000000000178, 10.37363466993041961, 12.81628187352647608 ) ) ;
#84958 = CARTESIAN_POINT ( 'NONE',  ( -0.03447792253739248580, 55.15514106990690379, 6.401564815979742917 ) ) ;
#84959 = CARTESIAN_POINT ( 'NONE',  ( 10.00000000000000000, 4.758931151000784787, -9.846743663894594434 ) ) ;
#84960 = DIRECTION ( 'NONE',  ( -0.4461978131098006117, 0.000000000000000000, -0.8949343616020291048 ) ) ;
#84961 = DIRECTION ( 'NONE',  ( 0.000000000000000000, 0.000000000000000000, 1.000000000000000000 ) ) ;
#84962 = CARTESIAN_POINT ( 'NONE',  ( -4.164238869374099039, 56.80374883491397497, 8.674139862899312516E-16 ) ) ;
#84963 = LINE ( 'NONE', #62944, #75126 ) ;
#84964 = CARTESIAN_POINT ( 'NONE',  ( 0.5774900079438607392, 28.48035201082150891, 5.440088680355550821 ) ) ;
#84965 = CARTESIAN_POINT ( 'NONE',  ( 0.5774900079438607392, 18.48035201082150536, 5.440088680355550821 ) ) ;
#84966 = CARTESIAN_POINT ( 'NONE',  ( 2.791683348922240793, 51.63393115100078745, 7.208316651077764092 ) ) ;
#84967 = CARTESIAN_POINT ( 'NONE',  ( 2.791683348922240793, 51.63393115100078745, 7.208316651077764092 ) ) ;
#84968 = CARTESIAN_POINT ( 'NONE',  ( 5.076628168052704559, 0.1755978176674514724, -8.527530157486179263 ) ) ;
#84969 = ORIENTED_EDGE ( 'NONE', *, *, #33326, .F. ) ;
#84970 = CARTESIAN_POINT ( 'NONE',  ( 2.035157376598824452, 28.68868534415484106, 7.964842623401179544 ) ) ;
#84971 = CARTESIAN_POINT ( 'NONE',  ( 3.591859063236761518, 19.95696800326375353, 11.09922568453594849 ) ) ;
#84972 = CARTESIAN_POINT ( 'NONE',  ( 0.000000000000000000, 14.49999999999999822, 0.000000000000000000 ) ) ;
#84973 = AXIS2_PLACEMENT_3D ( 'NONE', #92383, #68913, #23422 ) ;
#84974 = CARTESIAN_POINT ( 'NONE',  ( 18.52753015748617571, 63.09226448433412315, 4.923371831947298993 ) ) ;
#84975 = CARTESIAN_POINT ( 'NONE',  ( 15.44008868035555793, 46.39701867748817676, -9.422509992056140149 ) ) ;
#84976 = CARTESIAN_POINT ( 'NONE',  ( 19.84674366389459266, 8.717264484334116048, -2.638427012816827677 ) ) ;
#84977 = CARTESIAN_POINT ( 'NONE',  ( 19.38216949554541557, 17.24863466993041783, -9.382169495545420901 ) ) ;
#84978 = CIRCLE ( 'NONE', #33919, 7.000000000000005329 ) ;
#84980 = CARTESIAN_POINT ( 'NONE',  ( 20.88017736071110519, 15.56368534415483751, 2.639326808657452039E-16 ) ) ;
#84979 = CARTESIAN_POINT ( 'NONE',  ( 2.035157376598822676, 57.43868534415484106, -7.964842623401177768 ) ) ;
#84981 = DIRECTION ( 'NONE',  ( 0.000000000000000000, 0.000000000000000000, -1.000000000000000000 ) ) ;
#84982 = VECTOR ( 'NONE', #9773, 1000.000000000000000 ) ;
#84983 = ORIENTED_EDGE ( 'NONE', *, *, #33632, .F. ) ;
#84984 = CARTESIAN_POINT ( 'NONE',  ( 0.000000000000000000, 14.49999999999999822, 0.000000000000000000 ) ) ;
#84985 = CARTESIAN_POINT ( 'NONE',  ( 19.72487221294571214, 24.78217586085238011, 6.499999999999993783 ) ) ;
#84986 = CARTESIAN_POINT ( 'NONE',  ( 12.91533473730993009, 46.60535201082150536, -10.88017736071109987 ) ) ;
#84988 = CARTESIAN_POINT ( 'NONE',  ( 6.204703633549690345, 12.84541550158063572, 14.16423886937410082 ) ) ;
#84987 = CARTESIAN_POINT ( 'NONE',  ( 6.565887622018943937, 43.08196800326374643, -12.81628187352647608 ) ) ;
#84989 = CARTESIAN_POINT ( 'NONE',  ( 7.361572987183170547, 22.05059781766745530, 9.846743663894590881 ) ) ;
#84990 = AXIS2_PLACEMENT_3D ( 'NONE', #1646, #62597, #85619 ) ;
#84991 = CARTESIAN_POINT ( 'NONE',  ( 10.00000000000000178, 62.25893115100078745, 9.846743663894594434 ) ) ;
#84992 = CARTESIAN_POINT ( 'NONE',  ( 10.00000000000000178, 17.25893115100078745, 9.846743663894594434 ) ) ;
#84993 = DIRECTION ( 'NONE',  ( 0.000000000000000000, 0.000000000000000000, -1.000000000000000000 ) ) ;
#84994 = CARTESIAN_POINT ( 'NONE',  ( -2.266590686148945544, 56.38708216824731068, -7.082119434687050408 ) ) ;
#84995 = EDGE_LOOP ( 'NONE', ( #68573, #59794, #8499, #58795 ) ) ;
#84996 = CIRCLE ( 'NONE', #11541, 62.50000000000000000 ) ;
#84997 = ADVANCED_FACE ( 'NONE', ( #85910 ), #75323, .T. ) ;
#84998 = CARTESIAN_POINT ( 'NONE',  ( 3.927832320392154575, 15.00000000000000000, 13.69797916712106733 ) ) ;
#84999 = ADVANCED_FACE ( 'NONE', ( #82824 ), #6836, .T. ) ;
#85000 = CARTESIAN_POINT ( 'NONE',  ( 20.88017736071110519, 10.56368534415483751, 2.639326808657452039E-16 ) ) ;
#85001 = PLANE ( 'NONE',  #43980 ) ;
#85002 = CIRCLE ( 'NONE', #14790, 2.000000000000001776 ) ;
#85003 = EDGE_LOOP ( 'NONE', ( #16833, #7791, #52303, #34977 ) ) ;
#85004 = ORIENTED_EDGE ( 'NONE', *, *, #73061, .F. ) ;
#85005 = CARTESIAN_POINT ( 'NONE',  ( 12.91533473730992121, 4.522018677488170546, 10.88017736071110164 ) ) ;
#85006 = CARTESIAN_POINT ( 'NONE',  ( 12.91533473730992121, 4.522018677488170546, 10.88017736071110164 ) ) ;
#85007 = CARTESIAN_POINT ( 'NONE',  ( 18.52753015748617571, 38.09226448433412315, 4.923371831947298993 ) ) ;
#85008 = CARTESIAN_POINT ( 'NONE',  ( -2.816281873526473856, 44.12363466993042493, 9.499525473075851096E-16 ) ) ;
#85009 = CARTESIAN_POINT ( 'NONE',  ( -8.201146098718011146, 12.29405489584603828, -8.255447149008286800 ) ) ;
#85011 = CARTESIAN_POINT ( 'NONE',  ( 17.08211943468705840, 15.13708216824730179, -12.26659068614894466 ) ) ;
#85010 = CARTESIAN_POINT ( 'NONE',  ( 0.000000000000000000, 14.49999999999999822, 0.000000000000000000 ) ) ;
#85012 = CARTESIAN_POINT ( 'NONE',  ( 20.88017736071110164, 30.35535201082151247, 2.915334737309930979 ) ) ;
#85013 = CARTESIAN_POINT ( 'NONE',  ( 19.42250999205614193, 5.147018677488171434, 5.440088680355555262 ) ) ;
#85014 = CARTESIAN_POINT ( 'NONE',  ( 17.20831665107776587, 39.13393115100079456, -7.208316651077762316 ) ) ;
#85015 = CARTESIAN_POINT ( 'NONE',  ( -4.096035146093331747, 15.00000000000000000, -13.90943910019262653 ) ) ;
#85016 = CARTESIAN_POINT ( 'NONE',  ( 0.1532563361054100626, 30.80059781766744820, -2.638427012816831230 ) ) ;
#85017 = DIRECTION ( 'NONE',  ( -0.000000000000000000, -1.000000000000000000, -0.000000000000000000 ) ) ;
#85018 = CARTESIAN_POINT ( 'NONE',  ( -12.81628187352647963, -41.08469866340290366, -3.434112377981046293 ) ) ;
#85019 = ORIENTED_EDGE ( 'NONE', *, *, #47511, .T. ) ;
#85020 = PLANE ( 'NONE',  #15828 ) ;
#85021 = CARTESIAN_POINT ( 'NONE',  ( -0.8801773607111008646, 63.27201867748817676, 2.915334737309923430 ) ) ;
#85022 = CARTESIAN_POINT ( 'NONE',  ( 17.20831665107776587, 54.13393115100079456, -7.208316651077762316 ) ) ;
#85023 = CARTESIAN_POINT ( 'NONE',  ( 4.559911319644449179, 27.23035201082150536, -9.422509992056141925 ) ) ;
#85025 = CARTESIAN_POINT ( 'NONE',  ( 6.565887622018943937, 28.08196800326375353, -12.81628187352647608 ) ) ;
#85024 = CARTESIAN_POINT ( 'NONE',  ( 12.91533473730992121, 9.522018677488171434, 10.88017736071110164 ) ) ;
#85026 = CARTESIAN_POINT ( 'NONE',  ( -0.3689425029237881626, 12.42874883491396609, 10.36894250292379027 ) ) ;
#85027 = CIRCLE ( 'NONE', #17936, 15.00000000000000000 ) ;
#85028 = ADVANCED_FACE ( 'NONE', ( #35352 ), #43830, .F. ) ;
#85029 = CARTESIAN_POINT ( 'NONE',  ( 22.81628187352647785, 41.41530133659708923, 3.434112377981063169 ) ) ;
#85030 = ORIENTED_EDGE ( 'NONE', *, *, #70024, .F. ) ;
#85031 = CARTESIAN_POINT ( 'NONE',  ( 7.361572987183169658, 49.96726448433410894, -9.846743663894592657 ) ) ;
#85033 = ADVANCED_FACE ( 'NONE', ( #59819 ), #80861, .T. ) ;
#85032 = CARTESIAN_POINT ( 'NONE',  ( 20.88017736071110164, 50.35535201082151247, 2.915334737309930979 ) ) ;
#85034 = CARTESIAN_POINT ( 'NONE',  ( 4.559911319644449179, 18.89701867748817321, 9.422509992056141925 ) ) ;
#85035 = EDGE_LOOP ( 'NONE', ( #67810, #20011, #20195, #50383, #48600, #58597 ) ) ;
#85036 = CARTESIAN_POINT ( 'NONE',  ( 0.5774900079438590739, 17.64701867748817321, -5.440088680355550821 ) ) ;
#85037 = ORIENTED_EDGE ( 'NONE', *, *, #74844, .F. ) ;
#85038 = CARTESIAN_POINT ( 'NONE',  ( 4.559911319644449179, 62.23035201082150536, -9.422509992056141925 ) ) ;
#85039 = CARTESIAN_POINT ( 'NONE',  ( 8.731067818237036704, 6.563309369127505732, 8.731067818237033151 ) ) ;
#85040 = CARTESIAN_POINT ( 'NONE',  ( 5.076628168052703671, 6.842264484334118713, 8.527530157486179263 ) ) ;
#85041 = CARTESIAN_POINT ( 'NONE',  ( 19.42250999205614548, 65.98035201082151957, -5.440088680355545492 ) ) ;
#85044 = ORIENTED_EDGE ( 'NONE', *, *, #77853, .F. ) ;
#85043 = AXIS2_PLACEMENT_3D ( 'NONE', #31348, #40837, #16366 ) ;
#85042 = CARTESIAN_POINT ( 'NONE',  ( 5.076628168052704559, 5.175597817667451750, -8.527530157486179263 ) ) ;
#85045 = CARTESIAN_POINT ( 'NONE',  ( 0.1532563361054082862, 36.21726448433410894, 2.638427012816831674 ) ) ;
#85046 = ORIENTED_EDGE ( 'NONE', *, *, #57257, .T. ) ;
#85047 = VERTEX_POINT ( 'NONE', #27357 ) ;
#85048 = LINE ( 'NONE', #77531, #2715 ) ;
#85049 = CARTESIAN_POINT ( 'NONE',  ( -4.164238869374099927, 12.01208216824730357, 3.795296366450308767 ) ) ;
#85050 = VECTOR ( 'NONE', #86424, 1000.000000000000000 ) ;
#85051 = CARTESIAN_POINT ( 'NONE',  ( -1.099225684535947600, 58.70696800326375353, -6.408140936763238038 ) ) ;
#85052 = PRESENTATION_LAYER_ASSIGNMENT (  '', '', ( #96270 ) ) ;
#85053 = CARTESIAN_POINT ( 'NONE',  ( 24.16423886937409904, 9.095415501580633943, 3.795296366450317205 ) ) ;
#85054 = CARTESIAN_POINT ( 'NONE',  ( 6.204703633549690345, 25.76208216824730712, -14.16423886937410259 ) ) ;
#85055 = DIRECTION ( 'NONE',  ( 0.000000000000000000, 0.000000000000000000, -1.000000000000000000 ) ) ;
#85056 = LINE ( 'NONE', #69565, #21052 ) ;
#85057 = CARTESIAN_POINT ( 'NONE',  ( 17.96484262340118221, 21.18868534415483396, -7.964842623401177768 ) ) ;
#85058 = CARTESIAN_POINT ( 'NONE',  ( 0.9413316022086010149, 68.45508385108956873, 6.499999999999960032 ) ) ;
#85059 = B_SPLINE_CURVE_WITH_KNOTS ( 'NONE', 3,
 ( #29608, #8119, #45614, #47082, #60112, #15633 ),
 .UNSPECIFIED., .F., .F.,
 ( 4, 2, 4 ),
 ( 0.0002800671705680612489, 0.0006862730573397339204, 0.001092478944111406483 ),
 .UNSPECIFIED. ) ;
#85061 = VECTOR ( 'NONE', #64764, 1000.000000000000000 ) ;
#85060 = CARTESIAN_POINT ( 'NONE',  ( 19.84674366389459266, 8.717264484334116048, -2.638427012816827677 ) ) ;
#85062 = CARTESIAN_POINT ( 'NONE',  ( 14.92337183194729633, 7.675597817667451750, 8.527530157486181039 ) ) ;
#85063 = CARTESIAN_POINT ( 'NONE',  ( -1.099225684535947600, 38.70696800326375353, -6.408140936763238038 ) ) ;
#85065 = EDGE_CURVE ( 'NONE', #31048, #75691, #6334, .T. ) ;
#85064 = CARTESIAN_POINT ( 'NONE',  ( 5.076628168052704559, 30.17559781766745175, -8.527530157486179263 ) ) ;
#85066 = DIRECTION ( 'NONE',  ( 0.000000000000000000, 0.000000000000000000, 1.000000000000000000 ) ) ;
#85067 = CARTESIAN_POINT ( 'NONE',  ( 21.09922568453595559, 22.04030133659708923, -6.408140936763230044 ) ) ;
#85068 = CIRCLE ( 'NONE', #41973, 7.000000000000000000 ) ;
#85069 = DIRECTION ( 'NONE',  ( 0.000000000000000000, 1.000000000000000000, 0.000000000000000000 ) ) ;
#85070 = CARTESIAN_POINT ( 'NONE',  ( 0.1532563361054100626, 10.80059781766745175, -2.638427012816831230 ) ) ;
#85071 = ORIENTED_EDGE ( 'NONE', *, *, #79370, .T. ) ;
#85072 = ORIENTED_EDGE ( 'NONE', *, *, #56214, .F. ) ;
#85073 = CARTESIAN_POINT ( 'NONE',  ( 19.42250999205614548, 35.98035201082151247, -5.440088680355545492 ) ) ;
#85074 = CARTESIAN_POINT ( 'NONE',  ( 24.16423886937409904, 39.09541550158062506, 3.795296366450317205 ) ) ;
#85075 = CARTESIAN_POINT ( 'NONE',  ( 10.00000000000000178, 42.25893115100078745, 9.846743663894594434 ) ) ;
#85076 = CARTESIAN_POINT ( 'NONE',  ( 7.361572987183169658, -0.03273551566588185635, -9.846743663894592657 ) ) ;
#85078 = CARTESIAN_POINT ( 'NONE',  ( 14.56368227077858357, 0.2306972965111892260, -3.337246381125186456 ) ) ;
#85077 = CARTESIAN_POINT ( 'NONE',  ( -2.816281873526471635, 53.91530133659709634, -3.434112377981056508 ) ) ;
#85079 = CARTESIAN_POINT ( 'NONE',  ( 15.44008868035555793, 31.39701867748817676, -9.422509992056140149 ) ) ;
#85080 = FACE_OUTER_BOUND ( 'NONE', #73261, .T. ) ;
#85081 = VECTOR ( 'NONE', #59451, 1000.000000000000114 ) ;
#85082 = CARTESIAN_POINT ( 'NONE',  ( 6.565887622018943937, 8.081968003263751754, -12.81628187352647608 ) ) ;
#85083 = CARTESIAN_POINT ( 'NONE',  ( 12.63842701281683922, 39.55059781766744464, -9.846743663894590881 ) ) ;
#85084 = CARTESIAN_POINT ( 'NONE',  ( -9.422509992056136596, 3.480352010821509356, 5.440088680355559703 ) ) ;
#85085 = CARTESIAN_POINT ( 'NONE',  ( 0.6178305044545818747, 53.49863466993041072, -9.382169495545419124 ) ) ;
#85086 = CARTESIAN_POINT ( 'NONE',  ( 9.779999999999990479, 20.99999999999999645, 0.000000000000000000 ) ) ;
#85088 = PLANE ( 'NONE',  #43185 ) ;
#85087 = CARTESIAN_POINT ( 'NONE',  ( 12.91533473730993009, 51.60535201082149825, -10.88017736071109987 ) ) ;
#85089 = CARTESIAN_POINT ( 'NONE',  ( 1.377727649040772586E-15, 12.49999999999999112, 11.25000000000000178 ) ) ;
#85090 = CARTESIAN_POINT ( 'NONE',  ( -42.16485527613927076, 107.5383484153110061, -5.000000000000000000 ) ) ;
#85091 = CARTESIAN_POINT ( 'NONE',  ( -0.8801773607110991993, 57.85535201082149825, -2.915334737309923874 ) ) ;
#85093 = CARTESIAN_POINT ( 'NONE',  ( -0.8801773607111008646, 58.27201867748816966, 2.915334737309923430 ) ) ;
#85092 = CIRCLE ( 'NONE', #91523, 14.49999999999999822 ) ;
#85094 = LINE ( 'NONE', #8601, #85650 ) ;
#85095 = CARTESIAN_POINT ( 'NONE',  ( 15.44008868035555260, 64.73035201082151957, 9.422509992056143702 ) ) ;
#85096 = CARTESIAN_POINT ( 'NONE',  ( 4.559911319644449179, 7.230352010821505360, -9.422509992056141925 ) ) ;
#85097 = CARTESIAN_POINT ( 'NONE',  ( 10.00000000000000178, 47.25893115100078745, 9.846743663894594434 ) ) ;
#85099 = CARTESIAN_POINT ( 'NONE',  ( -10.58223187591015169, 0.2306972965111903362, 10.54772123337523837 ) ) ;
#85098 = CARTESIAN_POINT ( 'NONE',  ( 4.559911319644449179, 27.23035201082150536, -9.422509992056141925 ) ) ;
#85100 = CARTESIAN_POINT ( 'NONE',  ( 3.591859063236761518, 29.95696800326375708, 11.09922568453594849 ) ) ;
#85101 = EDGE_LOOP ( 'NONE', ( #29987, #81387, #75298, #1570, #55048, #69384 ) ) ;
#85102 = CARTESIAN_POINT ( 'NONE',  ( 0.5774900079438590739, 42.64701867748816966, -5.440088680355550821 ) ) ;
#85103 = CARTESIAN_POINT ( 'NONE',  ( 22.81628187352648496, 11.83196800326375531, -3.434112377981050290 ) ) ;
#85104 = CARTESIAN_POINT ( 'NONE',  ( 0.5774900079438607392, 8.480352010821505360, 5.440088680355550821 ) ) ;
#85105 = CARTESIAN_POINT ( 'NONE',  ( 4.559911319644449179, 43.89701867748816966, 9.422509992056141925 ) ) ;
#85106 = CARTESIAN_POINT ( 'NONE',  ( -2.266590686148945544, 51.38708216824730357, -7.082119434687050408 ) ) ;
#85107 = CARTESIAN_POINT ( 'NONE',  ( 2.791683348922240793, 21.63393115100078745, 7.208316651077764092 ) ) ;
#85108 = CARTESIAN_POINT ( 'NONE',  ( 19.42250999205614193, 60.14701867748817676, 5.440088680355555262 ) ) ;
#85109 = CARTESIAN_POINT ( 'NONE',  ( -4.431036607602660382, 15.00000000000000000, 14.33059365769907956 ) ) ;
#85110 = CARTESIAN_POINT ( 'NONE',  ( -4.164238869374099039, 11.80374883491396965, 8.674139862899312516E-16 ) ) ;
#85111 = ADVANCED_FACE ( 'NONE', ( #57851 ), #28348, .T. ) ;
#85112 = STYLED_ITEM ( 'NONE', ( #87790 ), #66016 ) ;
#85113 =( LENGTH_UNIT ( ) NAMED_UNIT ( * ) SI_UNIT ( .MILLI., .METRE. ) );
#85114 = CARTESIAN_POINT ( 'NONE',  ( -4.873787042390880231, 0.000000000000000000, 13.39061984619915791 ) ) ;
#85115 = EDGE_LOOP ( 'NONE', ( #88056, #34507, #19833, #91272 ) ) ;
#85116 = ORIENTED_EDGE ( 'NONE', *, *, #25227, .T. ) ;
#85117 = CARTESIAN_POINT ( 'NONE',  ( 22.26659068614894466, 38.88708216824731068, 7.082119434687054849 ) ) ;
#85118 = CARTESIAN_POINT ( 'NONE',  ( 10.00000000000000000, 35.55374883491396787, -14.16423886937410082 ) ) ;
#85119 = CARTESIAN_POINT ( 'NONE',  ( 1.472469842513823179, 0.5922644843341181575, -4.923371831947296329 ) ) ;
#85120 = CARTESIAN_POINT ( 'NONE',  ( 19.84674366389459621, 58.50893115100078745, 7.409399052514197653E-17 ) ) ;
#85121 = CARTESIAN_POINT ( 'NONE',  ( -9.793382739345220855, -28.00152668697253233, 4.000000000000000000 ) ) ;
#85123 = CARTESIAN_POINT ( 'NONE',  ( 22.81628187352647785, 21.41530133659708923, 3.434112377981063169 ) ) ;
#85122 = CARTESIAN_POINT ( 'NONE',  ( 17.96484262340118221, 54.93868534415484106, 7.964842623401181321 ) ) ;
#85124 = CARTESIAN_POINT ( 'NONE',  ( 24.16423886937410614, 24.51208216824730002, -3.795296366450302550 ) ) ;
#85125 = CARTESIAN_POINT ( 'NONE',  ( 0.5774900079438607392, 23.48035201082150536, 5.440088680355550821 ) ) ;
#85126 = CIRCLE ( 'NONE', #53145, 0.2500000000000002220 ) ;
#85127 = CARTESIAN_POINT ( 'NONE',  ( 4.559911319644449179, 32.23035201082150536, -9.422509992056141925 ) ) ;
#85128 = CIRCLE ( 'NONE', #11673, 14.49999999999999822 ) ;
#85129 = CARTESIAN_POINT ( 'NONE',  ( 12.54397927573569049, 0.2306972965111904195, -8.117058495689017050 ) ) ;
#85130 = CARTESIAN_POINT ( 'NONE',  ( 0.5774900079438607392, 58.48035201082151247, 5.440088680355550821 ) ) ;
#85131 = B_SPLINE_CURVE_WITH_KNOTS ( 'NONE', 3,
 ( #17834, #78824, #94307, #49789, #48316, #71814, #4312, #87787, #11796, #26304, #40832, #19787, #25830, #3320, #93823, #19303, #25353, #10334, #72292, #42303, #55836, #50276, #72775, #42797 ),
 .UNSPECIFIED., .F., .F.,
 ( 4, 2, 2, 2, 2, 2, 2, 2, 2, 2, 2, 4 ),
 ( 0.000000000000000000, 0.003100981433949152270, 0.006201962867898304539, 0.01240392573579660908, 0.02480785147159321816, 0.04961570294318642937, 0.06201962867898304366, 0.07442355441477965794, 0.08682748015057627222, 0.09302944301847457242, 0.09613042445242370171, 0.09923140588637283099 ),
 .UNSPECIFIED. ) ;
#85132 = AXIS2_PLACEMENT_3D ( 'NONE', #66631, #18676, #79665 ) ;
#85133 = CARTESIAN_POINT ( 'NONE',  ( -9.846743663894594434, -3.991068848999211660, 3.469446951953614189E-15 ) ) ;
#85134 = ORIENTED_EDGE ( 'NONE', *, *, #56782, .F. ) ;
#85135 = CARTESIAN_POINT ( 'NONE',  ( 8.673617379884035472E-16, 78.91966277462714174, 5.000000000000000000 ) ) ;
#85136 = MECHANICAL_DESIGN_GEOMETRIC_PRESENTATION_REPRESENTATION (  '', ( #46792 ), #89908 ) ;
#85137 = DIRECTION ( 'NONE',  ( -0.9681476403781084095, 0.000000000000000000, 0.2503800040544389982 ) ) ;
#85138 = EDGE_LOOP ( 'NONE', ( #39900, #53752, #77631, #75292 ) ) ;
#85139 = CARTESIAN_POINT ( 'NONE',  ( 20.36894250292379738, 9.928748834913966093, -10.36894250292379027 ) ) ;
#85141 = CARTESIAN_POINT ( 'NONE',  ( -4.164238869374099039, 61.80374883491397497, 8.674139862899312516E-16 ) ) ;
#85140 = CARTESIAN_POINT ( 'NONE',  ( -2.266590686148945544, 62.22041550158063927, 7.082119434687048631 ) ) ;
#85143 = CARTESIAN_POINT ( 'NONE',  ( 0.1532563361054083140, 66.00893115100079456, 1.131784320476157264E-15 ) ) ;
#85142 = CARTESIAN_POINT ( 'NONE',  ( 10.00000000000000178, 32.25893115100078745, 9.846743663894594434 ) ) ;
#85144 = CARTESIAN_POINT ( 'NONE',  ( 0.000000000000000000, 9.750000000000000000, -3.750000000000000000 ) ) ;
#85145 = DIRECTION ( 'NONE',  ( -0.000000000000000000, -0.000000000000000000, 1.000000000000000000 ) ) ;
#85146 = ADVANCED_FACE ( 'NONE', ( #37843 ), #63051, .T. ) ;
#85147 = CARTESIAN_POINT ( 'NONE',  ( 19.38216949554541202, 10.99863466993042138, 9.382169495545424454 ) ) ;
#85148 = ORIENTED_EDGE ( 'NONE', *, *, #68798, .T. ) ;
#85149 = CARTESIAN_POINT ( 'NONE',  ( 20.36894250292379738, 49.92874883491396787, -10.36894250292379027 ) ) ;
#85150 = VERTEX_POINT ( 'NONE', #8318 ) ;
#85151 = EDGE_CURVE ( 'NONE', #30913, #7321, #68334, .T. ) ;
#85152 = CARTESIAN_POINT ( 'NONE',  ( 24.16423886937410614, 44.30374883491397497, 8.672049930838204340E-16 ) ) ;
#85153 = VERTEX_POINT ( 'NONE', #84327 ) ;
#85154 = CARTESIAN_POINT ( 'NONE',  ( 15.44008868035555793, 21.39701867748817321, -9.422509992056140149 ) ) ;
#85155 = CARTESIAN_POINT ( 'NONE',  ( -0.8801773607110991993, 37.85535201082151247, -2.915334737309923874 ) ) ;
#85156 = CARTESIAN_POINT ( 'NONE',  ( 0.1532563361054100626, 45.80059781766745886, -2.638427012816831230 ) ) ;
#85157 = CARTESIAN_POINT ( 'NONE',  ( -0.8801773607111008646, 38.27201867748816255, 2.915334737309923430 ) ) ;
#85158 = DIRECTION ( 'NONE',  ( -0.7385627893568404989, 0.6741846973770935225, 0.000000000000000000 ) ) ;
#85159 = CARTESIAN_POINT ( 'NONE',  ( 20.88017736071110164, 65.35535201082150536, 2.915334737309930979 ) ) ;
#85160 = CARTESIAN_POINT ( 'NONE',  ( -0.8801773607110991993, 27.85535201082150181, -2.915334737309923874 ) ) ;
#85161 = CIRCLE ( 'NONE', #14874, 0.2500000000000002220 ) ;
#85162 = DIRECTION ( 'NONE',  ( -0.000000000000000000, -1.000000000000000000, -0.000000000000000000 ) ) ;
#85163 = VECTOR ( 'NONE', #56148, 1000.000000000000000 ) ;
#85164 = CARTESIAN_POINT ( 'NONE',  ( 0.1532563361054083140, 1.008931151000784787, 1.131784320476157264E-15 ) ) ;
#85165 = CARTESIAN_POINT ( 'NONE',  ( -3.627483523066825644, -3.617667194781895024, 2.749999999999798828 ) ) ;
#85166 = ORIENTED_EDGE ( 'NONE', *, *, #28828, .F. ) ;
#85167 = CYLINDRICAL_SURFACE ( 'NONE', #57346, 0.2500000000000002220 ) ;
#85168 = CARTESIAN_POINT ( 'NONE',  ( 2.791683348922240793, 36.63393115100078035, 7.208316651077764092 ) ) ;
#85169 = CARTESIAN_POINT ( 'NONE',  ( -45.94000000000001194, 100.9999999999999858, 9.500000000000000000 ) ) ;
#85170 = CARTESIAN_POINT ( 'NONE',  ( -1.099225684535947600, 49.54030133659708923, 6.408140936763237150 ) ) ;
#85171 = SURFACE_SIDE_STYLE ('',( #17667 ) ) ;
#85172 = LINE ( 'NONE', #93152, #4417 ) ;
#85173 = CARTESIAN_POINT ( 'NONE',  ( 19.84674366389459621, 63.50893115100078745, 7.409399052514197653E-17 ) ) ;
#85174 = CARTESIAN_POINT ( 'NONE',  ( -43.14347499112858486, 107.3164382878165668, 4.970428862813641935 ) ) ;
#85175 = CARTESIAN_POINT ( 'NONE',  ( 18.52753015748617571, 48.09226448433412315, 4.923371831947298993 ) ) ;
#85176 = CARTESIAN_POINT ( 'NONE',  ( 22.26659068614894466, 43.88708216824729647, 7.082119434687054849 ) ) ;
#85177 = CARTESIAN_POINT ( 'NONE',  ( 5.076628168052704559, 65.17559781766745175, -8.527530157486179263 ) ) ;
#85178 = CARTESIAN_POINT ( 'NONE',  ( 18.52753015748617571, 13.09226448433411960, 4.923371831947298993 ) ) ;
#85179 = CARTESIAN_POINT ( 'NONE',  ( 19.38216949554541557, 52.24863466993041072, -9.382169495545420901 ) ) ;
#85180 = CARTESIAN_POINT ( 'NONE',  ( 17.20831665107776587, 62.88393115100078745, 7.208316651077764980 ) ) ;
#85182 = EDGE_CURVE ( 'NONE', #28677, #34483, #58250, .T. ) ;
#85181 = CARTESIAN_POINT ( 'NONE',  ( 7.084665262690076126, 57.02201867748817676, -10.88017736071110164 ) ) ;
#85183 = CARTESIAN_POINT ( 'NONE',  ( 19.84674366389459621, 48.50893115100078745, 7.409399052514197653E-17 ) ) ;
#85184 = CARTESIAN_POINT ( 'NONE',  ( 12.83294900548062678, 14.49999999999999112, 7.766300266068507874 ) ) ;
#85185 = MECHANICAL_DESIGN_GEOMETRIC_PRESENTATION_REPRESENTATION (  '', ( #21315 ), #34271 ) ;
#85186 = CARTESIAN_POINT ( 'NONE',  ( 2.035157376598822676, 57.43868534415484106, -7.964842623401177768 ) ) ;
#85187 = TOROIDAL_SURFACE ( 'NONE', #42099, 14.49999999999999822, 0.5000000000000000000 ) ;
#85188 = ORIENTED_EDGE ( 'NONE', *, *, #79817, .F. ) ;
#85189 = CARTESIAN_POINT ( 'NONE',  ( 20.36894250292379382, 48.67874883491396076, 10.36894250292379205 ) ) ;
#85190 = FACE_OUTER_BOUND ( 'NONE', #67696, .T. ) ;
#85191 = CARTESIAN_POINT ( 'NONE',  ( 17.96484262340118221, 24.93868534415484461, 7.964842623401181321 ) ) ;
#85193 = CARTESIAN_POINT ( 'NONE',  ( 4.559911319644449179, 62.23035201082150536, -9.422509992056141925 ) ) ;
#85192 = CARTESIAN_POINT ( 'NONE',  ( -1.099225684535947600, 14.54030133659708568, 6.408140936763237150 ) ) ;
#85194 = CARTESIAN_POINT ( 'NONE',  ( -8.439016546559980014, 3.939291001653719071E-16, 11.79122553964967679 ) ) ;
#85195 = AXIS2_PLACEMENT_3D ( 'NONE', #16993, #17491, #85484 ) ;
#85196 = EDGE_CURVE ( 'NONE', #23413, #92402, #12024, .T. ) ;
#85197 = CARTESIAN_POINT ( 'NONE',  ( 19.80777595082616216, 10.68878173731741121, -6.500000000000000888 ) ) ;
#85198 = LINE ( 'NONE', #85687, #53353 ) ;
#85200 = CARTESIAN_POINT ( 'NONE',  ( 2.603489959281592991, 11.58210964143329313, 6.500000000000006217 ) ) ;
#85199 = CARTESIAN_POINT ( 'NONE',  ( 20.88017736071110875, 50.77201867748817676, -2.915334737309920765 ) ) ;
#85201 = CARTESIAN_POINT ( 'NONE',  ( 18.52753015748617571, 38.09226448433412315, 4.923371831947298993 ) ) ;
#85202 = CARTESIAN_POINT ( 'NONE',  ( 14.99999999999998046, 69.99999999999998579, -6.250000000000000000 ) ) ;
#85203 = PRESENTATION_LAYER_ASSIGNMENT (  '', '', ( #29301 ) ) ;
#85204 = CARTESIAN_POINT ( 'NONE',  ( 10.36894250292379027, 28.67874883491397142, 10.36894250292378672 ) ) ;
#85205 = CARTESIAN_POINT ( 'NONE',  ( 13.43411237798105340, 10.58196800326375353, 12.81628187352647963 ) ) ;
#85207 = FILL_AREA_STYLE_COLOUR ( '', #13805 ) ;
#85206 = CARTESIAN_POINT ( 'NONE',  ( 12.91533473730993009, 11.60535201082150714, -10.88017736071109987 ) ) ;
#85208 = DIRECTION ( 'NONE',  ( 0.000000000000000000, -1.000000000000000000, 0.000000000000000000 ) ) ;
#85209 = CARTESIAN_POINT ( 'NONE',  ( -0.3689425029237898834, 36.17874883491396787, -10.36894250292378850 ) ) ;
#85210 = CARTESIAN_POINT ( 'NONE',  ( -2.266590686148945544, 67.22041550158063217, 7.082119434687048631 ) ) ;
#85211 = CARTESIAN_POINT ( 'NONE',  ( 5.076628168052703671, 31.84226448433412315, 8.527530157486179263 ) ) ;
#85212 =( BOUNDED_SURFACE ( )  B_SPLINE_SURFACE ( 1, 2, ( 
 ( #72427, #54964, #40485, #48946, #93963, #16995, #24502, #32471, #93471, #85982, #47474, #62966, #24998, #18956, #87440, #71945, #32958, #33437, #48458, #63462, #3953, #17493, #92970, #85486, #49433, #2006, #94448, #47958, #55481, #64431, #78468, #70486, #3469, #40976, #25489, #79454, #79937, #94938, #70983, #2988, #55974, #77974, #9481, #78957, #10953, #39984, #10468, #26440, #18461, #41479, #56938, #63934, #11444, #25961, #56462, #62465, #5441, #34424, #74397, #35913, #27425, #42929, #34920, #87926, #51911, #4938, #74898, #64916, #72925, #20430, #73410, #5920, #57433, #4455, #97426, #27912, #73912, #35418, #65912, #59397, #66410, #65417, #88922, #82396, #95442, #57918, #89409, #12423, #95942, #88428, #50917, #19443, #19928, #81413, #20925, #49932, #51414, #80930, #96942, #66907, #28415, #96442, #89900, #13412, #13920, #81903, #44398, #58911, #43898, #26935, #36414, #11938, #58405, #12915, #43412, #42443, #50422, #28892, #21416, #80440, #46378, #68399, #90882, #83887, #53887, #52398, #30376, #98427, #7899, #60879, #97932, #38394, #52885, #61862, #54360, #15416, #75387, #15892, #29882, #6905, #37417, #84870, #44885, #67904, #76866, #45898, #83395, #16379, #8382, #68896, #90381, #98920, #424, #30875, #76384, #46862, #38890, #14915, #37911, #61371, #91379, #91881, #23403, #84393, #60384, #69378, #22907, #53377, #900, #22410, #45385, #31362, #75891, #92367, #23893, #6396, #36911, #67403, #7415, #29389, #14415, #59890, #21919, #82897, #16874, #19688, #40366, #62851, #55856, #27176, #24381, #2383, #70372, #78843, #32837, #69876, #10354, #24874, #35168, #27674, #86352, #47349, #88175, #1889, #77851, #9361, #58159, #39865, #32348, #50175, #17854, #55356, #88669, #80685, #40853, #62349, #70867, #71357, #4206, #48340, #20178, #12181, #85861, #9868, #34676, #63339, #65172, #95692, #57679, #93349, #42687, #93844, #25371, #73166, #17373, #47843, #4705, #78347, #65668, #96190, #77354, #8865, #39381, #1396, #31851, #92853, #54848, #85362, #59153, #21672, #50681, #90636, #52158, #43663, #89660, #51172, #5188, #68158, #21170, #91135, #81173, #89167, #36670, #51673, #22161, #73661, #20678, #14672, #44147, #90142, #82151, #13663, #75644, #82651, #81656, #6166, #98679, #12673, #74149, #6656, #28661, #13165, #5683, #67158, #35675, #36168, #97683, #37172, #66159, #67665, #97193, #14167, #83147, #44651, #74655, #7155, #29631, #30128, #98175, #60634, #75146, #60139, #43173, #52643, #28172, #29145, #66668, #59651, #45138, #96692, #58665, #37659, #39632, #76139, #61612, #93100, #77604, #70122, #16132, #30621, #9613, #15656, #92130, #83646, #47105 ),
 ( #70615, #54603, #9118, #15161, #85119, #173, #46618, #667, #84629, #61128, #76625, #55097, #91637, #23155, #62595, #77115, #8145, #1150, #1644, #68643, #8628, #46139, #24136, #39137, #45641, #16629, #69139, #78107, #2141, #31610, #53630, #32096, #38638, #84149, #31117, #32599, #23655, #54116, #24630, #62102, #69626, #63097, #85616, #17133, #7665, #92611, #47612, #40113, #22660, #53137, #38156, #41114, #26098, #19083, #18594, #64558, #3603, #11577, #33091, #95575, #56593, #49087, #57075, #10600, #33573, #49559, #94093, #11091, #50069, #93598, #34554, #72558, #88060, #86110, #42570, #95066, #41608, #3117, #26572, #25135, #65049, #87571, #86602, #64067, #25614, #48091, #12067, #94582, #35049, #55613, #63584, #79590, #87083, #27062, #17621, #56107, #57561, #72077, #34062, #80071, #42091, #78603, #10113, #18109, #48586, #79087, #40612, #71605, #4090, #80572, #19571, #73054, #4587, #71109, #2637, #36047, #75530, #89053, #96075, #88556, #90520, #5070, #97567, #51050, #35557, #67547, #20564, #73545, #6540, #44035, #97079, #52046, #83037, #37049, #96573, #74536, #28050, #20059, #12561, #58546, #82537, #50562, #5572, #98060, #21556, #14055, #59043, #66047, #52529, #81540, #66551, #27557, #90033, #58049, #43064, #6057, #44537, #81057, #13050, #36555, #43544, #74039, #28551, #67045, #89549, #59539, #75033, #60025, #21058, #51551, #22056, #29517, #82039, #29031, #13550, #14554, #45023, #7043, #65549, #8518, #39020, #16520, #23538, #30512, #85007, #92988, #60524, #76022, #46994, #46031, #54981, #62484, #15546, #8031, #31005, #16016, #77488, #61995, #76515, #92495, #24522, #54492, #17010, #46506, #38530, #54011, #9000, #65, #69026, #560, #61501, #39516, #77006, #23040, #70009, #84520, #1533, #84024, #92009, #69515, #1031, #31492, #24024, #31978, #47488, #30019, #85499, #77991, #37548, #68039, #61015, #98565, #91014, #22547, #53017, #83532, #53513, #15050, #45522, #7553, #38043, #68534, #91526, #41491, #63949, #3483, #56475, #87941, #2024, #55989, #94951, #40993, #62981, #70502, #78484, #40502, #32973, #93486, #9999, #70996, #64931, #34437, #18970, #78971, #79471, #33454, #10481, #19457, #63478, #39997, #32487, #95458, #47975, #71960, #93981, #2519, #11459, #25503, #17510, #49449, #86962, #71491, #26452, #26949, #79953, #86491, #18476, #17990, #25011, #55498, #48473, #56953, #85999, #3005, #41977, #64444, #87455, #94461, #25979, #57450, #48961, #10970, #33940, #72440, #3969, #49950, #9496, #59410, #11953, #50435, #20940, #72938, #34936, #19942, #58927, #42457, #74411, #28908, #74917, #12438, #58420, #36928, #82412, #42946, #51429 ) ),
 .UNSPECIFIED., .F., .F., .F. ) 
 B_SPLINE_SURFACE_WITH_KNOTS ( ( 2, 2 ),
 ( 3, 2, 2, 2, 2, 2, 2, 2, 2, 2, 2, 2, 2, 2, 2, 2, 2, 2, 2, 2, 2, 2, 2, 2, 2, 2, 2, 2, 2, 2, 2, 2, 2, 2, 2, 2, 2, 2, 2, 2, 2, 2, 2, 2, 2, 2, 2, 2, 2, 2, 2, 2, 2, 2, 2, 2, 2, 2, 2, 2, 2, 2, 2, 2, 2, 2, 2, 2, 2, 2, 2, 2, 2, 2, 2, 2, 2, 2, 2, 2, 2, 2, 2, 2, 2, 2, 2, 2, 2, 2, 2, 2, 2, 2, 2, 2, 2, 2, 2, 2, 2, 2, 2, 2, 2, 2, 2, 2, 2, 2, 2, 2, 2, 2, 2, 2, 2, 2, 2, 2, 2, 2, 2, 2, 2, 2, 2, 2, 2, 2, 2, 2, 2, 2, 2, 2, 2, 2, 2, 2, 2, 2, 2, 2, 2, 2, 2, 2, 2, 2, 2, 2, 2, 2, 2, 2, 2, 2, 2, 2, 2, 2, 3 ),
 ( 0.000000000000000000, 1.000000000000000000 ),
 ( 0.000000000000000000, 0.005952380952380952051, 0.01190476190476190410, 0.01785714285714285615, 0.02380952380952380820, 0.02976190476190476025, 0.03571428571428571230, 0.04166666666666666435, 0.04761904761904761640, 0.05357142857142856845, 0.05952380952380952051, 0.06547619047619047949, 0.07142857142857142461, 0.07738095238095238360, 0.08333333333333332871, 0.08928571428571428770, 0.09523809523809523281, 0.1011904761904761918, 0.1071428571428571369, 0.1130952380952380959, 0.1190476190476190410, 0.1250000000000000000, 0.1309523809523809590, 0.1369047619047619180, 0.1428571428571428492, 0.1488095238095238082, 0.1547619047619047672, 0.1607142857142857262, 0.1666666666666666574, 0.1726190476190476164, 0.1785714285714285754, 0.1845238095238095344, 0.1904761904761904656, 0.1964285714285714246, 0.2023809523809523836, 0.2083333333333333426, 0.2142857142857142738, 0.2202380952380952328, 0.2261904761904761918, 0.2321428571428571508, 0.2380952380952380820, 0.2440476190476190410, 0.2500000000000000000, 0.2559523809523809312, 0.2619047619047619180, 0.2678571428571428492, 0.2738095238095238360, 0.2797619047619047672, 0.2857142857142856984, 0.2916666666666666852, 0.2976190476190476164, 0.3035714285714285476, 0.3095238095238095344, 0.3154761904761904656, 0.3214285714285714524, 0.3273809523809523836, 0.3333333333333333148, 0.3392857142857143016, 0.3452380952380952328, 0.3511904761904761640, 0.3571428571428571508, 0.3630952380952380820, 0.3690476190476190688, 0.3750000000000000000, 0.3809523809523809312, 0.3869047619047619180, 0.3928571428571428492, 0.3988095238095238360, 0.4047619047619047672, 0.4107142857142856984, 0.4166666666666666852, 0.4226190476190476164, 0.4285714285714285476, 0.4345238095238095344, 0.4404761904761904656, 0.4464285714285714524, 0.4523809523809523836, 0.4583333333333333148, 0.4642857142857143016, 0.4702380952380952328, 0.4761904761904761640, 0.4821428571428571508, 0.4880952380952380820, 0.4940476190476190688, 0.5000000000000000000, 0.5059523809523809312, 0.5119047619047618625, 0.5178571428571429047, 0.5238095238095238360, 0.5297619047619047672, 0.5357142857142856984, 0.5416666666666666297, 0.5476190476190476719, 0.5535714285714286031, 0.5595238095238095344, 0.5654761904761904656, 0.5714285714285713969, 0.5773809523809523281, 0.5833333333333333703, 0.5892857142857143016, 0.5952380952380952328, 0.6011904761904761640, 0.6071428571428570953, 0.6130952380952381375, 0.6190476190476190688, 0.6250000000000000000, 0.6309523809523809312, 0.6369047619047618625, 0.6428571428571429047, 0.6488095238095238360, 0.6547619047619047672, 0.6607142857142856984, 0.6666666666666666297, 0.6726190476190476719, 0.6785714285714286031, 0.6845238095238095344, 0.6904761904761904656, 0.6964285714285713969, 0.7023809523809523281, 0.7083333333333333703, 0.7142857142857143016, 0.7202380952380952328, 0.7261904761904761640, 0.7321428571428570953, 0.7380952380952381375, 0.7440476190476190688, 0.7500000000000000000, 0.7559523809523809312, 0.7619047619047618625, 0.7678571428571429047, 0.7738095238095238360, 0.7797619047619047672, 0.7857142857142856984, 0.7916666666666666297, 0.7976190476190476719, 0.8035714285714286031, 0.8095238095238095344, 0.8154761904761904656, 0.8214285714285713969, 0.8273809523809523281, 0.8333333333333333703, 0.8392857142857143016, 0.8452380952380952328, 0.8511904761904761640, 0.8571428571428570953, 0.8630952380952381375, 0.8690476190476190688, 0.8750000000000000000, 0.8809523809523809312, 0.8869047619047618625, 0.8928571428571429047, 0.8988095238095238360, 0.9047619047619047672, 0.9107142857142856984, 0.9166666666666666297, 0.9226190476190476719, 0.9285714285714286031, 0.9345238095238095344, 0.9404761904761904656, 0.9464285714285713969, 0.9523809523809523281, 0.9583333333333333703, 0.9642857142857143016 ),
 .UNSPECIFIED. ) 
 GEOMETRIC_REPRESENTATION_ITEM ( )  RATIONAL_B_SPLINE_SURFACE ( (
 ( 1.000000000000000000, 0.9659258262890683122, 1.000000000000000000, 0.9659258262890683122, 1.000000000000000000, 0.9659258262890683122, 1.000000000000000000, 0.9659258262890683122, 1.000000000000000000, 0.9659258262890683122, 1.000000000000000000, 0.9659258262890683122, 1.000000000000000000, 0.9659258262890683122, 1.000000000000000000, 0.9659258262890683122, 1.000000000000000000, 0.9659258262890683122, 1.000000000000000000, 0.9659258262890683122, 1.000000000000000000, 0.9659258262890683122, 1.000000000000000000, 0.9659258262890683122, 1.000000000000000000, 0.9659258262890683122, 1.000000000000000000, 0.9659258262890683122, 1.000000000000000000, 0.9659258262890683122, 1.000000000000000000, 0.9659258262890683122, 1.000000000000000000, 0.9659258262890683122, 1.000000000000000000, 0.9659258262890683122, 1.000000000000000000, 0.9659258262890683122, 1.000000000000000000, 0.9659258262890683122, 1.000000000000000000, 0.9659258262890683122, 1.000000000000000000, 0.9659258262890683122, 1.000000000000000000, 0.9659258262890683122, 1.000000000000000000, 0.9659258262890683122, 1.000000000000000000, 0.9659258262890683122, 1.000000000000000000, 0.9659258262890683122, 1.000000000000000000, 0.9659258262890683122, 1.000000000000000000, 0.9659258262890683122, 1.000000000000000000, 0.9659258262890683122, 1.000000000000000000, 0.9659258262890683122, 1.000000000000000000, 0.9659258262890683122, 1.000000000000000000, 0.9659258262890683122, 1.000000000000000000, 0.9659258262890683122, 1.000000000000000000, 0.9659258262890683122, 1.000000000000000000, 0.9659258262890683122, 1.000000000000000000, 0.9659258262890683122, 1.000000000000000000, 0.9659258262890683122, 1.000000000000000000, 0.9659258262890683122, 1.000000000000000000, 0.9659258262890683122, 1.000000000000000000, 0.9659258262890683122, 1.000000000000000000, 0.9659258262890683122, 1.000000000000000000, 0.9659258262890683122, 1.000000000000000000, 0.9659258262890683122, 1.000000000000000000, 0.9659258262890683122, 1.000000000000000000, 0.9659258262890683122, 1.000000000000000000, 0.9659258262890683122, 1.000000000000000000, 0.9659258262890683122, 1.000000000000000000, 0.9659258262890683122, 1.000000000000000000, 0.9659258262890683122, 1.000000000000000000, 0.9659258262890683122, 1.000000000000000000, 0.9659258262890683122, 1.000000000000000000, 0.9659258262890683122, 1.000000000000000000, 0.9659258262890683122, 1.000000000000000000, 0.9659258262890683122, 1.000000000000000000, 0.9659258262890683122, 1.000000000000000000, 0.9659258262890683122, 1.000000000000000000, 0.9659258262890683122, 1.000000000000000000, 0.9659258262890683122, 1.000000000000000000, 0.9659258262890683122, 1.000000000000000000, 0.9659258262890683122, 1.000000000000000000, 0.9659258262890683122, 1.000000000000000000, 0.9659258262890683122, 1.000000000000000000, 0.9659258262890683122, 1.000000000000000000, 0.9659258262890683122, 1.000000000000000000, 0.9659258262890683122, 1.000000000000000000, 0.9659258262890683122, 1.000000000000000000, 0.9659258262890683122, 1.000000000000000000, 0.9659258262890683122, 1.000000000000000000, 0.9659258262890683122, 1.000000000000000000, 0.9659258262890683122, 1.000000000000000000, 0.9659258262890683122, 1.000000000000000000, 0.9659258262890683122, 1.000000000000000000, 0.9659258262890683122, 1.000000000000000000, 0.9659258262890683122, 1.000000000000000000, 0.9659258262890683122, 1.000000000000000000, 0.9659258262890683122, 1.000000000000000000, 0.9659258262890683122, 1.000000000000000000, 0.9659258262890683122, 1.000000000000000000, 0.9659258262890683122, 1.000000000000000000, 0.9659258262890683122, 1.000000000000000000, 0.9659258262890683122, 1.000000000000000000, 0.9659258262890683122, 1.000000000000000000, 0.9659258262890683122, 1.000000000000000000, 0.9659258262890683122, 1.000000000000000000, 0.9659258262890683122, 1.000000000000000000, 0.9659258262890683122, 1.000000000000000000, 0.9659258262890683122, 1.000000000000000000, 0.9659258262890683122, 1.000000000000000000, 0.9659258262890683122, 1.000000000000000000, 0.9659258262890683122, 1.000000000000000000, 0.9659258262890683122, 1.000000000000000000, 0.9659258262890683122, 1.000000000000000000, 0.9659258262890683122, 1.000000000000000000, 0.9659258262890683122, 1.000000000000000000, 0.9659258262890683122, 1.000000000000000000, 0.9659258262890683122, 1.000000000000000000, 0.9659258262890683122, 1.000000000000000000, 0.9659258262890683122, 1.000000000000000000, 0.9659258262890683122, 1.000000000000000000, 0.9659258262890683122, 1.000000000000000000, 0.9659258262890683122, 1.000000000000000000, 0.9659258262890683122, 1.000000000000000000, 0.9659258262890683122, 1.000000000000000000, 0.9659258262890683122, 1.000000000000000000, 0.9659258262890683122, 1.000000000000000000, 0.9659258262890683122, 1.000000000000000000, 0.9659258262890683122, 1.000000000000000000, 0.9659258262890683122, 1.000000000000000000, 0.9659258262890683122, 1.000000000000000000, 0.9659258262890683122, 1.000000000000000000, 0.9659258262890683122, 1.000000000000000000, 0.9659258262890683122, 1.000000000000000000, 0.9659258262890683122, 1.000000000000000000, 0.9659258262890683122, 1.000000000000000000, 0.9659258262890683122, 1.000000000000000000, 0.9659258262890683122, 1.000000000000000000, 0.9659258262890683122, 1.000000000000000000, 0.9659258262890683122, 1.000000000000000000, 0.9659258262890683122, 1.000000000000000000, 0.9659258262890683122, 1.000000000000000000, 0.9659258262890683122, 1.000000000000000000, 0.9659258262890683122, 1.000000000000000000, 0.9659258262890683122, 1.000000000000000000, 0.9659258262890683122, 1.000000000000000000, 0.9659258262890683122, 1.000000000000000000, 0.9659258262890683122, 1.000000000000000000, 0.9659258262890683122, 1.000000000000000000, 0.9659258262890683122, 1.000000000000000000, 0.9659258262890683122, 1.000000000000000000, 0.9659258262890683122, 1.000000000000000000, 0.9659258262890683122, 1.000000000000000000, 0.9659258262890683122, 1.000000000000000000, 0.9659258262890683122, 1.000000000000000000, 0.9659258262890683122, 1.000000000000000000, 0.9659258262890683122, 1.000000000000000000, 0.9659258262890683122, 1.000000000000000000, 0.9659258262890683122, 1.000000000000000000, 0.9659258262890683122, 1.000000000000000000, 0.9659258262890683122, 1.000000000000000000, 0.9659258262890683122, 1.000000000000000000, 0.9659258262890683122, 1.000000000000000000, 0.9659258262890683122, 1.000000000000000000, 0.9659258262890683122, 1.000000000000000000, 0.9659258262890683122, 1.000000000000000000, 0.9659258262890683122, 1.000000000000000000, 0.9659258262890683122, 1.000000000000000000, 0.9659258262890683122, 1.000000000000000000, 0.9659258262890683122, 1.000000000000000000, 0.9659258262890683122, 1.000000000000000000, 0.9659258262890683122, 1.000000000000000000, 0.9659258262890683122, 1.000000000000000000, 0.9659258262890683122, 1.000000000000000000, 0.9659258262890683122, 1.000000000000000000, 0.9659258262890683122, 1.000000000000000000, 0.9659258262890683122, 1.000000000000000000, 0.9659258262890683122, 1.000000000000000000, 0.9659258262890683122, 1.000000000000000000, 0.9659258262890683122, 1.000000000000000000, 0.9659258262890683122, 1.000000000000000000, 0.9659258262890683122, 1.000000000000000000, 0.9659258262890683122, 1.000000000000000000, 0.9659258262890683122, 1.000000000000000000),
 ( 1.000000000000000000, 0.9659258262890683122, 1.000000000000000000, 0.9659258262890683122, 1.000000000000000000, 0.9659258262890683122, 1.000000000000000000, 0.9659258262890683122, 1.000000000000000000, 0.9659258262890683122, 1.000000000000000000, 0.9659258262890683122, 1.000000000000000000, 0.9659258262890683122, 1.000000000000000000, 0.9659258262890683122, 1.000000000000000000, 0.9659258262890683122, 1.000000000000000000, 0.9659258262890683122, 1.000000000000000000, 0.9659258262890683122, 1.000000000000000000, 0.9659258262890683122, 1.000000000000000000, 0.9659258262890683122, 1.000000000000000000, 0.9659258262890683122, 1.000000000000000000, 0.9659258262890683122, 1.000000000000000000, 0.9659258262890683122, 1.000000000000000000, 0.9659258262890683122, 1.000000000000000000, 0.9659258262890683122, 1.000000000000000000, 0.9659258262890683122, 1.000000000000000000, 0.9659258262890683122, 1.000000000000000000, 0.9659258262890683122, 1.000000000000000000, 0.9659258262890683122, 1.000000000000000000, 0.9659258262890683122, 1.000000000000000000, 0.9659258262890683122, 1.000000000000000000, 0.9659258262890683122, 1.000000000000000000, 0.9659258262890683122, 1.000000000000000000, 0.9659258262890683122, 1.000000000000000000, 0.9659258262890683122, 1.000000000000000000, 0.9659258262890683122, 1.000000000000000000, 0.9659258262890683122, 1.000000000000000000, 0.9659258262890683122, 1.000000000000000000, 0.9659258262890683122, 1.000000000000000000, 0.9659258262890683122, 1.000000000000000000, 0.9659258262890683122, 1.000000000000000000, 0.9659258262890683122, 1.000000000000000000, 0.9659258262890683122, 1.000000000000000000, 0.9659258262890683122, 1.000000000000000000, 0.9659258262890683122, 1.000000000000000000, 0.9659258262890683122, 1.000000000000000000, 0.9659258262890683122, 1.000000000000000000, 0.9659258262890683122, 1.000000000000000000, 0.9659258262890683122, 1.000000000000000000, 0.9659258262890683122, 1.000000000000000000, 0.9659258262890683122, 1.000000000000000000, 0.9659258262890683122, 1.000000000000000000, 0.9659258262890683122, 1.000000000000000000, 0.9659258262890683122, 1.000000000000000000, 0.9659258262890683122, 1.000000000000000000, 0.9659258262890683122, 1.000000000000000000, 0.9659258262890683122, 1.000000000000000000, 0.9659258262890683122, 1.000000000000000000, 0.9659258262890683122, 1.000000000000000000, 0.9659258262890683122, 1.000000000000000000, 0.9659258262890683122, 1.000000000000000000, 0.9659258262890683122, 1.000000000000000000, 0.9659258262890683122, 1.000000000000000000, 0.9659258262890683122, 1.000000000000000000, 0.9659258262890683122, 1.000000000000000000, 0.9659258262890683122, 1.000000000000000000, 0.9659258262890683122, 1.000000000000000000, 0.9659258262890683122, 1.000000000000000000, 0.9659258262890683122, 1.000000000000000000, 0.9659258262890683122, 1.000000000000000000, 0.9659258262890683122, 1.000000000000000000, 0.9659258262890683122, 1.000000000000000000, 0.9659258262890683122, 1.000000000000000000, 0.9659258262890683122, 1.000000000000000000, 0.9659258262890683122, 1.000000000000000000, 0.9659258262890683122, 1.000000000000000000, 0.9659258262890683122, 1.000000000000000000, 0.9659258262890683122, 1.000000000000000000, 0.9659258262890683122, 1.000000000000000000, 0.9659258262890683122, 1.000000000000000000, 0.9659258262890683122, 1.000000000000000000, 0.9659258262890683122, 1.000000000000000000, 0.9659258262890683122, 1.000000000000000000, 0.9659258262890683122, 1.000000000000000000, 0.9659258262890683122, 1.000000000000000000, 0.9659258262890683122, 1.000000000000000000, 0.9659258262890683122, 1.000000000000000000, 0.9659258262890683122, 1.000000000000000000, 0.9659258262890683122, 1.000000000000000000, 0.9659258262890683122, 1.000000000000000000, 0.9659258262890683122, 1.000000000000000000, 0.9659258262890683122, 1.000000000000000000, 0.9659258262890683122, 1.000000000000000000, 0.9659258262890683122, 1.000000000000000000, 0.9659258262890683122, 1.000000000000000000, 0.9659258262890683122, 1.000000000000000000, 0.9659258262890683122, 1.000000000000000000, 0.9659258262890683122, 1.000000000000000000, 0.9659258262890683122, 1.000000000000000000, 0.9659258262890683122, 1.000000000000000000, 0.9659258262890683122, 1.000000000000000000, 0.9659258262890683122, 1.000000000000000000, 0.9659258262890683122, 1.000000000000000000, 0.9659258262890683122, 1.000000000000000000, 0.9659258262890683122, 1.000000000000000000, 0.9659258262890683122, 1.000000000000000000, 0.9659258262890683122, 1.000000000000000000, 0.9659258262890683122, 1.000000000000000000, 0.9659258262890683122, 1.000000000000000000, 0.9659258262890683122, 1.000000000000000000, 0.9659258262890683122, 1.000000000000000000, 0.9659258262890683122, 1.000000000000000000, 0.9659258262890683122, 1.000000000000000000, 0.9659258262890683122, 1.000000000000000000, 0.9659258262890683122, 1.000000000000000000, 0.9659258262890683122, 1.000000000000000000, 0.9659258262890683122, 1.000000000000000000, 0.9659258262890683122, 1.000000000000000000, 0.9659258262890683122, 1.000000000000000000, 0.9659258262890683122, 1.000000000000000000, 0.9659258262890683122, 1.000000000000000000, 0.9659258262890683122, 1.000000000000000000, 0.9659258262890683122, 1.000000000000000000, 0.9659258262890683122, 1.000000000000000000, 0.9659258262890683122, 1.000000000000000000, 0.9659258262890683122, 1.000000000000000000, 0.9659258262890683122, 1.000000000000000000, 0.9659258262890683122, 1.000000000000000000, 0.9659258262890683122, 1.000000000000000000, 0.9659258262890683122, 1.000000000000000000, 0.9659258262890683122, 1.000000000000000000, 0.9659258262890683122, 1.000000000000000000, 0.9659258262890683122, 1.000000000000000000, 0.9659258262890683122, 1.000000000000000000, 0.9659258262890683122, 1.000000000000000000, 0.9659258262890683122, 1.000000000000000000, 0.9659258262890683122, 1.000000000000000000, 0.9659258262890683122, 1.000000000000000000, 0.9659258262890683122, 1.000000000000000000, 0.9659258262890683122, 1.000000000000000000, 0.9659258262890683122, 1.000000000000000000, 0.9659258262890683122, 1.000000000000000000, 0.9659258262890683122, 1.000000000000000000, 0.9659258262890683122, 1.000000000000000000, 0.9659258262890683122, 1.000000000000000000, 0.9659258262890683122, 1.000000000000000000, 0.9659258262890683122, 1.000000000000000000, 0.9659258262890683122, 1.000000000000000000, 0.9659258262890683122, 1.000000000000000000, 0.9659258262890683122, 1.000000000000000000, 0.9659258262890683122, 1.000000000000000000, 0.9659258262890683122, 1.000000000000000000, 0.9659258262890683122, 1.000000000000000000, 0.9659258262890683122, 1.000000000000000000, 0.9659258262890683122, 1.000000000000000000, 0.9659258262890683122, 1.000000000000000000, 0.9659258262890683122, 1.000000000000000000, 0.9659258262890683122, 1.000000000000000000, 0.9659258262890683122, 1.000000000000000000, 0.9659258262890683122, 1.000000000000000000, 0.9659258262890683122, 1.000000000000000000, 0.9659258262890683122, 1.000000000000000000, 0.9659258262890683122, 1.000000000000000000, 0.9659258262890683122, 1.000000000000000000, 0.9659258262890683122, 1.000000000000000000, 0.9659258262890683122, 1.000000000000000000, 0.9659258262890683122, 1.000000000000000000, 0.9659258262890683122, 1.000000000000000000, 0.9659258262890683122, 1.000000000000000000) ) ) 
 REPRESENTATION_ITEM ( '' )  SURFACE ( )  );
#85213 = CARTESIAN_POINT ( 'NONE',  ( 14.92337183194729633, 17.67559781766745175, 8.527530157486181039 ) ) ;
#85214 = CARTESIAN_POINT ( 'NONE',  ( 4.559911319644449179, 18.89701867748817321, 9.422509992056141925 ) ) ;
#85215 = VERTEX_POINT ( 'NONE', #54783 ) ;
#85216 = CARTESIAN_POINT ( 'NONE',  ( 19.84674366389459266, 43.71726448433410894, -2.638427012816827677 ) ) ;
#85217 = CARTESIAN_POINT ( 'NONE',  ( 7.084665262690076126, 32.02201867748816966, -10.88017736071110164 ) ) ;
#85218 = CARTESIAN_POINT ( 'NONE',  ( 12.63842701281683034, 57.46726448433411605, 9.846743663894596210 ) ) ;
#85220 = DIRECTION ( 'NONE',  ( -0.000000000000000000, -0.000000000000000000, 1.000000000000000000 ) ) ;
#85219 = CARTESIAN_POINT ( 'NONE',  ( 24.16423886937409904, 4.095415501580634832, 3.795296366450317205 ) ) ;
#85221 = CARTESIAN_POINT ( 'NONE',  ( 14.88232117145533628, 14.63606897487930425, 1.875237731503260452 ) ) ;
#85222 = UNCERTAINTY_MEASURE_WITH_UNIT (LENGTH_MEASURE( 1.000000000000000082E-05 ), #75035, 'distance_accuracy_value', 'NONE');
#85223 = CARTESIAN_POINT ( 'NONE',  ( 17.20831665107776587, 17.88393115100078745, 7.208316651077764980 ) ) ;
#85224 = CARTESIAN_POINT ( 'NONE',  ( -2.816281873526471635, 48.91530133659708213, -3.434112377981056508 ) ) ;
#85225 = CARTESIAN_POINT ( 'NONE',  ( 0.1532563361054100626, 55.80059781766745175, -2.638427012816831230 ) ) ;
#85226 = ORIENTED_EDGE ( 'NONE', *, *, #67277, .F. ) ;
#85227 = CARTESIAN_POINT ( 'NONE',  ( 5.076628168052704559, 15.17559781766745175, -8.527530157486179263 ) ) ;
#85228 = DIRECTION ( 'NONE',  ( -0.9588197348681947174, 0.000000000000000000, 0.2840153447039170387 ) ) ;
#85229 = CARTESIAN_POINT ( 'NONE',  ( 19.72487221294570858, 70.00000000000000000, 6.500000000000000888 ) ) ;
#85230 = CARTESIAN_POINT ( 'NONE',  ( 2.035157376598822676, 2.438685344154838397, -7.964842623401177768 ) ) ;
#85231 = CARTESIAN_POINT ( 'NONE',  ( 4.559911319644449179, 48.89701867748817676, 9.422509992056141925 ) ) ;
#85232 = FACE_OUTER_BOUND ( 'NONE', #81792, .T. ) ;
#85233 = CARTESIAN_POINT ( 'NONE',  ( 10.00000000000000178, 54.31368534415484106, 10.88017736071110342 ) ) ;
#85234 = CARTESIAN_POINT ( 'NONE',  ( 0.1532563361054083140, 41.00893115100078745, 1.131784320476157264E-15 ) ) ;
#85235 = CARTESIAN_POINT ( 'NONE',  ( 19.42250999205614548, 15.98035201082150714, -5.440088680355545492 ) ) ;
#85236 =( LENGTH_UNIT ( ) NAMED_UNIT ( * ) SI_UNIT ( .MILLI., .METRE. ) );
#85237 = CARTESIAN_POINT ( 'NONE',  ( 19.84674366389459266, 53.30059781766744464, 2.638427012816836559 ) ) ;
#85238 = ADVANCED_FACE ( 'NONE', ( #61304 ), #61795, .T. ) ;
#85239 = ORIENTED_EDGE ( 'NONE', *, *, #6438, .F. ) ;
#85240 = EDGE_LOOP ( 'NONE', ( #80053, #58526, #88351, #71505 ) ) ;
#85241 = CARTESIAN_POINT ( 'NONE',  ( 4.096035146093422341, 15.00000000000000000, 13.90943910019259810 ) ) ;
#85242 = CARTESIAN_POINT ( 'NONE',  ( 12.63842701281683922, 39.55059781766744464, -9.846743663894590881 ) ) ;
#85243 = CARTESIAN_POINT ( 'NONE',  ( 2.791683348922240793, 16.63393115100078745, 7.208316651077764092 ) ) ;
#85244 = CARTESIAN_POINT ( 'NONE',  ( -2.816281873526471635, 53.91530133659709634, -3.434112377981056508 ) ) ;
#85246 = CARTESIAN_POINT ( 'NONE',  ( 5.076628168052704559, 55.17559781766745175, -8.527530157486179263 ) ) ;
#85245 = CARTESIAN_POINT ( 'NONE',  ( -0.8801773607111008646, 23.27201867748817676, 2.915334737309923430 ) ) ;
#85247 = LINE ( 'NONE', #25254, #61378 ) ;
#85248 = EDGE_CURVE ( 'NONE', #52573, #56319, #59644, .T. ) ;
#85249 = CARTESIAN_POINT ( 'NONE',  ( 6.204703633549690345, 45.76208216824729647, -14.16423886937410259 ) ) ;
#85250 = CARTESIAN_POINT ( 'NONE',  ( -0.3689425029237898834, 56.17874883491396076, -10.36894250292378850 ) ) ;
#85251 = CARTESIAN_POINT ( 'NONE',  ( 12.80781515976310203, -0.03417435944610275333, 6.246788841744411513 ) ) ;
#85252 = CARTESIAN_POINT ( 'NONE',  ( 17.99999999995698019, 77.36262727519604709, 4.161036774752517431 ) ) ;
#85253 = CARTESIAN_POINT ( 'NONE',  ( 20.88017736071110875, 45.77201867748816966, -2.915334737309920765 ) ) ;
#85254 = CARTESIAN_POINT ( 'NONE',  ( 0.1532563361054082862, 16.21726448433411960, 2.638427012816831674 ) ) ;
#85255 = CARTESIAN_POINT ( 'NONE',  ( -3.889970118577499747, -8.287734203612208361, 3.750000000000403233 ) ) ;
#85256 = ORIENTED_EDGE ( 'NONE', *, *, #45046, .T. ) ;
#85257 = DIRECTION ( 'NONE',  ( 1.000000000000000000, -0.000000000000000000, 0.000000000000000000 ) ) ;
#85258 = ORIENTED_EDGE ( 'NONE', *, *, #704, .T. ) ;
#85259 = ADVANCED_FACE ( 'NONE', ( #8802 ), #53313, .F. ) ;
#85260 = CARTESIAN_POINT ( 'NONE',  ( 14.92337183194729988, 14.34226448433411782, -8.527530157486177487 ) ) ;
#85261 = ORIENTED_EDGE ( 'NONE', *, *, #44833, .T. ) ;
#85262 = CARTESIAN_POINT ( 'NONE',  ( 24.16423886937410614, 14.51208216824730179, -3.795296366450302550 ) ) ;
#85263 = CARTESIAN_POINT ( 'NONE',  ( 7.361572987183169658, 24.96726448433412315, -9.846743663894592657 ) ) ;
#85264 = CARTESIAN_POINT ( 'NONE',  ( 12.91533473730993009, 46.60535201082150536, -10.88017736071109987 ) ) ;
#85265 = PRESENTATION_STYLE_ASSIGNMENT (( #54744 ) ) ;
#85266 = VERTEX_POINT ( 'NONE', #60326 ) ;
#85267 = CARTESIAN_POINT ( 'NONE',  ( 20.88017736071110164, 45.35535201082149115, 2.915334737309930979 ) ) ;
#85268 = ADVANCED_FACE ( 'NONE', ( #62282 ), #85299, .T. ) ;
#85269 = VECTOR ( 'NONE', #55216, 1000.000000000000000 ) ;
#85270 = EDGE_LOOP ( 'NONE', ( #13182, #79602, #81457, #17759 ) ) ;
#85271 = CARTESIAN_POINT ( 'NONE',  ( 17.08211943468705840, 10.13708216824730179, -12.26659068614894466 ) ) ;
#85272 = EDGE_CURVE ( 'NONE', #20606, #45049, #59853, .T. ) ;
#85273 = AXIS2_PLACEMENT_3D ( 'NONE', #33879, #56892, #33391 ) ;
#85274 = ORIENTED_EDGE ( 'NONE', *, *, #54887, .T. ) ;
#85275 = CARTESIAN_POINT ( 'NONE',  ( 19.38216949554541557, 22.24863466993041428, -9.382169495545420901 ) ) ;
#85276 = CARTESIAN_POINT ( 'NONE',  ( 7.361572987183169658, 4.967264484334119601, -9.846743663894592657 ) ) ;
#85277 = CARTESIAN_POINT ( 'NONE',  ( 20.88017736071110519, 5.563685344154837509, 2.639326808657452039E-16 ) ) ;
#85278 = CARTESIAN_POINT ( 'NONE',  ( 18.72515096720570327, 11.07228050351031712, -6.499999999999992006 ) ) ;
#85279 = CARTESIAN_POINT ( 'NONE',  ( 5.076628168052703671, 21.84226448433411960, 8.527530157486179263 ) ) ;
#85280 = CARTESIAN_POINT ( 'NONE',  ( -0.8801773607111008646, 28.27201867748817321, 2.915334737309923430 ) ) ;
#85281 = ORIENTED_EDGE ( 'NONE', *, *, #18867, .T. ) ;
#85282 = DIRECTION ( 'NONE',  ( -0.7253743710122912969, 0.000000000000000000, 0.6883545756937501370 ) ) ;
#85283 = CARTESIAN_POINT ( 'NONE',  ( 17.96484262340118221, 61.18868534415482685, -7.964842623401177768 ) ) ;
#85284 = CARTESIAN_POINT ( 'NONE',  ( 17.85158348494333325, 39.73726573380442773, -6.500000000000027534 ) ) ;
#85285 = CARTESIAN_POINT ( 'NONE',  ( 3.591859063236761518, 64.95696800326376774, 11.09922568453594849 ) ) ;
#85286 = CARTESIAN_POINT ( 'NONE',  ( -0.8801773607110991993, 57.85535201082149825, -2.915334737309923874 ) ) ;
#85287 =( BOUNDED_SURFACE ( )  B_SPLINE_SURFACE ( 1, 2, ( 
 ( #17029, #8049, #71016, #23559, #38549, #15564, #78505, #69044, #92029, #85519, #24540, #32504, #84539, #77025, #39040, #70027, #47995, #69534, #31515, #62014, #55516, #31997, #2538, #578, #86015, #32993, #31023, #54511, #1551, #10018, #92514, #40519, #63002, #63496, #93998, #61519, #47508, #85024, #16036, #46525, #25522, #16537, #47014, #77504, #9018, #39535, #62503, #93006, #55001, #78009, #9516, #40016, #70520, #2043, #88458, #65450, #49466, #64949, #73446, #56494, #27948, #94971, #78992, #86512, #56971, #18493, #27458, #41010, #63969, #80471, #49965, #4972, #25999, #71510, #10990, #26473, #33472, #57466, #35452, #80960, #48489, #87959, #87474, #10497, #41995, #65948, #96475, #86984, #48981, #19475, #18989, #50454, #34458, #79490, #11969, #42472, #72956, #18009, #72459, #41511, #95975, #3993, #19959, #71977, #95477, #3024, #3502, #79972, #11478, #4485, #34952, #57951, #12460, #42965, #94481, #26965, #33959, #64464, #81447, #96975, #37448, #66942, #12948, #43443, #89448, #37942, #98459, #83428, #89933, #90914, #58946, #73944, #29915, #52433, #97462, #98954, #44431, #97963, #75427, #20961, #28927, #21450, #13445, #60420, #14947, #28449, #5473, #51947, #50952, #88954, #13957, #59431, #90412, #74934, #51449, #82931, #68432, #6435, #14449, #58440, #29419, #22444, #20463, #81935, #43932, #74429, #35945, #52916, #59924, #66441, #36946, #7444, #6941, #5957, #67938, #67444, #82432, #36450, #21954, #44919, #45416, #75920, #62376, #15918, #453, #32377, #24415, #76415, #15445, #39411, #85393, #17404, #85890, #78376, #30410, #31390, #45926, #16906, #61890, #92395, #38919, #62882, #47871, #92882, #30903, #47381, #54881, #7930, #23920, #31878, #91415, #9897, #38427, #22941, #60912, #93379, #53409, #68924, #1426, #69906, #77880, #61397, #91908, #23433, #84901, #24906, #84421, #53912, #46409, #70399, #46891, #40401, #83916, #1918, #70895, #76897, #69407, #16414, #55389, #8412, #928, #9392, #39896, #54389, #77382, #8895, #10874, #2903, #55885, #19839, #71862, #42845, #2412, #40887, #94854, #32871, #94361, #25880, #19355, #79853, #34835, #56381, #93874, #4370, #80351, #64344, #11355, #88341, #71390, #63370, #41396, #25400, #86383, #3374, #33353, #42357, #17885, #78874, #95349, #64831, #50328, #63848, #48369, #86870, #57832, #10382, #87356, #26355, #26847, #56856, #18379, #49351, #80840, #57343, #33835, #18870, #41875, #72339, #65328, #3871, #49839, #48858, #34335, #95853, #79367, #87836, #11848, #72832, #27336, #12340, #90293, #20341, #96357, #73329, #97341, #65823, #74811, #20836, #81331, #90799, #36824, #5352, #97841, #74307, #73818 ),
 ( #27828, #58314, #35830, #52799, #14327, #98337, #5832, #6815, #66316, #88830, #44798, #67316, #13328, #14828, #59312, #13828, #21830, #96852, #81809, #36325, #28328, #75303, #29795, #43325, #50838, #66818, #12826, #4854, #28813, #43812, #6317, #89810, #58818, #29306, #83303, #21331, #59801, #35329, #44309, #37331, #89327, #51325, #51820, #82306, #52313, #67821, #82805, #60306, #22325, #93261, #92767, #24785, #24294, #92285, #46293, #75799, #7317, #68313, #70284, #83801, #77268, #30780, #15324, #47260, #39296, #91290, #30287, #54269, #1316, #32255, #1800, #55260, #45304, #76781, #60790, #31767, #8297, #38796, #53793, #77760, #68805, #84308, #22812, #16294, #85775, #39785, #37820, #46775, #15808, #98833, #816, #62757, #53293, #45806, #7814, #8779, #69295, #9275, #23808, #76297, #69787, #62261, #54760, #38309, #31270, #336, #85279, #61770, #61284, #91793, #84785, #23313, #16785, #79244, #10757, #87230, #41757, #18754, #49237, #95220, #95729, #41274, #32750, #57714, #25769, #70779, #40271, #48250, #27214, #57222, #42242, #48738, #49715, #17774, #2295, #87721, #11237, #56263, #17285, #3256, #56738, #34215, #78761, #86756, #71748, #71264, #19234, #72708, #86261, #63247, #33723, #9775, #47762, #64223, #18261, #79740, #94739, #10268, #72227, #78260, #26244, #3757, #93753, #64709, #80225, #25286, #40762, #2789, #33243, #55769, #11729, #26727, #63738, #4244, #65209, #34714, #94238, #67200, #36206, #89206, #19722, #50211, #12217, #14208, #27711, #21210, #73698, #58195, #90182, #82193, #35202, #73206, #97232, #44187, #75184, #44689, #37215, #88214, #20719, #4737, #74697, #51210, #81694, #96730, #21712, #12713, #28206, #65707, #59191, #67703, #82690, #80722, #89697, #58702, #42726, #43701, #6697, #98214, #88706, #50720, #51709, #13206, #52196, #66704, #20216, #13702, #6207, #36709, #29673, #74187, #81213, #97726, #5718, #96232, #43206, #28699, #5232, #35710, #29189, #59687, #66198, #69179, #46178, #76664, #92166, #31648, #211, #14710, #92646, #52684, #37699, #23691, #76179, #8182, #61168, #68197, #38679, #62138, #91676, #702, #60183, #31155, #16172, #22205, #98718, #60673, #22700, #7196, #77152, #61645, #30169, #23195, #90679, #84664, #83185, #8661, #54154, #53669, #45184, #75682, #83684, #91171, #30662, #1189, #46657, #84184, #53178, #15199, #15694, #39173, #69663, #45681, #7699, #38196, #68683, #50547, #51535, #66033, #37035, #82027, #13537, #59030, #83023, #74026, #89536, #96562, #21541, #98553, #45010, #12549, #52032, #21046, #43051, #6044, #68025, #37536, #51036, #13035, #82525, #44021, #14540, #97555, #81529, #14041, #44522 ) ),
 .UNSPECIFIED., .F., .F., .F. ) 
 B_SPLINE_SURFACE_WITH_KNOTS ( ( 2, 2 ),
 ( 3, 2, 2, 2, 2, 2, 2, 2, 2, 2, 2, 2, 2, 2, 2, 2, 2, 2, 2, 2, 2, 2, 2, 2, 2, 2, 2, 2, 2, 2, 2, 2, 2, 2, 2, 2, 2, 2, 2, 2, 2, 2, 2, 2, 2, 2, 2, 2, 2, 2, 2, 2, 2, 2, 2, 2, 2, 2, 2, 2, 2, 2, 2, 2, 2, 2, 2, 2, 2, 2, 2, 2, 2, 2, 2, 2, 2, 2, 2, 2, 2, 2, 2, 2, 2, 2, 2, 2, 2, 2, 2, 2, 2, 2, 2, 2, 2, 2, 2, 2, 2, 2, 2, 2, 2, 2, 2, 2, 2, 2, 2, 2, 2, 2, 2, 2, 2, 2, 2, 2, 2, 2, 2, 2, 2, 2, 2, 2, 2, 2, 2, 2, 2, 2, 2, 2, 2, 2, 2, 2, 2, 2, 2, 2, 2, 2, 2, 2, 2, 2, 2, 2, 2, 2, 2, 2, 2, 2, 2, 2, 2, 2, 3 ),
 ( 0.000000000000000000, 1.000000000000000000 ),
 ( 0.000000000000000000, 0.005952380952380952051, 0.01190476190476190410, 0.01785714285714285615, 0.02380952380952380820, 0.02976190476190476025, 0.03571428571428571230, 0.04166666666666666435, 0.04761904761904761640, 0.05357142857142856845, 0.05952380952380952051, 0.06547619047619047949, 0.07142857142857142461, 0.07738095238095238360, 0.08333333333333332871, 0.08928571428571428770, 0.09523809523809523281, 0.1011904761904761918, 0.1071428571428571369, 0.1130952380952380959, 0.1190476190476190410, 0.1250000000000000000, 0.1309523809523809590, 0.1369047619047619180, 0.1428571428571428492, 0.1488095238095238082, 0.1547619047619047672, 0.1607142857142857262, 0.1666666666666666574, 0.1726190476190476164, 0.1785714285714285754, 0.1845238095238095344, 0.1904761904761904656, 0.1964285714285714246, 0.2023809523809523836, 0.2083333333333333426, 0.2142857142857142738, 0.2202380952380952328, 0.2261904761904761918, 0.2321428571428571508, 0.2380952380952380820, 0.2440476190476190410, 0.2500000000000000000, 0.2559523809523809312, 0.2619047619047619180, 0.2678571428571428492, 0.2738095238095238360, 0.2797619047619047672, 0.2857142857142856984, 0.2916666666666666852, 0.2976190476190476164, 0.3035714285714285476, 0.3095238095238095344, 0.3154761904761904656, 0.3214285714285714524, 0.3273809523809523836, 0.3333333333333333148, 0.3392857142857143016, 0.3452380952380952328, 0.3511904761904761640, 0.3571428571428571508, 0.3630952380952380820, 0.3690476190476190688, 0.3750000000000000000, 0.3809523809523809312, 0.3869047619047619180, 0.3928571428571428492, 0.3988095238095238360, 0.4047619047619047672, 0.4107142857142856984, 0.4166666666666666852, 0.4226190476190476164, 0.4285714285714285476, 0.4345238095238095344, 0.4404761904761904656, 0.4464285714285714524, 0.4523809523809523836, 0.4583333333333333148, 0.4642857142857143016, 0.4702380952380952328, 0.4761904761904761640, 0.4821428571428571508, 0.4880952380952380820, 0.4940476190476190688, 0.5000000000000000000, 0.5059523809523809312, 0.5119047619047618625, 0.5178571428571429047, 0.5238095238095238360, 0.5297619047619047672, 0.5357142857142856984, 0.5416666666666666297, 0.5476190476190476719, 0.5535714285714286031, 0.5595238095238095344, 0.5654761904761904656, 0.5714285714285713969, 0.5773809523809523281, 0.5833333333333333703, 0.5892857142857143016, 0.5952380952380952328, 0.6011904761904761640, 0.6071428571428570953, 0.6130952380952381375, 0.6190476190476190688, 0.6250000000000000000, 0.6309523809523809312, 0.6369047619047618625, 0.6428571428571429047, 0.6488095238095238360, 0.6547619047619047672, 0.6607142857142856984, 0.6666666666666666297, 0.6726190476190476719, 0.6785714285714286031, 0.6845238095238095344, 0.6904761904761904656, 0.6964285714285713969, 0.7023809523809523281, 0.7083333333333333703, 0.7142857142857143016, 0.7202380952380952328, 0.7261904761904761640, 0.7321428571428570953, 0.7380952380952381375, 0.7440476190476190688, 0.7500000000000000000, 0.7559523809523809312, 0.7619047619047618625, 0.7678571428571429047, 0.7738095238095238360, 0.7797619047619047672, 0.7857142857142856984, 0.7916666666666666297, 0.7976190476190476719, 0.8035714285714286031, 0.8095238095238095344, 0.8154761904761904656, 0.8214285714285713969, 0.8273809523809523281, 0.8333333333333333703, 0.8392857142857143016, 0.8452380952380952328, 0.8511904761904761640, 0.8571428571428570953, 0.8630952380952381375, 0.8690476190476190688, 0.8750000000000000000, 0.8809523809523809312, 0.8869047619047618625, 0.8928571428571429047, 0.8988095238095238360, 0.9047619047619047672, 0.9107142857142856984, 0.9166666666666666297, 0.9226190476190476719, 0.9285714285714286031, 0.9345238095238095344, 0.9404761904761904656, 0.9464285714285713969, 0.9523809523809523281, 0.9583333333333333703, 0.9642857142857143016 ),
 .UNSPECIFIED. ) 
 GEOMETRIC_REPRESENTATION_ITEM ( )  RATIONAL_B_SPLINE_SURFACE ( (
 ( 1.000000000000000000, 0.9659258262890683122, 1.000000000000000000, 0.9659258262890683122, 1.000000000000000000, 0.9659258262890683122, 1.000000000000000000, 0.9659258262890683122, 1.000000000000000000, 0.9659258262890683122, 1.000000000000000000, 0.9659258262890683122, 1.000000000000000000, 0.9659258262890683122, 1.000000000000000000, 0.9659258262890683122, 1.000000000000000000, 0.9659258262890683122, 1.000000000000000000, 0.9659258262890683122, 1.000000000000000000, 0.9659258262890683122, 1.000000000000000000, 0.9659258262890683122, 1.000000000000000000, 0.9659258262890683122, 1.000000000000000000, 0.9659258262890683122, 1.000000000000000000, 0.9659258262890683122, 1.000000000000000000, 0.9659258262890683122, 1.000000000000000000, 0.9659258262890683122, 1.000000000000000000, 0.9659258262890683122, 1.000000000000000000, 0.9659258262890683122, 1.000000000000000000, 0.9659258262890683122, 1.000000000000000000, 0.9659258262890683122, 1.000000000000000000, 0.9659258262890683122, 1.000000000000000000, 0.9659258262890683122, 1.000000000000000000, 0.9659258262890683122, 1.000000000000000000, 0.9659258262890683122, 1.000000000000000000, 0.9659258262890683122, 1.000000000000000000, 0.9659258262890683122, 1.000000000000000000, 0.9659258262890683122, 1.000000000000000000, 0.9659258262890683122, 1.000000000000000000, 0.9659258262890683122, 1.000000000000000000, 0.9659258262890683122, 1.000000000000000000, 0.9659258262890683122, 1.000000000000000000, 0.9659258262890683122, 1.000000000000000000, 0.9659258262890683122, 1.000000000000000000, 0.9659258262890683122, 1.000000000000000000, 0.9659258262890683122, 1.000000000000000000, 0.9659258262890683122, 1.000000000000000000, 0.9659258262890683122, 1.000000000000000000, 0.9659258262890683122, 1.000000000000000000, 0.9659258262890683122, 1.000000000000000000, 0.9659258262890683122, 1.000000000000000000, 0.9659258262890683122, 1.000000000000000000, 0.9659258262890683122, 1.000000000000000000, 0.9659258262890683122, 1.000000000000000000, 0.9659258262890683122, 1.000000000000000000, 0.9659258262890683122, 1.000000000000000000, 0.9659258262890683122, 1.000000000000000000, 0.9659258262890683122, 1.000000000000000000, 0.9659258262890683122, 1.000000000000000000, 0.9659258262890683122, 1.000000000000000000, 0.9659258262890683122, 1.000000000000000000, 0.9659258262890683122, 1.000000000000000000, 0.9659258262890683122, 1.000000000000000000, 0.9659258262890683122, 1.000000000000000000, 0.9659258262890683122, 1.000000000000000000, 0.9659258262890683122, 1.000000000000000000, 0.9659258262890683122, 1.000000000000000000, 0.9659258262890683122, 1.000000000000000000, 0.9659258262890683122, 1.000000000000000000, 0.9659258262890683122, 1.000000000000000000, 0.9659258262890683122, 1.000000000000000000, 0.9659258262890683122, 1.000000000000000000, 0.9659258262890683122, 1.000000000000000000, 0.9659258262890683122, 1.000000000000000000, 0.9659258262890683122, 1.000000000000000000, 0.9659258262890683122, 1.000000000000000000, 0.9659258262890683122, 1.000000000000000000, 0.9659258262890683122, 1.000000000000000000, 0.9659258262890683122, 1.000000000000000000, 0.9659258262890683122, 1.000000000000000000, 0.9659258262890683122, 1.000000000000000000, 0.9659258262890683122, 1.000000000000000000, 0.9659258262890683122, 1.000000000000000000, 0.9659258262890683122, 1.000000000000000000, 0.9659258262890683122, 1.000000000000000000, 0.9659258262890683122, 1.000000000000000000, 0.9659258262890683122, 1.000000000000000000, 0.9659258262890683122, 1.000000000000000000, 0.9659258262890683122, 1.000000000000000000, 0.9659258262890683122, 1.000000000000000000, 0.9659258262890683122, 1.000000000000000000, 0.9659258262890683122, 1.000000000000000000, 0.9659258262890683122, 1.000000000000000000, 0.9659258262890683122, 1.000000000000000000, 0.9659258262890683122, 1.000000000000000000, 0.9659258262890683122, 1.000000000000000000, 0.9659258262890683122, 1.000000000000000000, 0.9659258262890683122, 1.000000000000000000, 0.9659258262890683122, 1.000000000000000000, 0.9659258262890683122, 1.000000000000000000, 0.9659258262890683122, 1.000000000000000000, 0.9659258262890683122, 1.000000000000000000, 0.9659258262890683122, 1.000000000000000000, 0.9659258262890683122, 1.000000000000000000, 0.9659258262890683122, 1.000000000000000000, 0.9659258262890683122, 1.000000000000000000, 0.9659258262890683122, 1.000000000000000000, 0.9659258262890683122, 1.000000000000000000, 0.9659258262890683122, 1.000000000000000000, 0.9659258262890683122, 1.000000000000000000, 0.9659258262890683122, 1.000000000000000000, 0.9659258262890683122, 1.000000000000000000, 0.9659258262890683122, 1.000000000000000000, 0.9659258262890683122, 1.000000000000000000, 0.9659258262890683122, 1.000000000000000000, 0.9659258262890683122, 1.000000000000000000, 0.9659258262890683122, 1.000000000000000000, 0.9659258262890683122, 1.000000000000000000, 0.9659258262890683122, 1.000000000000000000, 0.9659258262890683122, 1.000000000000000000, 0.9659258262890683122, 1.000000000000000000, 0.9659258262890683122, 1.000000000000000000, 0.9659258262890683122, 1.000000000000000000, 0.9659258262890683122, 1.000000000000000000, 0.9659258262890683122, 1.000000000000000000, 0.9659258262890683122, 1.000000000000000000, 0.9659258262890683122, 1.000000000000000000, 0.9659258262890683122, 1.000000000000000000, 0.9659258262890683122, 1.000000000000000000, 0.9659258262890683122, 1.000000000000000000, 0.9659258262890683122, 1.000000000000000000, 0.9659258262890683122, 1.000000000000000000, 0.9659258262890683122, 1.000000000000000000, 0.9659258262890683122, 1.000000000000000000, 0.9659258262890683122, 1.000000000000000000, 0.9659258262890683122, 1.000000000000000000, 0.9659258262890683122, 1.000000000000000000, 0.9659258262890683122, 1.000000000000000000, 0.9659258262890683122, 1.000000000000000000, 0.9659258262890683122, 1.000000000000000000, 0.9659258262890683122, 1.000000000000000000, 0.9659258262890683122, 1.000000000000000000, 0.9659258262890683122, 1.000000000000000000, 0.9659258262890683122, 1.000000000000000000, 0.9659258262890683122, 1.000000000000000000, 0.9659258262890683122, 1.000000000000000000, 0.9659258262890683122, 1.000000000000000000, 0.9659258262890683122, 1.000000000000000000, 0.9659258262890683122, 1.000000000000000000, 0.9659258262890683122, 1.000000000000000000, 0.9659258262890683122, 1.000000000000000000, 0.9659258262890683122, 1.000000000000000000, 0.9659258262890683122, 1.000000000000000000, 0.9659258262890683122, 1.000000000000000000, 0.9659258262890683122, 1.000000000000000000, 0.9659258262890683122, 1.000000000000000000, 0.9659258262890683122, 1.000000000000000000, 0.9659258262890683122, 1.000000000000000000, 0.9659258262890683122, 1.000000000000000000, 0.9659258262890683122, 1.000000000000000000, 0.9659258262890683122, 1.000000000000000000, 0.9659258262890683122, 1.000000000000000000, 0.9659258262890683122, 1.000000000000000000, 0.9659258262890683122, 1.000000000000000000, 0.9659258262890683122, 1.000000000000000000, 0.9659258262890683122, 1.000000000000000000, 0.9659258262890683122, 1.000000000000000000, 0.9659258262890683122, 1.000000000000000000, 0.9659258262890683122, 1.000000000000000000, 0.9659258262890683122, 1.000000000000000000, 0.9659258262890683122, 1.000000000000000000, 0.9659258262890683122, 1.000000000000000000),
 ( 1.000000000000000000, 0.9659258262890683122, 1.000000000000000000, 0.9659258262890683122, 1.000000000000000000, 0.9659258262890683122, 1.000000000000000000, 0.9659258262890683122, 1.000000000000000000, 0.9659258262890683122, 1.000000000000000000, 0.9659258262890683122, 1.000000000000000000, 0.9659258262890683122, 1.000000000000000000, 0.9659258262890683122, 1.000000000000000000, 0.9659258262890683122, 1.000000000000000000, 0.9659258262890683122, 1.000000000000000000, 0.9659258262890683122, 1.000000000000000000, 0.9659258262890683122, 1.000000000000000000, 0.9659258262890683122, 1.000000000000000000, 0.9659258262890683122, 1.000000000000000000, 0.9659258262890683122, 1.000000000000000000, 0.9659258262890683122, 1.000000000000000000, 0.9659258262890683122, 1.000000000000000000, 0.9659258262890683122, 1.000000000000000000, 0.9659258262890683122, 1.000000000000000000, 0.9659258262890683122, 1.000000000000000000, 0.9659258262890683122, 1.000000000000000000, 0.9659258262890683122, 1.000000000000000000, 0.9659258262890683122, 1.000000000000000000, 0.9659258262890683122, 1.000000000000000000, 0.9659258262890683122, 1.000000000000000000, 0.9659258262890683122, 1.000000000000000000, 0.9659258262890683122, 1.000000000000000000, 0.9659258262890683122, 1.000000000000000000, 0.9659258262890683122, 1.000000000000000000, 0.9659258262890683122, 1.000000000000000000, 0.9659258262890683122, 1.000000000000000000, 0.9659258262890683122, 1.000000000000000000, 0.9659258262890683122, 1.000000000000000000, 0.9659258262890683122, 1.000000000000000000, 0.9659258262890683122, 1.000000000000000000, 0.9659258262890683122, 1.000000000000000000, 0.9659258262890683122, 1.000000000000000000, 0.9659258262890683122, 1.000000000000000000, 0.9659258262890683122, 1.000000000000000000, 0.9659258262890683122, 1.000000000000000000, 0.9659258262890683122, 1.000000000000000000, 0.9659258262890683122, 1.000000000000000000, 0.9659258262890683122, 1.000000000000000000, 0.9659258262890683122, 1.000000000000000000, 0.9659258262890683122, 1.000000000000000000, 0.9659258262890683122, 1.000000000000000000, 0.9659258262890683122, 1.000000000000000000, 0.9659258262890683122, 1.000000000000000000, 0.9659258262890683122, 1.000000000000000000, 0.9659258262890683122, 1.000000000000000000, 0.9659258262890683122, 1.000000000000000000, 0.9659258262890683122, 1.000000000000000000, 0.9659258262890683122, 1.000000000000000000, 0.9659258262890683122, 1.000000000000000000, 0.9659258262890683122, 1.000000000000000000, 0.9659258262890683122, 1.000000000000000000, 0.9659258262890683122, 1.000000000000000000, 0.9659258262890683122, 1.000000000000000000, 0.9659258262890683122, 1.000000000000000000, 0.9659258262890683122, 1.000000000000000000, 0.9659258262890683122, 1.000000000000000000, 0.9659258262890683122, 1.000000000000000000, 0.9659258262890683122, 1.000000000000000000, 0.9659258262890683122, 1.000000000000000000, 0.9659258262890683122, 1.000000000000000000, 0.9659258262890683122, 1.000000000000000000, 0.9659258262890683122, 1.000000000000000000, 0.9659258262890683122, 1.000000000000000000, 0.9659258262890683122, 1.000000000000000000, 0.9659258262890683122, 1.000000000000000000, 0.9659258262890683122, 1.000000000000000000, 0.9659258262890683122, 1.000000000000000000, 0.9659258262890683122, 1.000000000000000000, 0.9659258262890683122, 1.000000000000000000, 0.9659258262890683122, 1.000000000000000000, 0.9659258262890683122, 1.000000000000000000, 0.9659258262890683122, 1.000000000000000000, 0.9659258262890683122, 1.000000000000000000, 0.9659258262890683122, 1.000000000000000000, 0.9659258262890683122, 1.000000000000000000, 0.9659258262890683122, 1.000000000000000000, 0.9659258262890683122, 1.000000000000000000, 0.9659258262890683122, 1.000000000000000000, 0.9659258262890683122, 1.000000000000000000, 0.9659258262890683122, 1.000000000000000000, 0.9659258262890683122, 1.000000000000000000, 0.9659258262890683122, 1.000000000000000000, 0.9659258262890683122, 1.000000000000000000, 0.9659258262890683122, 1.000000000000000000, 0.9659258262890683122, 1.000000000000000000, 0.9659258262890683122, 1.000000000000000000, 0.9659258262890683122, 1.000000000000000000, 0.9659258262890683122, 1.000000000000000000, 0.9659258262890683122, 1.000000000000000000, 0.9659258262890683122, 1.000000000000000000, 0.9659258262890683122, 1.000000000000000000, 0.9659258262890683122, 1.000000000000000000, 0.9659258262890683122, 1.000000000000000000, 0.9659258262890683122, 1.000000000000000000, 0.9659258262890683122, 1.000000000000000000, 0.9659258262890683122, 1.000000000000000000, 0.9659258262890683122, 1.000000000000000000, 0.9659258262890683122, 1.000000000000000000, 0.9659258262890683122, 1.000000000000000000, 0.9659258262890683122, 1.000000000000000000, 0.9659258262890683122, 1.000000000000000000, 0.9659258262890683122, 1.000000000000000000, 0.9659258262890683122, 1.000000000000000000, 0.9659258262890683122, 1.000000000000000000, 0.9659258262890683122, 1.000000000000000000, 0.9659258262890683122, 1.000000000000000000, 0.9659258262890683122, 1.000000000000000000, 0.9659258262890683122, 1.000000000000000000, 0.9659258262890683122, 1.000000000000000000, 0.9659258262890683122, 1.000000000000000000, 0.9659258262890683122, 1.000000000000000000, 0.9659258262890683122, 1.000000000000000000, 0.9659258262890683122, 1.000000000000000000, 0.9659258262890683122, 1.000000000000000000, 0.9659258262890683122, 1.000000000000000000, 0.9659258262890683122, 1.000000000000000000, 0.9659258262890683122, 1.000000000000000000, 0.9659258262890683122, 1.000000000000000000, 0.9659258262890683122, 1.000000000000000000, 0.9659258262890683122, 1.000000000000000000, 0.9659258262890683122, 1.000000000000000000, 0.9659258262890683122, 1.000000000000000000, 0.9659258262890683122, 1.000000000000000000, 0.9659258262890683122, 1.000000000000000000, 0.9659258262890683122, 1.000000000000000000, 0.9659258262890683122, 1.000000000000000000, 0.9659258262890683122, 1.000000000000000000, 0.9659258262890683122, 1.000000000000000000, 0.9659258262890683122, 1.000000000000000000, 0.9659258262890683122, 1.000000000000000000, 0.9659258262890683122, 1.000000000000000000, 0.9659258262890683122, 1.000000000000000000, 0.9659258262890683122, 1.000000000000000000, 0.9659258262890683122, 1.000000000000000000, 0.9659258262890683122, 1.000000000000000000, 0.9659258262890683122, 1.000000000000000000, 0.9659258262890683122, 1.000000000000000000, 0.9659258262890683122, 1.000000000000000000, 0.9659258262890683122, 1.000000000000000000, 0.9659258262890683122, 1.000000000000000000, 0.9659258262890683122, 1.000000000000000000, 0.9659258262890683122, 1.000000000000000000, 0.9659258262890683122, 1.000000000000000000, 0.9659258262890683122, 1.000000000000000000, 0.9659258262890683122, 1.000000000000000000, 0.9659258262890683122, 1.000000000000000000, 0.9659258262890683122, 1.000000000000000000, 0.9659258262890683122, 1.000000000000000000, 0.9659258262890683122, 1.000000000000000000, 0.9659258262890683122, 1.000000000000000000, 0.9659258262890683122, 1.000000000000000000, 0.9659258262890683122, 1.000000000000000000, 0.9659258262890683122, 1.000000000000000000, 0.9659258262890683122, 1.000000000000000000, 0.9659258262890683122, 1.000000000000000000, 0.9659258262890683122, 1.000000000000000000, 0.9659258262890683122, 1.000000000000000000) ) ) 
 REPRESENTATION_ITEM ( '' )  SURFACE ( )  );
#85288 = ORIENTED_EDGE ( 'NONE', *, *, #81572, .T. ) ;
#85289 = CARTESIAN_POINT ( 'NONE',  ( 11.48952521350018685, 4.805858850777305443E-16, 8.845383562533823962 ) ) ;
#85290 = CARTESIAN_POINT ( 'NONE',  ( 19.84674366389459621, 33.50893115100078745, 7.409399052514197653E-17 ) ) ;
#85291 = CARTESIAN_POINT ( 'NONE',  ( 22.81628187352647785, 56.41530133659708213, 3.434112377981063169 ) ) ;
#85292 = CARTESIAN_POINT ( 'NONE',  ( 10.00000000000000178, 13.05374883491396787, 14.16423886937410082 ) ) ;
#85293 = CARTESIAN_POINT ( 'NONE',  ( 5.076628168052703671, 21.84226448433411960, 8.527530157486179263 ) ) ;
#85294 = CARTESIAN_POINT ( 'NONE',  ( 16.40814093676323893, 25.79030133659708923, 11.09922568453595026 ) ) ;
#85296 = DIRECTION ( 'NONE',  ( -1.000000000000000000, 0.000000000000000000, 0.000000000000000000 ) ) ;
#85295 =( NAMED_UNIT ( * ) SI_UNIT ( $, .STERADIAN. ) SOLID_ANGLE_UNIT ( ) );
#85297 = CARTESIAN_POINT ( 'NONE',  ( 2.035157376598824452, 53.68868534415484817, 7.964842623401179544 ) ) ;
#85298 = CARTESIAN_POINT ( 'NONE',  ( 5.076628168052703671, 61.84226448433412315, 8.527530157486179263 ) ) ;
#85299 = CYLINDRICAL_SURFACE ( 'NONE', #50336, 15.00000000000000000 ) ;
#85300 = CARTESIAN_POINT ( 'NONE',  ( 14.92337183194729988, 34.34226448433411605, -8.527530157486177487 ) ) ;
#85301 = CARTESIAN_POINT ( 'NONE',  ( 18.52753015748618282, 18.92559781766745175, -4.923371831947291888 ) ) ;
#85303 = ADVANCED_FACE ( 'NONE', ( #32771 ), #75833, .T. ) ;
#85302 = CARTESIAN_POINT ( 'NONE',  ( 15.44008868035555260, 14.73035201082150536, 9.422509992056143702 ) ) ;
#85304 = CARTESIAN_POINT ( 'NONE',  ( 22.81628187352648496, 21.83196800326374643, -3.434112377981050290 ) ) ;
#85305 = CARTESIAN_POINT ( 'NONE',  ( 17.20831665107776587, 27.88393115100078390, 7.208316651077764980 ) ) ;
#85306 = CARTESIAN_POINT ( 'NONE',  ( -8.004649405379435478, 84.50413264541207070, 3.999860480132925833 ) ) ;
#85307 = CARTESIAN_POINT ( 'NONE',  ( 20.88017736071110875, 15.77201867748817143, -2.915334737309920765 ) ) ;
#85309 = CARTESIAN_POINT ( 'NONE',  ( 0.5774900079438590739, 12.64701867748817321, -5.440088680355550821 ) ) ;
#85308 = CARTESIAN_POINT ( 'NONE',  ( 0.1532563361054100626, 40.80059781766745886, -2.638427012816831230 ) ) ;
#85310 =( LENGTH_UNIT ( ) NAMED_UNIT ( * ) SI_UNIT ( .MILLI., .METRE. ) );
#85311 = CARTESIAN_POINT ( 'NONE',  ( 0.5774900079438590739, 37.64701867748817676, -5.440088680355550821 ) ) ;
#85312 = CARTESIAN_POINT ( 'NONE',  ( -4.164238869374099927, 62.01208216824728936, 3.795296366450308767 ) ) ;
#85313 = CARTESIAN_POINT ( 'NONE',  ( 10.00000000000000000, 19.75893115100078390, -9.846743663894594434 ) ) ;
#85314 = CARTESIAN_POINT ( 'NONE',  ( 14.92337183194729988, 44.34226448433412315, -8.527530157486177487 ) ) ;
#85315 = CARTESIAN_POINT ( 'NONE',  ( -12.69000000000001371, 93.50000000000000000, 9.500000000000000000 ) ) ;
#85316 = DIRECTION ( 'NONE',  ( 0.04361938736534638067, 0.000000000000000000, -0.9990482215818573541 ) ) ;
#85317 = CARTESIAN_POINT ( 'NONE',  ( -19.89999999999999858, 98.99999999999998579, -7.750000000000000000 ) ) ;
#85318 = CARTESIAN_POINT ( 'NONE',  ( -0.3689425029237898834, 21.17874883491396432, -10.36894250292378850 ) ) ;
#85319 = CARTESIAN_POINT ( 'NONE',  ( 0.1532563361054083140, 41.00893115100078745, 1.131784320476157264E-15 ) ) ;
#85320 = DIRECTION ( 'NONE',  ( 0.000000000000000000, 0.000000000000000000, -1.000000000000000000 ) ) ;
#85321 = AXIS2_PLACEMENT_3D ( 'NONE', #68458, #55910, #48881 ) ;
#85322 = CARTESIAN_POINT ( 'NONE',  ( -4.164238869374099927, 57.01208216824731068, 3.795296366450308767 ) ) ;
#85323 = CARTESIAN_POINT ( 'NONE',  ( 18.52753015748617571, 23.09226448433411960, 4.923371831947298993 ) ) ;
#85325 = CARTESIAN_POINT ( 'NONE',  ( 13.14228782657335870, 14.63595249122788999, 7.230509711182328658 ) ) ;
#85324 = LINE ( 'NONE', #91850, #24410 ) ;
#85326 = CARTESIAN_POINT ( 'NONE',  ( 0.5774900079438590739, 52.64701867748817676, -5.440088680355550821 ) ) ;
#85327 = CARTESIAN_POINT ( 'NONE',  ( 0.6178305044545818747, 53.49863466993041072, -9.382169495545419124 ) ) ;
#85328 = CARTESIAN_POINT ( 'NONE',  ( 2.035157376598824452, 18.68868534415484106, 7.964842623401179544 ) ) ;
#85329 = CARTESIAN_POINT ( 'NONE',  ( 22.81628187352647785, 51.62363466993042493, 6.195893100308588602E-16 ) ) ;
#85330 = CARTESIAN_POINT ( 'NONE',  ( 10.00000000000000178, 62.25893115100078745, 9.846743663894594434 ) ) ;
#85331 = CARTESIAN_POINT ( 'NONE',  ( 5.076628168052704559, 20.17559781766745175, -8.527530157486179263 ) ) ;
#85332 = VERTEX_POINT ( 'NONE', #87252 ) ;
#85333 = PRESENTATION_LAYER_ASSIGNMENT (  '', '', ( #66187 ) ) ;
#85334 = LINE ( 'NONE', #76842, #54839 ) ;
#85335 = CARTESIAN_POINT ( 'NONE',  ( 9.779999999999988702, 26.99999999999999645, -2.900000000000000799 ) ) ;
#85336 = CARTESIAN_POINT ( 'NONE',  ( 10.00000000000000000, 50.55374883491396787, -14.16423886937410082 ) ) ;
#85337 = CARTESIAN_POINT ( 'NONE',  ( -4.164238869374099927, 12.01208216824730357, 3.795296366450308767 ) ) ;
#85338 = CARTESIAN_POINT ( 'NONE',  ( -0.8801773607111008646, 18.27201867748817321, 2.915334737309923430 ) ) ;
#85339 = CARTESIAN_POINT ( 'NONE',  ( 4.559911319644449179, 37.23035201082150536, -9.422509992056141925 ) ) ;
#85340 = CARTESIAN_POINT ( 'NONE',  ( 14.35840480524200657, 0.3639308199838637292, 4.340070442838945830 ) ) ;
#85341 = CARTESIAN_POINT ( 'NONE',  ( -46.82017113615791004, 100.6079546444643569, -9.324761308090124601 ) ) ;
#85342 = CARTESIAN_POINT ( 'NONE',  ( 1.472469842513823179, 1.425597817667451528, 4.923371831947296329 ) ) ;
#85343 = CYLINDRICAL_SURFACE ( 'NONE', #6652, 15.00000000000000000 ) ;
#85344 = CARTESIAN_POINT ( 'NONE',  ( 1.472469842513823179, 20.59226448433411960, -4.923371831947296329 ) ) ;
#85345 = CARTESIAN_POINT ( 'NONE',  ( 18.28836319691946599, 19.34492782695771140, 6.499999999999979572 ) ) ;
#85346 =( LENGTH_UNIT ( ) NAMED_UNIT ( * ) SI_UNIT ( .MILLI., .METRE. ) );
#85347 = CARTESIAN_POINT ( 'NONE',  ( 10.00000000000000000, 9.758931151000785675, -9.846743663894594434 ) ) ;
#85348 = CARTESIAN_POINT ( 'NONE',  ( 1.472469842513823179, 36.42559781766745175, 4.923371831947296329 ) ) ;
#85349 = CARTESIAN_POINT ( 'NONE',  ( 7.084665262690076126, 9.105352010821503583, 10.88017736071109987 ) ) ;
#85350 = EDGE_CURVE ( 'NONE', #18642, #74685, #18384, .T. ) ;
#85351 = CARTESIAN_POINT ( 'NONE',  ( 16.40814093676323893, 25.79030133659708923, 11.09922568453595026 ) ) ;
#85352 = CARTESIAN_POINT ( 'NONE',  ( 10.00000000000000178, 54.31368534415484106, 10.88017736071110342 ) ) ;
#85354 = CARTESIAN_POINT ( 'NONE',  ( 12.63842701281683922, 4.550597817667451750, -9.846743663894590881 ) ) ;
#85353 = CARTESIAN_POINT ( 'NONE',  ( 20.36894250292379738, 44.92874883491396787, -10.36894250292379027 ) ) ;
#85356 = EDGE_CURVE ( 'NONE', #85047, #24064, #78781, .T. ) ;
#85355 = DIRECTION ( 'NONE',  ( 0.000000000000000000, 1.000000000000000000, 0.000000000000000000 ) ) ;
#85357 = EDGE_CURVE ( 'NONE', #37711, #24202, #60445, .T. ) ;
#85358 = CARTESIAN_POINT ( 'NONE',  ( 18.52753015748617571, 48.09226448433412315, 4.923371831947298993 ) ) ;
#85360 = CARTESIAN_POINT ( 'NONE',  ( -4.164238869374099927, 12.01208216824730357, 3.795296366450308767 ) ) ;
#85359 = CARTESIAN_POINT ( 'NONE',  ( 10.00000000000000178, 37.25893115100078745, 9.846743663894594434 ) ) ;
#85361 = CARTESIAN_POINT ( 'NONE',  ( -4.164238869374098151, 21.59541550158063217, -3.795296366450310543 ) ) ;
#85362 = CARTESIAN_POINT ( 'NONE',  ( -0.8801773607111008646, 53.27201867748816966, 2.915334737309923430 ) ) ;
#85363 = CARTESIAN_POINT ( 'NONE',  ( 20.88017736071110875, 5.772018677488170546, -2.915334737309920765 ) ) ;
#85364 = CARTESIAN_POINT ( 'NONE',  ( 10.00000000000000000, 51.81368534415484106, -10.88017736071110342 ) ) ;
#85365 = CARTESIAN_POINT ( 'NONE',  ( 10.00000000000000000, 36.81368534415484106, -10.88017736071110342 ) ) ;
#85366 = ORIENTED_EDGE ( 'NONE', *, *, #47982, .F. ) ;
#85367 = CARTESIAN_POINT ( 'NONE',  ( -2.816281873526471635, 33.91530133659708213, -3.434112377981056508 ) ) ;
#85368 = CARTESIAN_POINT ( 'NONE',  ( 4.559911319644449179, 38.89701867748817676, 9.422509992056141925 ) ) ;
#85369 = ORIENTED_EDGE ( 'NONE', *, *, #5580, .T. ) ;
#85370 = MECHANICAL_DESIGN_GEOMETRIC_PRESENTATION_REPRESENTATION (  '', ( #75801 ), #90206 ) ;
#85371 = CARTESIAN_POINT ( 'NONE',  ( -1.099225684535947600, 59.54030133659708923, 6.408140936763237150 ) ) ;
#85372 = CARTESIAN_POINT ( 'NONE',  ( 17.96484262340118221, 44.93868534415483396, 7.964842623401181321 ) ) ;
#85373 = ORIENTED_EDGE ( 'NONE', *, *, #72351, .F. ) ;
#85374 = CARTESIAN_POINT ( 'NONE',  ( 17.96484262340118221, 49.93868534415484106, 7.964842623401181321 ) ) ;
#85375 = PRESENTATION_STYLE_ASSIGNMENT (( #71845 ) ) ;
#85376 = CARTESIAN_POINT ( 'NONE',  ( 1.602071938427497289, 27.02224192338640663, -6.499999999999968914 ) ) ;
#85377 = CARTESIAN_POINT ( 'NONE',  ( 0.1916775849787262787, 37.25868815902071418, -6.499999999999990230 ) ) ;
#85378 = CARTESIAN_POINT ( 'NONE',  ( 10.00000000000000000, 60.55374883491397497, -14.16423886937410082 ) ) ;
#85379 = CARTESIAN_POINT ( 'NONE',  ( 10.00000000000000000, -0.2410688489992152128, -9.846743663894594434 ) ) ;
#85380 = CARTESIAN_POINT ( 'NONE',  ( 2.917880565312950480, 5.970415501580634832, -12.26659068614894821 ) ) ;
#85381 =( LENGTH_UNIT ( ) NAMED_UNIT ( * ) SI_UNIT ( .MILLI., .METRE. ) );
#85382 = CARTESIAN_POINT ( 'NONE',  ( 20.88017736071110519, 15.56368534415483751, 2.639326808657452039E-16 ) ) ;
#85383 = CARTESIAN_POINT ( 'NONE',  ( 5.076628168052703671, 46.84226448433412315, 8.527530157486179263 ) ) ;
#85384 = VERTEX_POINT ( 'NONE', #70306 ) ;
#85385 = EDGE_CURVE ( 'NONE', #88316, #84655, #95429, .T. ) ;
#85386 = CARTESIAN_POINT ( 'NONE',  ( 0.1532563361054082862, 46.21726448433411605, 2.638427012816831674 ) ) ;
#85387 = COLOUR_RGB ( '', 0.66274510, 0.83137255, 0.94901961) ;
#85388 = CARTESIAN_POINT ( 'NONE',  ( 19.42250999205614193, 45.14701867748817676, 5.440088680355555262 ) ) ;
#85389 = CARTESIAN_POINT ( 'NONE',  ( 14.92337183194729988, 44.34226448433412315, -8.527530157486177487 ) ) ;
#85390 = CARTESIAN_POINT ( 'NONE',  ( 19.38216949554541202, 30.99863466993042138, 9.382169495545424454 ) ) ;
#85392 = CARTESIAN_POINT ( 'NONE',  ( 20.15039907845753930, 1.748846992468885198, 6.262539305110068177 ) ) ;
#85391 =( NAMED_UNIT ( * ) SI_UNIT ( $, .STERADIAN. ) SOLID_ANGLE_UNIT ( ) );
#85393 = CARTESIAN_POINT ( 'NONE',  ( 15.44008868035555793, 41.39701867748817676, -9.422509992056140149 ) ) ;
#85394 = CARTESIAN_POINT ( 'NONE',  ( -2.266590686148945544, 61.38708216824730357, -7.082119434687050408 ) ) ;
#85395 = EDGE_CURVE ( 'NONE', #77130, #69916, #7, .T. ) ;
#85396 = AXIS2_PLACEMENT_3D ( 'NONE', #50862, #20861, #43350 ) ;
#85397 = CARTESIAN_POINT ( 'NONE',  ( -2.816281873526473856, 24.12363466993042138, 9.499525473075851096E-16 ) ) ;
#85398 = LINE ( 'NONE', #98959, #49891 ) ;
#85399 = ORIENTED_EDGE ( 'NONE', *, *, #85476, .F. ) ;
#85400 = TOROIDAL_SURFACE ( 'NONE', #18313, 1.000000000000000000, 0.5000000000000000000 ) ;
#85401 = CARTESIAN_POINT ( 'NONE',  ( -1.099225684535947600, 28.70696800326375353, -6.408140936763238038 ) ) ;
#85402 = CARTESIAN_POINT ( 'NONE',  ( 2.035157376598824452, 18.68868534415484106, 7.964842623401179544 ) ) ;
#85403 = ORIENTED_EDGE ( 'NONE', *, *, #24550, .T. ) ;
#85404 = CARTESIAN_POINT ( 'NONE',  ( 20.88017736071110875, 65.77201867748817676, -2.915334737309920765 ) ) ;
#85405 = AXIS2_PLACEMENT_3D ( 'NONE', #62789, #17311, #16812 ) ;
#85406 = CARTESIAN_POINT ( 'NONE',  ( 5.076628168052704559, 45.17559781766745175, -8.527530157486179263 ) ) ;
#85408 = CARTESIAN_POINT ( 'NONE',  ( 14.92337183194729633, 37.67559781766745175, 8.527530157486181039 ) ) ;
#85407 = CARTESIAN_POINT ( 'NONE',  ( 18.52753015748618282, 8.925597817667451750, -4.923371831947291888 ) ) ;
#85409 = DIRECTION ( 'NONE',  ( 0.000000000000000000, 1.000000000000000000, 0.000000000000000000 ) ) ;
#85410 = CARTESIAN_POINT ( 'NONE',  ( -14.02068044289375592, 0.3639308153356248243, -5.331089937175855553 ) ) ;
#85411 = CARTESIAN_POINT ( 'NONE',  ( 19.84674366389459266, 28.30059781766745886, 2.638427012816836559 ) ) ;
#85412 = CARTESIAN_POINT ( 'NONE',  ( 20.15039907845753220, 56.74884699246889141, 6.262539305110074395 ) ) ;
#85413 = PLANE ( 'NONE',  #73947 ) ;
#85415 = CARTESIAN_POINT ( 'NONE',  ( 18.52753015748617571, 3.092264484334118269, 4.923371831947298993 ) ) ;
#85414 = CARTESIAN_POINT ( 'NONE',  ( 1.472469842513823179, 25.59226448433412315, -4.923371831947296329 ) ) ;
#85417 = ORIENTED_EDGE ( 'NONE', *, *, #71835, .T. ) ;
#85416 = CARTESIAN_POINT ( 'NONE',  ( 19.84674366389459266, 48.71726448433413026, -2.638427012816827677 ) ) ;
#85418 = CARTESIAN_POINT ( 'NONE',  ( 21.92686044187657046, 17.39664270246083788, -3.195792623639524432 ) ) ;
#85419 = CARTESIAN_POINT ( 'NONE',  ( 16.40814093676323893, 30.79030133659708923, 11.09922568453595026 ) ) ;
#85420 = VECTOR ( 'NONE', #88891, 999.9999999999998863 ) ;
#85421 = DIRECTION ( 'NONE',  ( 0.000000000000000000, 0.000000000000000000, -1.000000000000000000 ) ) ;
#85422 = CARTESIAN_POINT ( 'NONE',  ( -4.164238869374099927, 47.01208216824729647, 3.795296366450308767 ) ) ;
#85423 = CARTESIAN_POINT ( 'NONE',  ( 10.00000000000000178, 22.25893115100078745, 9.846743663894594434 ) ) ;
#85424 = CARTESIAN_POINT ( 'NONE',  ( 19.84674366389459621, 3.508931151000785231, 7.409399052514197653E-17 ) ) ;
#85425 = CARTESIAN_POINT ( 'NONE',  ( 19.50000000000000711, 98.59912998021083297, 5.000000000000000888 ) ) ;
#85426 = CARTESIAN_POINT ( 'NONE',  ( 22.26659068614895176, 39.72041550158063217, -7.082119434687042414 ) ) ;
#85427 = CARTESIAN_POINT ( 'NONE',  ( 12.63842701281683922, 64.55059781766745175, -9.846743663894590881 ) ) ;
#85428 = CARTESIAN_POINT ( 'NONE',  ( 13.79529636645030344, 53.26208216824730357, 14.16423886937410614 ) ) ;
#85429 = CARTESIAN_POINT ( 'NONE',  ( -4.164238869374099927, 17.01208216824730357, 3.795296366450308767 ) ) ;
#85431 = CARTESIAN_POINT ( 'NONE',  ( -42.50369195530269195, 107.9060299417078426, -4.500000000000001776 ) ) ;
#85430 = CARTESIAN_POINT ( 'NONE',  ( 20.36894250292379382, 23.67874883491397142, 10.36894250292379205 ) ) ;
#85432 = CARTESIAN_POINT ( 'NONE',  ( 1.354709868695649577, 14.49999999999999112, -14.93870011653157448 ) ) ;
#85434 = CARTESIAN_POINT ( 'NONE',  ( 1.472469842513823179, 40.59226448433411605, -4.923371831947296329 ) ) ;
#85433 = CARTESIAN_POINT ( 'NONE',  ( 5.783743716948903213, -36.05632648177958544, 2.500000000000000888 ) ) ;
#85435 = CARTESIAN_POINT ( 'NONE',  ( 12.91533473730992121, 39.52201867748817676, 10.88017736071110164 ) ) ;
#85436 = FACE_OUTER_BOUND ( 'NONE', #26136, .T. ) ;
#85438 = EDGE_CURVE ( 'NONE', #84834, #20560, #64242, .T. ) ;
#85437 = VECTOR ( 'NONE', #24820, 1000.000000000000000 ) ;
#85439 = DIRECTION ( 'NONE',  ( 0.000000000000000000, 0.000000000000000000, 1.000000000000000000 ) ) ;
#85440 = CARTESIAN_POINT ( 'NONE',  ( 2.791683348922240793, 41.63393115100078745, 7.208316651077764092 ) ) ;
#85441 = CARTESIAN_POINT ( 'NONE',  ( 6.565887622018943937, 60.16530133659707502, 12.81628187352647430 ) ) ;
#85442 = CARTESIAN_POINT ( 'NONE',  ( -14.16423886937410082, -8.196251165086030355, 4.336808689942017736E-15 ) ) ;
#85443 = CARTESIAN_POINT ( 'NONE',  ( 0.1532563361054100626, 40.80059781766745886, -2.638427012816831230 ) ) ;
#85444 = CARTESIAN_POINT ( 'NONE',  ( 1.472469842513823179, 65.59226448433412315, -4.923371831947296329 ) ) ;
#85445 = B_SPLINE_CURVE_WITH_KNOTS ( 'NONE', 3,
 ( #53813, #61791, #23333, #54288, #2314, #46312, #1331, #92300, #17303, #76799, #62278, #55280, #69311, #92784, #53310, #16804, #70302, #47778, #832, #31292, #78276, #30803 ),
 .UNSPECIFIED., .F., .F.,
 ( 4, 2, 2, 2, 2, 2, 2, 2, 2, 2, 4 ),
 ( -6.000000000051943759E-08, 0.002788756152630997125, 0.005577572305261994760, 0.01115520461052398916, 0.02231046922104798144, 0.03346573383157196852, 0.04462099844209594518, 0.06693152766314391933, 0.07808679227366789599, 0.08366442457892990514, 0.08924205688419188653 ),
 .UNSPECIFIED. ) ;
#85446 = ORIENTED_EDGE ( 'NONE', *, *, #17197, .F. ) ;
#85447 = CARTESIAN_POINT ( 'NONE',  ( 22.26659068614895176, 19.72041550158063572, -7.082119434687042414 ) ) ;
#85448 = CARTESIAN_POINT ( 'NONE',  ( 0.2751277870542967463, 69.50000000000000000, -6.500000000000000888 ) ) ;
#85450 = DIRECTION ( 'NONE',  ( -0.2334453638558956767, 0.000000000000000000, -0.9723699203976788885 ) ) ;
#85449 = CARTESIAN_POINT ( 'NONE',  ( 19.39235739573469175, 44.87576471608600315, 6.499999999999993783 ) ) ;
#85451 = CARTESIAN_POINT ( 'NONE',  ( -0.8801773607111009756, 3.063685344154838397, 1.068504757029289695E-15 ) ) ;
#85452 = CARTESIAN_POINT ( 'NONE',  ( 10.00000000000000178, 15.37363466993042138, 12.81628187352647608 ) ) ;
#85453 = CARTESIAN_POINT ( 'NONE',  ( 10.00000000000000178, 69.31368534415484817, 10.88017736071110342 ) ) ;
#85454 = CARTESIAN_POINT ( 'NONE',  ( 4.395886033851783559, -0.8422402087859571784, -3.750000000000000000 ) ) ;
#85455 = FACE_OUTER_BOUND ( 'NONE', #96602, .T. ) ;
#85456 = CARTESIAN_POINT ( 'NONE',  ( 14.82269085861167035, 15.00000000000000000, 2.299529454047060550 ) ) ;
#85457 = CARTESIAN_POINT ( 'NONE',  ( 6.204703633549690345, 67.84541550158060375, 14.16423886937410082 ) ) ;
#85458 = DIRECTION ( 'NONE',  ( 0.000000000000000000, -1.000000000000000000, 0.000000000000000000 ) ) ;
#85459 = VECTOR ( 'NONE', #52010, 1000.000000000000000 ) ;
#85460 = CARTESIAN_POINT ( 'NONE',  ( 0.2751277870542965243, 3.218334437839379891, 6.500000000000000888 ) ) ;
#85461 = CARTESIAN_POINT ( 'NONE',  ( 20.88017736071110164, 25.35535201082150891, 2.915334737309930979 ) ) ;
#85462 = CARTESIAN_POINT ( 'NONE',  ( 7.084665262690076126, 44.10535201082151247, 10.88017736071109987 ) ) ;
#85463 = CARTESIAN_POINT ( 'NONE',  ( 22.81628187352647785, 6.415301336597088344, 3.434112377981063169 ) ) ;
#85464 = CARTESIAN_POINT ( 'NONE',  ( 14.92337183194729633, 57.67559781766745886, 8.527530157486181039 ) ) ;
#85465 = CARTESIAN_POINT ( 'NONE',  ( 10.00000000000000178, 65.37363466993042493, 12.81628187352647608 ) ) ;
#85466 = CARTESIAN_POINT ( 'NONE',  ( 18.52753015748617571, 3.092264484334118269, 4.923371831947298993 ) ) ;
#85467 = EDGE_CURVE ( 'NONE', #35320, #20878, #71767, .T. ) ;
#85468 = ORIENTED_EDGE ( 'NONE', *, *, #44718, .T. ) ;
#85469 = CARTESIAN_POINT ( 'NONE',  ( 0.5774900079438590739, 27.64701867748817676, -5.440088680355550821 ) ) ;
#85470 = CARTESIAN_POINT ( 'NONE',  ( 19.38216949554541202, 25.99863466993042138, 9.382169495545424454 ) ) ;
#85471 = CARTESIAN_POINT ( 'NONE',  ( 15.55000000000000071, 99.99999999999998579, 8.000000000000000000 ) ) ;
#85472 = EDGE_CURVE ( 'NONE', #67824, #49583, #78280, .T. ) ;
#85473 = CARTESIAN_POINT ( 'NONE',  ( 0.1532563361054100626, 60.80059781766744464, -2.638427012816831230 ) ) ;
#85474 = CARTESIAN_POINT ( 'NONE',  ( 15.44008868035555260, 44.73035201082151247, 9.422509992056143702 ) ) ;
#85475 = AXIS2_PLACEMENT_3D ( 'NONE', #21851, #88360, #97359 ) ;
#85476 = EDGE_CURVE ( 'NONE', #70888, #18498, #73990, .T. ) ;
#85477 = CARTESIAN_POINT ( 'NONE',  ( 5.076628168052704559, 15.17559781766745175, -8.527530157486179263 ) ) ;
#85478 = CARTESIAN_POINT ( 'NONE',  ( 13.43411237798106583, 37.66530133659708923, -12.81628187352647252 ) ) ;
#85480 = CARTESIAN_POINT ( 'NONE',  ( 18.72515096720570327, 16.07228050351031712, -6.499999999999992006 ) ) ;
#85479 = CARTESIAN_POINT ( 'NONE',  ( 2.035157376598824452, 58.68868534415482685, 7.964842623401179544 ) ) ;
#85481 = CARTESIAN_POINT ( 'NONE',  ( 0.1957200283969096621, 50.25733960839543357, 6.499999999999992895 ) ) ;
#85482 = CARTESIAN_POINT ( 'NONE',  ( 10.00000000000000178, 60.37363466993041783, 12.81628187352647608 ) ) ;
#85483 = ORIENTED_EDGE ( 'NONE', *, *, #81606, .T. ) ;
#85484 = DIRECTION ( 'NONE',  ( 0.000000000000000000, 0.000000000000000000, 1.000000000000000000 ) ) ;
#85485 = DIRECTION ( 'NONE',  ( 0.000000000000000000, 0.000000000000000000, 1.000000000000000000 ) ) ;
#85486 = CARTESIAN_POINT ( 'NONE',  ( 12.91533473730993009, 6.605352010821504471, -10.88017736071109987 ) ) ;
#85488 = CARTESIAN_POINT ( 'NONE',  ( 2.917880565312950480, 15.97041550158063217, -12.26659068614894821 ) ) ;
#85487 = CARTESIAN_POINT ( 'NONE',  ( 19.38216949554541202, 45.99863466993041072, 9.382169495545424454 ) ) ;
#85489 = CARTESIAN_POINT ( 'NONE',  ( 0.1532563361054083140, 16.00893115100078390, 1.131784320476157264E-15 ) ) ;
#85490 = CARTESIAN_POINT ( 'NONE',  ( 2.035157376598824452, 3.688685344154837953, 7.964842623401179544 ) ) ;
#85491 = CARTESIAN_POINT ( 'NONE',  ( 0.1532563361054082862, 26.21726448433411605, 2.638427012816831674 ) ) ;
#85492 = CARTESIAN_POINT ( 'NONE',  ( 2.917880565312950480, 50.97041550158064638, -12.26659068614894821 ) ) ;
#85493 = VERTEX_POINT ( 'NONE', #26259 ) ;
#85494 = CARTESIAN_POINT ( 'NONE',  ( 17.96484262340118221, 9.938685344154837509, 7.964842623401181321 ) ) ;
#85495 = DIRECTION ( 'NONE',  ( 0.000000000000000000, 0.000000000000000000, -1.000000000000000000 ) ) ;
#85496 = VERTEX_POINT ( 'NONE', #11258 ) ;
#85497 = CARTESIAN_POINT ( 'NONE',  ( -0.8801773607111009756, 13.06368534415483929, 1.068504757029289695E-15 ) ) ;
#85498 = CARTESIAN_POINT ( 'NONE',  ( 20.88017736071110519, 5.563685344154838397, 2.639326808657452039E-16 ) ) ;
#85499 = CARTESIAN_POINT ( 'NONE',  ( 5.076628168052703671, 46.84226448433412315, 8.527530157486179263 ) ) ;
#85500 = AXIS2_PLACEMENT_3D ( 'NONE', #16232, #91229, #76240 ) ;
#85501 = CARTESIAN_POINT ( 'NONE',  ( -1.099225684535947600, 54.54030133659708923, 6.408140936763237150 ) ) ;
#85502 = DIRECTION ( 'NONE',  ( 0.4461978131097943945, 0.000000000000000000, 0.8949343616020322134 ) ) ;
#85504 = CARTESIAN_POINT ( 'NONE',  ( 22.26659068614894466, 18.88708216824730002, 7.082119434687054849 ) ) ;
#85503 = CARTESIAN_POINT ( 'NONE',  ( 19.84674366389459266, 63.30059781766745886, 2.638427012816836559 ) ) ;
#85505 = CARTESIAN_POINT ( 'NONE',  ( 7.084665262690076126, 27.02201867748817676, -10.88017736071110164 ) ) ;
#85506 = CARTESIAN_POINT ( 'NONE',  ( -0.8801773607111008646, 3.272018677488171434, 2.915334737309923430 ) ) ;
#85507 = CARTESIAN_POINT ( 'NONE',  ( 7.361572987183169658, 59.96726448433410894, -9.846743663894592657 ) ) ;
#85508 = DIRECTION ( 'NONE',  ( 1.000000000000000000, 0.000000000000000000, 0.000000000000000000 ) ) ;
#85509 = CARTESIAN_POINT ( 'NONE',  ( 10.00000000000000000, 39.75893115100078745, -9.846743663894594434 ) ) ;
#85510 = ADVANCED_FACE ( 'NONE', ( #72246 ), #34233, .F. ) ;
#85511 = CARTESIAN_POINT ( 'NONE',  ( 0.000000000000000000, 15.00000000000000000, 0.000000000000000000 ) ) ;
#85512 = CARTESIAN_POINT ( 'NONE',  ( -9.846743663894590881, 31.21726448433413736, 2.638427012816840111 ) ) ;
#85513 = ORIENTED_EDGE ( 'NONE', *, *, #61551, .T. ) ;
#85514 = CARTESIAN_POINT ( 'NONE',  ( -6.767445849361070742, 14.63606917768312954, -13.38662304974510064 ) ) ;
#85515 = CARTESIAN_POINT ( 'NONE',  ( 2.035157376598822676, 62.43868534415483396, -7.964842623401177768 ) ) ;
#85516 = CARTESIAN_POINT ( 'NONE',  ( 1.472469842513823179, 61.42559781766745175, 4.923371831947296329 ) ) ;
#85518 = CARTESIAN_POINT ( 'NONE',  ( 2.035157376598822676, 47.43868534415484817, -7.964842623401177768 ) ) ;
#85517 = CARTESIAN_POINT ( 'NONE',  ( -0.8801773607110991993, 52.85535201082151247, -2.915334737309923874 ) ) ;
#85520 = CARTESIAN_POINT ( 'NONE',  ( 10.00000000000000000, 37.87363466993041783, -12.81628187352647608 ) ) ;
#85519 = CARTESIAN_POINT ( 'NONE',  ( 2.035157376598824452, 3.688685344154837953, 7.964842623401179544 ) ) ;
#85521 = CARTESIAN_POINT ( 'NONE',  ( 20.36894250292379382, 13.67874883491396965, 10.36894250292379205 ) ) ;
#85522 = AXIS2_PLACEMENT_3D ( 'NONE', #36263, #95789, #12765 ) ;
#85523 = CARTESIAN_POINT ( 'NONE',  ( 22.81628187352647785, 51.41530133659708923, 3.434112377981063169 ) ) ;
#85524 = ORIENTED_EDGE ( 'NONE', *, *, #19990, .F. ) ;
#85525 = CARTESIAN_POINT ( 'NONE',  ( 17.20831665107776587, 54.13393115100079456, -7.208316651077762316 ) ) ;
#85526 = CARTESIAN_POINT ( 'NONE',  ( 20.88017736071110875, 15.77201867748817143, -2.915334737309920765 ) ) ;
#85527 = ORIENTED_EDGE ( 'NONE', *, *, #4569, .F. ) ;
#85528 = CARTESIAN_POINT ( 'NONE',  ( 20.88017736071110164, 25.35535201082150891, 2.915334737309930979 ) ) ;
#85529 = VERTEX_POINT ( 'NONE', #80245 ) ;
#85530 = CARTESIAN_POINT ( 'NONE',  ( 4.559911319644449179, 68.89701867748817676, 9.422509992056141925 ) ) ;
#85531 = CARTESIAN_POINT ( 'NONE',  ( 4.559911319644449179, 67.23035201082150536, -9.422509992056141925 ) ) ;
#85532 = LINE ( 'NONE', #2055, #3693 ) ;
#85533 = CARTESIAN_POINT ( 'NONE',  ( 18.52753015748617571, 13.09226448433411960, 4.923371831947298993 ) ) ;
#85534 = CARTESIAN_POINT ( 'NONE',  ( 20.88017736071110164, 65.35535201082150536, 2.915334737309930979 ) ) ;
#85535 = DIRECTION ( 'NONE',  ( 1.257568779154408793E-17, 1.000000000000000000, -0.000000000000000000 ) ) ;
#85536 = CARTESIAN_POINT ( 'NONE',  ( -4.838527690343713772, 0.5000000000000004441, 14.19819177887723605 ) ) ;
#85537 = CARTESIAN_POINT ( 'NONE',  ( 7.084665262690076126, 64.10535201082150536, 10.88017736071109987 ) ) ;
#85538 = PRESENTATION_LAYER_ASSIGNMENT (  '', '', ( #58394 ) ) ;
#85540 = VERTEX_POINT ( 'NONE', #1821 ) ;
#85539 = CARTESIAN_POINT ( 'NONE',  ( 10.00000000000000178, 7.258931151000785675, 9.846743663894594434 ) ) ;
#85541 = CIRCLE ( 'NONE', #42433, 1.500000000000001332 ) ;
#85542 = CARTESIAN_POINT ( 'NONE',  ( 19.84674366389459266, 48.71726448433413026, -2.638427012816827677 ) ) ;
#85543 = ORIENTED_EDGE ( 'NONE', *, *, #80540, .F. ) ;
#85544 = ORIENTED_EDGE ( 'NONE', *, *, #26789, .F. ) ;
#85545 = CARTESIAN_POINT ( 'NONE',  ( -46.68456736488007408, 103.6675473310227034, -5.775421524742654356 ) ) ;
#85546 = AXIS2_PLACEMENT_3D ( 'NONE', #55463, #39485, #76485 ) ;
#85547 = CARTESIAN_POINT ( 'NONE',  ( 2.917880565312950480, 0.9704155015806342766, -12.26659068614894821 ) ) ;
#85548 = CARTESIAN_POINT ( 'NONE',  ( -2.816281873526473856, 64.33196800326376774, 3.434112377981055619 ) ) ;
#85549 = CARTESIAN_POINT ( 'NONE',  ( 24.16423886937410614, 9.512082168247301794, -3.795296366450302550 ) ) ;
#85550 = CARTESIAN_POINT ( 'NONE',  ( 22.26659068614895176, 14.72041550158063572, -7.082119434687042414 ) ) ;
#85551 = FILL_AREA_STYLE_COLOUR ( '', #84193 ) ;
#85552 = CARTESIAN_POINT ( 'NONE',  ( 19.05914839598884569, 9.966938638839758724, 6.499999999999981348 ) ) ;
#85553 = CARTESIAN_POINT ( 'NONE',  ( 20.88017736071110875, 20.77201867748816611, -2.915334737309920765 ) ) ;
#85554 = CARTESIAN_POINT ( 'NONE',  ( 2.603489959281613420, 65.43575266056828355, -6.500000000000031086 ) ) ;
#85555 = VERTEX_POINT ( 'NONE', #32276 ) ;
#85556 = CARTESIAN_POINT ( 'NONE',  ( 14.92337183194729988, 4.342264484334117824, -8.527530157486177487 ) ) ;
#85557 = CARTESIAN_POINT ( 'NONE',  ( 17.20831665107776587, 4.133931151000785675, -7.208316651077762316 ) ) ;
#85558 = CARTESIAN_POINT ( 'NONE',  ( 16.40814093676324603, 32.45696800326375353, -11.09922568453594671 ) ) ;
#85559 = CARTESIAN_POINT ( 'NONE',  ( 14.92337183194729633, 42.67559781766745886, 8.527530157486181039 ) ) ;
#85560 = EDGE_CURVE ( 'NONE', #38399, #59804, #77464, .T. ) ;
#85561 = CARTESIAN_POINT ( 'NONE',  ( -3.750000000000000000, 36.75000000000000000, 3.750000000000000000 ) ) ;
#85562 = CARTESIAN_POINT ( 'NONE',  ( 21.09922568453595559, 12.04030133659708746, -6.408140936763230044 ) ) ;
#85563 = CARTESIAN_POINT ( 'NONE',  ( -6.336512077239976115, 0.2306972965111889207, 13.53095227201380801 ) ) ;
#85564 = CARTESIAN_POINT ( 'NONE',  ( 1.472469842513823179, 20.59226448433411960, -4.923371831947296329 ) ) ;
#85565 = AXIS2_PLACEMENT_3D ( 'NONE', #36118, #28125, #97153 ) ;
#85566 = CARTESIAN_POINT ( 'NONE',  ( 5.076628168052703671, 1.842264484334118047, 8.527530157486179263 ) ) ;
#85567 = ORIENTED_EDGE ( 'NONE', *, *, #51593, .F. ) ;
#85568 = ORIENTED_EDGE ( 'NONE', *, *, #55341, .F. ) ;
#85569 = CARTESIAN_POINT ( 'NONE',  ( 20.88017736071110875, 40.77201867748818387, -2.915334737309920765 ) ) ;
#85570 = CARTESIAN_POINT ( 'NONE',  ( 10.00000000000000000, 30.55374883491397142, -14.16423886937410082 ) ) ;
#85571 = CARTESIAN_POINT ( 'NONE',  ( 0.1532563361054083140, 41.00893115100078745, 1.131784320476157264E-15 ) ) ;
#85572 = CARTESIAN_POINT ( 'NONE',  ( 18.52753015748618282, 3.925597817667451306, -4.923371831947291888 ) ) ;
#85574 = CARTESIAN_POINT ( 'NONE',  ( 14.09394518620612224, 3.883508853191620072E-16, -3.407449058785360752 ) ) ;
#85573 = CARTESIAN_POINT ( 'NONE',  ( -2.816281873526473856, 49.12363466993042493, 9.499525473075851096E-16 ) ) ;
#85575 = CARTESIAN_POINT ( 'NONE',  ( 19.42250999205614193, 30.14701867748817321, 5.440088680355555262 ) ) ;
#85576 = DIRECTION ( 'NONE',  ( 1.000000000000000000, 0.000000000000000000, 0.000000000000000000 ) ) ;
#85577 = CARTESIAN_POINT ( 'NONE',  ( 10.00000000000000178, 25.37363466993041783, 12.81628187352647608 ) ) ;
#85578 = CARTESIAN_POINT ( 'NONE',  ( 7.361572987183170547, 37.05059781766744464, 9.846743663894590881 ) ) ;
#85579 = CARTESIAN_POINT ( 'NONE',  ( 10.88017736071110519, 5.563685344154841950, -2.602085213965210642E-15 ) ) ;
#85580 = CARTESIAN_POINT ( 'NONE',  ( 6.565887622018943937, 43.08196800326374643, -12.81628187352647608 ) ) ;
#85581 = CARTESIAN_POINT ( 'NONE',  ( 4.838527690343616960, 14.63595249122790598, -14.19819177887726980 ) ) ;
#85583 = CARTESIAN_POINT ( 'NONE',  ( 0.4924038765061043432, 0.08682408883346362516, -9.500000000000000000 ) ) ;
#85582 = CARTESIAN_POINT ( 'NONE',  ( 2.035157376598824452, 48.68868534415483396, 7.964842623401179544 ) ) ;
#85584 = VECTOR ( 'NONE', #62174, 1000.000000000000000 ) ;
#85585 = CARTESIAN_POINT ( 'NONE',  ( -7.750000000000003553, -0.02150918539402481983, 4.000000000000000000 ) ) ;
#85586 = CARTESIAN_POINT ( 'NONE',  ( 19.72487221294570858, 69.50000000000000000, 6.500000000000000888 ) ) ;
#85587 = CARTESIAN_POINT ( 'NONE',  ( 20.88017736071110164, 55.35535201082149825, 2.915334737309930979 ) ) ;
#85588 = CARTESIAN_POINT ( 'NONE',  ( 2.035157376598822676, 52.43868534415483396, -7.964842623401177768 ) ) ;
#85589 = DIRECTION ( 'NONE',  ( 0.000000000000000000, 0.000000000000000000, -1.000000000000000000 ) ) ;
#85590 = EDGE_CURVE ( 'NONE', #30551, #62241, #67926, .T. ) ;
#85591 = CARTESIAN_POINT ( 'NONE',  ( -0.1688089201193209155, 79.91181047996344944, 5.000000000000000000 ) ) ;
#85592 = CARTESIAN_POINT ( 'NONE',  ( -0.8801773607111008646, 13.27201867748817321, 2.915334737309923430 ) ) ;
#85593 = EDGE_CURVE ( 'NONE', #73005, #5600, #82309, .T. ) ;
#85594 = CARTESIAN_POINT ( 'NONE',  ( 17.20831665107776587, 49.13393115100078745, -7.208316651077762316 ) ) ;
#85596 = CARTESIAN_POINT ( 'NONE',  ( 18.52753015748618282, 23.92559781766745530, -4.923371831947291888 ) ) ;
#85595 = CARTESIAN_POINT ( 'NONE',  ( 2.035157376598824452, 23.68868534415484461, 7.964842623401179544 ) ) ;
#85597 = CARTESIAN_POINT ( 'NONE',  ( 0.6178305044545818747, 23.49863466993041783, -9.382169495545419124 ) ) ;
#85598 = ORIENTED_EDGE ( 'NONE', *, *, #83788, .F. ) ;
#85599 = CARTESIAN_POINT ( 'NONE',  ( -0.8801773607111008646, 33.27201867748817676, 2.915334737309923430 ) ) ;
#85600 = CARTESIAN_POINT ( 'NONE',  ( 12.63842701281683922, 39.55059781766744464, -9.846743663894590881 ) ) ;
#85602 = CARTESIAN_POINT ( 'NONE',  ( 17.39651004071838969, 39.08210964143329846, -6.500000000000027534 ) ) ;
#85601 = CARTESIAN_POINT ( 'NONE',  ( 10.00000000000000000, 12.87363466993042138, -12.81628187352647608 ) ) ;
#85603 = CARTESIAN_POINT ( 'NONE',  ( 2.035157376598824452, 18.68868534415484106, 7.964842623401179544 ) ) ;
#85604 = CARTESIAN_POINT ( 'NONE',  ( 19.42250999205614193, 45.14701867748817676, 5.440088680355555262 ) ) ;
#85605 = CARTESIAN_POINT ( 'NONE',  ( 2.917880565312950480, 45.97041550158063927, -12.26659068614894821 ) ) ;
#85606 = CARTESIAN_POINT ( 'NONE',  ( 19.84674366389459266, 38.71726448433412315, -2.638427012816827677 ) ) ;
#85607 = CARTESIAN_POINT ( 'NONE',  ( 20.88017736071110519, 60.56368534415484106, 2.639326808657452039E-16 ) ) ;
#85608 = DIRECTION ( 'NONE',  ( 0.000000000000000000, 0.000000000000000000, 1.000000000000000000 ) ) ;
#85609 = CARTESIAN_POINT ( 'NONE',  ( -0.3689425029237881626, 17.42874883491397142, 10.36894250292379027 ) ) ;
#85610 = STYLED_ITEM ( 'NONE', ( #87867 ), #37262 ) ;
#85611 = CARTESIAN_POINT ( 'NONE',  ( 18.95785429995053306, 12.24216108172006834, 6.499999999999848121 ) ) ;
#85612 = AXIS2_PLACEMENT_3D ( 'NONE', #41380, #18855, #24891 ) ;
#85613 = ORIENTED_EDGE ( 'NONE', *, *, #29685, .T. ) ;
#85614 = CARTESIAN_POINT ( 'NONE',  ( 13.79529636645030344, 33.26208216824730357, 14.16423886937410614 ) ) ;
#85615 = CARTESIAN_POINT ( 'NONE',  ( -2.266590686148945544, 41.38708216824729647, -7.082119434687050408 ) ) ;
#85616 = CARTESIAN_POINT ( 'NONE',  ( 19.84674366389459621, 8.508931151000785675, 7.409399052514197653E-17 ) ) ;
#85617 = CARTESIAN_POINT ( 'NONE',  ( 21.09922568453594849, 16.20696800326375353, 6.408140936763242479 ) ) ;
#85618 = CARTESIAN_POINT ( 'NONE',  ( 14.92337183194729988, 64.34226448433412315, -8.527530157486177487 ) ) ;
#85619 = DIRECTION ( 'NONE',  ( 0.000000000000000000, 0.000000000000000000, 1.000000000000000000 ) ) ;
#85621 = CARTESIAN_POINT ( 'NONE',  ( 16.40814093676324603, 37.45696800326376064, -11.09922568453594671 ) ) ;
#85620 = CARTESIAN_POINT ( 'NONE',  ( 15.44008868035555793, 61.39701867748817676, -9.422509992056140149 ) ) ;
#85622 = CARTESIAN_POINT ( 'NONE',  ( 20.36894250292379738, 29.92874883491396432, -10.36894250292379027 ) ) ;
#85623 = CARTESIAN_POINT ( 'NONE',  ( 4.559911319644449179, 23.89701867748817321, 9.422509992056141925 ) ) ;
#85624 = STYLED_ITEM ( 'NONE', ( #327 ), #86830 ) ;
#85625 = DIRECTION ( 'NONE',  ( -0.000000000000000000, 1.000000000000000000, -0.000000000000000000 ) ) ;
#85626 = CARTESIAN_POINT ( 'NONE',  ( 1.472469842513823179, 1.425597817667451528, 4.923371831947296329 ) ) ;
#85627 = CARTESIAN_POINT ( 'NONE',  ( -7.208316651077764980, -9.616068848999210772, -7.208316651077759651 ) ) ;
#85628 = ORIENTED_EDGE ( 'NONE', *, *, #91599, .T. ) ;
#85629 = DIRECTION ( 'NONE',  ( -0.000000000000000000, -1.000000000000000000, -0.000000000000000000 ) ) ;
#85630 = EDGE_LOOP ( 'NONE', ( #52306, #86738, #65335 ) ) ;
#85631 = CARTESIAN_POINT ( 'NONE',  ( -0.3689425029237881626, 7.428748834913967869, 10.36894250292379027 ) ) ;
#85633 = CARTESIAN_POINT ( 'NONE',  ( -0.8801773607111009756, 18.06368534415484106, 1.068504757029289695E-15 ) ) ;
#85632 = CARTESIAN_POINT ( 'NONE',  ( 0.5774900079438607392, 3.480352010821504916, 5.440088680355550821 ) ) ;
#85635 = CARTESIAN_POINT ( 'NONE',  ( 2.791683348922240793, 61.63393115100079456, 7.208316651077764092 ) ) ;
#85634 = CARTESIAN_POINT ( 'NONE',  ( 10.00000000000000178, 42.25893115100078745, 9.846743663894594434 ) ) ;
#85636 = FACE_OUTER_BOUND ( 'NONE', #38009, .T. ) ;
#85637 = CARTESIAN_POINT ( 'NONE',  ( -14.16722289976682170, 14.63606870530283643, -4.928467845925730728 ) ) ;
#85638 = CARTESIAN_POINT ( 'NONE',  ( 21.09922568453594849, 1.206968003263753531, 6.408140936763242479 ) ) ;
#85639 = EDGE_LOOP ( 'NONE', ( #42847, #90652, #6157, #23810 ) ) ;
#85640 = CARTESIAN_POINT ( 'NONE',  ( -0.3689425029237881626, 42.42874883491396787, 10.36894250292379027 ) ) ;
#85641 = EDGE_LOOP ( 'NONE', ( #56950, #40492, #33332, #32482, #25567, #69297 ) ) ;
#85642 = CARTESIAN_POINT ( 'NONE',  ( 6.204703633549690345, 60.76208216824730357, -14.16423886937410259 ) ) ;
#85643 = ORIENTED_EDGE ( 'NONE', *, *, #98297, .T. ) ;
#85644 = CARTESIAN_POINT ( 'NONE',  ( 15.44008868035555793, 26.39701867748817321, -9.422509992056140149 ) ) ;
#85645 = CARTESIAN_POINT ( 'NONE',  ( 2.035157376598822676, 32.43868534415483396, -7.964842623401177768 ) ) ;
#85646 = CARTESIAN_POINT ( 'NONE',  ( 0.1532563361054082862, 46.21726448433411605, 2.638427012816831674 ) ) ;
#85647 = CARTESIAN_POINT ( 'NONE',  ( -0.8801773607111008646, 33.27201867748817676, 2.915334737309923430 ) ) ;
#85648 = CARTESIAN_POINT ( 'NONE',  ( 19.42250999205614193, 65.14701867748817676, 5.440088680355555262 ) ) ;
#85649 = CARTESIAN_POINT ( 'NONE',  ( -0.8801773607110991993, 22.85535201082150181, -2.915334737309923874 ) ) ;
#85650 = VECTOR ( 'NONE', #41080, 1000.000000000000000 ) ;
#85651 = DIRECTION ( 'NONE',  ( 0.000000000000000000, -0.000000000000000000, -1.000000000000000000 ) ) ;
#85652 = B_SPLINE_CURVE_WITH_KNOTS ( 'NONE', 3,
 ( #65310, #78751, #94226, #62253, #77751, #56251 ),
 .UNSPECIFIED., .F., .F.,
 ( 4, 2, 4 ),
 ( 0.000000000000000000, 0.0002565770811490988542, 0.0005131541622981977083 ),
 .UNSPECIFIED. ) ;
#85653 = CARTESIAN_POINT ( 'NONE',  ( 14.92337183194729633, 7.675597817667451750, 8.527530157486181039 ) ) ;
#85654 = CARTESIAN_POINT ( 'NONE',  ( -5.328486666255602522, -28.65465727419762487, 2.750000000000000444 ) ) ;
#85655 = VERTEX_POINT ( 'NONE', #12238 ) ;
#85656 = LINE ( 'NONE', #47148, #14256 ) ;
#85657 = CARTESIAN_POINT ( 'NONE',  ( 2.791683348922240793, 46.63393115100077324, 7.208316651077764092 ) ) ;
#85658 = DIRECTION ( 'NONE',  ( 0.000000000000000000, 1.000000000000000000, 0.000000000000000000 ) ) ;
#85659 = CARTESIAN_POINT ( 'NONE',  ( 6.565887622018943937, 45.16530133659708923, 12.81628187352647430 ) ) ;
#85660 = PRESENTATION_STYLE_ASSIGNMENT (( #70666 ) ) ;
#85661 = LINE ( 'NONE', #55660, #61854 ) ;
#85662 = VERTEX_POINT ( 'NONE', #88729 ) ;
#85663 = CARTESIAN_POINT ( 'NONE',  ( 5.076628168052703671, 66.84226448433412315, 8.527530157486179263 ) ) ;
#85664 = FACE_OUTER_BOUND ( 'NONE', #31860, .T. ) ;
#85665 = CARTESIAN_POINT ( 'NONE',  ( 0.1532563361054100626, 50.80059781766745175, -2.638427012816831230 ) ) ;
#85666 = CARTESIAN_POINT ( 'NONE',  ( 20.36894250292379382, 53.67874883491397497, 10.36894250292379205 ) ) ;
#85667 = CARTESIAN_POINT ( 'NONE',  ( 5.076628168052704559, 60.17559781766745175, -8.527530157486179263 ) ) ;
#85668 = ORIENTED_EDGE ( 'NONE', *, *, #24292, .F. ) ;
#85669 = SURFACE_STYLE_FILL_AREA ( #25670 ) ;
#85670 = CARTESIAN_POINT ( 'NONE',  ( 2.791683348922240793, 16.63393115100078745, 7.208316651077764092 ) ) ;
#85672 = VECTOR ( 'NONE', #12637, 1000.000000000000000 ) ;
#85671 = CARTESIAN_POINT ( 'NONE',  ( 13.43411237798105340, 50.58196800326375353, 12.81628187352647963 ) ) ;
#85673 = CARTESIAN_POINT ( 'NONE',  ( 1.472469842513823179, 66.42559781766745175, 4.923371831947296329 ) ) ;
#85674 = CARTESIAN_POINT ( 'NONE',  ( 19.42250999205614193, 60.14701867748817676, 5.440088680355555262 ) ) ;
#85675 = ADVANCED_FACE ( 'NONE', ( #65726 ), #59978, .T. ) ;
#85676 = CARTESIAN_POINT ( 'NONE',  ( 13.07751017357383994, 4.340377266345630487E-16, -6.263284095430506682 ) ) ;
#85677 = PRESENTATION_LAYER_ASSIGNMENT (  '', '', ( #33000 ) ) ;
#85678 = ORIENTED_EDGE ( 'NONE', *, *, #90385, .F. ) ;
#85679 = CARTESIAN_POINT ( 'NONE',  ( 17.08211943468705840, 65.13708216824730357, -12.26659068614894466 ) ) ;
#85680 = CARTESIAN_POINT ( 'NONE',  ( 8.879999999999991900, 76.07179676972447169, 4.000000000000000000 ) ) ;
#85681 = CARTESIAN_POINT ( 'NONE',  ( 2.035157376598824452, 23.68868534415484461, 7.964842623401179544 ) ) ;
#85683 = CARTESIAN_POINT ( 'NONE',  ( 15.44008868035555260, 54.73035201082150536, 9.422509992056143702 ) ) ;
#85682 = CARTESIAN_POINT ( 'NONE',  ( 10.00000000000000000, 17.87363466993041783, -12.81628187352647608 ) ) ;
#85684 = TOROIDAL_SURFACE ( 'NONE', #2484, 14.49999999999999822, 0.5000000000000000000 ) ;
#85685 = CARTESIAN_POINT ( 'NONE',  ( 19.10478245763057714, 65.10160829253887016, 5.990408912944228170 ) ) ;
#85686 = CARTESIAN_POINT ( 'NONE',  ( -3.897244926436313150, 4.087811286569849197E-16, 13.96644127841328142 ) ) ;
#85687 = CARTESIAN_POINT ( 'NONE',  ( 12.34086200392821908, 15.00000000000000000, 7.125000000000058620 ) ) ;
#85688 = DIRECTION ( 'NONE',  ( 1.257402221000611116E-16, -1.000000000000000000, 0.000000000000000000 ) ) ;
#85689 = CARTESIAN_POINT ( 'NONE',  ( 5.076628168052703671, 51.84226448433412315, 8.527530157486179263 ) ) ;
#85690 = CARTESIAN_POINT ( 'NONE',  ( 7.361572987183169658, -0.03273551566588185635, -9.846743663894592657 ) ) ;
#85691 = CARTESIAN_POINT ( 'NONE',  ( -14.16423886937409726, 27.01208216824730712, 3.795296366450320757 ) ) ;
#85692 = CARTESIAN_POINT ( 'NONE',  ( 10.00000000000000178, 15.37363466993042138, 12.81628187352647608 ) ) ;
#85694 = CARTESIAN_POINT ( 'NONE',  ( 2.153642693323479129, 66.13791097397319163, -6.500000000000079048 ) ) ;
#85693 = CARTESIAN_POINT ( 'NONE',  ( 20.88017736071110875, 15.77201867748817143, -2.915334737309920765 ) ) ;
#85695 = STYLED_ITEM ( 'NONE', ( #98420 ), #32379 ) ;
#85696 = CARTESIAN_POINT ( 'NONE',  ( -3.750000000000000000, 37.25000000000000000, 3.750000000000000000 ) ) ;
#85697 = CARTESIAN_POINT ( 'NONE',  ( -0.3689425029237881626, 42.42874883491396787, 10.36894250292379027 ) ) ;
#85698 = COLOUR_RGB ( '', 0.72549020, 0.75294118, 0.79215686) ;
#85699 = CARTESIAN_POINT ( 'NONE',  ( 24.16423886937410614, 34.51208216824731068, -3.795296366450302550 ) ) ;
#85700 = CARTESIAN_POINT ( 'NONE',  ( 10.00000000000000000, 1.813685344154838175, -10.88017736071110342 ) ) ;
#85701 = AXIS2_PLACEMENT_3D ( 'NONE', #33858, #1940, #70916 ) ;
#85702 = CARTESIAN_POINT ( 'NONE',  ( 0.1532563361054083140, 21.00893115100078745, 1.131784320476157264E-15 ) ) ;
#85703 = CARTESIAN_POINT ( 'NONE',  ( 15.44008868035555260, 19.73035201082150536, 9.422509992056143702 ) ) ;
#85704 = VERTEX_POINT ( 'NONE', #34735 ) ;
#85705 = CARTESIAN_POINT ( 'NONE',  ( 2.791683348922237240, 40.38393115100078035, -7.208316651077763204 ) ) ;
#85707 = EDGE_CURVE ( 'NONE', #65197, #96234, #26433, .T. ) ;
#85706 = VECTOR ( 'NONE', #16078, 1000.000000000000000 ) ;
#85708 = CARTESIAN_POINT ( 'NONE',  ( 12.91533473730992121, 39.52201867748817676, 10.88017736071110164 ) ) ;
#85709 = CARTESIAN_POINT ( 'NONE',  ( 14.92337183194729988, 59.34226448433412315, -8.527530157486177487 ) ) ;
#85711 = CARTESIAN_POINT ( 'NONE',  ( -8.564643372776718167, 14.49999999999999112, 12.31449893000741369 ) ) ;
#85710 = CARTESIAN_POINT ( 'NONE',  ( 2.917880565312948704, 22.63708216824730002, 12.26659068614894643 ) ) ;
#85712 = CARTESIAN_POINT ( 'NONE',  ( 4.862001128006681938, 4.613545383394330660E-16, 13.66056166602463229 ) ) ;
#85713 = CARTESIAN_POINT ( 'NONE',  ( 18.52753015748617571, 8.092264484334117824, 4.923371831947298993 ) ) ;
#85714 = CARTESIAN_POINT ( 'NONE',  ( 19.38216949554541202, 50.99863466993042493, 9.382169495545424454 ) ) ;
#85715 = CARTESIAN_POINT ( 'NONE',  ( 10.00000000000000000, 59.75893115100078745, -9.846743663894594434 ) ) ;
#85716 = ORIENTED_EDGE ( 'NONE', *, *, #13123, .T. ) ;
#85717 = CARTESIAN_POINT ( 'NONE',  ( 8.955816604532303771, -3.107613341149440878, -3.750000000000000000 ) ) ;
#85718 = CARTESIAN_POINT ( 'NONE',  ( 14.62617646268094518, 14.49999999999999112, -3.327906561566873478 ) ) ;
#85719 = CARTESIAN_POINT ( 'NONE',  ( 4.559911319644449179, 3.897018677488171434, 9.422509992056141925 ) ) ;
#85720 = CARTESIAN_POINT ( 'NONE',  ( 12.91533473730992121, 54.52201867748816255, 10.88017736071110164 ) ) ;
#85721 = CARTESIAN_POINT ( 'NONE',  ( -2.266590686148945544, 17.22041550158063572, 7.082119434687048631 ) ) ;
#85722 = CARTESIAN_POINT ( 'NONE',  ( 15.44008868035555260, 54.73035201082150536, 9.422509992056143702 ) ) ;
#85723 = CARTESIAN_POINT ( 'NONE',  ( 5.076628168052704559, 40.17559781766745175, -8.527530157486179263 ) ) ;
#85724 = CARTESIAN_POINT ( 'NONE',  ( 20.88017736071110164, 20.35535201082150891, 2.915334737309930979 ) ) ;
#85725 = SURFACE_STYLE_USAGE ( .BOTH. , #32704 ) ;
#85726 = CARTESIAN_POINT ( 'NONE',  ( 17.20831665107776587, 59.13393115100078745, -7.208316651077762316 ) ) ;
#85727 = VECTOR ( 'NONE', #9232, 1000.000000000000227 ) ;
#85728 = CARTESIAN_POINT ( 'NONE',  ( 17.20831665107776587, 2.883931151000785231, 7.208316651077764980 ) ) ;
#85729 = CARTESIAN_POINT ( 'NONE',  ( -1.099225684535947600, 64.54030133659709634, 6.408140936763237150 ) ) ;
#85730 = VERTEX_POINT ( 'NONE', #4757 ) ;
#85731 = ORIENTED_EDGE ( 'NONE', *, *, #71933, .T. ) ;
#85732 = DIRECTION ( 'NONE',  ( 0.000000000000000000, -0.000000000000000000, -1.000000000000000000 ) ) ;
#85733 = DIRECTION ( 'NONE',  ( 0.000000000000000000, 0.000000000000000000, 1.000000000000000000 ) ) ;
#85734 = PRESENTATION_STYLE_ASSIGNMENT (( #55219 ) ) ;
#85735 = CARTESIAN_POINT ( 'NONE',  ( 10.00000000000000178, 43.05374883491397497, 14.16423886937410082 ) ) ;
#85736 = CARTESIAN_POINT ( 'NONE',  ( 5.076628168052704559, 40.17559781766745175, -8.527530157486179263 ) ) ;
#85737 = CARTESIAN_POINT ( 'NONE',  ( 0.1532563361054082862, 21.21726448433412315, 2.638427012816831674 ) ) ;
#85738 = FILL_AREA_STYLE_COLOUR ( '', #35858 ) ;
#85740 = CARTESIAN_POINT ( 'NONE',  ( 17.20831665107776587, 64.13393115100079456, -7.208316651077762316 ) ) ;
#85739 = CARTESIAN_POINT ( 'NONE',  ( 19.42250999205614193, 25.14701867748817321, 5.440088680355555262 ) ) ;
#85741 = CARTESIAN_POINT ( 'NONE',  ( 24.35999999999999233, 37.99999999999997868, 9.500000000000000000 ) ) ;
#85742 = CARTESIAN_POINT ( 'NONE',  ( -0.3689425029237881626, 37.42874883491396787, 10.36894250292379027 ) ) ;
#85743 = AXIS2_PLACEMENT_3D ( 'NONE', #84669, #84189, #31160 ) ;
#85744 = CARTESIAN_POINT ( 'NONE',  ( 24.16423886937410614, 59.30374883491397497, 8.672049930838204340E-16 ) ) ;
#85745 = PLANE ( 'NONE',  #17866 ) ;
#85746 = CARTESIAN_POINT ( 'NONE',  ( 0.000000000000000000, 0.000000000000000000, 0.000000000000000000 ) ) ;
#85747 = CARTESIAN_POINT ( 'NONE',  ( 15.44008868035555793, 61.39701867748817676, -9.422509992056140149 ) ) ;
#85748 = CARTESIAN_POINT ( 'NONE',  ( 0.1532563361054083140, 21.00893115100078745, 1.131784320476157264E-15 ) ) ;
#85749 = CARTESIAN_POINT ( 'NONE',  ( -3.889970118670757593, -8.287734203605914729, 4.000000000000807354 ) ) ;
#85750 = EDGE_CURVE ( 'NONE', #21472, #31285, #21680, .T. ) ;
#85751 = ORIENTED_EDGE ( 'NONE', *, *, #56782, .T. ) ;
#85752 = CARTESIAN_POINT ( 'NONE',  ( -1.236355250167165964, 0.04962892728883445959, -14.70131747622450114 ) ) ;
#85753 = VERTEX_POINT ( 'NONE', #13725 ) ;
#85754 = CARTESIAN_POINT ( 'NONE',  ( 18.52753015748617571, 13.09226448433411960, 4.923371831947298993 ) ) ;
#85755 = ORIENTED_EDGE ( 'NONE', *, *, #11758, .T. ) ;
#85756 = CARTESIAN_POINT ( 'NONE',  ( 17.08211943468705130, 23.47041550158063572, 12.26659068614894998 ) ) ;
#85757 = CARTESIAN_POINT ( 'NONE',  ( 19.84674366389459266, 18.30059781766745175, 2.638427012816836559 ) ) ;
#85758 = CARTESIAN_POINT ( 'NONE',  ( 0.5774900079438607392, 48.48035201082150536, 5.440088680355550821 ) ) ;
#85759 = ADVANCED_FACE ( 'NONE', ( #73722 ), #44210, .T. ) ;
#85760 = DIRECTION ( 'NONE',  ( -0.000000000000000000, -1.000000000000000000, -0.000000000000000000 ) ) ;
#85761 = ORIENTED_EDGE ( 'NONE', *, *, #92324, .F. ) ;
#85762 = CARTESIAN_POINT ( 'NONE',  ( 7.084665262690076126, 47.02201867748818387, -10.88017736071110164 ) ) ;
#85763 = CIRCLE ( 'NONE', #42633, 0.2500000000000000000 ) ;
#85764 = CARTESIAN_POINT ( 'NONE',  ( 12.81628187352647608, 1.415301336597085013, 3.434112377981052511 ) ) ;
#85765 = EDGE_LOOP ( 'NONE', ( #95253, #24161, #96413, #40539 ) ) ;
#85766 = CARTESIAN_POINT ( 'NONE',  ( 17.96484262340118221, 44.93868534415483396, 7.964842623401181321 ) ) ;
#85767 = CARTESIAN_POINT ( 'NONE',  ( 2.917880565312948704, 7.637082168247301794, 12.26659068614894643 ) ) ;
#85768 = ORIENTED_EDGE ( 'NONE', *, *, #1740, .F. ) ;
#85769 = CARTESIAN_POINT ( 'NONE',  ( 10.00000000000000178, 35.37363466993042493, 12.81628187352647608 ) ) ;
#85770 = STYLED_ITEM ( 'NONE', ( #27963 ), #11640 ) ;
#85771 = CARTESIAN_POINT ( 'NONE',  ( 19.84674366389459266, 3.717264484334118713, -2.638427012816827677 ) ) ;
#85772 = LINE ( 'NONE', #41753, #48278 ) ;
#85773 = CARTESIAN_POINT ( 'NONE',  ( -1.099225684535947600, 43.70696800326375353, -6.408140936763238038 ) ) ;
#85774 = CARTESIAN_POINT ( 'NONE',  ( 19.42250999205614548, 10.98035201082150536, -5.440088680355545492 ) ) ;
#85775 = CARTESIAN_POINT ( 'NONE',  ( 10.00000000000000178, 17.25893115100078745, 9.846743663894594434 ) ) ;
#85776 = CARTESIAN_POINT ( 'NONE',  ( 15.44008868035555260, 49.73035201082150536, 9.422509992056143702 ) ) ;
#85777 = AXIS2_PLACEMENT_3D ( 'NONE', #62527, #78531, #63029 ) ;
#85778 = VERTEX_POINT ( 'NONE', #58724 ) ;
#85779 = DIRECTION ( 'NONE',  ( -1.000000000000000000, 6.938893903907222067E-15, 0.000000000000000000 ) ) ;
#85780 = CARTESIAN_POINT ( 'NONE',  ( 4.559911319644449179, 53.89701867748817676, 9.422509992056141925 ) ) ;
#85781 = CARTESIAN_POINT ( 'NONE',  ( 18.72515096720571393, 41.07228050351032778, -6.499999999999974243 ) ) ;
#85782 = CARTESIAN_POINT ( 'NONE',  ( 19.84674366389459621, 8.508931151000785675, 7.409399052514197653E-17 ) ) ;
#85783 = CARTESIAN_POINT ( 'NONE',  ( 10.00000000000000000, 12.87363466993042138, -12.81628187352647608 ) ) ;
#85784 = CARTESIAN_POINT ( 'NONE',  ( 0.000000000000000000, 15.00000000000000000, 0.000000000000000000 ) ) ;
#85785 = CARTESIAN_POINT ( 'NONE',  ( 1.472469842513823179, 36.42559781766745175, 4.923371831947296329 ) ) ;
#85786 = CARTESIAN_POINT ( 'NONE',  ( -0.3689425029237898834, 11.17874883491396787, -10.36894250292378850 ) ) ;
#85787 = CARTESIAN_POINT ( 'NONE',  ( 0.1532563361054083140, 21.00893115100078745, 1.131784320476157264E-15 ) ) ;
#85788 = CARTESIAN_POINT ( 'NONE',  ( 16.40814093676323893, 20.79030133659708923, 11.09922568453595026 ) ) ;
#85789 = DIRECTION ( 'NONE',  ( -0.6776733583268309546, 0.7353630527936758643, 0.000000000000000000 ) ) ;
#85790 = CARTESIAN_POINT ( 'NONE',  ( 15.44008868035555793, 51.39701867748816966, -9.422509992056140149 ) ) ;
#85791 = CARTESIAN_POINT ( 'NONE',  ( 18.52753015748617571, 58.09226448433411605, 4.923371831947298993 ) ) ;
#85792 = CARTESIAN_POINT ( 'NONE',  ( 4.862001128006681050, 15.00000000000000000, 13.66056166602463229 ) ) ;
#85793 = CARTESIAN_POINT ( 'NONE',  ( 5.076628168052703671, 26.84226448433411960, 8.527530157486179263 ) ) ;
#85794 = CARTESIAN_POINT ( 'NONE',  ( 7.361572987183169658, 19.96726448433411960, -9.846743663894592657 ) ) ;
#85795 = CARTESIAN_POINT ( 'NONE',  ( 20.88017736071110875, 15.77201867748817143, -2.915334737309920765 ) ) ;
#85796 = EDGE_CURVE ( 'NONE', #45156, #85704, #53556, .T. ) ;
#85797 = CARTESIAN_POINT ( 'NONE',  ( 10.00000000000000000, 17.87363466993041783, -12.81628187352647608 ) ) ;
#85798 = CARTESIAN_POINT ( 'NONE',  ( 18.52753015748617571, 18.09226448433411960, 4.923371831947298993 ) ) ;
#85799 = LINE ( 'NONE', #54789, #39102 ) ;
#85801 = ADVANCED_FACE ( 'NONE', ( #74718, #66727, #50228 ), #21736, .T. ) ;
#85800 = CARTESIAN_POINT ( 'NONE',  ( 15.44008868035555260, 19.73035201082150536, 9.422509992056143702 ) ) ;
#85802 = AXIS2_PLACEMENT_3D ( 'NONE', #31837, #92354, #410 ) ;
#85803 = ORIENTED_EDGE ( 'NONE', *, *, #95271, .T. ) ;
#85804 = CARTESIAN_POINT ( 'NONE',  ( 19.42250999205614193, 55.14701867748817676, 5.440088680355555262 ) ) ;
#85806 = CARTESIAN_POINT ( 'NONE',  ( 10.00000000000000000, 11.81368534415483751, -10.88017736071110342 ) ) ;
#85805 = CARTESIAN_POINT ( 'NONE',  ( 12.63842701281683034, 42.46726448433412315, 9.846743663894596210 ) ) ;
#85807 = FILL_AREA_STYLE_COLOUR ( '', #53533 ) ;
#85808 = CARTESIAN_POINT ( 'NONE',  ( 0.5774900079438590739, 47.64701867748817676, -5.440088680355550821 ) ) ;
#85810 = SURFACE_SIDE_STYLE ('',( #69827 ) ) ;
#85809 = CARTESIAN_POINT ( 'NONE',  ( 7.084665262690076126, 7.022018677488170546, -10.88017736071110164 ) ) ;
#85811 = CARTESIAN_POINT ( 'NONE',  ( 19.84674366389459266, 18.30059781766745175, 2.638427012816836559 ) ) ;
#85812 = CARTESIAN_POINT ( 'NONE',  ( 2.791683348922240793, 36.63393115100078035, 7.208316651077764092 ) ) ;
#85813 = CARTESIAN_POINT ( 'NONE',  ( -5.803070148808147088, 3.900978891399319278E-16, -13.28812917035395813 ) ) ;
#85814 = FACE_OUTER_BOUND ( 'NONE', #56410, .T. ) ;
#85815 = CARTESIAN_POINT ( 'NONE',  ( 2.791683348922240793, 66.63393115100079456, 7.208316651077764092 ) ) ;
#85816 = CARTESIAN_POINT ( 'NONE',  ( 8.606322355898619492, 15.00000000000000000, -11.66967075399251996 ) ) ;
#85817 = CARTESIAN_POINT ( 'NONE',  ( 13.79529636645031943, 20.34541550158063572, -14.16423886937409904 ) ) ;
#85818 = CARTESIAN_POINT ( 'NONE',  ( 0.1532563361054100626, 40.80059781766745886, -2.638427012816831230 ) ) ;
#85819 = DIRECTION ( 'NONE',  ( -0.000000000000000000, -1.000000000000000000, 0.000000000000000000 ) ) ;
#85820 = ORIENTED_EDGE ( 'NONE', *, *, #74422, .F. ) ;
#85821 = ADVANCED_FACE ( 'NONE', ( #81232 ), #2495, .T. ) ;
#85822 = CARTESIAN_POINT ( 'NONE',  ( 13.79529636645030344, 58.26208216824728936, 14.16423886937410614 ) ) ;
#85823 = CARTESIAN_POINT ( 'NONE',  ( 14.92337183194729988, 24.34226448433411960, -8.527530157486177487 ) ) ;
#85824 = DIRECTION ( 'NONE',  ( 1.000000000000000000, -0.000000000000000000, -0.000000000000000000 ) ) ;
#85825 = CARTESIAN_POINT ( 'NONE',  ( 20.88017736071110875, 45.77201867748816966, -2.915334737309920765 ) ) ;
#85826 = CARTESIAN_POINT ( 'NONE',  ( -15.81765804549835330, -0.03417435944610275333, -2.383084218347030880 ) ) ;
#85827 = CARTESIAN_POINT ( 'NONE',  ( 2.035157376598822676, 22.43868534415483396, -7.964842623401177768 ) ) ;
#85828 = CARTESIAN_POINT ( 'NONE',  ( -2.816281873526473856, 49.12363466993042493, 9.499525473075851096E-16 ) ) ;
#85829 = CARTESIAN_POINT ( 'NONE',  ( 0.6178305044545818747, 8.498634669930421381, -9.382169495545419124 ) ) ;
#85830 = CARTESIAN_POINT ( 'NONE',  ( 0.1532563361054100626, 15.80059781766745353, -2.638427012816831230 ) ) ;
#85832 = ORIENTED_EDGE ( 'NONE', *, *, #68028, .T. ) ;
#85831 = EDGE_CURVE ( 'NONE', #98827, #95512, #69226, .T. ) ;
#85833 = FACE_OUTER_BOUND ( 'NONE', #696, .T. ) ;
#85834 = LINE ( 'NONE', #63793, #30052 ) ;
#85835 = CARTESIAN_POINT ( 'NONE',  ( 6.204703633549690345, 55.76208216824730357, -14.16423886937410259 ) ) ;
#85836 = CARTESIAN_POINT ( 'NONE',  ( 24.16423886937409904, 34.09541550158064638, 3.795296366450317205 ) ) ;
#85837 = CARTESIAN_POINT ( 'NONE',  ( 4.559911319644449179, 17.23035201082150536, -9.422509992056141925 ) ) ;
#85838 = AXIS2_PLACEMENT_3D ( 'NONE', #78619, #32612, #10128 ) ;
#85839 = CARTESIAN_POINT ( 'NONE',  ( 0.5774900079438590739, 47.64701867748817676, -5.440088680355550821 ) ) ;
#85840 = FACE_OUTER_BOUND ( 'NONE', #13934, .T. ) ;
#85841 = CARTESIAN_POINT ( 'NONE',  ( 19.50000000000000355, 70.00000000000000000, -5.000000000000000000 ) ) ;
#85842 = CARTESIAN_POINT ( 'NONE',  ( 1.472469842513823179, 0.5922644843341181575, -4.923371831947296329 ) ) ;
#85843 = FILL_AREA_STYLE ('',( #25832 ) ) ;
#85844 = CARTESIAN_POINT ( 'NONE',  ( 14.92337183194729988, 14.34226448433411782, -8.527530157486177487 ) ) ;
#85845 = PRESENTATION_STYLE_ASSIGNMENT (( #40836 ) ) ;
#85846 = CARTESIAN_POINT ( 'NONE',  ( 19.84674366389459266, 28.71726448433411960, -2.638427012816827677 ) ) ;
#85847 = CARTESIAN_POINT ( 'NONE',  ( 7.361572987183170547, 52.05059781766745175, 9.846743663894590881 ) ) ;
#85848 = CIRCLE ( 'NONE', #65041, 14.49999999999999822 ) ;
#85849 = CARTESIAN_POINT ( 'NONE',  ( 17.96484262340118221, 11.18868534415483929, -7.964842623401177768 ) ) ;
#85850 = VECTOR ( 'NONE', #73841, 1000.000000000000000 ) ;
#85851 = AXIS2_PLACEMENT_3D ( 'NONE', #48825, #24508, #31481 ) ;
#85852 = CARTESIAN_POINT ( 'NONE',  ( 19.38216949554541557, 32.24863466993041783, -9.382169495545420901 ) ) ;
#85853 = CARTESIAN_POINT ( 'NONE',  ( 4.559911319644449179, 48.89701867748817676, 9.422509992056141925 ) ) ;
#85855 = CARTESIAN_POINT ( 'NONE',  ( 14.92337183194729988, 9.342264484334119601, -8.527530157486177487 ) ) ;
#85854 = CARTESIAN_POINT ( 'NONE',  ( -0.3689425029237898834, 41.17874883491397497, -10.36894250292378850 ) ) ;
#85856 = DIRECTION ( 'NONE',  ( -1.000000000000000000, -1.927470528863119542E-16, 0.000000000000000000 ) ) ;
#85857 = CARTESIAN_POINT ( 'NONE',  ( 19.84674366389459266, 53.30059781766744464, 2.638427012816836559 ) ) ;
#85858 = CARTESIAN_POINT ( 'NONE',  ( 12.63842701281683922, 34.55059781766745886, -9.846743663894590881 ) ) ;
#85859 = CARTESIAN_POINT ( 'NONE',  ( 13.79529636645031943, 15.34541550158063750, -14.16423886937409904 ) ) ;
#85860 = CARTESIAN_POINT ( 'NONE',  ( 12.63842701281683034, 27.46726448433411250, 9.846743663894596210 ) ) ;
#85861 = CARTESIAN_POINT ( 'NONE',  ( -0.8801773607111009756, 48.06368534415484817, 1.068504757029289695E-15 ) ) ;
#85862 = CARTESIAN_POINT ( 'NONE',  ( 10.00000000000000000, 16.81368534415483751, -10.88017736071110342 ) ) ;
#85863 = CARTESIAN_POINT ( 'NONE',  ( 20.88017736071110519, 45.56368534415484106, 2.639326808657452039E-16 ) ) ;
#85864 = CARTESIAN_POINT ( 'NONE',  ( 20.88017736071110875, 25.77201867748816966, -2.915334737309920765 ) ) ;
#85865 = VERTEX_POINT ( 'NONE', #52218 ) ;
#85866 = CARTESIAN_POINT ( 'NONE',  ( 21.09922568453594849, 31.20696800326375353, 6.408140936763242479 ) ) ;
#85867 = CARTESIAN_POINT ( 'NONE',  ( 0.5774900079438590739, 37.64701867748817676, -5.440088680355550821 ) ) ;
#85868 = ORIENTED_EDGE ( 'NONE', *, *, #58506, .F. ) ;
#85869 = CARTESIAN_POINT ( 'NONE',  ( 10.00000000000000178, 65.37363466993042493, 12.81628187352647608 ) ) ;
#85870 = EDGE_CURVE ( 'NONE', #50110, #47708, #82712, .T. ) ;
#85871 = CARTESIAN_POINT ( 'NONE',  ( 17.96484262340118221, 59.93868534415484106, 7.964842623401181321 ) ) ;
#85872 = ORIENTED_EDGE ( 'NONE', *, *, #58377, .F. ) ;
#85873 = CARTESIAN_POINT ( 'NONE',  ( 4.559911319644449179, 52.23035201082151247, -9.422509992056141925 ) ) ;
#85874 = SURFACE_STYLE_FILL_AREA ( #78856 ) ;
#85875 = CARTESIAN_POINT ( 'NONE',  ( 19.84674366389459621, 8.508931151000785675, 7.409399052514197653E-17 ) ) ;
#85876 = DIRECTION ( 'NONE',  ( 0.000000000000000000, 0.000000000000000000, 1.000000000000000000 ) ) ;
#85877 = CARTESIAN_POINT ( 'NONE',  ( -2.266590686148945544, 62.22041550158063927, 7.082119434687048631 ) ) ;
#85878 = CARTESIAN_POINT ( 'NONE',  ( 17.20831665107776587, 7.883931151000784787, 7.208316651077764980 ) ) ;
#85879 = CARTESIAN_POINT ( 'NONE',  ( 17.08211943468705130, 8.470415501580635720, 12.26659068614894998 ) ) ;
#85880 = CARTESIAN_POINT ( 'NONE',  ( 14.92337183194729988, 9.342264484334119601, -8.527530157486177487 ) ) ;
#85881 = CARTESIAN_POINT ( 'NONE',  ( 17.96484262340118221, 16.18868534415483396, -7.964842623401177768 ) ) ;
#85882 = CARTESIAN_POINT ( 'NONE',  ( 19.84674366389459621, 43.50893115100078745, 7.409399052514197653E-17 ) ) ;
#85883 = ORIENTED_EDGE ( 'NONE', *, *, #62342, .T. ) ;
#85884 = CARTESIAN_POINT ( 'NONE',  ( 14.92337183194729633, 47.67559781766745175, 8.527530157486181039 ) ) ;
#85885 = LINE ( 'NONE', #47867, #12614 ) ;
#85886 = CARTESIAN_POINT ( 'NONE',  ( 4.559911319644449179, 43.89701867748816966, 9.422509992056141925 ) ) ;
#85887 = CARTESIAN_POINT ( 'NONE',  ( 0.1532563361054083140, 56.00893115100078745, 1.131784320476157264E-15 ) ) ;
#85889 = CARTESIAN_POINT ( 'NONE',  ( 6.336512077239798479, 14.76930270348881002, 13.53095227201389328 ) ) ;
#85888 =( LENGTH_UNIT ( ) NAMED_UNIT ( * ) SI_UNIT ( .MILLI., .METRE. ) );
#85890 = CARTESIAN_POINT ( 'NONE',  ( 10.00000000000000000, 41.81368534415484106, -10.88017736071110342 ) ) ;
#85891 = CARTESIAN_POINT ( 'NONE',  ( 0.5774900079438590739, 2.647018677488171434, -5.440088680355550821 ) ) ;
#85892 = CIRCLE ( 'NONE', #58689, 2.899999999999998579 ) ;
#85893 = CARTESIAN_POINT ( 'NONE',  ( 13.43411237798105340, 20.58196800326374643, 12.81628187352647963 ) ) ;
#85894 = CARTESIAN_POINT ( 'NONE',  ( 0.000000000000000000, 15.00000000000000000, 0.000000000000000000 ) ) ;
#85895 = EDGE_LOOP ( 'NONE', ( #6413, #29425, #69278, #20668 ) ) ;
#85896 = CARTESIAN_POINT ( 'NONE',  ( 16.40814093676324603, 32.45696800326375353, -11.09922568453594671 ) ) ;
#85897 = CARTESIAN_POINT ( 'NONE',  ( -0.8801773607111008646, 18.27201867748817321, 2.915334737309923430 ) ) ;
#85898 = EDGE_CURVE ( 'NONE', #25477, #86614, #36208, .T. ) ;
#85899 = ORIENTED_EDGE ( 'NONE', *, *, #67189, .T. ) ;
#85900 = DIRECTION ( 'NONE',  ( 0.000000000000000000, 1.000000000000000000, 0.000000000000000000 ) ) ;
#85901 = TOROIDAL_SURFACE ( 'NONE', #4480, 2.250000000000001332, 0.2500000000000000000 ) ;
#85902 = CARTESIAN_POINT ( 'NONE',  ( 1.472469842513823179, 1.425597817667451528, 4.923371831947296329 ) ) ;
#85903 = CARTESIAN_POINT ( 'NONE',  ( 10.00000000000000178, 47.25893115100078745, 9.846743663894594434 ) ) ;
#85905 = CARTESIAN_POINT ( 'NONE',  ( 19.84674366389459621, 43.50893115100078745, 7.409399052514197653E-17 ) ) ;
#85904 = CARTESIAN_POINT ( 'NONE',  ( 0.1532563361054083140, 6.008931151000784787, 1.131784320476157264E-15 ) ) ;
#85906 = LINE ( 'NONE', #17420, #95201 ) ;
#85907 = CARTESIAN_POINT ( 'NONE',  ( -1.847237859018842299, 0.04962896072145024651, 14.63711110085118783 ) ) ;
#85908 = CARTESIAN_POINT ( 'NONE',  ( 19.84674366389459266, 23.30059781766745530, 2.638427012816836559 ) ) ;
#85909 = CYLINDRICAL_SURFACE ( 'NONE', #50648, 0.2500000000000002220 ) ;
#85910 = FACE_OUTER_BOUND ( 'NONE', #78, .T. ) ;
#85913 = CARTESIAN_POINT ( 'NONE',  ( 2.791683348922240793, 1.633931151000784565, 7.208316651077764092 ) ) ;
#85912 = VECTOR ( 'NONE', #15138, 1000.000000000000000 ) ;
#85911 = CARTESIAN_POINT ( 'NONE',  ( 17.20831665107776587, 22.88393115100078745, 7.208316651077764980 ) ) ;
#85914 =( NAMED_UNIT ( * ) SI_UNIT ( $, .STERADIAN. ) SOLID_ANGLE_UNIT ( ) );
#85915 = ADVANCED_FACE ( 'NONE', ( #91700 ), #5566, .T. ) ;
#85917 = VERTEX_POINT ( 'NONE', #81022 ) ;
#85916 = CARTESIAN_POINT ( 'NONE',  ( 10.00000000000000178, 52.25893115100078745, 9.846743663894594434 ) ) ;
#85918 = STYLED_ITEM ( 'NONE', ( #37668 ), #69668 ) ;
#85919 = CARTESIAN_POINT ( 'NONE',  ( 13.59943737456458024, 14.95077488074853456, -5.718514076972845750 ) ) ;
#85920 = CARTESIAN_POINT ( 'NONE',  ( 0.6178305044545838731, 29.74863466993042138, 9.382169495545420901 ) ) ;
#85921 = EDGE_CURVE ( 'NONE', #25175, #91846, #42534, .T. ) ;
#85922 = LINE ( 'NONE', #33380, #56835 ) ;
#85924 = EDGE_CURVE ( 'NONE', #50559, #27193, #7247, .T. ) ;
#85923 = CARTESIAN_POINT ( 'NONE',  ( -4.164238869374099039, 46.80374883491397497, 8.674139862899312516E-16 ) ) ;
#85925 = CARTESIAN_POINT ( 'NONE',  ( 5.076628168052703671, 16.84226448433411960, 8.527530157486179263 ) ) ;
#85926 = CARTESIAN_POINT ( 'NONE',  ( 7.361572987183169658, 4.967264484334119601, -9.846743663894592657 ) ) ;
#85927 = CARTESIAN_POINT ( 'NONE',  ( 0.000000000000000000, 0.000000000000000000, 0.000000000000000000 ) ) ;
#85928 = CARTESIAN_POINT ( 'NONE',  ( 10.00000000000000178, 38.05374883491396787, 14.16423886937410082 ) ) ;
#85929 = CARTESIAN_POINT ( 'NONE',  ( 7.361572987183170547, 62.05059781766745886, 9.846743663894590881 ) ) ;
#85930 = CARTESIAN_POINT ( 'NONE',  ( 20.88017736071110164, 10.35535201082150714, 2.915334737309930979 ) ) ;
#85931 = CARTESIAN_POINT ( 'NONE',  ( 24.16423886937410614, 29.30374883491396787, 8.672049930838204340E-16 ) ) ;
#85932 = CARTESIAN_POINT ( 'NONE',  ( 17.08211943468705840, 40.13708216824731068, -12.26659068614894466 ) ) ;
#85933 = DIRECTION ( 'NONE',  ( -0.000000000000000000, -0.000000000000000000, -1.000000000000000000 ) ) ;
#85935 = CARTESIAN_POINT ( 'NONE',  ( 19.84674366389459621, 53.50893115100078745, 7.409399052514197653E-17 ) ) ;
#85934 = DIRECTION ( 'NONE',  ( -0.000000000000000000, -0.000000000000000000, 1.000000000000000000 ) ) ;
#85936 = ORIENTED_EDGE ( 'NONE', *, *, #57943, .T. ) ;
#85937 = CARTESIAN_POINT ( 'NONE',  ( 17.96484262340118221, 36.18868534415484106, -7.964842623401177768 ) ) ;
#85938 = CARTESIAN_POINT ( 'NONE',  ( 3.843542995449656718, 0.2301500725087332888, -14.43777707752878925 ) ) ;
#85939 = DIRECTION ( 'NONE',  ( 0.000000000000000000, 0.000000000000000000, -1.000000000000000000 ) ) ;
#85940 = CARTESIAN_POINT ( 'NONE',  ( 18.52753015748618282, 38.92559781766745175, -4.923371831947291888 ) ) ;
#85941 = CARTESIAN_POINT ( 'NONE',  ( 10.00000000000000000, 62.87363466993042493, -12.81628187352647608 ) ) ;
#85942 = CARTESIAN_POINT ( 'NONE',  ( -7.082119434687058401, -4.029584498419364280, -12.26659068614894110 ) ) ;
#85943 = CARTESIAN_POINT ( 'NONE',  ( 5.076628168052704559, 40.17559781766745175, -8.527530157486179263 ) ) ;
#85944 = DIRECTION ( 'NONE',  ( 1.000000000000000000, -0.000000000000000000, -0.000000000000000000 ) ) ;
#85946 = EDGE_CURVE ( 'NONE', #25822, #78552, #51328, .T. ) ;
#85945 = ORIENTED_EDGE ( 'NONE', *, *, #5339, .F. ) ;
#85947 = CARTESIAN_POINT ( 'NONE',  ( 17.08211943468705840, 20.13708216824730357, -12.26659068614894466 ) ) ;
#85948 = CARTESIAN_POINT ( 'NONE',  ( 9.879999999999990123, 20.99999999999999645, 1.249999999999987121 ) ) ;
#85950 = CARTESIAN_POINT ( 'NONE',  ( 19.50000000000000711, 105.0000000000000000, 4.500000000000000888 ) ) ;
#85949 = CARTESIAN_POINT ( 'NONE',  ( 0.1089645850228990742, 68.16234555792571825, 6.479102184480824533 ) ) ;
#85951 = CARTESIAN_POINT ( 'NONE',  ( 15.44008868035555260, 4.730352010821505360, 9.422509992056143702 ) ) ;
#85952 = CARTESIAN_POINT ( 'NONE',  ( 6.565887622018943937, 30.16530133659708568, 12.81628187352647430 ) ) ;
#85953 = CARTESIAN_POINT ( 'NONE',  ( 2.791683348922237240, 0.3839311510007847872, -7.208316651077763204 ) ) ;
#85954 = EDGE_CURVE ( 'NONE', #36088, #36584, #41074, .T. ) ;
#85955 = DIRECTION ( 'NONE',  ( 1.000000000000000000, 2.107602052970794797E-16, -0.000000000000000000 ) ) ;
#85956 = CARTESIAN_POINT ( 'NONE',  ( -1.926860441876562025, 9.479976035794173583, -3.195792623639529761 ) ) ;
#85957 = CYLINDRICAL_SURFACE ( 'NONE', #35919, 0.5000000000000004441 ) ;
#85958 = CARTESIAN_POINT ( 'NONE',  ( 6.204703633549690345, 60.76208216824730357, -14.16423886937410259 ) ) ;
#85959 = PRESENTATION_LAYER_ASSIGNMENT (  '', '', ( #73151 ) ) ;
#85960 = CARTESIAN_POINT ( 'NONE',  ( 0.2751277870542871429, 42.28217586085238366, -6.499999999999984901 ) ) ;
#85961 = CARTESIAN_POINT ( 'NONE',  ( 17.96484262340118221, 24.93868534415484461, 7.964842623401181321 ) ) ;
#85962 = CARTESIAN_POINT ( 'NONE',  ( -0.8801773607110991993, 32.85535201082151247, -2.915334737309923874 ) ) ;
#85963 = CARTESIAN_POINT ( 'NONE',  ( 12.63842701281683922, 64.55059781766745175, -9.846743663894590881 ) ) ;
#85964 = CARTESIAN_POINT ( 'NONE',  ( 12.63842701281683034, 57.46726448433411605, 9.846743663894596210 ) ) ;
#85965 = CARTESIAN_POINT ( 'NONE',  ( 16.40814093676323893, 60.79030133659709634, 11.09922568453595026 ) ) ;
#85966 = FILL_AREA_STYLE_COLOUR ( '', #42436 ) ;
#85967 = ORIENTED_EDGE ( 'NONE', *, *, #58957, .F. ) ;
#85968 = CARTESIAN_POINT ( 'NONE',  ( 12.91533473730993009, 36.60535201082151247, -10.88017736071109987 ) ) ;
#85969 = CARTESIAN_POINT ( 'NONE',  ( 3.591859063236763294, 28.29030133659708568, -11.09922568453595026 ) ) ;
#85970 = DIRECTION ( 'NONE',  ( 1.000000000000000000, 0.000000000000000000, 0.000000000000000000 ) ) ;
#85971 = CIRCLE ( 'NONE', #6094, 15.00000000000000000 ) ;
#85972 = CARTESIAN_POINT ( 'NONE',  ( 5.076628168052703671, 61.84226448433412315, 8.527530157486179263 ) ) ;
#85973 = CARTESIAN_POINT ( 'NONE',  ( 20.88017736071110875, 45.77201867748816966, -2.915334737309920765 ) ) ;
#85974 = CARTESIAN_POINT ( 'NONE',  ( 5.076628168052703671, 11.84226448433411960, 8.527530157486179263 ) ) ;
#85975 = CARTESIAN_POINT ( 'NONE',  ( 0.6178305044545838731, 39.74863466993041072, 9.382169495545420901 ) ) ;
#85976 = CARTESIAN_POINT ( 'NONE',  ( 4.559911319644449179, 67.23035201082150536, -9.422509992056141925 ) ) ;
#85977 = CARTESIAN_POINT ( 'NONE',  ( 10.93781366033340596, 0.3640475087720985159, 10.26470809774073700 ) ) ;
#85978 = CARTESIAN_POINT ( 'NONE',  ( 22.81628187352647785, 61.41530133659709634, 3.434112377981063169 ) ) ;
#85979 = ORIENTED_EDGE ( 'NONE', *, *, #62557, .T. ) ;
#85980 = FACE_OUTER_BOUND ( 'NONE', #90907, .T. ) ;
#85981 = DIRECTION ( 'NONE',  ( -1.257402221000611116E-16, 1.000000000000000000, 0.000000000000000000 ) ) ;
#85982 = CARTESIAN_POINT ( 'NONE',  ( 2.035157376598824452, 3.688685344154837953, 7.964842623401179544 ) ) ;
#85984 = CARTESIAN_POINT ( 'NONE',  ( 13.79529636645030344, 18.26208216824730002, 14.16423886937410614 ) ) ;
#85983 = CARTESIAN_POINT ( 'NONE',  ( 22.81628187352647785, 46.62363466993041783, 6.195893100308588602E-16 ) ) ;
#85985 = CARTESIAN_POINT ( 'NONE',  ( 19.84674366389459621, 18.50893115100078745, 7.409399052514197653E-17 ) ) ;
#85986 = CARTESIAN_POINT ( 'NONE',  ( 4.559911319644449179, 7.230352010821504471, -9.422509992056141925 ) ) ;
#85987 = CARTESIAN_POINT ( 'NONE',  ( 1.472469842513823179, 15.59226448433411960, -4.923371831947296329 ) ) ;
#85988 = CARTESIAN_POINT ( 'NONE',  ( 20.36894250292379382, 58.67874883491396076, 10.36894250292379205 ) ) ;
#85989 = VERTEX_POINT ( 'NONE', #19538 ) ;
#85990 = CARTESIAN_POINT ( 'NONE',  ( 10.00000000000000000, 1.813685344154837731, -10.88017736071110342 ) ) ;
#85991 = TOROIDAL_SURFACE ( 'NONE', #61989, 2.899999999999999467, 0.1000000000000000056 ) ;
#85992 = CARTESIAN_POINT ( 'NONE',  ( 7.084665262690076126, 22.02201867748817321, -10.88017736071110164 ) ) ;
#85993 = DIRECTION ( 'NONE',  ( 0.000000000000000000, 0.000000000000000000, 1.000000000000000000 ) ) ;
#85994 = VECTOR ( 'NONE', #71006, 1000.000000000000000 ) ;
#85995 = ORIENTED_EDGE ( 'NONE', *, *, #61925, .T. ) ;
#85996 = ORIENTED_EDGE ( 'NONE', *, *, #45977, .F. ) ;
#85997 = CARTESIAN_POINT ( 'NONE',  ( 2.035157376598822676, 17.43868534415483751, -7.964842623401177768 ) ) ;
#85998 = CARTESIAN_POINT ( 'NONE',  ( 2.035157376598824452, 8.688685344154839285, 7.964842623401179544 ) ) ;
#85999 = CARTESIAN_POINT ( 'NONE',  ( 1.472469842513823179, 60.59226448433412315, -4.923371831947296329 ) ) ;
#86000 = CARTESIAN_POINT ( 'NONE',  ( -2.816281873526473856, 54.12363466993041783, 9.499525473075851096E-16 ) ) ;
#86001 = CARTESIAN_POINT ( 'NONE',  ( -13.55157833323639238, 0.2306972965111898921, 6.292279346205288171 ) ) ;
#86002 = CARTESIAN_POINT ( 'NONE',  ( 22.26659068614895176, 19.72041550158063572, -7.082119434687042414 ) ) ;
#86003 = CARTESIAN_POINT ( 'NONE',  ( 15.44008868035555260, 24.73035201082150891, 9.422509992056143702 ) ) ;
#86004 = CARTESIAN_POINT ( 'NONE',  ( 20.88017736071110519, 15.56368534415483751, 2.639326808657452039E-16 ) ) ;
#86005 = CARTESIAN_POINT ( 'NONE',  ( 14.92337183194729988, 49.34226448433411605, -8.527530157486177487 ) ) ;
#86006 = CARTESIAN_POINT ( 'NONE',  ( 7.361572987183169658, 39.96726448433411605, -9.846743663894592657 ) ) ;
#86007 = DIRECTION ( 'NONE',  ( 1.000000000000000000, 0.000000000000000000, 0.000000000000000000 ) ) ;
#86008 = CARTESIAN_POINT ( 'NONE',  ( 2.791683348922237240, 10.38393115100078390, -7.208316651077763204 ) ) ;
#86009 = CARTESIAN_POINT ( 'NONE',  ( -8.527530157486182816, 25.59226448433413026, -4.923371831947288335 ) ) ;
#86010 = VERTEX_POINT ( 'NONE', #66013 ) ;
#86011 = FACE_OUTER_BOUND ( 'NONE', #812, .T. ) ;
#86012 = CARTESIAN_POINT ( 'NONE',  ( 0.1532563361054082862, 16.21726448433411960, 2.638427012816831674 ) ) ;
#86013 = CARTESIAN_POINT ( 'NONE',  ( 16.40814093676324603, 2.456968003263753531, -11.09922568453594671 ) ) ;
#86014 = CARTESIAN_POINT ( 'NONE',  ( -0.8801773607111009756, 53.06368534415484106, 1.068504757029289695E-15 ) ) ;
#86016 = CARTESIAN_POINT ( 'NONE',  ( -2.816281873526471635, 43.91530133659708923, -3.434112377981056508 ) ) ;
#86015 = CARTESIAN_POINT ( 'NONE',  ( 10.00000000000000000, 6.813685344154838397, -10.88017736071110342 ) ) ;
#86017 = CARTESIAN_POINT ( 'NONE',  ( 10.00000000000000178, 18.05374883491396787, 14.16423886937410082 ) ) ;
#86018 = CARTESIAN_POINT ( 'NONE',  ( 0.6178305044545838731, 54.74863466993042493, 9.382169495545420901 ) ) ;
#86019 = ORIENTED_EDGE ( 'NONE', *, *, #59281, .F. ) ;
#86020 = CARTESIAN_POINT ( 'NONE',  ( 17.20831665107776587, 59.13393115100078745, -7.208316651077762316 ) ) ;
#86021 = CARTESIAN_POINT ( 'NONE',  ( -0.8801773607110991993, 22.85535201082150181, -2.915334737309923874 ) ) ;
#86022 = EDGE_LOOP ( 'NONE', ( #5864, #69820, #82351, #63727 ) ) ;
#86023 = CARTESIAN_POINT ( 'NONE',  ( 10.00000000000000178, 7.258931151000785675, 9.846743663894594434 ) ) ;
#86024 = CARTESIAN_POINT ( 'NONE',  ( 17.96484262340118221, 66.18868534415483396, -7.964842623401177768 ) ) ;
#86025 = AXIS2_PLACEMENT_3D ( 'NONE', #19177, #43153, #49657 ) ;
#86026 = CARTESIAN_POINT ( 'NONE',  ( 18.52753015748618282, 13.92559781766745175, -4.923371831947291888 ) ) ;
#86027 = ADVANCED_FACE ( 'NONE', ( #36014 ), #43511, .F. ) ;
#86028 = CARTESIAN_POINT ( 'NONE',  ( 15.44008868035555793, 66.39701867748817676, -9.422509992056140149 ) ) ;
#86029 = CARTESIAN_POINT ( 'NONE',  ( -57.13414634146340632, 45.70731707317067816, -8.000000000000000000 ) ) ;
#86031 = SURFACE_STYLE_FILL_AREA ( #18025 ) ;
#86030 = CARTESIAN_POINT ( 'NONE',  ( 19.42250999205614548, 60.98035201082151247, -5.440088680355545492 ) ) ;
#86032 = CARTESIAN_POINT ( 'NONE',  ( 20.88017736071110164, 65.35535201082150536, 2.915334737309930979 ) ) ;
#86034 = VERTEX_POINT ( 'NONE', #37515 ) ;
#86033 = CARTESIAN_POINT ( 'NONE',  ( 0.1532563361054083140, 6.008931151000784787, 1.131784320476157264E-15 ) ) ;
#86035 = EDGE_CURVE ( 'NONE', #24202, #74944, #22652, .T. ) ;
#86036 = CARTESIAN_POINT ( 'NONE',  ( -9.065164099344613646, 0.5000000000000004441, 11.95084933600761445 ) ) ;
#86037 = CARTESIAN_POINT ( 'NONE',  ( 18.52753015748618282, 53.92559781766745175, -4.923371831947291888 ) ) ;
#86038 = ORIENTED_EDGE ( 'NONE', *, *, #3671, .T. ) ;
#86039 = ORIENTED_EDGE ( 'NONE', *, *, #82686, .F. ) ;
#86040 = LINE ( 'NONE', #56521, #60210 ) ;
#86042 = EDGE_CURVE ( 'NONE', #44839, #23568, #79112, .T. ) ;
#86041 = CARTESIAN_POINT ( 'NONE',  ( 22.26659068614894466, 3.887082168247300906, 7.082119434687054849 ) ) ;
#86043 = CARTESIAN_POINT ( 'NONE',  ( 13.43411237798105340, 60.58196800326376064, 12.81628187352647963 ) ) ;
#86044 = CARTESIAN_POINT ( 'NONE',  ( 6.204703633549690345, 5.762082168247301794, -14.16423886937410259 ) ) ;
#86045 = CARTESIAN_POINT ( 'NONE',  ( 13.79529636645031943, 15.34541550158063750, -14.16423886937409904 ) ) ;
#86046 = AXIS2_PLACEMENT_3D ( 'NONE', #58901, #56925, #72912 ) ;
#86047 = SURFACE_STYLE_FILL_AREA ( #16567 ) ;
#86048 = CARTESIAN_POINT ( 'NONE',  ( 22.26659068614895176, 4.720415501580633943, -7.082119434687042414 ) ) ;
#86049 = CARTESIAN_POINT ( 'NONE',  ( 12.91533473730992121, 24.52201867748816966, 10.88017736071110164 ) ) ;
#86050 = DIRECTION ( 'NONE',  ( 0.000000000000000000, 0.000000000000000000, -1.000000000000000000 ) ) ;
#86051 = VERTEX_POINT ( 'NONE', #13519 ) ;
#86052 = CARTESIAN_POINT ( 'NONE',  ( 5.076628168052704559, 5.175597817667451750, -8.527530157486179263 ) ) ;
#86053 = CARTESIAN_POINT ( 'NONE',  ( 7.361572987183170547, 22.05059781766745530, 9.846743663894590881 ) ) ;
#86054 = CARTESIAN_POINT ( 'NONE',  ( 22.81628187352647785, 36.41530133659707502, 3.434112377981063169 ) ) ;
#86055 = CARTESIAN_POINT ( 'NONE',  ( 5.076628168052704559, 35.17559781766745175, -8.527530157486179263 ) ) ;
#86056 = AXIS2_PLACEMENT_3D ( 'NONE', #84167, #22675, #15179 ) ;
#86057 = CARTESIAN_POINT ( 'NONE',  ( 24.35999999999999233, 44.99999999999997158, 10.00000000000000000 ) ) ;
#86058 = CARTESIAN_POINT ( 'NONE',  ( 10.00000000000000178, 20.37363466993042138, 12.81628187352647608 ) ) ;
#86059 = PRESENTATION_LAYER_ASSIGNMENT (  '', '', ( #4624 ) ) ;
#86060 = CARTESIAN_POINT ( 'NONE',  ( 2.791683348922240793, 31.63393115100078745, 7.208316651077764092 ) ) ;
#86061 = CARTESIAN_POINT ( 'NONE',  ( 6.204703633549690345, 17.84541550158063217, 14.16423886937410082 ) ) ;
#86062 = ORIENTED_EDGE ( 'NONE', *, *, #94080, .F. ) ;
#86063 = EDGE_LOOP ( 'NONE', ( #12176, #1224, #94716, #83941 ) ) ;
#86064 = CARTESIAN_POINT ( 'NONE',  ( 12.91533473730992121, 34.52201867748817676, 10.88017736071110164 ) ) ;
#86065 = CARTESIAN_POINT ( 'NONE',  ( 24.16423886937410614, 34.51208216824731068, -3.795296366450302550 ) ) ;
#86066 = CARTESIAN_POINT ( 'NONE',  ( 5.076628168052703671, 41.84226448433411605, 8.527530157486179263 ) ) ;
#86067 = CARTESIAN_POINT ( 'NONE',  ( 7.361572987183169658, 14.96726448433411960, -9.846743663894592657 ) ) ;
#86069 = CARTESIAN_POINT ( 'NONE',  ( 19.72487221294570858, 0.000000000000000000, -6.500000000000000888 ) ) ;
#86068 = CARTESIAN_POINT ( 'NONE',  ( 6.565887622018943937, 53.08196800326374643, -12.81628187352647608 ) ) ;
#86070 = CARTESIAN_POINT ( 'NONE',  ( 12.91533473730992121, 29.52201867748817321, 10.88017736071110164 ) ) ;
#86071 = EDGE_CURVE ( 'NONE', #40720, #50188, #68007, .T. ) ;
#86072 = CARTESIAN_POINT ( 'NONE',  ( 21.09922568453595559, 27.04030133659708568, -6.408140936763230044 ) ) ;
#86073 = CARTESIAN_POINT ( 'NONE',  ( 1.472469842513823179, 45.59226448433412315, -4.923371831947296329 ) ) ;
#86074 = CARTESIAN_POINT ( 'NONE',  ( -5.440088680355558814, -2.769647989178489311, -9.422509992056136596 ) ) ;
#86075 = CARTESIAN_POINT ( 'NONE',  ( 10.00000000000000000, 47.87363466993042493, -12.81628187352647608 ) ) ;
#86076 =( BOUNDED_CURVE ( )  B_SPLINE_CURVE ( 2, ( #8446, #53947, #7483, #14487, #75462, #6978, #67972, #15479, #98497 ),
 .UNSPECIFIED., .F., .T. ) 
 B_SPLINE_CURVE_WITH_KNOTS ( ( 3, 2, 2, 2, 3 ),
 ( 0.4401409369402313199, 0.4404761904761904656, 0.4464285714285713969, 0.4523809523809524391, 0.4527162059169115849 ),
 .UNSPECIFIED. ) 
 CURVE ( )  GEOMETRIC_REPRESENTATION_ITEM ( )  RATIONAL_B_SPLINE_CURVE ( ( 0.9963778908391760503, 0.9980808541467920403, 1.000000000000000000, 0.9659258262890682012, 1.000000000000000000, 0.9659258262890682012, 1.000000000000000000, 0.9980808541467920403, 0.9963778908391759392 ) ) 
 REPRESENTATION_ITEM ( '' )  );
#86078 = CARTESIAN_POINT ( 'NONE',  ( 20.04068437667223890, 9.719743609177204036, 6.396802510829703969 ) ) ;
#86077 = CARTESIAN_POINT ( 'NONE',  ( 2.035157376598824452, 58.68868534415482685, 7.964842623401179544 ) ) ;
#86079 = CARTESIAN_POINT ( 'NONE',  ( -8.000000000000000000, 80.07179676972448590, -6.500000000000000888 ) ) ;
#86080 = DIRECTION ( 'NONE',  ( 0.3173046564050899243, 0.000000000000000000, 0.9483236552061999891 ) ) ;
#86081 = CARTESIAN_POINT ( 'NONE',  ( 12.91533473730992121, 54.52201867748816255, 10.88017736071110164 ) ) ;
#86082 = CARTESIAN_POINT ( 'NONE',  ( -0.8801773607111008646, 53.27201867748816966, 2.915334737309923430 ) ) ;
#86083 = CARTESIAN_POINT ( 'NONE',  ( 19.72487221294570858, 56.86607318730075633, 6.500000000000000888 ) ) ;
#86084 = CARTESIAN_POINT ( 'NONE',  ( 10.32896413005679825, 12.60497603579417714, -5.963430220938286119 ) ) ;
#86085 = CARTESIAN_POINT ( 'NONE',  ( 12.91533473730992121, 4.522018677488170546, 10.88017736071110164 ) ) ;
#86086 = CARTESIAN_POINT ( 'NONE',  ( 14.92337183194729988, 59.34226448433412315, -8.527530157486177487 ) ) ;
#86088 = CARTESIAN_POINT ( 'NONE',  ( -4.260926550508235877, -13.83313246298655130, -3.749999999999999112 ) ) ;
#86087 = CARTESIAN_POINT ( 'NONE',  ( 12.91533473730993009, 16.60535201082150891, -10.88017736071109987 ) ) ;
#86089 = CARTESIAN_POINT ( 'NONE',  ( 6.565887622018943937, 28.08196800326375353, -12.81628187352647608 ) ) ;
#86090 = ORIENTED_EDGE ( 'NONE', *, *, #4098, .F. ) ;
#86091 = CARTESIAN_POINT ( 'NONE',  ( -0.8801773607110991993, 57.85535201082149825, -2.915334737309923874 ) ) ;
#86092 = CARTESIAN_POINT ( 'NONE',  ( 7.361572987183169658, 39.96726448433411605, -9.846743663894592657 ) ) ;
#86094 = CARTESIAN_POINT ( 'NONE',  ( 8.979999999999991545, 27.03929484861773958, 3.000000000000000000 ) ) ;
#86093 = CARTESIAN_POINT ( 'NONE',  ( 13.43411237798106583, 12.66530133659708746, -12.81628187352647252 ) ) ;
#86095 = CARTESIAN_POINT ( 'NONE',  ( 7.084665262690076126, 17.02201867748817676, -10.88017736071110164 ) ) ;
#86096 = CARTESIAN_POINT ( 'NONE',  ( 20.88017736071110875, 35.77201867748816966, -2.915334737309920765 ) ) ;
#86097 = CARTESIAN_POINT ( 'NONE',  ( 6.204703633549690345, 50.76208216824730357, -14.16423886937410259 ) ) ;
#86098 = CARTESIAN_POINT ( 'NONE',  ( 14.92337183194729988, 44.34226448433412315, -8.527530157486177487 ) ) ;
#86099 = VECTOR ( 'NONE', #90947, 1000.000000000000000 ) ;
#86100 = CARTESIAN_POINT ( 'NONE',  ( 4.559911319644449179, 53.89701867748817676, 9.422509992056141925 ) ) ;
#86101 = CARTESIAN_POINT ( 'NONE',  ( 13.16740645155971201, 14.95077488074853456, -6.653232860246546920 ) ) ;
#86102 = CARTESIAN_POINT ( 'NONE',  ( 13.79529636645030344, 13.26208216824729824, 14.16423886937410614 ) ) ;
#86103 = B_SPLINE_CURVE_WITH_KNOTS ( 'NONE', 3,
 ( #38273, #68766, #297, #91754, #23276, #53753 ),
 .UNSPECIFIED., .F., .F.,
 ( 4, 2, 4 ),
 ( 0.0002800225282622560924, 0.0006862279780598563861, 0.001092433427857456571 ),
 .UNSPECIFIED. ) ;
#86104 = DIRECTION ( 'NONE',  ( 0.000000000000000000, 1.000000000000000000, 0.000000000000000000 ) ) ;
#86105 = CARTESIAN_POINT ( 'NONE',  ( 2.603489959281581889, 20.43575266056827999, -6.499999999999995559 ) ) ;
#86106 = ORIENTED_EDGE ( 'NONE', *, *, #96583, .T. ) ;
#86107 = VERTEX_POINT ( 'NONE', #82504 ) ;
#86108 = CARTESIAN_POINT ( 'NONE',  ( -2.266590686148945544, 42.22041550158063217, 7.082119434687048631 ) ) ;
#86109 = CARTESIAN_POINT ( 'NONE',  ( 22.26659068614895176, 39.72041550158063217, -7.082119434687042414 ) ) ;
#86110 = CARTESIAN_POINT ( 'NONE',  ( 7.361572987183169658, 14.96726448433411960, -9.846743663894592657 ) ) ;
#86111 = CARTESIAN_POINT ( 'NONE',  ( 22.81628187352647785, 16.41530133659708923, 3.434112377981063169 ) ) ;
#86112 = CARTESIAN_POINT ( 'NONE',  ( 10.00000000000000178, 67.25893115100079456, 9.846743663894594434 ) ) ;
#86113 = DIRECTION ( 'NONE',  ( 1.000000000000000000, 0.000000000000000000, 0.000000000000000000 ) ) ;
#86115 = CARTESIAN_POINT ( 'NONE',  ( -2.816281873526473856, 39.33196800326374643, 3.434112377981055619 ) ) ;
#86114 = CARTESIAN_POINT ( 'NONE',  ( 12.91533473730993009, 56.60535201082151247, -10.88017736071109987 ) ) ;
#86116 = CARTESIAN_POINT ( 'NONE',  ( 22.26659068614895176, 29.72041550158063572, -7.082119434687042414 ) ) ;
#86117 = CARTESIAN_POINT ( 'NONE',  ( 20.88017736071110519, 20.56368534415484106, 2.639326808657452039E-16 ) ) ;
#86118 = CARTESIAN_POINT ( 'NONE',  ( 3.969999999999999751, 10.00000000000000000, -4.000000000000000000 ) ) ;
#86119 = CARTESIAN_POINT ( 'NONE',  ( 15.44008868035555793, 66.39701867748817676, -9.422509992056140149 ) ) ;
#86120 = MECHANICAL_DESIGN_GEOMETRIC_PRESENTATION_REPRESENTATION (  '', ( #94029 ), #98922 ) ;
#86121 = CARTESIAN_POINT ( 'NONE',  ( -2.638427012816840111, -15.03273551566587685, -9.846743663894590881 ) ) ;
#86122 = EDGE_CURVE ( 'NONE', #45903, #56516, #56766, .T. ) ;
#86123 = ORIENTED_EDGE ( 'NONE', *, *, #12478, .T. ) ;
#86124 = FACE_OUTER_BOUND ( 'NONE', #91540, .T. ) ;
#86125 = DIRECTION ( 'NONE',  ( 0.000000000000000000, 1.000000000000000000, 0.000000000000000000 ) ) ;
#86126 = VERTEX_POINT ( 'NONE', #22513 ) ;
#86127 = CARTESIAN_POINT ( 'NONE',  ( -4.164238869374099039, 1.803748834913967647, 8.674139862899312516E-16 ) ) ;
#86129 = CARTESIAN_POINT ( 'NONE',  ( 0.5774900079438607392, 18.48035201082150536, 5.440088680355550821 ) ) ;
#86128 = CARTESIAN_POINT ( 'NONE',  ( 4.559911319644449179, 7.230352010821505360, -9.422509992056141925 ) ) ;
#86131 = CARTESIAN_POINT ( 'NONE',  ( 0.6178305044545818747, 3.498634669930420049, -9.382169495545419124 ) ) ;
#86130 = CARTESIAN_POINT ( 'NONE',  ( 5.076628168052704559, 35.17559781766745175, -8.527530157486179263 ) ) ;
#86132 = LINE ( 'NONE', #62124, #7147 ) ;
#86133 = ADVANCED_FACE ( 'NONE', ( #28518 ), #89515, .F. ) ;
#86134 = DIRECTION ( 'NONE',  ( 0.1736481776669283605, -0.9848077530122084644, 0.000000000000000000 ) ) ;
#86135 = CARTESIAN_POINT ( 'NONE',  ( 22.81628187352647785, 11.41530133659708390, 3.434112377981063169 ) ) ;
#86136 = ORIENTED_EDGE ( 'NONE', *, *, #67304, .T. ) ;
#86137 = CARTESIAN_POINT ( 'NONE',  ( 17.08211943468705840, 50.13708216824730357, -12.26659068614894466 ) ) ;
#86138 = ORIENTED_EDGE ( 'NONE', *, *, #26216, .F. ) ;
#86139 = CARTESIAN_POINT ( 'NONE',  ( -2.266590686148945544, 56.38708216824731068, -7.082119434687050408 ) ) ;
#86140 = ORIENTED_EDGE ( 'NONE', *, *, #97321, .T. ) ;
#86141 = CARTESIAN_POINT ( 'NONE',  ( 20.88017736071110164, 40.35535201082150536, 2.915334737309930979 ) ) ;
#86142 = AXIS2_PLACEMENT_3D ( 'NONE', #58688, #89681, #73189 ) ;
#86143 = CARTESIAN_POINT ( 'NONE',  ( 4.559911319644449179, 37.23035201082150536, -9.422509992056141925 ) ) ;
#86144 = CARTESIAN_POINT ( 'NONE',  ( 20.88017736071110164, 35.35535201082150536, 2.915334737309930979 ) ) ;
#86145 = CARTESIAN_POINT ( 'NONE',  ( -28.94000000000001549, 93.50000000000000000, -9.500000000000000000 ) ) ;
#86146 = CARTESIAN_POINT ( 'NONE',  ( 17.96484262340118221, 26.18868534415483396, -7.964842623401177768 ) ) ;
#86147 = VECTOR ( 'NONE', #64915, 1000.000000000000114 ) ;
#86148 =( BOUNDED_CURVE ( )  B_SPLINE_CURVE ( 2, ( #15504, #22013, #23002, #89995, #13512, #30468, #83491, #82995, #98022 ),
 .UNSPECIFIED., .F., .F. ) 
 B_SPLINE_CURVE_WITH_KNOTS ( ( 3, 2, 2, 2, 3 ),
 ( 0.5829980797973742801, 0.5833333333333333703, 0.5892857142857143016, 0.5952380952380952328, 0.5955733487740544341 ),
 .UNSPECIFIED. ) 
 CURVE ( )  GEOMETRIC_REPRESENTATION_ITEM ( )  RATIONAL_B_SPLINE_CURVE ( ( 0.9963778908391764944, 0.9980808541467923733, 1.000000000000000000, 0.9659258262890682012, 1.000000000000000000, 0.9659258262890682012, 1.000000000000000000, 0.9980808541467918182, 0.9963778908391756062 ) ) 
 REPRESENTATION_ITEM ( '' )  );
#86150 = ORIENTED_EDGE ( 'NONE', *, *, #6509, .T. ) ;
#86149 = DIRECTION ( 'NONE',  ( -0.000000000000000000, 1.000000000000000000, -0.000000000000000000 ) ) ;
#86151 = EDGE_CURVE ( 'NONE', #38777, #73854, #74008, .T. ) ;
#86152 = CARTESIAN_POINT ( 'NONE',  ( 1.472469842513823179, 21.42559781766745175, 4.923371831947296329 ) ) ;
#86153 = EDGE_LOOP ( 'NONE', ( #51092, #82851, #61262, #14321 ) ) ;
#86154 = CARTESIAN_POINT ( 'NONE',  ( 10.00000000000000000, 44.75893115100078745, -9.846743663894594434 ) ) ;
#86156 = EDGE_CURVE ( 'NONE', #20729, #66694, #5035, .T. ) ;
#86155 = DIRECTION ( 'NONE',  ( 0.000000000000000000, 1.000000000000000000, 0.000000000000000000 ) ) ;
#86157 = CARTESIAN_POINT ( 'NONE',  ( 0.4400000000000020006, 1.019547802438468986, 3.750000000000000000 ) ) ;
#86158 = LINE ( 'NONE', #1206, #18755 ) ;
#86159 = VERTEX_POINT ( 'NONE', #21519 ) ;
#86160 = DIRECTION ( 'NONE',  ( -0.000000000000000000, -0.000000000000000000, 1.000000000000000000 ) ) ;
#86161 = CARTESIAN_POINT ( 'NONE',  ( 0.2751277870542967463, 70.00000000000000000, -6.500000000000000888 ) ) ;
#86162 = CARTESIAN_POINT ( 'NONE',  ( 12.63842701281683034, 57.46726448433411605, 9.846743663894596210 ) ) ;
#86163 = CARTESIAN_POINT ( 'NONE',  ( 10.00000000000000178, 48.05374883491396787, 14.16423886937410082 ) ) ;
#86164 = CARTESIAN_POINT ( 'NONE',  ( 5.076628168052703671, 66.84226448433412315, 8.527530157486179263 ) ) ;
#86165 = ORIENTED_EDGE ( 'NONE', *, *, #75674, .F. ) ;
#86166 = SURFACE_SIDE_STYLE ('',( #85669 ) ) ;
#86167 = CARTESIAN_POINT ( 'NONE',  ( 0.1532563361054083140, 21.00893115100078745, 1.131784320476157264E-15 ) ) ;
#86168 = CARTESIAN_POINT ( 'NONE',  ( -2.816281873526471635, 58.91530133659707502, -3.434112377981056508 ) ) ;
#86169 = VECTOR ( 'NONE', #43873, 1000.000000000000114 ) ;
#86170 = CARTESIAN_POINT ( 'NONE',  ( 12.63842701281683922, 59.55059781766744464, -9.846743663894590881 ) ) ;
#86171 = CARTESIAN_POINT ( 'NONE',  ( -0.8801773607111008646, 63.27201867748817676, 2.915334737309923430 ) ) ;
#86172 = CARTESIAN_POINT ( 'NONE',  ( 17.20831665107776587, 44.13393115100078745, -7.208316651077762316 ) ) ;
#86173 = CARTESIAN_POINT ( 'NONE',  ( 20.15039907845754286, 14.72266099184918531, 6.262539305110064625 ) ) ;
#86174 = EDGE_CURVE ( 'NONE', #37579, #65662, #17863, .T. ) ;
#86175 = EDGE_LOOP ( 'NONE', ( #11598, #6685, #34209, #96709 ) ) ;
#86176 = CARTESIAN_POINT ( 'NONE',  ( -2.266590686148945544, 66.38708216824730357, -7.082119434687050408 ) ) ;
#86177 = PLANE ( 'NONE',  #7424 ) ;
#86178 = CARTESIAN_POINT ( 'NONE',  ( 20.88017736071110875, 45.77201867748816966, -2.915334737309920765 ) ) ;
#86180 = CARTESIAN_POINT ( 'NONE',  ( -0.8801773607111009756, 68.06368534415484817, 1.068504757029289695E-15 ) ) ;
#86179 = CARTESIAN_POINT ( 'NONE',  ( 19.38216949554541557, 17.24863466993041783, -9.382169495545420901 ) ) ;
#86181 = CARTESIAN_POINT ( 'NONE',  ( 14.16722289976685722, 14.63595249122789177, -4.928467845925526447 ) ) ;
#86183 = EDGE_CURVE ( 'NONE', #51686, #10866, #6025, .T. ) ;
#86182 = DIRECTION ( 'NONE',  ( -0.000000000000000000, -1.000000000000000000, -0.000000000000000000 ) ) ;
#86184 = DIRECTION ( 'NONE',  ( -1.000000000000000000, 0.000000000000000000, 0.000000000000000000 ) ) ;
#86185 = CARTESIAN_POINT ( 'NONE',  ( -14.16722289976689630, 14.63595249122789532, 4.928467845925427859 ) ) ;
#86186 = CARTESIAN_POINT ( 'NONE',  ( 18.52753015748618282, 48.92559781766745886, -4.923371831947291888 ) ) ;
#86187 = CARTESIAN_POINT ( 'NONE',  ( 0.1532563361054082862, 6.217264484334118713, 2.638427012816831674 ) ) ;
#86188 = CARTESIAN_POINT ( 'NONE',  ( 7.082119434687047743, 30.13708216824731423, -12.26659068614894821 ) ) ;
#86189 = CARTESIAN_POINT ( 'NONE',  ( 16.40814093676323893, 10.79030133659708923, 11.09922568453595026 ) ) ;
#86190 = CARTESIAN_POINT ( 'NONE',  ( 17.96484262340118221, 9.938685344154839285, 7.964842623401181321 ) ) ;
#86191 = DIRECTION ( 'NONE',  ( -1.000000000000000000, 0.000000000000000000, 0.000000000000000000 ) ) ;
#86192 = CARTESIAN_POINT ( 'NONE',  ( 10.00000000000000178, 33.05374883491396787, 14.16423886937410082 ) ) ;
#86193 = CARTESIAN_POINT ( 'NONE',  ( 17.08211943468705130, 28.47041550158063572, 12.26659068614894998 ) ) ;
#86194 = CARTESIAN_POINT ( 'NONE',  ( 24.16423886937410614, 59.30374883491397497, 8.672049930838204340E-16 ) ) ;
#86195 = CARTESIAN_POINT ( 'NONE',  ( 21.09922568453594849, 36.20696800326375353, 6.408140936763242479 ) ) ;
#86196 = CARTESIAN_POINT ( 'NONE',  ( 19.42250999205614548, 10.98035201082150358, -5.440088680355545492 ) ) ;
#86197 = ORIENTED_EDGE ( 'NONE', *, *, #60532, .F. ) ;
#86198 = CARTESIAN_POINT ( 'NONE',  ( 0.1532563361054083140, 41.00893115100078745, 1.131784320476157264E-15 ) ) ;
#86199 = CARTESIAN_POINT ( 'NONE',  ( 10.00000000000000000, 46.81368534415484106, -10.88017736071110342 ) ) ;
#86200 = CARTESIAN_POINT ( 'NONE',  ( 17.20831665107776587, 64.13393115100079456, -7.208316651077762316 ) ) ;
#86202 = DIRECTION ( 'NONE',  ( -0.000000000000000000, -0.000000000000000000, -1.000000000000000000 ) ) ;
#86201 = CARTESIAN_POINT ( 'NONE',  ( 13.79529636645031943, 15.34541550158063750, -14.16423886937409904 ) ) ;
#86203 = CARTESIAN_POINT ( 'NONE',  ( 18.50749283717776805, 34.69955587570481015, 6.500000000000000888 ) ) ;
#86204 = UNCERTAINTY_MEASURE_WITH_UNIT (LENGTH_MEASURE( 1.000000000000000082E-05 ), #63143, 'distance_accuracy_value', 'NONE');
#86205 = CARTESIAN_POINT ( 'NONE',  ( 14.92337183194729988, 19.34226448433411960, -8.527530157486177487 ) ) ;
#86206 = CARTESIAN_POINT ( 'NONE',  ( 6.565887622018943937, 45.16530133659708923, 12.81628187352647430 ) ) ;
#86207 = CARTESIAN_POINT ( 'NONE',  ( 7.361572987183170547, 57.05059781766744464, 9.846743663894590881 ) ) ;
#86208 = ORIENTED_EDGE ( 'NONE', *, *, #56040, .T. ) ;
#86209 = DIRECTION ( 'NONE',  ( 0.000000000000000000, 0.000000000000000000, 1.000000000000000000 ) ) ;
#86210 = CIRCLE ( 'NONE', #62210, 15.00000000000000000 ) ;
#86211 = CARTESIAN_POINT ( 'NONE',  ( 17.96484262340118221, 4.938685344154837509, 7.964842623401181321 ) ) ;
#86212 = CARTESIAN_POINT ( 'NONE',  ( 10.00000000000000178, 8.053748834913967869, 14.16423886937410082 ) ) ;
#86213 = CARTESIAN_POINT ( 'NONE',  ( 10.00000000000000178, 69.31368534415484817, 10.88017736071110342 ) ) ;
#86214 = CARTESIAN_POINT ( 'NONE',  ( 18.52753015748618282, 48.92559781766745886, -4.923371831947291888 ) ) ;
#86215 = CARTESIAN_POINT ( 'NONE',  ( 4.559911319644449179, 23.89701867748817321, 9.422509992056141925 ) ) ;
#86216 = CARTESIAN_POINT ( 'NONE',  ( 0.1532563361054083140, 61.00893115100078745, 1.131784320476157264E-15 ) ) ;
#86217 = CIRCLE ( 'NONE', #84644, 5.999999999999998224 ) ;
#86218 = PRESENTATION_STYLE_ASSIGNMENT (( #24252 ) ) ;
#86219 = CARTESIAN_POINT ( 'NONE',  ( -8.157527544167827216, 14.76984925468920196, 12.51706795611529621 ) ) ;
#86220 = ORIENTED_EDGE ( 'NONE', *, *, #63902, .T. ) ;
#86221 = VERTEX_POINT ( 'NONE', #14521 ) ;
#86222 = CARTESIAN_POINT ( 'NONE',  ( 34.56412365047464874, 29.50000000000000000, 9.500000000000000000 ) ) ;
#86223 = CARTESIAN_POINT ( 'NONE',  ( 18.72515096720583827, 30.05509018479937566, 6.499999999999810818 ) ) ;
#86224 = CARTESIAN_POINT ( 'NONE',  ( -10.77730536144846596, -98.63085534186639336, -3.750000000000000000 ) ) ;
#86225 = CARTESIAN_POINT ( 'NONE',  ( 2.917880565312948704, 37.63708216824731068, 12.26659068614894643 ) ) ;
#86226 = CARTESIAN_POINT ( 'NONE',  ( 0.1532563361054083140, 51.00893115100078745, 1.131784320476157264E-15 ) ) ;
#86227 = CARTESIAN_POINT ( 'NONE',  ( 5.076628168052703671, 26.84226448433411960, 8.527530157486179263 ) ) ;
#86229 = CARTESIAN_POINT ( 'NONE',  ( 19.84674366389459266, 63.71726448433412315, -2.638427012816827677 ) ) ;
#86228 = CARTESIAN_POINT ( 'NONE',  ( 20.88017736071110164, 20.35535201082150891, 2.915334737309930979 ) ) ;
#86230 = CARTESIAN_POINT ( 'NONE',  ( -6.000000000000000000, 78.07179676972447169, -6.500000000000000888 ) ) ;
#86231 = CARTESIAN_POINT ( 'NONE',  ( 17.08211943468705130, 38.47041550158063217, 12.26659068614894998 ) ) ;
#86232 = CARTESIAN_POINT ( 'NONE',  ( 10.00000000000000178, 68.05374883491397497, 14.16423886937410082 ) ) ;
#86233 = CARTESIAN_POINT ( 'NONE',  ( -42.50369195530268485, 107.9060299417078426, 4.500000000000000888 ) ) ;
#86234 = CARTESIAN_POINT ( 'NONE',  ( 17.99999999999999645, 78.53751499213471732, 3.955843470927898675 ) ) ;
#86235 = CARTESIAN_POINT ( 'NONE',  ( 19.42250999205614193, 60.14701867748817676, 5.440088680355555262 ) ) ;
#86236 = CARTESIAN_POINT ( 'NONE',  ( 5.076628168052704559, 10.17559781766745175, -8.527530157486179263 ) ) ;
#86237 = CARTESIAN_POINT ( 'NONE',  ( -6.982525766850296911, -88.11956318484570261, 3.750000000000000000 ) ) ;
#86238 = ORIENTED_EDGE ( 'NONE', *, *, #89636, .T. ) ;
#86239 = CARTESIAN_POINT ( 'NONE',  ( -14.15369600240089909, 15.00000000000000888, 3.689340892730124555 ) ) ;
#86240 = EDGE_LOOP ( 'NONE', ( #24562, #51813, #19701, #79795 ) ) ;
#86241 = CARTESIAN_POINT ( 'NONE',  ( 17.20831665107776587, 27.88393115100078390, 7.208316651077764980 ) ) ;
#86242 = ORIENTED_EDGE ( 'NONE', *, *, #67747, .F. ) ;
#86243 = CARTESIAN_POINT ( 'NONE',  ( 20.36894250292379738, 29.92874883491396432, -10.36894250292379027 ) ) ;
#86244 = CARTESIAN_POINT ( 'NONE',  ( 17.20831665107776587, 34.13393115100078745, -7.208316651077762316 ) ) ;
#86245 = CARTESIAN_POINT ( 'NONE',  ( 2.035157376598824452, 38.68868534415483396, 7.964842623401179544 ) ) ;
#86246 = EDGE_CURVE ( 'NONE', #60661, #15080, #44990, .T. ) ;
#86247 = FILL_AREA_STYLE_COLOUR ( '', #7549 ) ;
#86248 = ORIENTED_EDGE ( 'NONE', *, *, #98035, .T. ) ;
#86249 = CARTESIAN_POINT ( 'NONE',  ( 4.559911319644449179, 37.23035201082150536, -9.422509992056141925 ) ) ;
#86250 = CARTESIAN_POINT ( 'NONE',  ( 12.34557190004675320, 14.95077488074853633, 8.076692058882576575 ) ) ;
#86251 = CARTESIAN_POINT ( 'NONE',  ( -6.408140936763246032, -1.709698663402911656, -11.09922568453594316 ) ) ;
#86252 = VERTEX_POINT ( 'NONE', #54461 ) ;
#86253 = CARTESIAN_POINT ( 'NONE',  ( -4.164238869374098151, 11.59541550158063217, -3.795296366450310543 ) ) ;
#86254 = ORIENTED_EDGE ( 'NONE', *, *, #97258, .T. ) ;
#86255 = EDGE_LOOP ( 'NONE', ( #10653, #1319, #13696, #32044 ) ) ;
#86256 = CARTESIAN_POINT ( 'NONE',  ( 16.40814093676324603, 32.45696800326375353, -11.09922568453594671 ) ) ;
#86257 = DIRECTION ( 'NONE',  ( -5.818595309480553908E-17, -1.000000000000000000, -0.000000000000000000 ) ) ;
#86258 = CARTESIAN_POINT ( 'NONE',  ( 19.84674366389459266, 18.30059781766745175, 2.638427012816836559 ) ) ;
#86259 = LINE ( 'NONE', #18258, #41886 ) ;
#86260 = FACE_OUTER_BOUND ( 'NONE', #26719, .T. ) ;
#86261 = CARTESIAN_POINT ( 'NONE',  ( 1.472469842513823179, 30.59226448433411960, -4.923371831947296329 ) ) ;
#86263 = VECTOR ( 'NONE', #26801, 1000.000000000000000 ) ;
#86262 = CARTESIAN_POINT ( 'NONE',  ( -0.8801773607111009756, 58.06368534415484106, 1.068504757029289695E-15 ) ) ;
#86264 = EDGE_CURVE ( 'NONE', #74198, #42986, #20084, .T. ) ;
#86265 = DIRECTION ( 'NONE',  ( -0.3665012267242880872, 0.000000000000000000, -0.9304175679820281264 ) ) ;
#86266 = CARTESIAN_POINT ( 'NONE',  ( 2.035157376598822676, 67.43868534415484817, -7.964842623401177768 ) ) ;
#86267 = CARTESIAN_POINT ( 'NONE',  ( 0.000000000000000000, 15.00000000000000000, 0.000000000000000000 ) ) ;
#86268 = CARTESIAN_POINT ( 'NONE',  ( 4.469999999999999751, 36.75000000000000000, -3.750000000000000000 ) ) ;
#86269 = CARTESIAN_POINT ( 'NONE',  ( 12.63842701281683034, 2.467264484334118269, 9.846743663894596210 ) ) ;
#86270 = EDGE_CURVE ( 'NONE', #45712, #55747, #84487, .T. ) ;
#86271 = CARTESIAN_POINT ( 'NONE',  ( 13.43411237798106583, 7.665301336597086568, -12.81628187352647252 ) ) ;
#86272 = AXIS2_PLACEMENT_3D ( 'NONE', #72903, #78937, #11919 ) ;
#86273 = CARTESIAN_POINT ( 'NONE',  ( -6.732636091893141383, -88.11213685669363826, -2.750000000000000000 ) ) ;
#86274 =( GEOMETRIC_REPRESENTATION_CONTEXT ( 3 ) GLOBAL_UNCERTAINTY_ASSIGNED_CONTEXT ( ( #17227 ) ) GLOBAL_UNIT_ASSIGNED_CONTEXT ( ( #48315, #33306, #70847 ) ) REPRESENTATION_CONTEXT ( 'NONE', 'WORKASPACE' ) );
#86275 = CARTESIAN_POINT ( 'NONE',  ( 18.52753015748617571, 48.09226448433412315, 4.923371831947298993 ) ) ;
#86276 = DIRECTION ( 'NONE',  ( 0.000000000000000000, -0.000000000000000000, -1.000000000000000000 ) ) ;
#86277 = CARTESIAN_POINT ( 'NONE',  ( 22.26659068614894466, 3.887082168247300906, 7.082119434687054849 ) ) ;
#86278 = CARTESIAN_POINT ( 'NONE',  ( 0.1532563361054083140, 16.00893115100078390, 1.131784320476157264E-15 ) ) ;
#86279 = CARTESIAN_POINT ( 'NONE',  ( -1.099225684535947600, 39.54030133659708923, 6.408140936763237150 ) ) ;
#86281 = CARTESIAN_POINT ( 'NONE',  ( -4.084234479374336146, 0.000000000000000000, 3.613425430272898975 ) ) ;
#86280 = FILL_AREA_STYLE_COLOUR ( '', #98002 ) ;
#86282 = CARTESIAN_POINT ( 'NONE',  ( 20.88017736071110519, 50.56368534415484106, 2.639326808657452039E-16 ) ) ;
#86283 = AXIS2_PLACEMENT_3D ( 'NONE', #39295, #55768, #78760 ) ;
#86284 = CARTESIAN_POINT ( 'NONE',  ( 10.00000000000000000, 12.87363466993042138, -12.81628187352647608 ) ) ;
#86285 = CARTESIAN_POINT ( 'NONE',  ( 2.603489959281614308, 41.58210964143329846, 6.500000000000031086 ) ) ;
#86286 = CARTESIAN_POINT ( 'NONE',  ( 10.00000000000000000, 24.75893115100078745, -9.846743663894594434 ) ) ;
#86287 = CARTESIAN_POINT ( 'NONE',  ( 2.035157376598822676, 32.43868534415483396, -7.964842623401177768 ) ) ;
#86288 = CARTESIAN_POINT ( 'NONE',  ( 0.6178305044545838731, 34.74863466993042493, 9.382169495545420901 ) ) ;
#86289 = CARTESIAN_POINT ( 'NONE',  ( 10.00000000000000178, 17.25893115100078745, 9.846743663894594434 ) ) ;
#86290 = FILL_AREA_STYLE_COLOUR ( '', #39085 ) ;
#86291 = LINE ( 'NONE', #8809, #58192 ) ;
#86292 = CARTESIAN_POINT ( 'NONE',  ( 7.084665262690076126, 22.02201867748817321, -10.88017736071110164 ) ) ;
#86293 = ORIENTED_EDGE ( 'NONE', *, *, #71757, .F. ) ;
#86294 = CARTESIAN_POINT ( 'NONE',  ( 20.88017736071110519, 55.56368534415484817, 2.639326808657452039E-16 ) ) ;
#86295 = CARTESIAN_POINT ( 'NONE',  ( -0.8801773607110991993, 7.855352010821504471, -2.915334737309923874 ) ) ;
#86297 = CARTESIAN_POINT ( 'NONE',  ( 15.44008868035555260, 14.73035201082150536, 9.422509992056143702 ) ) ;
#86296 = CARTESIAN_POINT ( 'NONE',  ( 18.52753015748618282, 38.92559781766745175, -4.923371831947291888 ) ) ;
#86298 = PRESENTATION_STYLE_ASSIGNMENT (( #92804 ) ) ;
#86299 = CARTESIAN_POINT ( 'NONE',  ( 10.00000000000000000, 41.81368534415484106, -10.88017736071110342 ) ) ;
#86301 = CARTESIAN_POINT ( 'NONE',  ( 19.89220837332773684, 59.74062864464242040, 6.478736007406005193 ) ) ;
#86300 = CARTESIAN_POINT ( 'NONE',  ( 10.00000000000000178, 19.31368534415484106, 10.88017736071110342 ) ) ;
#86302 = AXIS2_PLACEMENT_3D ( 'NONE', #8597, #47074, #47579 ) ;
#86303 = CARTESIAN_POINT ( 'NONE',  ( 5.076628168052703671, 31.84226448433412315, 8.527530157486179263 ) ) ;
#86304 = LINE ( 'NONE', #48782, #32995 ) ;
#86305 = DIRECTION ( 'NONE',  ( -1.000000000000000000, 0.000000000000000000, 0.000000000000000000 ) ) ;
#86306 = EDGE_CURVE ( 'NONE', #70448, #63236, #61471, .T. ) ;
#86307 = CARTESIAN_POINT ( 'NONE',  ( 21.09922568453594849, 1.206968003263753531, 6.408140936763242479 ) ) ;
#86308 = DIRECTION ( 'NONE',  ( 0.000000000000000000, 1.000000000000000000, 0.000000000000000000 ) ) ;
#86309 = CARTESIAN_POINT ( 'NONE',  ( 13.79529636645031943, 25.34541550158063572, -14.16423886937409904 ) ) ;
#86311 = DIRECTION ( 'NONE',  ( 0.000000000000000000, 0.000000000000000000, -1.000000000000000000 ) ) ;
#86310 = AXIS2_PLACEMENT_3D ( 'NONE', #53688, #8204, #15714 ) ;
#86312 = VERTEX_POINT ( 'NONE', #39965 ) ;
#86313 = CARTESIAN_POINT ( 'NONE',  ( 24.16423886937410614, 64.30374883491396076, 8.672049930838204340E-16 ) ) ;
#86314 = CARTESIAN_POINT ( 'NONE',  ( 1.472469842513823179, 21.42559781766745175, 4.923371831947296329 ) ) ;
#86315 = CARTESIAN_POINT ( 'NONE',  ( -8.114998381645635916, 86.24535146302233102, -4.289708087854925189 ) ) ;
#86316 = CARTESIAN_POINT ( 'NONE',  ( 0.5774900079438607392, 43.48035201082151247, 5.440088680355550821 ) ) ;
#86317 = CARTESIAN_POINT ( 'NONE',  ( -2.816281873526471635, 58.91530133659707502, -3.434112377981056508 ) ) ;
#86318 = CARTESIAN_POINT ( 'NONE',  ( 20.88017736071110164, 30.35535201082151247, 2.915334737309930979 ) ) ;
#86319 = CYLINDRICAL_SURFACE ( 'NONE', #81835, 11.92686044187656513 ) ;
#86320 = CARTESIAN_POINT ( 'NONE',  ( 16.40814093676323893, 10.79030133659708923, 11.09922568453595026 ) ) ;
#86321 = CARTESIAN_POINT ( 'NONE',  ( 1.472469842513823179, 21.42559781766745175, 4.923371831947296329 ) ) ;
#86322 = ORIENTED_EDGE ( 'NONE', *, *, #6894, .T. ) ;
#86323 = LINE ( 'NONE', #32319, #24545 ) ;
#86324 = CARTESIAN_POINT ( 'NONE',  ( -7.750000000000000000, 0.000000000000000000, 4.000000000000000000 ) ) ;
#86325 = CARTESIAN_POINT ( 'NONE',  ( -2.266590686148945544, 52.22041550158064638, 7.082119434687048631 ) ) ;
#86326 = CARTESIAN_POINT ( 'NONE',  ( 22.26659068614894466, 28.88708216824730357, 7.082119434687054849 ) ) ;
#86327 = CARTESIAN_POINT ( 'NONE',  ( 20.88017736071110164, 25.35535201082150891, 2.915334737309930979 ) ) ;
#86328 = CARTESIAN_POINT ( 'NONE',  ( 20.88017736071110519, 50.56368534415484106, 2.639326808657452039E-16 ) ) ;
#86329 = DIRECTION ( 'NONE',  ( -0.000000000000000000, -1.000000000000000000, -0.000000000000000000 ) ) ;
#86330 = CARTESIAN_POINT ( 'NONE',  ( 70.68973184038034674, 41.77083333333331439, -9.500000000000000000 ) ) ;
#86331 = CARTESIAN_POINT ( 'NONE',  ( 17.20831665107776587, 14.13393115100078568, -7.208316651077762316 ) ) ;
#86332 = CARTESIAN_POINT ( 'NONE',  ( 6.880000000000009663, 41.24999999999999289, -6.250000000000000000 ) ) ;
#86333 = CARTESIAN_POINT ( 'NONE',  ( 19.84674366389459266, 18.71726448433411960, -2.638427012816827677 ) ) ;
#86334 = SURFACE_STYLE_FILL_AREA ( #55840 ) ;
#86335 = CARTESIAN_POINT ( 'NONE',  ( 1.472469842513823179, 30.59226448433411960, -4.923371831947296329 ) ) ;
#86336 = CARTESIAN_POINT ( 'NONE',  ( 18.52753015748618282, 48.92559781766745886, -4.923371831947291888 ) ) ;
#86337 = CARTESIAN_POINT ( 'NONE',  ( 7.084665262690076126, 22.02201867748817321, -10.88017736071110164 ) ) ;
#86338 = UNCERTAINTY_MEASURE_WITH_UNIT (LENGTH_MEASURE( 1.000000000000000082E-05 ), #6784, 'distance_accuracy_value', 'NONE');
#86339 = AXIS2_PLACEMENT_3D ( 'NONE', #64528, #16599, #2110 ) ;
#86340 = CARTESIAN_POINT ( 'NONE',  ( 22.81628187352647785, 36.41530133659707502, 3.434112377981063169 ) ) ;
#86341 = CARTESIAN_POINT ( 'NONE',  ( 12.91533473730993009, 56.60535201082151247, -10.88017736071109987 ) ) ;
#86342 = CARTESIAN_POINT ( 'NONE',  ( 19.84674366389459266, 23.30059781766745530, 2.638427012816836559 ) ) ;
#86344 = CARTESIAN_POINT ( 'NONE',  ( 19.84674366389459266, 28.71726448433411960, -2.638427012816827677 ) ) ;
#86343 = CARTESIAN_POINT ( 'NONE',  ( 22.26659068614895176, 39.72041550158063217, -7.082119434687042414 ) ) ;
#86345 = CARTESIAN_POINT ( 'NONE',  ( -0.1503990784575329198, 2.222660991849184864, -6.262539305110070842 ) ) ;
#86346 = CARTESIAN_POINT ( 'NONE',  ( 10.00000000000000178, 47.25893115100078745, 9.846743663894594434 ) ) ;
#86348 = CARTESIAN_POINT ( 'NONE',  ( -4.164238869374098151, 6.595415501580634832, -3.795296366450310543 ) ) ;
#86347 = CARTESIAN_POINT ( 'NONE',  ( 5.076628168052703671, 26.84226448433411960, 8.527530157486179263 ) ) ;
#86349 = CARTESIAN_POINT ( 'NONE',  ( 17.08211943468705130, 13.47041550158063572, 12.26659068614894998 ) ) ;
#86350 = CARTESIAN_POINT ( 'NONE',  ( 17.20831665107776587, 27.88393115100078390, 7.208316651077764980 ) ) ;
#86351 = CIRCLE ( 'NONE', #84700, 19.99999999999999645 ) ;
#86352 = CARTESIAN_POINT ( 'NONE',  ( 0.5774900079438607392, 43.48035201082151247, 5.440088680355550821 ) ) ;
#86353 = CARTESIAN_POINT ( 'NONE',  ( 2.035157376598822676, 22.43868534415483396, -7.964842623401177768 ) ) ;
#86354 = AXIS2_PLACEMENT_3D ( 'NONE', #59517, #6517, #51027 ) ;
#86355 = CARTESIAN_POINT ( 'NONE',  ( 4.559911319644449179, 47.23035201082150536, -9.422509992056141925 ) ) ;
#86356 = CARTESIAN_POINT ( 'NONE',  ( 0.5774900079438607392, 33.48035201082150536, 5.440088680355550821 ) ) ;
#86357 = ORIENTED_EDGE ( 'NONE', *, *, #87058, .T. ) ;
#86358 = AXIS2_PLACEMENT_3D ( 'NONE', #91662, #45667, #98200 ) ;
#86359 = CARTESIAN_POINT ( 'NONE',  ( -0.8801773607111009756, 58.06368534415484106, 1.068504757029289695E-15 ) ) ;
#86360 = ORIENTED_EDGE ( 'NONE', *, *, #97677, .T. ) ;
#86361 = CARTESIAN_POINT ( 'NONE',  ( -9.240973841163681257, 4.382479893023984083E-16, 11.17382667070366331 ) ) ;
#86362 = EDGE_CURVE ( 'NONE', #11778, #53014, #50089, .T. ) ;
#86363 = CARTESIAN_POINT ( 'NONE',  ( 10.00000000000000000, 61.81368534415484106, -10.88017736071110342 ) ) ;
#86364 = ORIENTED_EDGE ( 'NONE', *, *, #41252, .F. ) ;
#86365 = LINE ( 'NONE', #88815, #14193 ) ;
#86366 = CARTESIAN_POINT ( 'NONE',  ( 20.88017736071110875, 5.772018677488170546, -2.915334737309920765 ) ) ;
#86367 = CARTESIAN_POINT ( 'NONE',  ( 1.932340009482140353, 26.49127512925449324, -6.499999999999992006 ) ) ;
#86368 = LINE ( 'NONE', #70880, #28072 ) ;
#86369 = CARTESIAN_POINT ( 'NONE',  ( 22.26659068614895176, 59.72041550158063927, -7.082119434687042414 ) ) ;
#86370 = CARTESIAN_POINT ( 'NONE',  ( 5.076628168052704559, 5.175597817667451750, -8.527530157486179263 ) ) ;
#86371 = CARTESIAN_POINT ( 'NONE',  ( 6.204703633549690345, 0.7620821682473009062, -14.16423886937410259 ) ) ;
#86372 = CARTESIAN_POINT ( 'NONE',  ( 17.20831665107776587, 4.133931151000785675, -7.208316651077762316 ) ) ;
#86373 = CARTESIAN_POINT ( 'NONE',  ( 19.42250999205614193, 5.147018677488171434, 5.440088680355555262 ) ) ;
#86374 = CARTESIAN_POINT ( 'NONE',  ( 18.52753015748617571, 43.09226448433412315, 4.923371831947298993 ) ) ;
#86375 = ORIENTED_EDGE ( 'NONE', *, *, #49716, .T. ) ;
#86376 = CARTESIAN_POINT ( 'NONE',  ( 1.472469842513823179, 45.59226448433412315, -4.923371831947296329 ) ) ;
#86377 = ORIENTED_EDGE ( 'NONE', *, *, #81063, .F. ) ;
#86378 = DIRECTION ( 'NONE',  ( 0.000000000000000000, 0.000000000000000000, -1.000000000000000000 ) ) ;
#86379 = CARTESIAN_POINT ( 'NONE',  ( 19.42250999205614193, 55.14701867748817676, 5.440088680355555262 ) ) ;
#86380 = CARTESIAN_POINT ( 'NONE',  ( 7.361572987183170547, 57.05059781766744464, 9.846743663894590881 ) ) ;
#86382 = FACE_OUTER_BOUND ( 'NONE', #58063, .T. ) ;
#86381 = SURFACE_STYLE_USAGE ( .BOTH. , #1916 ) ;
#86383 = CARTESIAN_POINT ( 'NONE',  ( 0.5774900079438607392, 58.48035201082151247, 5.440088680355550821 ) ) ;
#86384 = CARTESIAN_POINT ( 'NONE',  ( 7.084665262690076126, 2.022018677488171434, -10.88017736071110164 ) ) ;
#86385 = CIRCLE ( 'NONE', #76738, 2.000000000000000000 ) ;
#86386 = EDGE_CURVE ( 'NONE', #1778, #1194, #87103, .T. ) ;
#86387 = CARTESIAN_POINT ( 'NONE',  ( 19.38216949554541202, 40.99863466993042493, 9.382169495545424454 ) ) ;
#86388 = CARTESIAN_POINT ( 'NONE',  ( 0.1143410931637261624, 10.21691075486302580, 6.480892540919854561 ) ) ;
#86389 = ORIENTED_EDGE ( 'NONE', *, *, #65153, .F. ) ;
#86390 = CARTESIAN_POINT ( 'NONE',  ( 0.6178305044545838731, 29.74863466993042138, 9.382169495545420901 ) ) ;
#86391 = CARTESIAN_POINT ( 'NONE',  ( -0.8801773607111008646, 38.27201867748816255, 2.915334737309923430 ) ) ;
#86392 = EDGE_CURVE ( 'NONE', #67453, #50286, #43987, .T. ) ;
#86393 = ORIENTED_EDGE ( 'NONE', *, *, #81565, .F. ) ;
#86394 = FACE_OUTER_BOUND ( 'NONE', #87974, .T. ) ;
#86395 = CARTESIAN_POINT ( 'NONE',  ( 19.84674366389459621, 63.50893115100078745, 7.409399052514197653E-17 ) ) ;
#86397 = CARTESIAN_POINT ( 'NONE',  ( 7.361572987183170547, 37.05059781766744464, 9.846743663894590881 ) ) ;
#86396 = CARTESIAN_POINT ( 'NONE',  ( 7.361572987183170547, 17.05059781766745530, 9.846743663894590881 ) ) ;
#86398 = CARTESIAN_POINT ( 'NONE',  ( -0.03932841506543702931, 28.12161441960501307, 6.397827110478937485 ) ) ;
#86399 = FACE_OUTER_BOUND ( 'NONE', #73309, .T. ) ;
#86400 = MECHANICAL_DESIGN_GEOMETRIC_PRESENTATION_REPRESENTATION (  '', ( #8184 ), #78476 ) ;
#86401 = CARTESIAN_POINT ( 'NONE',  ( 2.791683348922240793, 36.63393115100078035, 7.208316651077764092 ) ) ;
#86402 = CARTESIAN_POINT ( 'NONE',  ( 0.000000000000000000, 0.5000000000000004441, 0.000000000000000000 ) ) ;
#86403 = CARTESIAN_POINT ( 'NONE',  ( -10.88853822400146676, 46.97908644289115898, -2.900000000000000799 ) ) ;
#86405 = FACE_OUTER_BOUND ( 'NONE', #37150, .T. ) ;
#86404 = CARTESIAN_POINT ( 'NONE',  ( 5.076628168052703671, 21.84226448433411960, 8.527530157486179263 ) ) ;
#86406 = DIRECTION ( 'NONE',  ( 0.000000000000000000, 0.000000000000000000, 1.000000000000000000 ) ) ;
#86408 = ORIENTED_EDGE ( 'NONE', *, *, #68403, .T. ) ;
#86407 = CARTESIAN_POINT ( 'NONE',  ( 5.076628168052703671, 46.84226448433412315, 8.527530157486179263 ) ) ;
#86409 = AXIS2_PLACEMENT_3D ( 'NONE', #60982, #7522, #60497 ) ;
#86410 =( LENGTH_UNIT ( ) NAMED_UNIT ( * ) SI_UNIT ( .MILLI., .METRE. ) );
#86411 = CARTESIAN_POINT ( 'NONE',  ( 16.40814093676323893, 25.79030133659708923, 11.09922568453595026 ) ) ;
#86412 = CARTESIAN_POINT ( 'NONE',  ( 18.52753015748617571, 43.09226448433412315, 4.923371831947298993 ) ) ;
#86413 = CARTESIAN_POINT ( 'NONE',  ( 4.879999999999994564, 43.00000000000000711, -6.500000000000000888 ) ) ;
#86414 = CARTESIAN_POINT ( 'NONE',  ( 22.26659068614894466, 48.88708216824730357, 7.082119434687054849 ) ) ;
#86415 = CARTESIAN_POINT ( 'NONE',  ( 14.92337183194729633, 22.67559781766745175, 8.527530157486181039 ) ) ;
#86417 = CARTESIAN_POINT ( 'NONE',  ( 1.472469842513823179, 1.425597817667451528, 4.923371831947296329 ) ) ;
#86416 = TOROIDAL_SURFACE ( 'NONE', #51218, 14.49999999999999822, 0.5000000000000000000 ) ;
#86418 = CARTESIAN_POINT ( 'NONE',  ( -13.86102707272226731, -2.652907190800467873E-15, 4.666951904077105695 ) ) ;
#86419 = CARTESIAN_POINT ( 'NONE',  ( 20.36894250292379738, 44.92874883491396787, -10.36894250292379027 ) ) ;
#86420 = CARTESIAN_POINT ( 'NONE',  ( 10.00000000000000178, 62.25893115100078745, 9.846743663894594434 ) ) ;
#86421 = CARTESIAN_POINT ( 'NONE',  ( 20.88017736071110164, 5.355352010821503583, 2.915334737309930979 ) ) ;
#86422 = CARTESIAN_POINT ( 'NONE',  ( -0.3689425029237898834, 21.17874883491396432, -10.36894250292378850 ) ) ;
#86423 = CARTESIAN_POINT ( 'NONE',  ( 17.08211943468705130, 38.47041550158063217, 12.26659068614894998 ) ) ;
#86424 = DIRECTION ( 'NONE',  ( -0.000000000000000000, 1.000000000000000000, 0.000000000000000000 ) ) ;
#86426 = CARTESIAN_POINT ( 'NONE',  ( 18.52753015748617571, 58.09226448433411605, 4.923371831947298993 ) ) ;
#86425 = CARTESIAN_POINT ( 'NONE',  ( -8.157527544166347511, 0.2301507453079257859, -12.51706795611459100 ) ) ;
#86427 = ORIENTED_EDGE ( 'NONE', *, *, #19935, .F. ) ;
#86428 = CARTESIAN_POINT ( 'NONE',  ( -0.8801773607111008646, 38.27201867748816255, 2.915334737309923430 ) ) ;
#86429 = CARTESIAN_POINT ( 'NONE',  ( 19.80427997160309417, 22.75733960839544778, -6.499999999999987566 ) ) ;
#86430 = CARTESIAN_POINT ( 'NONE',  ( 9.113259239972942183, -7.249774014816905421, 3.750000000000001332 ) ) ;
#86431 = EDGE_CURVE ( 'NONE', #69653, #96102, #75975, .T. ) ;
#86432 = CARTESIAN_POINT ( 'NONE',  ( 12.63842701281683034, 42.46726448433412315, 9.846743663894596210 ) ) ;
#86433 = CARTESIAN_POINT ( 'NONE',  ( 26.00000000000000355, 35.99999999999997158, 7.000000000000000888 ) ) ;
#86434 = CARTESIAN_POINT ( 'NONE',  ( -7.082119434687044190, 12.63708216824730535, 12.26659068614894998 ) ) ;
#86435 = CARTESIAN_POINT ( 'NONE',  ( 0.1532563361054082862, 61.21726448433412315, 2.638427012816831674 ) ) ;
#86436 = CARTESIAN_POINT ( 'NONE',  ( 0.1532563361054083140, 61.00893115100078745, 1.131784320476157264E-15 ) ) ;
#86437 = ORIENTED_EDGE ( 'NONE', *, *, #66614, .F. ) ;
#86438 = CARTESIAN_POINT ( 'NONE',  ( 10.00000000000000000, 30.55374883491397142, -14.16423886937410082 ) ) ;
#86439 = DIRECTION ( 'NONE',  ( 0.000000000000000000, -0.5943319733994194554, 0.8042198116156749066 ) ) ;
#86441 = DIRECTION ( 'NONE',  ( -6.608470384673550777E-17, -1.000000000000000000, 0.000000000000000000 ) ) ;
#86440 = CARTESIAN_POINT ( 'NONE',  ( -5.068142462297546835, -24.94450071861959728, -2.500000000000806022 ) ) ;
#86442 = CARTESIAN_POINT ( 'NONE',  ( 12.91533473730992121, 4.522018677488170546, 10.88017736071110164 ) ) ;
#86443 = CARTESIAN_POINT ( 'NONE',  ( 19.38216949554541557, 22.24863466993041428, -9.382169495545420901 ) ) ;
#86444 = CARTESIAN_POINT ( 'NONE',  ( 20.32896413005680003, 1.771642702460841212, 5.963430220938287007 ) ) ;
#86445 = CARTESIAN_POINT ( 'NONE',  ( 1.472469842513823179, 16.42559781766745175, 4.923371831947296329 ) ) ;
#86446 = CARTESIAN_POINT ( 'NONE',  ( 4.879999999999991900, 76.07179676972444327, -4.250000000000000000 ) ) ;
#86447 = ADVANCED_FACE ( 'NONE', ( #7518 ), #29780, .T. ) ;
#86448 = FACE_OUTER_BOUND ( 'NONE', #5588, .T. ) ;
#86449 = FACE_OUTER_BOUND ( 'NONE', #96986, .T. ) ;
#86450 = CARTESIAN_POINT ( 'NONE',  ( 19.42250999205614193, 15.14701867748817143, 5.440088680355555262 ) ) ;
#86451 = CARTESIAN_POINT ( 'NONE',  ( 32.06412365047463453, 26.99999999999998224, 9.500000000000000000 ) ) ;
#86452 = CARTESIAN_POINT ( 'NONE',  ( -14.43100913236848371, 4.112960668137814512E-16, -1.412789942453356318 ) ) ;
#86453 = CARTESIAN_POINT ( 'NONE',  ( 19.42250999205614548, 30.98035201082150536, -5.440088680355545492 ) ) ;
#86454 = CARTESIAN_POINT ( 'NONE',  ( 19.42250999205614193, 40.14701867748817676, 5.440088680355555262 ) ) ;
#86455 = CARTESIAN_POINT ( 'NONE',  ( 0.1532563361054082862, 66.21726448433413736, 2.638427012816831674 ) ) ;
#86456 = PRESENTATION_STYLE_ASSIGNMENT (( #18941 ) ) ;
#86457 = CARTESIAN_POINT ( 'NONE',  ( -43.18663561153960728, 107.2766636452753062, -4.499999999609646473 ) ) ;
#86458 = CARTESIAN_POINT ( 'NONE',  ( 0.1532563361054083140, 16.00893115100078390, 1.131784320476157264E-15 ) ) ;
#86459 = ORIENTED_EDGE ( 'NONE', *, *, #39203, .F. ) ;
#86460 = AXIS2_PLACEMENT_3D ( 'NONE', #58865, #96398, #59849 ) ;
#86461 = CARTESIAN_POINT ( 'NONE',  ( 20.88017736071110875, 30.77201867748816966, -2.915334737309920765 ) ) ;
#86462 = CARTESIAN_POINT ( 'NONE',  ( 19.38216949554541557, 32.24863466993041783, -9.382169495545420901 ) ) ;
#86463 = DIRECTION ( 'NONE',  ( 0.000000000000000000, 1.000000000000000000, 0.000000000000000000 ) ) ;
#86464 = UNCERTAINTY_MEASURE_WITH_UNIT (LENGTH_MEASURE( 1.000000000000000082E-05 ), #55175, 'distance_accuracy_value', 'NONE');
#86465 = PRESENTATION_LAYER_ASSIGNMENT (  '', '', ( #78456 ) ) ;
#86466 = CARTESIAN_POINT ( 'NONE',  ( 2.791683348922240793, 61.63393115100079456, 7.208316651077764092 ) ) ;
#86467 = CARTESIAN_POINT ( 'NONE',  ( 4.559911319644449179, 67.23035201082150536, -9.422509992056141925 ) ) ;
#86468 = CARTESIAN_POINT ( 'NONE',  ( 19.84674366389459266, 18.30059781766745175, 2.638427012816836559 ) ) ;
#86469 = CARTESIAN_POINT ( 'NONE',  ( 21.09922568453595559, 32.04030133659708923, -6.408140936763230044 ) ) ;
#86471 = CARTESIAN_POINT ( 'NONE',  ( 6.432108699068925795, -88.20011490510430008, -2.750000000000000000 ) ) ;
#86470 = CARTESIAN_POINT ( 'NONE',  ( 10.00000000000000000, 66.81368534415484817, -10.88017736071110342 ) ) ;
#86472 =( BOUNDED_SURFACE ( )  B_SPLINE_SURFACE ( 1, 2, ( 
 ( #81731, #28738, #81248, #59228, #72748, #57262, #13246, #66236, #80762, #82231, #43245, #73741, #58741, #4281, #50246, #5271, #57752, #43738, #89731, #34755, #87757, #96770, #34250, #72267, #28246, #20755, #21249, #51748, #65245, #41794, #19272, #49755, #88254, #19762, #22245, #36750, #44229, #21755, #82728, #44728, #29228, #253, #98760, #59728, #45225, #53708, #15245, #84228, #45724, #75722, #60226, #13746, #74733, #97763, #15736, #14247, #53221, #98261, #75225, #61212, #83723, #52236, #90223, #30210, #76226, #46219, #6246, #67240, #7237, #6737, #22738, #37253, #7739, #38234, #68724, #67742, #29719, #37744, #90720, #52722, #83227, #14752, #60713, #68243, #91210, #91716, #30701, #23236, #96771, #67743, #65744, #97268, #5759, #6247, #74225, #88751, #59230, #29720, #36751, #21756, #28739, #44729, #43246, #66744, #96273, #66237, #36247, #89732, #82232, #67241, #13747, #44230, #90224, #12747, #60227, #90721, #82729, #35248, #50760, #52237, #20756, #22246, #37255, #89246, #81732, #14248, #98263, #43739, #75226, #73742, #27748, #6739, #97765, #51245, #52723, #21250, #51749, #29229, #5272, #13247, #74734, #28247, #12257, #42765, #81249, #58231, #59729, #4775, #73248, #20261, #35749, #58742, #38719, #53222, #77195, #62677, #69218, #30702, #69704, #15737, #37745, #45226, #83724, #15248, #7741, #60714, #16706, #84710, #91211, #744, #32174, #31689, #93177, #62179, #31197, #84229, #14753, #75724, #7239, #9198, #22739, #16213, #68725, #45725, #85201, #8701, #30211, #68244, #92207, #39218, #70199, #39711, #24703, #76227, #47179, #91717, #54680, #46220, #76705, #23238, #77684, #1718, #38235, #1234, #83228, #98761, #254, #61213, #54195, #53710, #8225, #61690, #23732, #46697, #92689, #24214, #56659, #25690, #19155, #3179, #55687, #87147, #49158, #11157, #65129, #10674, #93674, #25208, #79661, #34630, #41189, #2709, #41677, #86674, #9692, #17209, #86186, #17696, #78680, #32672, #87641, #18672, #63166, #71669, #4162, #3674, #95650, #34136, #33645, #56181, #85689, #47686, #78179, #80142, #48167, #72146, #40684, #10191, #57144, #64628, #2213, #40187, #64141, #95137, #42167, #11652, #55174, #71184, #49634, #63655, #26648, #18179, #48659, #94162, #72630, #70694, #33160, #79161, #94658, #26167, #21633, #88133, #97156, #35634, #19646, #81617, #44614, #14129, #27633, #88626, #28624, #96649, #90108, #74109, #58118, #59111, #21133, #82113, #37130, #13126, #65625, #36636, #43623, #59611, #20135, #5643, #12141, #81128, #89126, #20638, #89621, #51634, #13623, #44105, #6130, #50639, #75110, #6616, #97644, #50138, #96150, #67119, #66120, #67625, #52119 ),
 ( #82613, #74616, #12630, #29108, #27134, #42646, #51127, #57638, #80647, #73122, #35126, #4664, #43129, #73621, #5144, #28128, #58628, #36119, #66627, #37621, #60599, #68117, #30092, #22621, #75606, #31571, #634, #7117, #84103, #47067, #46582, #77565, #77080, #46104, #137, #29595, #60097, #22125, #24097, #98643, #31082, #83610, #91094, #1109, #92088, #45099, #83107, #8106, #54081, #85082, #54566, #9081, #53100, #62066, #7629, #69589, #30586, #61091, #38120, #92573, #16590, #15125, #84597, #39595, #98134, #90598, #52606, #69100, #68608, #14636, #53589, #45600, #76098, #91601, #23117, #61577, #15619, #76588, #38601, #23616, #16095, #8591, #39098, #81385, #25577, #9574, #79552, #56069, #3568, #2102, #86564, #55059, #25091, #33050, #63546, #41070, #94542, #71565, #3077, #49048, #70575, #20404, #50891, #41571, #93063, #40074, #11051, #78563, #88895, #96411, #48049, #40574, #72038, #27887, #2596, #34026, #32561, #24594, #64523, #64030, #10073, #12887, #18067, #10559, #87045, #63059, #71071, #94055, #55574, #58374, #70083, #93557, #85577, #48546, #62559, #1607, #79046, #33535, #26060, #56550, #86072, #18556, #32056, #17091, #17584, #47573, #78069, #96912, #5412, #52859, #29362, #75863, #74365, #97904, #28389, #97398, #6371, #36885, #14387, #67878, #44858, #75362, #22384, #43869, #91351, #22878, #14889, #66379, #81873, #83366, #51885, #60852, #68375, #21388, #13889, #45358, #98894, #74871, #7384, #5894, #58882, #37881, #37388, #82366, #83857, #59865, #82873, #60358, #36386, #44373, #67374, #28867, #30345, #53349, #13385, #89384, #90352, #35883, #73882, #21890, #52368, #6877, #98399, #66881, #29855, #43384, #90853, #89874, #20898, #51387, #59370, #76356, #84366, #46350, #38860, #91855, #47813, #16843, #23370, #1370, #63302, #62819, #93811, #93317, #62319, #16350, #45866, #7871, #38366, #40334, #53856, #47317, #873, #15865, #17343, #9332, #61344, #396, #24355, #70340, #2350, #70837, #25341, #76838, #78313, #23864, #85828, #46832, #77324, #54328, #9833, #32806, #8352, #1858, #55825, #15381, #68865, #30846, #85329, #84842, #69349, #69846, #31332, #61832, #92340, #8838, #77817, #39352, #31821, #92826, #54818, #39834, #32314, #24839, #55322, #41814, #25819, #72281, #56316, #95790, #3811, #19776, #18316, #34267, #71323, #41332, #49291, #79792, #57282, #11785, #87776, #19292, #65261, #86812, #35267, #65763, #57770, #10321, #48796, #27271, #94791, #4790, #12277, #64279, #56793, #88275, #42784, #18808, #50264, #79305, #40823, #80780, #80285, #26293, #27767, #64769, #26784, #4301, #10813, #87288, #11294, #71804, #73269, #96290, #3309 ) ),
 .UNSPECIFIED., .F., .F., .F. ) 
 B_SPLINE_SURFACE_WITH_KNOTS ( ( 2, 2 ),
 ( 3, 2, 2, 2, 2, 2, 2, 2, 2, 2, 2, 2, 2, 2, 2, 2, 2, 2, 2, 2, 2, 2, 2, 2, 2, 2, 2, 2, 2, 2, 2, 2, 2, 2, 2, 2, 2, 2, 2, 2, 2, 2, 2, 2, 2, 2, 2, 2, 2, 2, 2, 2, 2, 2, 2, 2, 2, 2, 2, 2, 2, 2, 2, 2, 2, 2, 2, 2, 2, 2, 2, 2, 2, 2, 2, 2, 2, 2, 2, 2, 2, 2, 2, 2, 2, 2, 2, 2, 2, 2, 2, 2, 2, 2, 2, 2, 2, 2, 2, 2, 2, 2, 2, 2, 2, 2, 2, 2, 2, 2, 2, 2, 2, 2, 2, 2, 2, 2, 2, 2, 2, 2, 2, 2, 2, 2, 2, 2, 2, 2, 2, 2, 2, 2, 2, 2, 2, 2, 2, 2, 2, 2, 2, 2, 2, 2, 2, 2, 2, 2, 2, 2, 2, 2, 2, 2, 2, 2, 2, 2, 2, 2, 3 ),
 ( 0.000000000000000000, 1.000000000000000000 ),
 ( 0.000000000000000000, 0.005952380952380952051, 0.01190476190476190410, 0.01785714285714285615, 0.02380952380952380820, 0.02976190476190476025, 0.03571428571428571230, 0.04166666666666666435, 0.04761904761904761640, 0.05357142857142856845, 0.05952380952380952051, 0.06547619047619047949, 0.07142857142857142461, 0.07738095238095238360, 0.08333333333333332871, 0.08928571428571428770, 0.09523809523809523281, 0.1011904761904761918, 0.1071428571428571369, 0.1130952380952380959, 0.1190476190476190410, 0.1250000000000000000, 0.1309523809523809590, 0.1369047619047619180, 0.1428571428571428492, 0.1488095238095238082, 0.1547619047619047672, 0.1607142857142857262, 0.1666666666666666574, 0.1726190476190476164, 0.1785714285714285754, 0.1845238095238095344, 0.1904761904761904656, 0.1964285714285714246, 0.2023809523809523836, 0.2083333333333333426, 0.2142857142857142738, 0.2202380952380952328, 0.2261904761904761918, 0.2321428571428571508, 0.2380952380952380820, 0.2440476190476190410, 0.2500000000000000000, 0.2559523809523809312, 0.2619047619047619180, 0.2678571428571428492, 0.2738095238095238360, 0.2797619047619047672, 0.2857142857142856984, 0.2916666666666666852, 0.2976190476190476164, 0.3035714285714285476, 0.3095238095238095344, 0.3154761904761904656, 0.3214285714285714524, 0.3273809523809523836, 0.3333333333333333148, 0.3392857142857143016, 0.3452380952380952328, 0.3511904761904761640, 0.3571428571428571508, 0.3630952380952380820, 0.3690476190476190688, 0.3750000000000000000, 0.3809523809523809312, 0.3869047619047619180, 0.3928571428571428492, 0.3988095238095238360, 0.4047619047619047672, 0.4107142857142856984, 0.4166666666666666852, 0.4226190476190476164, 0.4285714285714285476, 0.4345238095238095344, 0.4404761904761904656, 0.4464285714285714524, 0.4523809523809523836, 0.4583333333333333148, 0.4642857142857143016, 0.4702380952380952328, 0.4761904761904761640, 0.4821428571428571508, 0.4880952380952380820, 0.4940476190476190688, 0.5000000000000000000, 0.5059523809523809312, 0.5119047619047618625, 0.5178571428571429047, 0.5238095238095238360, 0.5297619047619047672, 0.5357142857142856984, 0.5416666666666666297, 0.5476190476190476719, 0.5535714285714286031, 0.5595238095238095344, 0.5654761904761904656, 0.5714285714285713969, 0.5773809523809523281, 0.5833333333333333703, 0.5892857142857143016, 0.5952380952380952328, 0.6011904761904761640, 0.6071428571428570953, 0.6130952380952381375, 0.6190476190476190688, 0.6250000000000000000, 0.6309523809523809312, 0.6369047619047618625, 0.6428571428571429047, 0.6488095238095238360, 0.6547619047619047672, 0.6607142857142856984, 0.6666666666666666297, 0.6726190476190476719, 0.6785714285714286031, 0.6845238095238095344, 0.6904761904761904656, 0.6964285714285713969, 0.7023809523809523281, 0.7083333333333333703, 0.7142857142857143016, 0.7202380952380952328, 0.7261904761904761640, 0.7321428571428570953, 0.7380952380952381375, 0.7440476190476190688, 0.7500000000000000000, 0.7559523809523809312, 0.7619047619047618625, 0.7678571428571429047, 0.7738095238095238360, 0.7797619047619047672, 0.7857142857142856984, 0.7916666666666666297, 0.7976190476190476719, 0.8035714285714286031, 0.8095238095238095344, 0.8154761904761904656, 0.8214285714285713969, 0.8273809523809523281, 0.8333333333333333703, 0.8392857142857143016, 0.8452380952380952328, 0.8511904761904761640, 0.8571428571428570953, 0.8630952380952381375, 0.8690476190476190688, 0.8750000000000000000, 0.8809523809523809312, 0.8869047619047618625, 0.8928571428571429047, 0.8988095238095238360, 0.9047619047619047672, 0.9107142857142856984, 0.9166666666666666297, 0.9226190476190476719, 0.9285714285714286031, 0.9345238095238095344, 0.9404761904761904656, 0.9464285714285713969, 0.9523809523809523281, 0.9583333333333333703, 0.9642857142857143016 ),
 .UNSPECIFIED. ) 
 GEOMETRIC_REPRESENTATION_ITEM ( )  RATIONAL_B_SPLINE_SURFACE ( (
 ( 1.000000000000000000, 0.9659258262890683122, 1.000000000000000000, 0.9659258262890683122, 1.000000000000000000, 0.9659258262890683122, 1.000000000000000000, 0.9659258262890683122, 1.000000000000000000, 0.9659258262890683122, 1.000000000000000000, 0.9659258262890683122, 1.000000000000000000, 0.9659258262890683122, 1.000000000000000000, 0.9659258262890683122, 1.000000000000000000, 0.9659258262890683122, 1.000000000000000000, 0.9659258262890683122, 1.000000000000000000, 0.9659258262890683122, 1.000000000000000000, 0.9659258262890683122, 1.000000000000000000, 0.9659258262890683122, 1.000000000000000000, 0.9659258262890683122, 1.000000000000000000, 0.9659258262890683122, 1.000000000000000000, 0.9659258262890683122, 1.000000000000000000, 0.9659258262890683122, 1.000000000000000000, 0.9659258262890683122, 1.000000000000000000, 0.9659258262890683122, 1.000000000000000000, 0.9659258262890683122, 1.000000000000000000, 0.9659258262890683122, 1.000000000000000000, 0.9659258262890683122, 1.000000000000000000, 0.9659258262890683122, 1.000000000000000000, 0.9659258262890683122, 1.000000000000000000, 0.9659258262890683122, 1.000000000000000000, 0.9659258262890683122, 1.000000000000000000, 0.9659258262890683122, 1.000000000000000000, 0.9659258262890683122, 1.000000000000000000, 0.9659258262890683122, 1.000000000000000000, 0.9659258262890683122, 1.000000000000000000, 0.9659258262890683122, 1.000000000000000000, 0.9659258262890683122, 1.000000000000000000, 0.9659258262890683122, 1.000000000000000000, 0.9659258262890683122, 1.000000000000000000, 0.9659258262890683122, 1.000000000000000000, 0.9659258262890683122, 1.000000000000000000, 0.9659258262890683122, 1.000000000000000000, 0.9659258262890683122, 1.000000000000000000, 0.9659258262890683122, 1.000000000000000000, 0.9659258262890683122, 1.000000000000000000, 0.9659258262890683122, 1.000000000000000000, 0.9659258262890683122, 1.000000000000000000, 0.9659258262890683122, 1.000000000000000000, 0.9659258262890683122, 1.000000000000000000, 0.9659258262890683122, 1.000000000000000000, 0.9659258262890683122, 1.000000000000000000, 0.9659258262890683122, 1.000000000000000000, 0.9659258262890683122, 1.000000000000000000, 0.9659258262890683122, 1.000000000000000000, 0.9659258262890683122, 1.000000000000000000, 0.9659258262890683122, 1.000000000000000000, 0.9659258262890683122, 1.000000000000000000, 0.9659258262890683122, 1.000000000000000000, 0.9659258262890683122, 1.000000000000000000, 0.9659258262890683122, 1.000000000000000000, 0.9659258262890683122, 1.000000000000000000, 0.9659258262890683122, 1.000000000000000000, 0.9659258262890683122, 1.000000000000000000, 0.9659258262890683122, 1.000000000000000000, 0.9659258262890683122, 1.000000000000000000, 0.9659258262890683122, 1.000000000000000000, 0.9659258262890683122, 1.000000000000000000, 0.9659258262890683122, 1.000000000000000000, 0.9659258262890683122, 1.000000000000000000, 0.9659258262890683122, 1.000000000000000000, 0.9659258262890683122, 1.000000000000000000, 0.9659258262890683122, 1.000000000000000000, 0.9659258262890683122, 1.000000000000000000, 0.9659258262890683122, 1.000000000000000000, 0.9659258262890683122, 1.000000000000000000, 0.9659258262890683122, 1.000000000000000000, 0.9659258262890683122, 1.000000000000000000, 0.9659258262890683122, 1.000000000000000000, 0.9659258262890683122, 1.000000000000000000, 0.9659258262890683122, 1.000000000000000000, 0.9659258262890683122, 1.000000000000000000, 0.9659258262890683122, 1.000000000000000000, 0.9659258262890683122, 1.000000000000000000, 0.9659258262890683122, 1.000000000000000000, 0.9659258262890683122, 1.000000000000000000, 0.9659258262890683122, 1.000000000000000000, 0.9659258262890683122, 1.000000000000000000, 0.9659258262890683122, 1.000000000000000000, 0.9659258262890683122, 1.000000000000000000, 0.9659258262890683122, 1.000000000000000000, 0.9659258262890683122, 1.000000000000000000, 0.9659258262890683122, 1.000000000000000000, 0.9659258262890683122, 1.000000000000000000, 0.9659258262890683122, 1.000000000000000000, 0.9659258262890683122, 1.000000000000000000, 0.9659258262890683122, 1.000000000000000000, 0.9659258262890683122, 1.000000000000000000, 0.9659258262890683122, 1.000000000000000000, 0.9659258262890683122, 1.000000000000000000, 0.9659258262890683122, 1.000000000000000000, 0.9659258262890683122, 1.000000000000000000, 0.9659258262890683122, 1.000000000000000000, 0.9659258262890683122, 1.000000000000000000, 0.9659258262890683122, 1.000000000000000000, 0.9659258262890683122, 1.000000000000000000, 0.9659258262890683122, 1.000000000000000000, 0.9659258262890683122, 1.000000000000000000, 0.9659258262890683122, 1.000000000000000000, 0.9659258262890683122, 1.000000000000000000, 0.9659258262890683122, 1.000000000000000000, 0.9659258262890683122, 1.000000000000000000, 0.9659258262890683122, 1.000000000000000000, 0.9659258262890683122, 1.000000000000000000, 0.9659258262890683122, 1.000000000000000000, 0.9659258262890683122, 1.000000000000000000, 0.9659258262890683122, 1.000000000000000000, 0.9659258262890683122, 1.000000000000000000, 0.9659258262890683122, 1.000000000000000000, 0.9659258262890683122, 1.000000000000000000, 0.9659258262890683122, 1.000000000000000000, 0.9659258262890683122, 1.000000000000000000, 0.9659258262890683122, 1.000000000000000000, 0.9659258262890683122, 1.000000000000000000, 0.9659258262890683122, 1.000000000000000000, 0.9659258262890683122, 1.000000000000000000, 0.9659258262890683122, 1.000000000000000000, 0.9659258262890683122, 1.000000000000000000, 0.9659258262890683122, 1.000000000000000000, 0.9659258262890683122, 1.000000000000000000, 0.9659258262890683122, 1.000000000000000000, 0.9659258262890683122, 1.000000000000000000, 0.9659258262890683122, 1.000000000000000000, 0.9659258262890683122, 1.000000000000000000, 0.9659258262890683122, 1.000000000000000000, 0.9659258262890683122, 1.000000000000000000, 0.9659258262890683122, 1.000000000000000000, 0.9659258262890683122, 1.000000000000000000, 0.9659258262890683122, 1.000000000000000000, 0.9659258262890683122, 1.000000000000000000, 0.9659258262890683122, 1.000000000000000000, 0.9659258262890683122, 1.000000000000000000, 0.9659258262890683122, 1.000000000000000000, 0.9659258262890683122, 1.000000000000000000, 0.9659258262890683122, 1.000000000000000000, 0.9659258262890683122, 1.000000000000000000, 0.9659258262890683122, 1.000000000000000000, 0.9659258262890683122, 1.000000000000000000, 0.9659258262890683122, 1.000000000000000000, 0.9659258262890683122, 1.000000000000000000, 0.9659258262890683122, 1.000000000000000000, 0.9659258262890683122, 1.000000000000000000, 0.9659258262890683122, 1.000000000000000000, 0.9659258262890683122, 1.000000000000000000, 0.9659258262890683122, 1.000000000000000000, 0.9659258262890683122, 1.000000000000000000, 0.9659258262890683122, 1.000000000000000000, 0.9659258262890683122, 1.000000000000000000, 0.9659258262890683122, 1.000000000000000000, 0.9659258262890683122, 1.000000000000000000, 0.9659258262890683122, 1.000000000000000000, 0.9659258262890683122, 1.000000000000000000, 0.9659258262890683122, 1.000000000000000000, 0.9659258262890683122, 1.000000000000000000, 0.9659258262890683122, 1.000000000000000000, 0.9659258262890683122, 1.000000000000000000, 0.9659258262890683122, 1.000000000000000000, 0.9659258262890683122, 1.000000000000000000),
 ( 1.000000000000000000, 0.9659258262890683122, 1.000000000000000000, 0.9659258262890683122, 1.000000000000000000, 0.9659258262890683122, 1.000000000000000000, 0.9659258262890683122, 1.000000000000000000, 0.9659258262890683122, 1.000000000000000000, 0.9659258262890683122, 1.000000000000000000, 0.9659258262890683122, 1.000000000000000000, 0.9659258262890683122, 1.000000000000000000, 0.9659258262890683122, 1.000000000000000000, 0.9659258262890683122, 1.000000000000000000, 0.9659258262890683122, 1.000000000000000000, 0.9659258262890683122, 1.000000000000000000, 0.9659258262890683122, 1.000000000000000000, 0.9659258262890683122, 1.000000000000000000, 0.9659258262890683122, 1.000000000000000000, 0.9659258262890683122, 1.000000000000000000, 0.9659258262890683122, 1.000000000000000000, 0.9659258262890683122, 1.000000000000000000, 0.9659258262890683122, 1.000000000000000000, 0.9659258262890683122, 1.000000000000000000, 0.9659258262890683122, 1.000000000000000000, 0.9659258262890683122, 1.000000000000000000, 0.9659258262890683122, 1.000000000000000000, 0.9659258262890683122, 1.000000000000000000, 0.9659258262890683122, 1.000000000000000000, 0.9659258262890683122, 1.000000000000000000, 0.9659258262890683122, 1.000000000000000000, 0.9659258262890683122, 1.000000000000000000, 0.9659258262890683122, 1.000000000000000000, 0.9659258262890683122, 1.000000000000000000, 0.9659258262890683122, 1.000000000000000000, 0.9659258262890683122, 1.000000000000000000, 0.9659258262890683122, 1.000000000000000000, 0.9659258262890683122, 1.000000000000000000, 0.9659258262890683122, 1.000000000000000000, 0.9659258262890683122, 1.000000000000000000, 0.9659258262890683122, 1.000000000000000000, 0.9659258262890683122, 1.000000000000000000, 0.9659258262890683122, 1.000000000000000000, 0.9659258262890683122, 1.000000000000000000, 0.9659258262890683122, 1.000000000000000000, 0.9659258262890683122, 1.000000000000000000, 0.9659258262890683122, 1.000000000000000000, 0.9659258262890683122, 1.000000000000000000, 0.9659258262890683122, 1.000000000000000000, 0.9659258262890683122, 1.000000000000000000, 0.9659258262890683122, 1.000000000000000000, 0.9659258262890683122, 1.000000000000000000, 0.9659258262890683122, 1.000000000000000000, 0.9659258262890683122, 1.000000000000000000, 0.9659258262890683122, 1.000000000000000000, 0.9659258262890683122, 1.000000000000000000, 0.9659258262890683122, 1.000000000000000000, 0.9659258262890683122, 1.000000000000000000, 0.9659258262890683122, 1.000000000000000000, 0.9659258262890683122, 1.000000000000000000, 0.9659258262890683122, 1.000000000000000000, 0.9659258262890683122, 1.000000000000000000, 0.9659258262890683122, 1.000000000000000000, 0.9659258262890683122, 1.000000000000000000, 0.9659258262890683122, 1.000000000000000000, 0.9659258262890683122, 1.000000000000000000, 0.9659258262890683122, 1.000000000000000000, 0.9659258262890683122, 1.000000000000000000, 0.9659258262890683122, 1.000000000000000000, 0.9659258262890683122, 1.000000000000000000, 0.9659258262890683122, 1.000000000000000000, 0.9659258262890683122, 1.000000000000000000, 0.9659258262890683122, 1.000000000000000000, 0.9659258262890683122, 1.000000000000000000, 0.9659258262890683122, 1.000000000000000000, 0.9659258262890683122, 1.000000000000000000, 0.9659258262890683122, 1.000000000000000000, 0.9659258262890683122, 1.000000000000000000, 0.9659258262890683122, 1.000000000000000000, 0.9659258262890683122, 1.000000000000000000, 0.9659258262890683122, 1.000000000000000000, 0.9659258262890683122, 1.000000000000000000, 0.9659258262890683122, 1.000000000000000000, 0.9659258262890683122, 1.000000000000000000, 0.9659258262890683122, 1.000000000000000000, 0.9659258262890683122, 1.000000000000000000, 0.9659258262890683122, 1.000000000000000000, 0.9659258262890683122, 1.000000000000000000, 0.9659258262890683122, 1.000000000000000000, 0.9659258262890683122, 1.000000000000000000, 0.9659258262890683122, 1.000000000000000000, 0.9659258262890683122, 1.000000000000000000, 0.9659258262890683122, 1.000000000000000000, 0.9659258262890683122, 1.000000000000000000, 0.9659258262890683122, 1.000000000000000000, 0.9659258262890683122, 1.000000000000000000, 0.9659258262890683122, 1.000000000000000000, 0.9659258262890683122, 1.000000000000000000, 0.9659258262890683122, 1.000000000000000000, 0.9659258262890683122, 1.000000000000000000, 0.9659258262890683122, 1.000000000000000000, 0.9659258262890683122, 1.000000000000000000, 0.9659258262890683122, 1.000000000000000000, 0.9659258262890683122, 1.000000000000000000, 0.9659258262890683122, 1.000000000000000000, 0.9659258262890683122, 1.000000000000000000, 0.9659258262890683122, 1.000000000000000000, 0.9659258262890683122, 1.000000000000000000, 0.9659258262890683122, 1.000000000000000000, 0.9659258262890683122, 1.000000000000000000, 0.9659258262890683122, 1.000000000000000000, 0.9659258262890683122, 1.000000000000000000, 0.9659258262890683122, 1.000000000000000000, 0.9659258262890683122, 1.000000000000000000, 0.9659258262890683122, 1.000000000000000000, 0.9659258262890683122, 1.000000000000000000, 0.9659258262890683122, 1.000000000000000000, 0.9659258262890683122, 1.000000000000000000, 0.9659258262890683122, 1.000000000000000000, 0.9659258262890683122, 1.000000000000000000, 0.9659258262890683122, 1.000000000000000000, 0.9659258262890683122, 1.000000000000000000, 0.9659258262890683122, 1.000000000000000000, 0.9659258262890683122, 1.000000000000000000, 0.9659258262890683122, 1.000000000000000000, 0.9659258262890683122, 1.000000000000000000, 0.9659258262890683122, 1.000000000000000000, 0.9659258262890683122, 1.000000000000000000, 0.9659258262890683122, 1.000000000000000000, 0.9659258262890683122, 1.000000000000000000, 0.9659258262890683122, 1.000000000000000000, 0.9659258262890683122, 1.000000000000000000, 0.9659258262890683122, 1.000000000000000000, 0.9659258262890683122, 1.000000000000000000, 0.9659258262890683122, 1.000000000000000000, 0.9659258262890683122, 1.000000000000000000, 0.9659258262890683122, 1.000000000000000000, 0.9659258262890683122, 1.000000000000000000, 0.9659258262890683122, 1.000000000000000000, 0.9659258262890683122, 1.000000000000000000, 0.9659258262890683122, 1.000000000000000000, 0.9659258262890683122, 1.000000000000000000, 0.9659258262890683122, 1.000000000000000000, 0.9659258262890683122, 1.000000000000000000, 0.9659258262890683122, 1.000000000000000000, 0.9659258262890683122, 1.000000000000000000, 0.9659258262890683122, 1.000000000000000000, 0.9659258262890683122, 1.000000000000000000, 0.9659258262890683122, 1.000000000000000000, 0.9659258262890683122, 1.000000000000000000, 0.9659258262890683122, 1.000000000000000000, 0.9659258262890683122, 1.000000000000000000, 0.9659258262890683122, 1.000000000000000000, 0.9659258262890683122, 1.000000000000000000, 0.9659258262890683122, 1.000000000000000000, 0.9659258262890683122, 1.000000000000000000, 0.9659258262890683122, 1.000000000000000000, 0.9659258262890683122, 1.000000000000000000, 0.9659258262890683122, 1.000000000000000000, 0.9659258262890683122, 1.000000000000000000, 0.9659258262890683122, 1.000000000000000000, 0.9659258262890683122, 1.000000000000000000, 0.9659258262890683122, 1.000000000000000000, 0.9659258262890683122, 1.000000000000000000, 0.9659258262890683122, 1.000000000000000000, 0.9659258262890683122, 1.000000000000000000) ) ) 
 REPRESENTATION_ITEM ( '' )  SURFACE ( )  );
#86473 = ORIENTED_EDGE ( 'NONE', *, *, #14994, .T. ) ;
#86474 = CARTESIAN_POINT ( 'NONE',  ( 0.000000000000000000, 0.5000000000000004441, 0.000000000000000000 ) ) ;
#86475 = DIRECTION ( 'NONE',  ( -4.336808689942013792E-16, 1.000000000000000000, 0.000000000000000000 ) ) ;
#86477 = CARTESIAN_POINT ( 'NONE',  ( 2.917880565312950480, 25.97041550158063572, -12.26659068614894821 ) ) ;
#86476 = CARTESIAN_POINT ( 'NONE',  ( -2.816281873526471635, 58.91530133659707502, -3.434112377981056508 ) ) ;
#86478 = CARTESIAN_POINT ( 'NONE',  ( 17.20831665107776587, 22.88393115100078745, 7.208316651077764980 ) ) ;
#86479 = EDGE_CURVE ( 'NONE', #28504, #87109, #41480, .T. ) ;
#86480 = CARTESIAN_POINT ( 'NONE',  ( 17.96484262340118221, 6.188685344154836621, -7.964842623401177768 ) ) ;
#86481 = CARTESIAN_POINT ( 'NONE',  ( 17.20831665107776587, 19.13393115100078035, -7.208316651077762316 ) ) ;
#86482 = CARTESIAN_POINT ( 'NONE',  ( -2.266590686148945544, 52.22041550158064638, 7.082119434687048631 ) ) ;
#86483 = ORIENTED_EDGE ( 'NONE', *, *, #69317, .F. ) ;
#86484 = DIRECTION ( 'NONE',  ( -0.000000000000000000, 1.000000000000000000, 0.000000000000000000 ) ) ;
#86485 = ADVANCED_FACE ( 'NONE', ( #72428 ), #71946, .T. ) ;
#86486 = CARTESIAN_POINT ( 'NONE',  ( 7.084665262690076126, 27.02201867748817676, -10.88017736071110164 ) ) ;
#86487 = CARTESIAN_POINT ( 'NONE',  ( 20.03743638938528449, 46.75197528031019090, 6.399506433553902696 ) ) ;
#86488 = CIRCLE ( 'NONE', #40225, 0.5000000000000073275 ) ;
#86489 = VERTEX_POINT ( 'NONE', #7416 ) ;
#86490 = CARTESIAN_POINT ( 'NONE',  ( 0.5774900079438607392, 28.48035201082150891, 5.440088680355550821 ) ) ;
#86491 = CARTESIAN_POINT ( 'NONE',  ( 17.20831665107776587, 59.13393115100078745, -7.208316651077762316 ) ) ;
#86492 = CARTESIAN_POINT ( 'NONE',  ( 16.40814093676324603, 52.45696800326375353, -11.09922568453594671 ) ) ;
#86493 = CARTESIAN_POINT ( 'NONE',  ( 13.50249619331273720, -1.423015351387222844E-16, 5.623250243473579602 ) ) ;
#86494 = CARTESIAN_POINT ( 'NONE',  ( 10.00000000000000000, 20.55374883491396787, -14.16423886937410082 ) ) ;
#86495 = CARTESIAN_POINT ( 'NONE',  ( 15.44008868035555260, 39.73035201082150536, 9.422509992056143702 ) ) ;
#86496 = CARTESIAN_POINT ( 'NONE',  ( 20.88017736071110875, 10.77201867748817143, -2.915334737309920765 ) ) ;
#86497 = EDGE_CURVE ( 'NONE', #39436, #37440, #90883, .T. ) ;
#86498 = ADVANCED_FACE ( 'NONE', ( #74398 ), #5921, .T. ) ;
#86499 = CARTESIAN_POINT ( 'NONE',  ( 14.92337183194729633, 57.67559781766745886, 8.527530157486181039 ) ) ;
#86500 =( NAMED_UNIT ( * ) SI_UNIT ( $, .STERADIAN. ) SOLID_ANGLE_UNIT ( ) );
#86501 = CARTESIAN_POINT ( 'NONE',  ( 5.076628168052704559, 30.17559781766745175, -8.527530157486179263 ) ) ;
#86502 = AXIS2_PLACEMENT_3D ( 'NONE', #21037, #7022, #51527 ) ;
#86503 = DIRECTION ( 'NONE',  ( -1.000000000000000000, 0.000000000000000000, 0.000000000000000000 ) ) ;
#86504 = CARTESIAN_POINT ( 'NONE',  ( 18.52753015748617571, 8.092264484334117824, 4.923371831947298993 ) ) ;
#86505 = CARTESIAN_POINT ( 'NONE',  ( 6.408140936763236262, -32.54303199673623936, -11.09922568453595026 ) ) ;
#86506 = ORIENTED_EDGE ( 'NONE', *, *, #39553, .T. ) ;
#86507 = CARTESIAN_POINT ( 'NONE',  ( 19.42250999205614193, 5.147018677488171434, 5.440088680355555262 ) ) ;
#86508 = CARTESIAN_POINT ( 'NONE',  ( 12.63842701281683922, 14.55059781766744997, -9.846743663894590881 ) ) ;
#86509 = EDGE_CURVE ( 'NONE', #26347, #81670, #59398, .T. ) ;
#86510 = CARTESIAN_POINT ( 'NONE',  ( 18.52753015748618282, 63.92559781766745886, -4.923371831947291888 ) ) ;
#86511 = CARTESIAN_POINT ( 'NONE',  ( 10.00000000000000178, 44.31368534415484106, 10.88017736071110342 ) ) ;
#86513 = CARTESIAN_POINT ( 'NONE',  ( 6.565887622018943937, 45.16530133659708923, 12.81628187352647430 ) ) ;
#86512 = CARTESIAN_POINT ( 'NONE',  ( 17.96484262340118221, 14.93868534415483751, 7.964842623401181321 ) ) ;
#86514 = CARTESIAN_POINT ( 'NONE',  ( -0.3689425029237898834, 36.17874883491396787, -10.36894250292378850 ) ) ;
#86515 = CARTESIAN_POINT ( 'NONE',  ( 3.591859063236761518, 54.95696800326376064, 11.09922568453594849 ) ) ;
#86516 = ORIENTED_EDGE ( 'NONE', *, *, #54745, .T. ) ;
#86517 = CARTESIAN_POINT ( 'NONE',  ( 5.076628168052703671, 56.84226448433412315, 8.527530157486179263 ) ) ;
#86518 = CARTESIAN_POINT ( 'NONE',  ( 4.559911319644449179, 28.89701867748817321, 9.422509992056141925 ) ) ;
#86519 = EDGE_CURVE ( 'NONE', #96104, #94230, #97427, .T. ) ;
#86520 = VERTEX_POINT ( 'NONE', #89901 ) ;
#86521 = CARTESIAN_POINT ( 'NONE',  ( 0.1532563361054083140, 1.008931151000784787, 1.131784320476157264E-15 ) ) ;
#86522 = CARTESIAN_POINT ( 'NONE',  ( 10.00000000000000178, 7.258931151000785675, 9.846743663894594434 ) ) ;
#86523 = CARTESIAN_POINT ( 'NONE',  ( 19.84674366389459266, 3.717264484334118713, -2.638427012816827677 ) ) ;
#86525 = DIRECTION ( 'NONE',  ( 0.000000000000000000, 0.000000000000000000, 1.000000000000000000 ) ) ;
#86524 = CARTESIAN_POINT ( 'NONE',  ( -0.8801773607110991993, 57.85535201082149825, -2.915334737309923874 ) ) ;
#86526 = CARTESIAN_POINT ( 'NONE',  ( -0.8801773607111009756, 58.06368534415484106, 1.068504757029289695E-15 ) ) ;
#86528 = ORIENTED_EDGE ( 'NONE', *, *, #11878, .F. ) ;
#86527 = CARTESIAN_POINT ( 'NONE',  ( 2.791683348922237240, 10.38393115100078390, -7.208316651077763204 ) ) ;
#86529 = VECTOR ( 'NONE', #61024, 1000.000000000000000 ) ;
#86530 = LINE ( 'NONE', #18030, #61336 ) ;
#86531 = CARTESIAN_POINT ( 'NONE',  ( 0.1532563361054082862, 56.21726448433411605, 2.638427012816831674 ) ) ;
#86532 = VERTEX_POINT ( 'NONE', #20431 ) ;
#86533 = FACE_OUTER_BOUND ( 'NONE', #97974, .T. ) ;
#86534 = CARTESIAN_POINT ( 'NONE',  ( -2.816281873526473856, 64.12363466993042493, 9.499525473075851096E-16 ) ) ;
#86535 = CARTESIAN_POINT ( 'NONE',  ( 13.79529636645030344, 3.262082168247301350, 14.16423886937410614 ) ) ;
#86536 = CARTESIAN_POINT ( 'NONE',  ( 24.16423886937409904, 29.09541550158063572, 3.795296366450317205 ) ) ;
#86537 = DIRECTION ( 'NONE',  ( 0.7489557207889945278, 0.000000000000000000, 0.6626200482157461602 ) ) ;
#86538 = CARTESIAN_POINT ( 'NONE',  ( 15.44008868035555793, 26.39701867748817321, -9.422509992056140149 ) ) ;
#86539 = SURFACE_SIDE_STYLE ('',( #18529 ) ) ;
#86540 = ORIENTED_EDGE ( 'NONE', *, *, #73494, .T. ) ;
#86541 = CARTESIAN_POINT ( 'NONE',  ( 5.076628168052703671, 11.84226448433411960, 8.527530157486179263 ) ) ;
#86542 = CARTESIAN_POINT ( 'NONE',  ( 3.591859063236761518, 44.95696800326376064, 11.09922568453594849 ) ) ;
#86543 = CARTESIAN_POINT ( 'NONE',  ( 1.472469842513823179, 36.42559781766745175, 4.923371831947296329 ) ) ;
#86544 = CARTESIAN_POINT ( 'NONE',  ( -0.03447792253739276336, 25.15514106990690379, 6.401564815979735812 ) ) ;
#86545 = ADVANCED_FACE ( 'NONE', ( #52886 ), #50918, .F. ) ;
#86546 = CARTESIAN_POINT ( 'NONE',  ( 2.791683348922240793, 21.63393115100078745, 7.208316651077764092 ) ) ;
#86547 = CARTESIAN_POINT ( 'NONE',  ( -1.099225684535947600, 34.54030133659708923, 6.408140936763237150 ) ) ;
#86548 = CARTESIAN_POINT ( 'NONE',  ( 14.16423886937410437, -30.90458449841936073, 3.795296366450304770 ) ) ;
#86549 = TOROIDAL_SURFACE ( 'NONE', #5104, 0.5000000000000043299, 0.5000000000000000000 ) ;
#86550 = CARTESIAN_POINT ( 'NONE',  ( 2.791683348922237240, 25.38393115100078390, -7.208316651077763204 ) ) ;
#86551 = PRESENTATION_LAYER_ASSIGNMENT (  '', '', ( #3484 ) ) ;
#86552 = CARTESIAN_POINT ( 'NONE',  ( -2.266590686148945544, 7.220415501580634832, 7.082119434687048631 ) ) ;
#86553 = ORIENTED_EDGE ( 'NONE', *, *, #83094, .F. ) ;
#86554 = CARTESIAN_POINT ( 'NONE',  ( 17.96484262340118221, 34.93868534415482685, 7.964842623401181321 ) ) ;
#86555 = CARTESIAN_POINT ( 'NONE',  ( 22.26659068614894466, 28.88708216824730357, 7.082119434687054849 ) ) ;
#86556 = CARTESIAN_POINT ( 'NONE',  ( 19.84674366389459621, 48.50893115100078745, 7.409399052514197653E-17 ) ) ;
#86557 = CARTESIAN_POINT ( 'NONE',  ( 7.361572987183170547, 7.050597817667451750, 9.846743663894590881 ) ) ;
#86558 = VECTOR ( 'NONE', #27824, 1000.000000000000000 ) ;
#86560 = DIRECTION ( 'NONE',  ( 2.569960705150826877E-16, -1.000000000000000000, 0.000000000000000000 ) ) ;
#86559 = CARTESIAN_POINT ( 'NONE',  ( 0.6178305044545838731, 49.74863466993041072, 9.382169495545420901 ) ) ;
#86561 = CARTESIAN_POINT ( 'NONE',  ( -0.8801773607111008646, 28.27201867748817321, 2.915334737309923430 ) ) ;
#86562 = CIRCLE ( 'NONE', #6763, 0.2500000000000002220 ) ;
#86563 = DIRECTION ( 'NONE',  ( 0.000000000000000000, 1.000000000000000000, 0.000000000000000000 ) ) ;
#86564 = CARTESIAN_POINT ( 'NONE',  ( 22.81628187352647785, 16.62363466993042138, 6.195893100308588602E-16 ) ) ;
#86565 = CARTESIAN_POINT ( 'NONE',  ( 14.92337183194729988, 44.34226448433412315, -8.527530157486177487 ) ) ;
#86566 = CARTESIAN_POINT ( 'NONE',  ( -5.204170427930421283E-15, 1.813685344154845946, -10.88017736071110342 ) ) ;
#86567 = CARTESIAN_POINT ( 'NONE',  ( 3.822225673302248605, 0.000000000000000000, 3.889525102760262865 ) ) ;
#86568 = MECHANICAL_DESIGN_GEOMETRIC_PRESENTATION_REPRESENTATION (  '', ( #24273 ), #81765 ) ;
#86570 = LINE ( 'NONE', #56556, #62163 ) ;
#86569 = CARTESIAN_POINT ( 'NONE',  ( -11.48952521350012113, 4.018634162980579609E-16, -8.845383562533903898 ) ) ;
#86571 = CARTESIAN_POINT ( 'NONE',  ( -9.823916613421536326, -32.16564667764521346, 4.000000000000000888 ) ) ;
#86572 = CARTESIAN_POINT ( 'NONE',  ( -0.8801773607111009756, 58.06368534415484106, 1.068504757029289695E-15 ) ) ;
#86573 = CARTESIAN_POINT ( 'NONE',  ( -0.8801773607111009756, 58.06368534415484106, 1.068504757029289695E-15 ) ) ;
#86574 = CARTESIAN_POINT ( 'NONE',  ( 20.10384461210892226, 56.74302437010793199, 6.337995344473749348 ) ) ;
#86575 = CARTESIAN_POINT ( 'NONE',  ( 3.195792623639533758, 11.14664270246084499, 11.92686044187656158 ) ) ;
#86576 = CARTESIAN_POINT ( 'NONE',  ( 12.91533473730992121, 9.522018677488171434, 10.88017736071110164 ) ) ;
#86577 = CARTESIAN_POINT ( 'NONE',  ( 1.472469842513823179, 66.42559781766745175, 4.923371831947296329 ) ) ;
#86579 = CARTESIAN_POINT ( 'NONE',  ( -6.982525766850296911, -88.11956318484570261, -3.750000000000000000 ) ) ;
#86578 = CARTESIAN_POINT ( 'NONE',  ( 0.5774900079438590739, 27.64701867748817676, -5.440088680355550821 ) ) ;
#86580 = CARTESIAN_POINT ( 'NONE',  ( -2.816281873526471635, 18.91530133659708213, -3.434112377981056508 ) ) ;
#86581 = ORIENTED_EDGE ( 'NONE', *, *, #68078, .F. ) ;
#86582 = CARTESIAN_POINT ( 'NONE',  ( 15.44008868035555793, 56.39701867748817676, -9.422509992056140149 ) ) ;
#86583 = CARTESIAN_POINT ( 'NONE',  ( 14.92337183194729988, 34.34226448433411605, -8.527530157486177487 ) ) ;
#86585 = CARTESIAN_POINT ( 'NONE',  ( 0.000000000000000000, 70.00000000000000000, 6.500000000000000888 ) ) ;
#86584 = CARTESIAN_POINT ( 'NONE',  ( 16.40814093676323893, 0.7903013365970867898, 11.09922568453595026 ) ) ;
#86586 = CARTESIAN_POINT ( 'NONE',  ( 7.084665262690076126, 27.02201867748817676, -10.88017736071110164 ) ) ;
#86587 = CARTESIAN_POINT ( 'NONE',  ( 15.44008868035555793, 41.39701867748817676, -9.422509992056140149 ) ) ;
#86588 = CARTESIAN_POINT ( 'NONE',  ( -2.266590686148945544, 47.22041550158063927, 7.082119434687048631 ) ) ;
#86589 = CARTESIAN_POINT ( 'NONE',  ( 1.472469842513823179, 36.42559781766745175, 4.923371831947296329 ) ) ;
#86590 = CARTESIAN_POINT ( 'NONE',  ( 10.00000000000000000, 56.81368534415484106, -10.88017736071110342 ) ) ;
#86591 = CARTESIAN_POINT ( 'NONE',  ( 7.084665262690076126, 44.10535201082151247, 10.88017736071109987 ) ) ;
#86592 = DIRECTION ( 'NONE',  ( 0.000000000000000000, -1.000000000000000000, 0.000000000000000000 ) ) ;
#86593 = CARTESIAN_POINT ( 'NONE',  ( 13.79529636645030344, 18.26208216824730002, 14.16423886937410614 ) ) ;
#86594 = EDGE_CURVE ( 'NONE', #4978, #95793, #81414, .T. ) ;
#86595 = CARTESIAN_POINT ( 'NONE',  ( -16.94000000000001549, 92.00000000000000000, -9.500000000000000000 ) ) ;
#86596 = CARTESIAN_POINT ( 'NONE',  ( 20.15039907845753930, 70.00000000000000000, 6.262539305110068177 ) ) ;
#86598 = VERTEX_POINT ( 'NONE', #60385 ) ;
#86597 = EDGE_CURVE ( 'NONE', #87349, #74857, #16958, .T. ) ;
#86599 = AXIS2_PLACEMENT_3D ( 'NONE', #33840, #10387, #9901 ) ;
#86600 = CARTESIAN_POINT ( 'NONE',  ( -2.266590686148945544, 46.38708216824730357, -7.082119434687050408 ) ) ;
#86601 = CARTESIAN_POINT ( 'NONE',  ( 22.26659068614895176, 34.72041550158063927, -7.082119434687042414 ) ) ;
#86602 = CARTESIAN_POINT ( 'NONE',  ( 5.076628168052703671, 16.84226448433411960, 8.527530157486179263 ) ) ;
#86603 = PLANE ( 'NONE',  #92243 ) ;
#86604 = DIRECTION ( 'NONE',  ( -0.000000000000000000, -0.000000000000000000, -1.000000000000000000 ) ) ;
#86606 = CARTESIAN_POINT ( 'NONE',  ( 22.81628187352647785, 31.41530133659709279, 3.434112377981063169 ) ) ;
#86605 = CARTESIAN_POINT ( 'NONE',  ( 10.00000000000000000, 66.81368534415484817, -10.88017736071110342 ) ) ;
#86607 = CARTESIAN_POINT ( 'NONE',  ( 17.08211943468705840, 50.13708216824730357, -12.26659068614894466 ) ) ;
#86608 = ADVANCED_FACE ( 'NONE', ( #43413 ), #40019, .T. ) ;
#86609 = ADVANCED_FACE ( 'NONE', ( #811 ), #95159, .T. ) ;
#86610 = DIRECTION ( 'NONE',  ( 0.000000000000000000, 0.000000000000000000, -1.000000000000000000 ) ) ;
#86611 = CARTESIAN_POINT ( 'NONE',  ( 4.559911319644449179, 67.23035201082150536, -9.422509992056141925 ) ) ;
#86612 = CARTESIAN_POINT ( 'NONE',  ( -2.638427012816840111, -10.03273551566587507, -9.846743663894590881 ) ) ;
#86613 = CARTESIAN_POINT ( 'NONE',  ( 2.791683348922237240, 5.383931151000785675, -7.208316651077763204 ) ) ;
#86614 = VERTEX_POINT ( 'NONE', #45799 ) ;
#86615 = CARTESIAN_POINT ( 'NONE',  ( 7.361572987183170547, 22.05059781766745530, 9.846743663894590881 ) ) ;
#86616 = CYLINDRICAL_SURFACE ( 'NONE', #26942, 15.00000000000000000 ) ;
#86617 = EDGE_LOOP ( 'NONE', ( #26205, #15785, #48015, #76741 ) ) ;
#86618 = CARTESIAN_POINT ( 'NONE',  ( 24.16423886937410614, 4.303748834913967869, 8.672049930838204340E-16 ) ) ;
#86620 = CARTESIAN_POINT ( 'NONE',  ( 7.084665262690076126, 12.02201867748817321, -10.88017736071110164 ) ) ;
#86619 = CARTESIAN_POINT ( 'NONE',  ( -2.266590686148945544, 67.22041550158063217, 7.082119434687048631 ) ) ;
#86622 = CARTESIAN_POINT ( 'NONE',  ( -2.816281873526471635, 3.915301336597087456, -3.434112377981056508 ) ) ;
#86621 = CARTESIAN_POINT ( 'NONE',  ( 18.52753015748618282, 33.92559781766745886, -4.923371831947291888 ) ) ;
#86623 = DIRECTION ( 'NONE',  ( 0.000000000000000000, 0.000000000000000000, -1.000000000000000000 ) ) ;
#86624 = CARTESIAN_POINT ( 'NONE',  ( 3.591859063236761518, 14.95696800326375531, 11.09922568453594849 ) ) ;
#86625 = CARTESIAN_POINT ( 'NONE',  ( -9.382169495545413795, 29.74863466993043559, 9.382169495545428006 ) ) ;
#86626 = ORIENTED_EDGE ( 'NONE', *, *, #73948, .F. ) ;
#86627 = STYLED_ITEM ( 'NONE', ( #38097 ), #48292 ) ;
#86628 = CARTESIAN_POINT ( 'NONE',  ( 13.79529636645030344, 53.26208216824730357, 14.16423886937410614 ) ) ;
#86629 = VERTEX_POINT ( 'NONE', #7804 ) ;
#86630 = ADVANCED_FACE ( 'NONE', ( #45296 ), #61276, .T. ) ;
#86631 = VECTOR ( 'NONE', #73374, 1000.000000000000000 ) ;
#86632 = CARTESIAN_POINT ( 'NONE',  ( 20.36894250292379738, 59.92874883491397497, -10.36894250292379027 ) ) ;
#86633 = ORIENTED_EDGE ( 'NONE', *, *, #52829, .T. ) ;
#86634 = CARTESIAN_POINT ( 'NONE',  ( 20.88017736071110519, 35.56368534415484106, 2.639326808657452039E-16 ) ) ;
#86635 = CARTESIAN_POINT ( 'NONE',  ( 2.035157376598824452, 33.68868534415484106, 7.964842623401179544 ) ) ;
#86636 = CIRCLE ( 'NONE', #38752, 7.000000000000000000 ) ;
#86637 = LINE ( 'NONE', #18146, #88857 ) ;
#86638 = CARTESIAN_POINT ( 'NONE',  ( 17.96484262340118221, 31.18868534415483751, -7.964842623401177768 ) ) ;
#86639 =( GEOMETRIC_REPRESENTATION_CONTEXT ( 3 ) GLOBAL_UNCERTAINTY_ASSIGNED_CONTEXT ( ( #84140 ) ) GLOBAL_UNIT_ASSIGNED_CONTEXT ( ( #21266, #68259, #44250 ) ) REPRESENTATION_CONTEXT ( 'NONE', 'WORKASPACE' ) );
#86640 = CARTESIAN_POINT ( 'NONE',  ( -0.1042174387088606879, 33.10736173766203905, 6.337391062633419558 ) ) ;
#86641 = CARTESIAN_POINT ( 'NONE',  ( 12.63842701281683922, 19.55059781766745175, -9.846743663894590881 ) ) ;
#86642 = CARTESIAN_POINT ( 'NONE',  ( -3.585386599742081071, -2.690194976740612809, 2.750000000000202061 ) ) ;
#86643 = ORIENTED_EDGE ( 'NONE', *, *, #93876, .F. ) ;
#86644 = CARTESIAN_POINT ( 'NONE',  ( 10.72176212046095145, -40.27637155869545893, 3.750000000000000000 ) ) ;
#86645 = CARTESIAN_POINT ( 'NONE',  ( 2.791683348922237240, 50.38393115100078035, -7.208316651077763204 ) ) ;
#86646 = EDGE_CURVE ( 'NONE', #63634, #54365, #44460, .T. ) ;
#86647 = DIRECTION ( 'NONE',  ( -4.352074256530613638E-14, 0.000000000000000000, 1.000000000000000000 ) ) ;
#86648 = AXIS2_PLACEMENT_3D ( 'NONE', #80558, #12547, #90017 ) ;
#86649 = CARTESIAN_POINT ( 'NONE',  ( -4.000000000000000000, 37.00000000000000000, 2.500000000000000000 ) ) ;
#86650 = LINE ( 'NONE', #33617, #28444 ) ;
#86651 = DIRECTION ( 'NONE',  ( 0.000000000000000000, 0.000000000000000000, 1.000000000000000000 ) ) ;
#86652 = DIRECTION ( 'NONE',  ( -1.000000000000000000, -1.483861936729427615E-16, 0.000000000000000000 ) ) ;
#86653 = CARTESIAN_POINT ( 'NONE',  ( 6.204703633549690345, 45.76208216824729647, -14.16423886937410259 ) ) ;
#86654 = DIRECTION ( 'NONE',  ( 0.000000000000000000, 0.000000000000000000, 1.000000000000000000 ) ) ;
#86655 = ORIENTED_EDGE ( 'NONE', *, *, #82839, .F. ) ;
#86656 =( BOUNDED_SURFACE ( )  B_SPLINE_SURFACE ( 3, 2, ( 
 ( #39061, #60566, #76550 ),
 ( #54046, #7590, #91057 ),
 ( #46545, #24060, #70044 ),
 ( #84065, #8558, #1568 ),
 ( #32017, #15582, #77523 ),
 ( #98606, #45565, #1071 ),
 ( #46065, #600, #61541 ),
 ( #62030, #62520, #84557 ),
 ( #38082, #61051, #103 ),
 ( #9041, #30549, #91564 ) ),
 .UNSPECIFIED., .F., .F., .F. ) 
 B_SPLINE_SURFACE_WITH_KNOTS ( ( 4, 2, 2, 2, 4 ),
 ( 3, 3 ),
 ( 0.000000000000000000, 0.002067014858588510882, 0.003100522287882766324, 0.003617276002529893827, 0.004134029717177021765 ),
 ( 0.000000000000000000, 1.000000000000000000 ),
 .UNSPECIFIED. ) 
 GEOMETRIC_REPRESENTATION_ITEM ( )  RATIONAL_B_SPLINE_SURFACE ( (
 ( 1.000000000000000000, 0.7411386215561424073, 1.000000000000000000),
 ( 1.000000000000000000, 0.7517628147009809414, 1.000000000000000000),
 ( 1.000000000000000000, 0.7644153482607498606, 1.000000000000000000),
 ( 1.000000000000000000, 0.8033584422216667464, 1.000000000000000000),
 ( 1.000000000000000000, 0.8197614970480194829, 1.000000000000000000),
 ( 1.000000000000000000, 0.8550190949536496943, 1.000000000000000000),
 ( 1.000000000000000000, 0.8686037895732486858, 1.000000000000000000),
 ( 1.000000000000000000, 0.9009153382757982831, 1.000000000000000000),
 ( 1.000000000000000000, 0.9197777054298900135, 1.000000000000000000),
 ( 1.000000000000000000, 0.9412039349194007976, 1.000000000000000000) ) ) 
 REPRESENTATION_ITEM ( '' )  SURFACE ( )  );
#86657 = CARTESIAN_POINT ( 'NONE',  ( 0.1532563361054082862, 21.21726448433412315, 2.638427012816831674 ) ) ;
#86658 = CARTESIAN_POINT ( 'NONE',  ( -7.771322705631315664, 15.00000000000000000, -12.24159072199926257 ) ) ;
#86659 = CARTESIAN_POINT ( 'NONE',  ( 0.1532563361054082862, 61.21726448433412315, 2.638427012816831674 ) ) ;
#86660 = CARTESIAN_POINT ( 'NONE',  ( 2.035157376598824452, 68.68868534415484817, 7.964842623401179544 ) ) ;
#86661 = CARTESIAN_POINT ( 'NONE',  ( 14.92337183194729633, 57.67559781766745886, 8.527530157486181039 ) ) ;
#86662 =( BOUNDED_SURFACE ( )  B_SPLINE_SURFACE ( 1, 2, ( 
 ( #56708, #26215, #49685, #79211, #87199, #11702, #50182, #48708, #42694, #41725, #27183, #58166, #88181, #26695, #50688, #73173, #43179, #4712, #73667, #57685, #80692, #56230, #19695, #71716, #87688, #72195, #19202, #18722, #35174, #42211, #11206, #34683, #65675, #34185, #88677, #64677, #20185, #95699, #86724, #12680, #95187, #5194, #35682, #25738, #49204, #10721, #41238, #97689, #66675, #67165, #52165, #98182, #21679, #22667, #29638, #36175, #22168, #60146, #51179, #59658, #67672, #90643, #44658, #45648, #37665, #6663, #83652, #75650, #15167, #37179, #75153, #83153, #5689, #68165, #29151, #90149, #52650, #82158, #6173, #14678, #97200, #82658, #53143, #66166, #7162, #45144, #60640, #58672, #76145, #98685, #14174, #74662, #30134, #96699, #91141, #7671, #59160, #36677, #28668, #20685, #28178, #89174, #81662, #13172, #89666, #43669, #74156, #21177, #51679, #13670, #44154, #70621, #31122, #25142, #16635, #85124, #46145, #55619, #672, #78113, #40120, #61617, #93105, #16137, #92135, #76631, #92617, #23161, #8150, #24141, #24635, #91643, #55102, #84635, #70127, #2146, #32101, #69632, #93604, #17139, #86116, #85622, #17627, #1649, #47618, #178, #62600, #15662, #31616, #46623, #1156, #38643, #23660, #32606, #69144, #54122, #48097, #9619, #77121, #63102, #78610, #53636, #62107, #39638, #38162, #47110, #68648, #30626, #77610, #61133, #84156, #8633, #9123, #39142, #54608, #48591, #12073, #72082, #34069, #72563, #26103, #49093, #34560, #10606, #26578, #65552, #10119, #50073, #88064, #4592, #2643, #58054, #11583, #57081, #18600, #80077, #40617, #80577, #42098, #3121, #79596, #41120, #63591, #27561, #11097, #50566, #71116, #79094, #95073, #41613, #42575, #33097, #27068, #87576, #73058, #33579, #96080, #19088, #49565, #18116, #88561, #71610, #35054, #20064, #64073, #65055, #87090, #94588, #56599, #64563, #94099, #3608, #4097, #95581, #25620, #57566, #19576, #56113, #86607, #75039, #13555, #37555, #60031, #30024, #29524, #60530, #14060, #37055, #43067, #44543, #58550, #74542, #59048, #44041, #89057, #36053, #14559, #51055, #20570, #22061, #6062, #66555, #59545, #90526, #21062, #75535, #89552, #98065, #36561, #73549, #82543, #28555, #68045, #91021, #90040, #81545, #98571, #97084, #67050, #13055, #82043, #97573, #6545, #29036, #81062, #52535, #67554, #74043, #51557, #43549, #35561, #22553, #21563, #12566, #5075, #5578, #52052, #83043, #45028, #66052, #7051, #96579, #28055, #46036, #40004, #31498, #1037, #61020, #70506, #15551, #92994, #54987, #76521, #9006, #31012, #8037, #91532, #8525, #38048, #23047, #39027, #39522, #7559, #70014, #566 ),
 ( #83538, #47001, #1540, #47494, #84031, #61508, #9502, #85506, #38535, #24030, #77012, #53519, #92015, #2030, #77494, #54498, #85013, #31984, #62001, #76028, #16023, #92500, #68540, #69031, #62490, #23545, #32492, #77997, #54017, #84526, #71, #46512, #69522, #30517, #16526, #24528, #17016, #62987, #93493, #53023, #15057, #45530, #41982, #86496, #33459, #56482, #48967, #72446, #3489, #10487, #3976, #80460, #34445, #55996, #79477, #63956, #56958, #10976, #18976, #71966, #4475, #17515, #71496, #11464, #86968, #78491, #86004, #93987, #17996, #48478, #10005, #25509, #78977, #11958, #49955, #64936, #94468, #94957, #26459, #41497, #32979, #25985, #42463, #49454, #87461, #79960, #95464, #33946, #47981, #18482, #64450, #40507, #63483, #26955, #57455, #72945, #34941, #3010, #87948, #71003, #40998, #19463, #2526, #65439, #25016, #55504, #52782, #37314, #38782, #83291, #37804, #15307, #58427, #6800, #29777, #22310, #45792, #75782, #82792, #76283, #53777, #7798, #27934, #14816, #67803, #30273, #45287, #91277, #7305, #76765, #88447, #44784, #83784, #60287, #50442, #57939, #65934, #88941, #21812, #80947, #96463, #52296, #84293, #23299, #38294, #98323, #68301, #98820, #90784, #8285, #14314, #27445, #19947, #15792, #35439, #60775, #75290, #22799, #321, #53277, #4959, #68789, #30763, #61269, #46280, #95963, #12445, #42953, #73432, #91777, #55754, #25271, #39767, #31256, #17269, #9260, #40745, #86245, #17758, #62740, #77256, #56248, #62248, #70267, #61752, #93737, #92270, #46761, #9755, #48235, #803, #39282, #40257, #23794, #54259, #8765, #47744, #84770, #63234, #78744, #63721, #1300, #47246, #25754, #71249, #31753, #16279, #69770, #10252, #77747, #86741, #94224, #1783, #32241, #92754, #85264, #93240, #24279, #78241, #2772, #70764, #24766, #55244, #10738, #85758, #2278, #33226, #54743, #32734, #18243, #48724, #79228, #69281, #16771, #88690, #96713, #20198, #72212, #95713, #80207, #73187, #27196, #35186, #88198, #20700, #33708, #87701, #27694, #72691, #94723, #3242, #11222, #3740, #64693, #26230, #41741, #34200, #28191, #66179, #50700, #11713, #12200, #65191, #42225, #51192, #95204, #71732, #64208, #58686, #79722, #4723, #26709, #57204, #43191, #19217, #49218, #81194, #19707, #96212, #89187, #81674, #41257, #56723, #87215, #18738, #58178, #12695, #4228, #49698, #50194, #34698, #73679, #5211, #35695, #57698, #80705, #42709, #65688, #52181, #74168, #37683, #5702, #89680, #52668, #91158, #43681, #82172, #83170, #36188, #66688, #51693, #90661, #97213, #7180, #60659, #7685, #44171, #90165, #68668, #15186, #74679, #14695, #37199, #21193, #21695 ) ),
 .UNSPECIFIED., .F., .F., .F. ) 
 B_SPLINE_SURFACE_WITH_KNOTS ( ( 2, 2 ),
 ( 3, 2, 2, 2, 2, 2, 2, 2, 2, 2, 2, 2, 2, 2, 2, 2, 2, 2, 2, 2, 2, 2, 2, 2, 2, 2, 2, 2, 2, 2, 2, 2, 2, 2, 2, 2, 2, 2, 2, 2, 2, 2, 2, 2, 2, 2, 2, 2, 2, 2, 2, 2, 2, 2, 2, 2, 2, 2, 2, 2, 2, 2, 2, 2, 2, 2, 2, 2, 2, 2, 2, 2, 2, 2, 2, 2, 2, 2, 2, 2, 2, 2, 2, 2, 2, 2, 2, 2, 2, 2, 2, 2, 2, 2, 2, 2, 2, 2, 2, 2, 2, 2, 2, 2, 2, 2, 2, 2, 2, 2, 2, 2, 2, 2, 2, 2, 2, 2, 2, 2, 2, 2, 2, 2, 2, 2, 2, 2, 2, 2, 2, 2, 2, 2, 2, 2, 2, 2, 2, 2, 2, 2, 2, 2, 2, 2, 2, 2, 2, 2, 2, 2, 2, 2, 2, 2, 2, 2, 2, 2, 2, 2, 3 ),
 ( 0.000000000000000000, 1.000000000000000000 ),
 ( 0.000000000000000000, 0.005952380952380952051, 0.01190476190476190410, 0.01785714285714285615, 0.02380952380952380820, 0.02976190476190476025, 0.03571428571428571230, 0.04166666666666666435, 0.04761904761904761640, 0.05357142857142856845, 0.05952380952380952051, 0.06547619047619047949, 0.07142857142857142461, 0.07738095238095238360, 0.08333333333333332871, 0.08928571428571428770, 0.09523809523809523281, 0.1011904761904761918, 0.1071428571428571369, 0.1130952380952380959, 0.1190476190476190410, 0.1250000000000000000, 0.1309523809523809590, 0.1369047619047619180, 0.1428571428571428492, 0.1488095238095238082, 0.1547619047619047672, 0.1607142857142857262, 0.1666666666666666574, 0.1726190476190476164, 0.1785714285714285754, 0.1845238095238095344, 0.1904761904761904656, 0.1964285714285714246, 0.2023809523809523836, 0.2083333333333333426, 0.2142857142857142738, 0.2202380952380952328, 0.2261904761904761918, 0.2321428571428571508, 0.2380952380952380820, 0.2440476190476190410, 0.2500000000000000000, 0.2559523809523809312, 0.2619047619047619180, 0.2678571428571428492, 0.2738095238095238360, 0.2797619047619047672, 0.2857142857142856984, 0.2916666666666666852, 0.2976190476190476164, 0.3035714285714285476, 0.3095238095238095344, 0.3154761904761904656, 0.3214285714285714524, 0.3273809523809523836, 0.3333333333333333148, 0.3392857142857143016, 0.3452380952380952328, 0.3511904761904761640, 0.3571428571428571508, 0.3630952380952380820, 0.3690476190476190688, 0.3750000000000000000, 0.3809523809523809312, 0.3869047619047619180, 0.3928571428571428492, 0.3988095238095238360, 0.4047619047619047672, 0.4107142857142856984, 0.4166666666666666852, 0.4226190476190476164, 0.4285714285714285476, 0.4345238095238095344, 0.4404761904761904656, 0.4464285714285714524, 0.4523809523809523836, 0.4583333333333333148, 0.4642857142857143016, 0.4702380952380952328, 0.4761904761904761640, 0.4821428571428571508, 0.4880952380952380820, 0.4940476190476190688, 0.5000000000000000000, 0.5059523809523809312, 0.5119047619047618625, 0.5178571428571429047, 0.5238095238095238360, 0.5297619047619047672, 0.5357142857142856984, 0.5416666666666666297, 0.5476190476190476719, 0.5535714285714286031, 0.5595238095238095344, 0.5654761904761904656, 0.5714285714285713969, 0.5773809523809523281, 0.5833333333333333703, 0.5892857142857143016, 0.5952380952380952328, 0.6011904761904761640, 0.6071428571428570953, 0.6130952380952381375, 0.6190476190476190688, 0.6250000000000000000, 0.6309523809523809312, 0.6369047619047618625, 0.6428571428571429047, 0.6488095238095238360, 0.6547619047619047672, 0.6607142857142856984, 0.6666666666666666297, 0.6726190476190476719, 0.6785714285714286031, 0.6845238095238095344, 0.6904761904761904656, 0.6964285714285713969, 0.7023809523809523281, 0.7083333333333333703, 0.7142857142857143016, 0.7202380952380952328, 0.7261904761904761640, 0.7321428571428570953, 0.7380952380952381375, 0.7440476190476190688, 0.7500000000000000000, 0.7559523809523809312, 0.7619047619047618625, 0.7678571428571429047, 0.7738095238095238360, 0.7797619047619047672, 0.7857142857142856984, 0.7916666666666666297, 0.7976190476190476719, 0.8035714285714286031, 0.8095238095238095344, 0.8154761904761904656, 0.8214285714285713969, 0.8273809523809523281, 0.8333333333333333703, 0.8392857142857143016, 0.8452380952380952328, 0.8511904761904761640, 0.8571428571428570953, 0.8630952380952381375, 0.8690476190476190688, 0.8750000000000000000, 0.8809523809523809312, 0.8869047619047618625, 0.8928571428571429047, 0.8988095238095238360, 0.9047619047619047672, 0.9107142857142856984, 0.9166666666666666297, 0.9226190476190476719, 0.9285714285714286031, 0.9345238095238095344, 0.9404761904761904656, 0.9464285714285713969, 0.9523809523809523281, 0.9583333333333333703, 0.9642857142857143016 ),
 .UNSPECIFIED. ) 
 GEOMETRIC_REPRESENTATION_ITEM ( )  RATIONAL_B_SPLINE_SURFACE ( (
 ( 1.000000000000000000, 0.9659258262890683122, 1.000000000000000000, 0.9659258262890683122, 1.000000000000000000, 0.9659258262890683122, 1.000000000000000000, 0.9659258262890683122, 1.000000000000000000, 0.9659258262890683122, 1.000000000000000000, 0.9659258262890683122, 1.000000000000000000, 0.9659258262890683122, 1.000000000000000000, 0.9659258262890683122, 1.000000000000000000, 0.9659258262890683122, 1.000000000000000000, 0.9659258262890683122, 1.000000000000000000, 0.9659258262890683122, 1.000000000000000000, 0.9659258262890683122, 1.000000000000000000, 0.9659258262890683122, 1.000000000000000000, 0.9659258262890683122, 1.000000000000000000, 0.9659258262890683122, 1.000000000000000000, 0.9659258262890683122, 1.000000000000000000, 0.9659258262890683122, 1.000000000000000000, 0.9659258262890683122, 1.000000000000000000, 0.9659258262890683122, 1.000000000000000000, 0.9659258262890683122, 1.000000000000000000, 0.9659258262890683122, 1.000000000000000000, 0.9659258262890683122, 1.000000000000000000, 0.9659258262890683122, 1.000000000000000000, 0.9659258262890683122, 1.000000000000000000, 0.9659258262890683122, 1.000000000000000000, 0.9659258262890683122, 1.000000000000000000, 0.9659258262890683122, 1.000000000000000000, 0.9659258262890683122, 1.000000000000000000, 0.9659258262890683122, 1.000000000000000000, 0.9659258262890683122, 1.000000000000000000, 0.9659258262890683122, 1.000000000000000000, 0.9659258262890683122, 1.000000000000000000, 0.9659258262890683122, 1.000000000000000000, 0.9659258262890683122, 1.000000000000000000, 0.9659258262890683122, 1.000000000000000000, 0.9659258262890683122, 1.000000000000000000, 0.9659258262890683122, 1.000000000000000000, 0.9659258262890683122, 1.000000000000000000, 0.9659258262890683122, 1.000000000000000000, 0.9659258262890683122, 1.000000000000000000, 0.9659258262890683122, 1.000000000000000000, 0.9659258262890683122, 1.000000000000000000, 0.9659258262890683122, 1.000000000000000000, 0.9659258262890683122, 1.000000000000000000, 0.9659258262890683122, 1.000000000000000000, 0.9659258262890683122, 1.000000000000000000, 0.9659258262890683122, 1.000000000000000000, 0.9659258262890683122, 1.000000000000000000, 0.9659258262890683122, 1.000000000000000000, 0.9659258262890683122, 1.000000000000000000, 0.9659258262890683122, 1.000000000000000000, 0.9659258262890683122, 1.000000000000000000, 0.9659258262890683122, 1.000000000000000000, 0.9659258262890683122, 1.000000000000000000, 0.9659258262890683122, 1.000000000000000000, 0.9659258262890683122, 1.000000000000000000, 0.9659258262890683122, 1.000000000000000000, 0.9659258262890683122, 1.000000000000000000, 0.9659258262890683122, 1.000000000000000000, 0.9659258262890683122, 1.000000000000000000, 0.9659258262890683122, 1.000000000000000000, 0.9659258262890683122, 1.000000000000000000, 0.9659258262890683122, 1.000000000000000000, 0.9659258262890683122, 1.000000000000000000, 0.9659258262890683122, 1.000000000000000000, 0.9659258262890683122, 1.000000000000000000, 0.9659258262890683122, 1.000000000000000000, 0.9659258262890683122, 1.000000000000000000, 0.9659258262890683122, 1.000000000000000000, 0.9659258262890683122, 1.000000000000000000, 0.9659258262890683122, 1.000000000000000000, 0.9659258262890683122, 1.000000000000000000, 0.9659258262890683122, 1.000000000000000000, 0.9659258262890683122, 1.000000000000000000, 0.9659258262890683122, 1.000000000000000000, 0.9659258262890683122, 1.000000000000000000, 0.9659258262890683122, 1.000000000000000000, 0.9659258262890683122, 1.000000000000000000, 0.9659258262890683122, 1.000000000000000000, 0.9659258262890683122, 1.000000000000000000, 0.9659258262890683122, 1.000000000000000000, 0.9659258262890683122, 1.000000000000000000, 0.9659258262890683122, 1.000000000000000000, 0.9659258262890683122, 1.000000000000000000, 0.9659258262890683122, 1.000000000000000000, 0.9659258262890683122, 1.000000000000000000, 0.9659258262890683122, 1.000000000000000000, 0.9659258262890683122, 1.000000000000000000, 0.9659258262890683122, 1.000000000000000000, 0.9659258262890683122, 1.000000000000000000, 0.9659258262890683122, 1.000000000000000000, 0.9659258262890683122, 1.000000000000000000, 0.9659258262890683122, 1.000000000000000000, 0.9659258262890683122, 1.000000000000000000, 0.9659258262890683122, 1.000000000000000000, 0.9659258262890683122, 1.000000000000000000, 0.9659258262890683122, 1.000000000000000000, 0.9659258262890683122, 1.000000000000000000, 0.9659258262890683122, 1.000000000000000000, 0.9659258262890683122, 1.000000000000000000, 0.9659258262890683122, 1.000000000000000000, 0.9659258262890683122, 1.000000000000000000, 0.9659258262890683122, 1.000000000000000000, 0.9659258262890683122, 1.000000000000000000, 0.9659258262890683122, 1.000000000000000000, 0.9659258262890683122, 1.000000000000000000, 0.9659258262890683122, 1.000000000000000000, 0.9659258262890683122, 1.000000000000000000, 0.9659258262890683122, 1.000000000000000000, 0.9659258262890683122, 1.000000000000000000, 0.9659258262890683122, 1.000000000000000000, 0.9659258262890683122, 1.000000000000000000, 0.9659258262890683122, 1.000000000000000000, 0.9659258262890683122, 1.000000000000000000, 0.9659258262890683122, 1.000000000000000000, 0.9659258262890683122, 1.000000000000000000, 0.9659258262890683122, 1.000000000000000000, 0.9659258262890683122, 1.000000000000000000, 0.9659258262890683122, 1.000000000000000000, 0.9659258262890683122, 1.000000000000000000, 0.9659258262890683122, 1.000000000000000000, 0.9659258262890683122, 1.000000000000000000, 0.9659258262890683122, 1.000000000000000000, 0.9659258262890683122, 1.000000000000000000, 0.9659258262890683122, 1.000000000000000000, 0.9659258262890683122, 1.000000000000000000, 0.9659258262890683122, 1.000000000000000000, 0.9659258262890683122, 1.000000000000000000, 0.9659258262890683122, 1.000000000000000000, 0.9659258262890683122, 1.000000000000000000, 0.9659258262890683122, 1.000000000000000000, 0.9659258262890683122, 1.000000000000000000, 0.9659258262890683122, 1.000000000000000000, 0.9659258262890683122, 1.000000000000000000, 0.9659258262890683122, 1.000000000000000000, 0.9659258262890683122, 1.000000000000000000, 0.9659258262890683122, 1.000000000000000000, 0.9659258262890683122, 1.000000000000000000, 0.9659258262890683122, 1.000000000000000000, 0.9659258262890683122, 1.000000000000000000, 0.9659258262890683122, 1.000000000000000000, 0.9659258262890683122, 1.000000000000000000, 0.9659258262890683122, 1.000000000000000000, 0.9659258262890683122, 1.000000000000000000, 0.9659258262890683122, 1.000000000000000000, 0.9659258262890683122, 1.000000000000000000, 0.9659258262890683122, 1.000000000000000000, 0.9659258262890683122, 1.000000000000000000, 0.9659258262890683122, 1.000000000000000000, 0.9659258262890683122, 1.000000000000000000, 0.9659258262890683122, 1.000000000000000000, 0.9659258262890683122, 1.000000000000000000, 0.9659258262890683122, 1.000000000000000000, 0.9659258262890683122, 1.000000000000000000, 0.9659258262890683122, 1.000000000000000000, 0.9659258262890683122, 1.000000000000000000, 0.9659258262890683122, 1.000000000000000000, 0.9659258262890683122, 1.000000000000000000, 0.9659258262890683122, 1.000000000000000000, 0.9659258262890683122, 1.000000000000000000, 0.9659258262890683122, 1.000000000000000000, 0.9659258262890683122, 1.000000000000000000),
 ( 1.000000000000000000, 0.9659258262890683122, 1.000000000000000000, 0.9659258262890683122, 1.000000000000000000, 0.9659258262890683122, 1.000000000000000000, 0.9659258262890683122, 1.000000000000000000, 0.9659258262890683122, 1.000000000000000000, 0.9659258262890683122, 1.000000000000000000, 0.9659258262890683122, 1.000000000000000000, 0.9659258262890683122, 1.000000000000000000, 0.9659258262890683122, 1.000000000000000000, 0.9659258262890683122, 1.000000000000000000, 0.9659258262890683122, 1.000000000000000000, 0.9659258262890683122, 1.000000000000000000, 0.9659258262890683122, 1.000000000000000000, 0.9659258262890683122, 1.000000000000000000, 0.9659258262890683122, 1.000000000000000000, 0.9659258262890683122, 1.000000000000000000, 0.9659258262890683122, 1.000000000000000000, 0.9659258262890683122, 1.000000000000000000, 0.9659258262890683122, 1.000000000000000000, 0.9659258262890683122, 1.000000000000000000, 0.9659258262890683122, 1.000000000000000000, 0.9659258262890683122, 1.000000000000000000, 0.9659258262890683122, 1.000000000000000000, 0.9659258262890683122, 1.000000000000000000, 0.9659258262890683122, 1.000000000000000000, 0.9659258262890683122, 1.000000000000000000, 0.9659258262890683122, 1.000000000000000000, 0.9659258262890683122, 1.000000000000000000, 0.9659258262890683122, 1.000000000000000000, 0.9659258262890683122, 1.000000000000000000, 0.9659258262890683122, 1.000000000000000000, 0.9659258262890683122, 1.000000000000000000, 0.9659258262890683122, 1.000000000000000000, 0.9659258262890683122, 1.000000000000000000, 0.9659258262890683122, 1.000000000000000000, 0.9659258262890683122, 1.000000000000000000, 0.9659258262890683122, 1.000000000000000000, 0.9659258262890683122, 1.000000000000000000, 0.9659258262890683122, 1.000000000000000000, 0.9659258262890683122, 1.000000000000000000, 0.9659258262890683122, 1.000000000000000000, 0.9659258262890683122, 1.000000000000000000, 0.9659258262890683122, 1.000000000000000000, 0.9659258262890683122, 1.000000000000000000, 0.9659258262890683122, 1.000000000000000000, 0.9659258262890683122, 1.000000000000000000, 0.9659258262890683122, 1.000000000000000000, 0.9659258262890683122, 1.000000000000000000, 0.9659258262890683122, 1.000000000000000000, 0.9659258262890683122, 1.000000000000000000, 0.9659258262890683122, 1.000000000000000000, 0.9659258262890683122, 1.000000000000000000, 0.9659258262890683122, 1.000000000000000000, 0.9659258262890683122, 1.000000000000000000, 0.9659258262890683122, 1.000000000000000000, 0.9659258262890683122, 1.000000000000000000, 0.9659258262890683122, 1.000000000000000000, 0.9659258262890683122, 1.000000000000000000, 0.9659258262890683122, 1.000000000000000000, 0.9659258262890683122, 1.000000000000000000, 0.9659258262890683122, 1.000000000000000000, 0.9659258262890683122, 1.000000000000000000, 0.9659258262890683122, 1.000000000000000000, 0.9659258262890683122, 1.000000000000000000, 0.9659258262890683122, 1.000000000000000000, 0.9659258262890683122, 1.000000000000000000, 0.9659258262890683122, 1.000000000000000000, 0.9659258262890683122, 1.000000000000000000, 0.9659258262890683122, 1.000000000000000000, 0.9659258262890683122, 1.000000000000000000, 0.9659258262890683122, 1.000000000000000000, 0.9659258262890683122, 1.000000000000000000, 0.9659258262890683122, 1.000000000000000000, 0.9659258262890683122, 1.000000000000000000, 0.9659258262890683122, 1.000000000000000000, 0.9659258262890683122, 1.000000000000000000, 0.9659258262890683122, 1.000000000000000000, 0.9659258262890683122, 1.000000000000000000, 0.9659258262890683122, 1.000000000000000000, 0.9659258262890683122, 1.000000000000000000, 0.9659258262890683122, 1.000000000000000000, 0.9659258262890683122, 1.000000000000000000, 0.9659258262890683122, 1.000000000000000000, 0.9659258262890683122, 1.000000000000000000, 0.9659258262890683122, 1.000000000000000000, 0.9659258262890683122, 1.000000000000000000, 0.9659258262890683122, 1.000000000000000000, 0.9659258262890683122, 1.000000000000000000, 0.9659258262890683122, 1.000000000000000000, 0.9659258262890683122, 1.000000000000000000, 0.9659258262890683122, 1.000000000000000000, 0.9659258262890683122, 1.000000000000000000, 0.9659258262890683122, 1.000000000000000000, 0.9659258262890683122, 1.000000000000000000, 0.9659258262890683122, 1.000000000000000000, 0.9659258262890683122, 1.000000000000000000, 0.9659258262890683122, 1.000000000000000000, 0.9659258262890683122, 1.000000000000000000, 0.9659258262890683122, 1.000000000000000000, 0.9659258262890683122, 1.000000000000000000, 0.9659258262890683122, 1.000000000000000000, 0.9659258262890683122, 1.000000000000000000, 0.9659258262890683122, 1.000000000000000000, 0.9659258262890683122, 1.000000000000000000, 0.9659258262890683122, 1.000000000000000000, 0.9659258262890683122, 1.000000000000000000, 0.9659258262890683122, 1.000000000000000000, 0.9659258262890683122, 1.000000000000000000, 0.9659258262890683122, 1.000000000000000000, 0.9659258262890683122, 1.000000000000000000, 0.9659258262890683122, 1.000000000000000000, 0.9659258262890683122, 1.000000000000000000, 0.9659258262890683122, 1.000000000000000000, 0.9659258262890683122, 1.000000000000000000, 0.9659258262890683122, 1.000000000000000000, 0.9659258262890683122, 1.000000000000000000, 0.9659258262890683122, 1.000000000000000000, 0.9659258262890683122, 1.000000000000000000, 0.9659258262890683122, 1.000000000000000000, 0.9659258262890683122, 1.000000000000000000, 0.9659258262890683122, 1.000000000000000000, 0.9659258262890683122, 1.000000000000000000, 0.9659258262890683122, 1.000000000000000000, 0.9659258262890683122, 1.000000000000000000, 0.9659258262890683122, 1.000000000000000000, 0.9659258262890683122, 1.000000000000000000, 0.9659258262890683122, 1.000000000000000000, 0.9659258262890683122, 1.000000000000000000, 0.9659258262890683122, 1.000000000000000000, 0.9659258262890683122, 1.000000000000000000, 0.9659258262890683122, 1.000000000000000000, 0.9659258262890683122, 1.000000000000000000, 0.9659258262890683122, 1.000000000000000000, 0.9659258262890683122, 1.000000000000000000, 0.9659258262890683122, 1.000000000000000000, 0.9659258262890683122, 1.000000000000000000, 0.9659258262890683122, 1.000000000000000000, 0.9659258262890683122, 1.000000000000000000, 0.9659258262890683122, 1.000000000000000000, 0.9659258262890683122, 1.000000000000000000, 0.9659258262890683122, 1.000000000000000000, 0.9659258262890683122, 1.000000000000000000, 0.9659258262890683122, 1.000000000000000000, 0.9659258262890683122, 1.000000000000000000, 0.9659258262890683122, 1.000000000000000000, 0.9659258262890683122, 1.000000000000000000, 0.9659258262890683122, 1.000000000000000000, 0.9659258262890683122, 1.000000000000000000, 0.9659258262890683122, 1.000000000000000000, 0.9659258262890683122, 1.000000000000000000, 0.9659258262890683122, 1.000000000000000000, 0.9659258262890683122, 1.000000000000000000, 0.9659258262890683122, 1.000000000000000000, 0.9659258262890683122, 1.000000000000000000, 0.9659258262890683122, 1.000000000000000000, 0.9659258262890683122, 1.000000000000000000, 0.9659258262890683122, 1.000000000000000000, 0.9659258262890683122, 1.000000000000000000, 0.9659258262890683122, 1.000000000000000000, 0.9659258262890683122, 1.000000000000000000, 0.9659258262890683122, 1.000000000000000000, 0.9659258262890683122, 1.000000000000000000) ) ) 
 REPRESENTATION_ITEM ( '' )  SURFACE ( )  );
#86663 = CARTESIAN_POINT ( 'NONE',  ( -11.92686044187656869, 7.453790035174482576, -3.195792623639521768 ) ) ;
#86664 = VECTOR ( 'NONE', #44805, 1000.000000000000000 ) ;
#86665 = ORIENTED_EDGE ( 'NONE', *, *, #86306, .T. ) ;
#86666 = CARTESIAN_POINT ( 'NONE',  ( -4.164238869374098151, 66.59541550158060375, -3.795296366450310543 ) ) ;
#86667 = DIRECTION ( 'NONE',  ( -0.1305261922200445512, 0.000000000000000000, -0.9914448613738113814 ) ) ;
#86668 = CARTESIAN_POINT ( 'NONE',  ( 10.00000000000000000, 46.81368534415484106, -10.88017736071110342 ) ) ;
#86670 = CARTESIAN_POINT ( 'NONE',  ( 19.42250999205614193, 65.14701867748817676, 5.440088680355555262 ) ) ;
#86669 = CARTESIAN_POINT ( 'NONE',  ( -2.816281873526473856, 19.12363466993042138, 9.499525473075851096E-16 ) ) ;
#86671 = CARTESIAN_POINT ( 'NONE',  ( 6.898461952320431578, 15.00000000000000000, -12.75387089053309175 ) ) ;
#86672 = PLANE ( 'NONE',  #26164 ) ;
#86673 = CARTESIAN_POINT ( 'NONE',  ( 1.821158202401524262, 31.16688879859523453, 6.499999999999990230 ) ) ;
#86674 = CARTESIAN_POINT ( 'NONE',  ( 19.84674366389459266, 48.30059781766745175, 2.638427012816836559 ) ) ;
#86675 = CARTESIAN_POINT ( 'NONE',  ( 0.1532563361054082862, 1.217264484334117824, 2.638427012816831674 ) ) ;
#86676 = CARTESIAN_POINT ( 'NONE',  ( 7.964842623401181321, -35.06131465584515183, 7.964842623401174215 ) ) ;
#86677 = CARTESIAN_POINT ( 'NONE',  ( -2.816281873526473856, 9.123634669930421381, 9.499525473075851096E-16 ) ) ;
#86679 = LINE ( 'NONE', #11163, #85672 ) ;
#86678 = CARTESIAN_POINT ( 'NONE',  ( 10.00000000000000000, 11.81368534415483751, -10.88017736071110342 ) ) ;
#86680 = DIRECTION ( 'NONE',  ( 1.000000000000000000, -0.000000000000000000, 0.000000000000000000 ) ) ;
#86681 = EDGE_CURVE ( 'NONE', #84166, #76088, #67131, .T. ) ;
#86682 = CARTESIAN_POINT ( 'NONE',  ( 13.79529636645031943, 30.34541550158063927, -14.16423886937409904 ) ) ;
#86683 = CARTESIAN_POINT ( 'NONE',  ( 24.16423886937410614, 29.30374883491396787, 8.672049930838204340E-16 ) ) ;
#86684 = CARTESIAN_POINT ( 'NONE',  ( 10.00000000000000000, 65.55374883491396076, -14.16423886937410082 ) ) ;
#86685 = CARTESIAN_POINT ( 'NONE',  ( 2.791683348922237240, 45.38393115100079456, -7.208316651077763204 ) ) ;
#86686 = CARTESIAN_POINT ( 'NONE',  ( -1.099225684535947600, 43.70696800326375353, -6.408140936763238038 ) ) ;
#86687 = CARTESIAN_POINT ( 'NONE',  ( 12.91533473730993009, 11.60535201082150536, -10.88017736071109987 ) ) ;
#86688 = VERTEX_POINT ( 'NONE', #52790 ) ;
#86689 = CARTESIAN_POINT ( 'NONE',  ( 2.791683348922240793, 31.63393115100078745, 7.208316651077764092 ) ) ;
#86690 = CARTESIAN_POINT ( 'NONE',  ( 10.00000000000000178, 44.31368534415484106, 10.88017736071110342 ) ) ;
#86691 = CARTESIAN_POINT ( 'NONE',  ( 19.38216949554541202, 5.998634669930420493, 9.382169495545424454 ) ) ;
#86693 = DIRECTION ( 'NONE',  ( -0.7716245833877148907, 0.000000000000000000, -0.6360782202777701677 ) ) ;
#86692 = CARTESIAN_POINT ( 'NONE',  ( 6.204703633549690345, 22.84541550158062861, 14.16423886937410082 ) ) ;
#86694 = CARTESIAN_POINT ( 'NONE',  ( 18.17829156368507171, 34.16792564121897158, 6.500000000000019540 ) ) ;
#86695 = CIRCLE ( 'NONE', #24403, 1.000000000000000000 ) ;
#86696 = CARTESIAN_POINT ( 'NONE',  ( 18.52753015748618282, 18.92559781766745175, -4.923371831947291888 ) ) ;
#86697 = CARTESIAN_POINT ( 'NONE',  ( 10.00000000000000000, 52.87363466993041783, -12.81628187352647608 ) ) ;
#86698 = CARTESIAN_POINT ( 'NONE',  ( 1.472469842513823179, 56.42559781766745886, 4.923371831947296329 ) ) ;
#86699 = EDGE_LOOP ( 'NONE', ( #60748, #80213, #28968, #66582 ) ) ;
#86700 = STYLED_ITEM ( 'NONE', ( #49051 ), #93125 ) ;
#86701 = CARTESIAN_POINT ( 'NONE',  ( 1.816707512666844604, 35.10290668512023871, -6.499999999999958256 ) ) ;
#86702 = CARTESIAN_POINT ( 'NONE',  ( 4.722628015970558479, -9.822377395415374579, 2.750000000000000000 ) ) ;
#86703 = CARTESIAN_POINT ( 'NONE',  ( 20.88017736071110164, 5.355352010821503583, 2.915334737309930979 ) ) ;
#86704 = CARTESIAN_POINT ( 'NONE',  ( 6.204703633549690345, 5.762082168247301794, -14.16423886937410259 ) ) ;
#86705 = CARTESIAN_POINT ( 'NONE',  ( 5.076628168052704559, 5.175597817667451750, -8.527530157486179263 ) ) ;
#86706 = CARTESIAN_POINT ( 'NONE',  ( 12.63842701281683922, 44.55059781766745175, -9.846743663894590881 ) ) ;
#86707 = CARTESIAN_POINT ( 'NONE',  ( 2.035157376598824452, 18.68868534415484106, 7.964842623401179544 ) ) ;
#86708 = VECTOR ( 'NONE', #51835, 1000.000000000000114 ) ;
#86709 = CARTESIAN_POINT ( 'NONE',  ( 12.00809552683952752, 15.00000000000000000, 8.989195838243626113 ) ) ;
#86710 = CARTESIAN_POINT ( 'NONE',  ( 0.1532563361054082862, 61.21726448433412315, 2.638427012816831674 ) ) ;
#86711 = VERTEX_POINT ( 'NONE', #75790 ) ;
#86713 = EDGE_LOOP ( 'NONE', ( #79967, #14607, #58579, #83892 ) ) ;
#86712 = EDGE_CURVE ( 'NONE', #8076, #26237, #13818, .T. ) ;
#86714 = ORIENTED_EDGE ( 'NONE', *, *, #62755, .F. ) ;
#86715 = CARTESIAN_POINT ( 'NONE',  ( 0.000000000000000000, 14.49999999999999822, 0.000000000000000000 ) ) ;
#86716 = CARTESIAN_POINT ( 'NONE',  ( 17.08211943468705840, 15.13708216824730179, -12.26659068614894466 ) ) ;
#86717 = CARTESIAN_POINT ( 'NONE',  ( -4.164238869374099927, 2.012082168247300906, 3.795296366450308767 ) ) ;
#86718 = CARTESIAN_POINT ( 'NONE',  ( -4.164238869374099927, 47.01208216824729647, 3.795296366450308767 ) ) ;
#86719 = CARTESIAN_POINT ( 'NONE',  ( 1.472469842513823179, 55.59226448433412315, -4.923371831947296329 ) ) ;
#86720 = CARTESIAN_POINT ( 'NONE',  ( 17.20831665107776587, 19.13393115100078035, -7.208316651077762316 ) ) ;
#86721 = SURFACE_STYLE_USAGE ( .BOTH. , #64187 ) ;
#86723 = CARTESIAN_POINT ( 'NONE',  ( -2.816281873526473856, -0.8763653300695799508, 9.499525473075851096E-16 ) ) ;
#86722 = CARTESIAN_POINT ( 'NONE',  ( 7.084665262690076126, 22.02201867748817321, -10.88017736071110164 ) ) ;
#86724 = CARTESIAN_POINT ( 'NONE',  ( 17.08211943468705130, 8.470415501580635720, 12.26659068614894998 ) ) ;
#86725 = CARTESIAN_POINT ( 'NONE',  ( -4.164238869374098151, 41.59541550158061796, -3.795296366450310543 ) ) ;
#86726 = EDGE_CURVE ( 'NONE', #68457, #89588, #14320, .T. ) ;
#86727 = CARTESIAN_POINT ( 'NONE',  ( -0.8801773607111009756, 8.063685344154837509, 1.068504757029289695E-15 ) ) ;
#86728 = CARTESIAN_POINT ( 'NONE',  ( -4.391347328462822830, 0.2301508954901552439, -14.28069739540086580 ) ) ;
#86729 = CARTESIAN_POINT ( 'NONE',  ( 9.879999999999991900, 20.99999999999999645, 0.000000000000000000 ) ) ;
#86730 = CARTESIAN_POINT ( 'NONE',  ( 2.035157376598822676, 62.43868534415483396, -7.964842623401177768 ) ) ;
#86731 = CARTESIAN_POINT ( 'NONE',  ( 0.1532563361054082862, 11.21726448433411605, 2.638427012816831674 ) ) ;
#86732 = AXIS2_PLACEMENT_3D ( 'NONE', #1411, #10369, #63832 ) ;
#86733 = CARTESIAN_POINT ( 'NONE',  ( -7.080143328635299049, -69.54337233422661768, 4.000000000001613820 ) ) ;
#86734 = ORIENTED_EDGE ( 'NONE', *, *, #71994, .F. ) ;
#86735 = CARTESIAN_POINT ( 'NONE',  ( -6.689969769698787871, -0.03417435944610275333, -12.58200319823979285 ) ) ;
#86736 = ORIENTED_EDGE ( 'NONE', *, *, #51145, .F. ) ;
#86737 = CARTESIAN_POINT ( 'NONE',  ( 10.00000000000000178, 17.25893115100078745, 9.846743663894594434 ) ) ;
#86738 = ORIENTED_EDGE ( 'NONE', *, *, #47800, .T. ) ;
#86739 = CARTESIAN_POINT ( 'NONE',  ( 20.36894250292379738, 34.92874883491396076, -10.36894250292379027 ) ) ;
#86740 = CARTESIAN_POINT ( 'NONE',  ( 19.84674366389459266, 33.71726448433410894, -2.638427012816827677 ) ) ;
#86741 = CARTESIAN_POINT ( 'NONE',  ( 20.88017736071110519, 45.56368534415484106, 2.639326808657452039E-16 ) ) ;
#86742 = TOROIDAL_SURFACE ( 'NONE', #43605, 3.699999999999999289, 0.2999999999999999889 ) ;
#86743 = CARTESIAN_POINT ( 'NONE',  ( 2.035157376598822676, 47.43868534415484817, -7.964842623401177768 ) ) ;
#86744 = VECTOR ( 'NONE', #26374, 1000.000000000000000 ) ;
#86745 = CARTESIAN_POINT ( 'NONE',  ( 3.434112377981060948, 0.5819680032637514211, 12.81628187352647430 ) ) ;
#86746 = ORIENTED_EDGE ( 'NONE', *, *, #17081, .T. ) ;
#86747 = CARTESIAN_POINT ( 'NONE',  ( -0.3689425029237881626, 2.428748834913967869, 10.36894250292379027 ) ) ;
#86748 = ORIENTED_EDGE ( 'NONE', *, *, #37970, .F. ) ;
#86749 = EDGE_CURVE ( 'NONE', #75285, #21162, #48001, .T. ) ;
#86750 = VERTEX_POINT ( 'NONE', #60298 ) ;
#86751 = CARTESIAN_POINT ( 'NONE',  ( 22.81628187352648496, 26.83196800326374998, -3.434112377981050290 ) ) ;
#86752 = CARTESIAN_POINT ( 'NONE',  ( 19.84674366389459621, 28.50893115100078745, 7.409399052514197653E-17 ) ) ;
#86753 = CARTESIAN_POINT ( 'NONE',  ( 0.000000000000000000, 81.99999999999992895, 5.000000000000000000 ) ) ;
#86754 = CARTESIAN_POINT ( 'NONE',  ( 16.40814093676323893, 45.79030133659708923, 11.09922568453595026 ) ) ;
#86755 = LINE ( 'NONE', #18260, #49575 ) ;
#86756 = CARTESIAN_POINT ( 'NONE',  ( 12.63842701281683922, 29.55059781766745175, -9.846743663894590881 ) ) ;
#86757 = CARTESIAN_POINT ( 'NONE',  ( 2.035157376598822676, 57.43868534415484106, -7.964842623401177768 ) ) ;
#86758 = VECTOR ( 'NONE', #84960, 1000.000000000000114 ) ;
#86759 = CARTESIAN_POINT ( 'NONE',  ( 13.99999999999999822, 11.50000000000000000, -6.500000000000000888 ) ) ;
#86760 = CYLINDRICAL_SURFACE ( 'NONE', #75527, 15.00000000000000000 ) ;
#86761 = DIRECTION ( 'NONE',  ( 0.000000000000000000, 0.000000000000000000, 1.000000000000000000 ) ) ;
#86762 = CARTESIAN_POINT ( 'NONE',  ( 0.1532563361054100626, 0.8005978176674514168, -2.638427012816831230 ) ) ;
#86763 = VECTOR ( 'NONE', #34347, 1000.000000000000000 ) ;
#86764 = CARTESIAN_POINT ( 'NONE',  ( 16.40814093676323893, 15.79030133659708746, 11.09922568453595026 ) ) ;
#86766 = DIRECTION ( 'NONE',  ( -0.000000000000000000, -1.000000000000000000, -0.000000000000000000 ) ) ;
#86765 = AXIS2_PLACEMENT_3D ( 'NONE', #6243, #3419, #64868 ) ;
#86767 = B_SPLINE_CURVE_WITH_KNOTS ( 'NONE', 3,
 ( #60012, #52517, #20355, #4869 ),
 .UNSPECIFIED., .F., .F.,
 ( 4, 4 ),
 ( 4.336808689942017255E-19, 0.002657014572711318117 ),
 .UNSPECIFIED. ) ;
#86768 = CARTESIAN_POINT ( 'NONE',  ( 19.84674366389459621, 48.50893115100078745, 7.409399052514197653E-17 ) ) ;
#86769 = CARTESIAN_POINT ( 'NONE',  ( 16.40814093676324603, 62.45696800326376064, -11.09922568453594671 ) ) ;
#86770 = CARTESIAN_POINT ( 'NONE',  ( 24.16423886937410614, 4.303748834913967869, 8.672049930838204340E-16 ) ) ;
#86771 = CARTESIAN_POINT ( 'NONE',  ( 18.52753015748617571, 38.09226448433412315, 4.923371831947298993 ) ) ;
#86772 = VECTOR ( 'NONE', #90019, 1000.000000000000000 ) ;
#86773 = CARTESIAN_POINT ( 'NONE',  ( 16.40814093676324603, 32.45696800326375353, -11.09922568453594671 ) ) ;
#86775 = DIRECTION ( 'NONE',  ( 0.000000000000000000, 1.000000000000000000, 0.000000000000000000 ) ) ;
#86774 = SURFACE_SIDE_STYLE ('',( #17789 ) ) ;
#86776 = CARTESIAN_POINT ( 'NONE',  ( 0.5774900079438590739, 52.64701867748817676, -5.440088680355550821 ) ) ;
#86777 = CARTESIAN_POINT ( 'NONE',  ( 16.40814093676323893, 0.7903013365970867898, 11.09922568453595026 ) ) ;
#86778 = CARTESIAN_POINT ( 'NONE',  ( -9.898881779040801021, 15.00000000000000000, 10.25059215482569641 ) ) ;
#86779 = CARTESIAN_POINT ( 'NONE',  ( 2.791683348922237240, 20.38393115100078745, -7.208316651077763204 ) ) ;
#86780 = CARTESIAN_POINT ( 'NONE',  ( 20.88017736071110164, 30.35535201082151247, 2.915334737309930979 ) ) ;
#86781 = CARTESIAN_POINT ( 'NONE',  ( -1.099225684535947600, 29.54030133659708923, 6.408140936763237150 ) ) ;
#86782 = CARTESIAN_POINT ( 'NONE',  ( 19.84674366389459266, 23.71726448433412315, -2.638427012816827677 ) ) ;
#86783 =( LENGTH_UNIT ( ) NAMED_UNIT ( * ) SI_UNIT ( .MILLI., .METRE. ) );
#86784 = CARTESIAN_POINT ( 'NONE',  ( -7.754961693898215991, 84.52280956283338753, 4.000000000000000000 ) ) ;
#86785 = CARTESIAN_POINT ( 'NONE',  ( 0.5774900079438607392, 38.48035201082150536, 5.440088680355550821 ) ) ;
#86786 = ORIENTED_EDGE ( 'NONE', *, *, #86035, .F. ) ;
#86787 = CARTESIAN_POINT ( 'NONE',  ( 0.5774900079438590739, 57.64701867748817676, -5.440088680355550821 ) ) ;
#86788 = SURFACE_STYLE_USAGE ( .BOTH. , #17802 ) ;
#86790 = CARTESIAN_POINT ( 'NONE',  ( 20.88017736071110164, 25.35535201082150891, 2.915334737309930979 ) ) ;
#86789 = CARTESIAN_POINT ( 'NONE',  ( 19.84674366389459266, 43.71726448433410894, -2.638427012816827677 ) ) ;
#86791 = CARTESIAN_POINT ( 'NONE',  ( -5.817157072110894056, 14.63595249122789177, 13.82608706751083893 ) ) ;
#86792 = CARTESIAN_POINT ( 'NONE',  ( 20.88017736071110875, 45.77201867748816966, -2.915334737309920765 ) ) ;
#86794 = CARTESIAN_POINT ( 'NONE',  ( 20.15039907845753575, 59.72266099184918176, 6.262539305110074395 ) ) ;
#86793 = CARTESIAN_POINT ( 'NONE',  ( 15.44008868035555793, 11.39701867748817143, -9.422509992056140149 ) ) ;
#86795 = DIRECTION ( 'NONE',  ( -0.8788171126619616080, 0.000000000000000000, -0.4771587602596153999 ) ) ;
#86796 = CARTESIAN_POINT ( 'NONE',  ( 18.52753015748617571, 38.09226448433412315, 4.923371831947298993 ) ) ;
#86798 = CARTESIAN_POINT ( 'NONE',  ( -1.548803529117957822, 0.000000000000000000, -5.228673087012116305 ) ) ;
#86797 = CARTESIAN_POINT ( 'NONE',  ( 10.00000000000000000, 40.55374883491397497, -14.16423886937410082 ) ) ;
#86799 = CARTESIAN_POINT ( 'NONE',  ( 1.711636803080551772, 6.844927826957706074, -6.500000000000008882 ) ) ;
#86800 = AXIS2_PLACEMENT_3D ( 'NONE', #69224, #22744, #37261 ) ;
#86801 = ADVANCED_FACE ( 'NONE', ( #46286 ), #90790, .F. ) ;
#86802 =( NAMED_UNIT ( * ) PLANE_ANGLE_UNIT ( ) SI_UNIT ( $, .RADIAN. ) );
#86803 = CARTESIAN_POINT ( 'NONE',  ( 22.26659068614894466, 28.88708216824730357, 7.082119434687054849 ) ) ;
#86804 = CARTESIAN_POINT ( 'NONE',  ( -3.499999999999998668, 1.019547802438465434, 2.750000000000000444 ) ) ;
#86805 = CARTESIAN_POINT ( 'NONE',  ( 10.00000000000000178, 68.05374883491397497, 14.16423886937410082 ) ) ;
#86806 = CARTESIAN_POINT ( 'NONE',  ( 7.361572987183170547, 32.05059781766745175, 9.846743663894590881 ) ) ;
#86808 = DIRECTION ( 'NONE',  ( 1.000000000000000000, 0.000000000000000000, -0.000000000000000000 ) ) ;
#86807 = DIRECTION ( 'NONE',  ( -1.000000000000000000, 0.000000000000000000, 0.000000000000000000 ) ) ;
#86809 = CARTESIAN_POINT ( 'NONE',  ( -0.8801773607111008646, 63.27201867748817676, 2.915334737309923430 ) ) ;
#86810 = CARTESIAN_POINT ( 'NONE',  ( 3.591859063236761518, 64.95696800326376774, 11.09922568453594849 ) ) ;
#86811 = CARTESIAN_POINT ( 'NONE',  ( 20.88017736071110519, 25.56368534415483751, 2.639326808657452039E-16 ) ) ;
#86812 = CARTESIAN_POINT ( 'NONE',  ( -2.816281873526471635, 58.91530133659707502, -3.434112377981056508 ) ) ;
#86813 = CARTESIAN_POINT ( 'NONE',  ( 19.38216949554541557, 12.24863466993041961, -9.382169495545420901 ) ) ;
#86814 = CARTESIAN_POINT ( 'NONE',  ( 19.84674366389459621, 13.50893115100078568, 7.409399052514197653E-17 ) ) ;
#86815 = ORIENTED_EDGE ( 'NONE', *, *, #24182, .F. ) ;
#86816 = DIRECTION ( 'NONE',  ( 0.000000000000000000, 1.000000000000000000, 0.000000000000000000 ) ) ;
#86817 = CARTESIAN_POINT ( 'NONE',  ( 2.913501739333762774, 15.00000000000000000, -14.20427779279532565 ) ) ;
#86818 = CARTESIAN_POINT ( 'NONE',  ( 24.16423886937410614, 59.30374883491397497, 8.672049930838204340E-16 ) ) ;
#86819 = CARTESIAN_POINT ( 'NONE',  ( -0.3689425029237898834, 31.17874883491396787, -10.36894250292378850 ) ) ;
#86820 = CARTESIAN_POINT ( 'NONE',  ( 4.559911319644449179, 33.89701867748817676, 9.422509992056141925 ) ) ;
#86821 = CARTESIAN_POINT ( 'NONE',  ( -0.8801773607111009756, 43.06368534415484106, 1.068504757029289695E-15 ) ) ;
#86822 = CARTESIAN_POINT ( 'NONE',  ( -19.64999999999999858, 0.000000000000000000, 8.000000000000000000 ) ) ;
#86823 = CARTESIAN_POINT ( 'NONE',  ( 1.472469842513823179, 5.592264484334118713, -4.923371831947296329 ) ) ;
#86824 = CARTESIAN_POINT ( 'NONE',  ( 14.92337183194729988, 24.34226448433411960, -8.527530157486177487 ) ) ;
#86825 = DIRECTION ( 'NONE',  ( 0.000000000000000000, -1.000000000000000000, 0.000000000000000000 ) ) ;
#86826 = CARTESIAN_POINT ( 'NONE',  ( -12.00809552683969272, 14.63606912728209508, 8.989195838243468017 ) ) ;
#86827 = CARTESIAN_POINT ( 'NONE',  ( 18.52753015748617571, 23.09226448433411960, 4.923371831947298993 ) ) ;
#86828 = CARTESIAN_POINT ( 'NONE',  ( 18.52753015748617571, 48.09226448433412315, 4.923371831947298993 ) ) ;
#86829 = CARTESIAN_POINT ( 'NONE',  ( -0.8801773607111009756, 28.06368534415484106, 1.068504757029289695E-15 ) ) ;
#86830 = ADVANCED_FACE ( 'NONE', ( #68796 ), #91704, .T. ) ;
#86831 = CARTESIAN_POINT ( 'NONE',  ( 3.591859063236763294, 48.29030133659708923, -11.09922568453595026 ) ) ;
#86832 =( GEOMETRIC_REPRESENTATION_CONTEXT ( 3 ) GLOBAL_UNCERTAINTY_ASSIGNED_CONTEXT ( ( #18522 ) ) GLOBAL_UNIT_ASSIGNED_CONTEXT ( ( #37169, #21669, #82148 ) ) REPRESENTATION_CONTEXT ( 'NONE', 'WORKASPACE' ) );
#86833 = CARTESIAN_POINT ( 'NONE',  ( 17.96484262340118221, 49.93868534415484106, 7.964842623401181321 ) ) ;
#86834 = CARTESIAN_POINT ( 'NONE',  ( 0.1532563361054082862, 31.21726448433412315, 2.638427012816831674 ) ) ;
#86836 = CARTESIAN_POINT ( 'NONE',  ( 7.361572987183170547, 22.05059781766745530, 9.846743663894590881 ) ) ;
#86835 = CARTESIAN_POINT ( 'NONE',  ( -0.3689425029237898834, 51.17874883491397497, -10.36894250292378850 ) ) ;
#86837 = DIRECTION ( 'NONE',  ( 1.927470528863119542E-16, -1.000000000000000000, 0.000000000000000000 ) ) ;
#86838 = CARTESIAN_POINT ( 'NONE',  ( 12.63842701281683034, 57.46726448433411605, 9.846743663894596210 ) ) ;
#86839 = CARTESIAN_POINT ( 'NONE',  ( 10.00000000000000178, 8.053748834913967869, 14.16423886937410082 ) ) ;
#86840 = EDGE_CURVE ( 'NONE', #91650, #71473, #26580, .T. ) ;
#86841 = CARTESIAN_POINT ( 'NONE',  ( 6.204703633549690345, 32.84541550158063927, 14.16423886937410082 ) ) ;
#86842 = CARTESIAN_POINT ( 'NONE',  ( 10.00000000000000000, 24.75893115100078745, -9.846743663894594434 ) ) ;
#86843 = DIRECTION ( 'NONE',  ( -0.000000000000000000, 1.000000000000000000, -0.000000000000000000 ) ) ;
#86844 = CARTESIAN_POINT ( 'NONE',  ( 7.084665262690076126, 24.10535201082150181, 10.88017736071109987 ) ) ;
#86845 = VECTOR ( 'NONE', #57635, 1000.000000000000114 ) ;
#86846 = CARTESIAN_POINT ( 'NONE',  ( 15.44008868035555793, 41.39701867748817676, -9.422509992056140149 ) ) ;
#86847 = CARTESIAN_POINT ( 'NONE',  ( 0.5774900079438590739, 37.64701867748817676, -5.440088680355550821 ) ) ;
#86848 = ORIENTED_EDGE ( 'NONE', *, *, #68674, .F. ) ;
#86849 = CARTESIAN_POINT ( 'NONE',  ( 7.084665262690076126, 54.10535201082151247, 10.88017736071109987 ) ) ;
#86850 = VERTEX_POINT ( 'NONE', #27714 ) ;
#86851 = LINE ( 'NONE', #95325, #82478 ) ;
#86852 = CARTESIAN_POINT ( 'NONE',  ( 0.5774900079438590739, 67.64701867748817676, -5.440088680355550821 ) ) ;
#86853 = VERTEX_POINT ( 'NONE', #57224 ) ;
#86854 = CARTESIAN_POINT ( 'NONE',  ( 20.88017736071110164, 60.35535201082151957, 2.915334737309930979 ) ) ;
#86855 = PLANE ( 'NONE',  #53172 ) ;
#86856 = CARTESIAN_POINT ( 'NONE',  ( 0.000000000000000000, 0.5000000000000004441, 0.000000000000000000 ) ) ;
#86857 = CARTESIAN_POINT ( 'NONE',  ( 7.084665262690076126, 9.105352010821503583, 10.88017736071109987 ) ) ;
#86858 = CARTESIAN_POINT ( 'NONE',  ( 17.20831665107776587, 12.88393115100078390, 7.208316651077764980 ) ) ;
#86859 = CARTESIAN_POINT ( 'NONE',  ( -4.164238869374098151, 6.595415501580634832, -3.795296366450310543 ) ) ;
#86860 = CARTESIAN_POINT ( 'NONE',  ( 2.791683348922240793, 1.633931151000784565, 7.208316651077764092 ) ) ;
#86861 = CARTESIAN_POINT ( 'NONE',  ( 17.96484262340118221, 9.938685344154837509, 7.964842623401181321 ) ) ;
#86862 = CARTESIAN_POINT ( 'NONE',  ( 2.791683348922237240, 40.38393115100078035, -7.208316651077763204 ) ) ;
#86863 = ORIENTED_EDGE ( 'NONE', *, *, #43644, .T. ) ;
#86864 = CARTESIAN_POINT ( 'NONE',  ( 14.92337183194729988, 54.34226448433412315, -8.527530157486177487 ) ) ;
#86865 = ORIENTED_EDGE ( 'NONE', *, *, #88187, .T. ) ;
#86866 = CARTESIAN_POINT ( 'NONE',  ( 19.42250999205614193, 50.14701867748817676, 5.440088680355555262 ) ) ;
#86867 = CARTESIAN_POINT ( 'NONE',  ( 10.00000000000000178, 52.25893115100078745, 9.846743663894594434 ) ) ;
#86868 = CARTESIAN_POINT ( 'NONE',  ( 16.40814093676324603, 27.45696800326375708, -11.09922568453594671 ) ) ;
#86869 = CARTESIAN_POINT ( 'NONE',  ( 7.084665262690076126, 67.02201867748817676, -10.88017736071110164 ) ) ;
#86870 = CARTESIAN_POINT ( 'NONE',  ( 20.88017736071110875, 60.77201867748817676, -2.915334737309920765 ) ) ;
#86871 = CARTESIAN_POINT ( 'NONE',  ( 15.44008868035555793, 6.397018677488171434, -9.422509992056140149 ) ) ;
#86872 = CARTESIAN_POINT ( 'NONE',  ( 3.591859063236763294, 43.29030133659708923, -11.09922568453595026 ) ) ;
#86873 = FACE_OUTER_BOUND ( 'NONE', #70757, .T. ) ;
#86874 = ORIENTED_EDGE ( 'NONE', *, *, #1938, .T. ) ;
#86875 = CARTESIAN_POINT ( 'NONE',  ( 13.43411237798106583, 22.66530133659708923, -12.81628187352647252 ) ) ;
#86876 = CARTESIAN_POINT ( 'NONE',  ( -0.8801773607110991993, 37.85535201082151247, -2.915334737309923874 ) ) ;
#86877 = ORIENTED_EDGE ( 'NONE', *, *, #50359, .F. ) ;
#86878 = CARTESIAN_POINT ( 'NONE',  ( 10.00000000000000000, 64.75893115100078035, -9.846743663894594434 ) ) ;
#86880 = CARTESIAN_POINT ( 'NONE',  ( 0.1532563361054083140, 46.00893115100079456, 1.131784320476157264E-15 ) ) ;
#86879 = CARTESIAN_POINT ( 'NONE',  ( 5.076628168052704559, 15.17559781766745175, -8.527530157486179263 ) ) ;
#86881 = CARTESIAN_POINT ( 'NONE',  ( -8.029112100182558720, -1.061264519223844571, 3.750000000000001332 ) ) ;
#86882 = CARTESIAN_POINT ( 'NONE',  ( 17.20831665107776587, 34.13393115100078745, -7.208316651077762316 ) ) ;
#86883 = CARTESIAN_POINT ( 'NONE',  ( 5.056330833731752072, 3.901243639414221473E-16, -13.58983143750699973 ) ) ;
#86884 = CARTESIAN_POINT ( 'NONE',  ( -4.000000000000000000, 37.25000000000000000, -4.000000000000000000 ) ) ;
#86885 = CARTESIAN_POINT ( 'NONE',  ( 2.791683348922240793, 26.63393115100078745, 7.208316651077764092 ) ) ;
#86886 = DIRECTION ( 'NONE',  ( 0.000000000000000000, 0.000000000000000000, 1.000000000000000000 ) ) ;
#86888 = ORIENTED_EDGE ( 'NONE', *, *, #93932, .T. ) ;
#86887 = CARTESIAN_POINT ( 'NONE',  ( 12.63842701281683034, 62.46726448433410894, 9.846743663894596210 ) ) ;
#86889 = DIRECTION ( 'NONE',  ( -0.000000000000000000, -0.000000000000000000, -1.000000000000000000 ) ) ;
#86890 = CARTESIAN_POINT ( 'NONE',  ( 0.6178305044545818747, 23.49863466993041783, -9.382169495545419124 ) ) ;
#86891 = CARTESIAN_POINT ( 'NONE',  ( 12.63842701281683034, 47.46726448433412315, 9.846743663894596210 ) ) ;
#86892 = AXIS2_PLACEMENT_3D ( 'NONE', #79013, #87007, #56032 ) ;
#86893 = CARTESIAN_POINT ( 'NONE',  ( -14.02068044289389626, 14.49999999999999112, 5.331089937175563342 ) ) ;
#86894 = CARTESIAN_POINT ( 'NONE',  ( -2.266590686148945544, 47.22041550158063927, 7.082119434687048631 ) ) ;
#86895 = CARTESIAN_POINT ( 'NONE',  ( 5.076628168052704559, 20.17559781766745175, -8.527530157486179263 ) ) ;
#86896 = CARTESIAN_POINT ( 'NONE',  ( 13.48086198287162141, 15.00000000000000000, 8.610676897597548063 ) ) ;
#86897 = CIRCLE ( 'NONE', #43785, 15.00000000000000000 ) ;
#86898 = CARTESIAN_POINT ( 'NONE',  ( -2.266590686148945544, 61.38708216824730357, -7.082119434687050408 ) ) ;
#86899 = CARTESIAN_POINT ( 'NONE',  ( 19.84674366389459266, 53.30059781766744464, 2.638427012816836559 ) ) ;
#86900 = CARTESIAN_POINT ( 'NONE',  ( 10.00000000000000178, 4.313685344154837509, 10.88017736071110342 ) ) ;
#86901 = CARTESIAN_POINT ( 'NONE',  ( 10.00000000000000178, 33.05374883491396787, 14.16423886937410082 ) ) ;
#86902 = CARTESIAN_POINT ( 'NONE',  ( 20.36894250292379382, 43.67874883491397497, 10.36894250292379205 ) ) ;
#86903 = DIRECTION ( 'NONE',  ( 0.000000000000000000, 0.000000000000000000, 1.000000000000000000 ) ) ;
#86905 = CARTESIAN_POINT ( 'NONE',  ( 0.1532563361054082862, 56.21726448433411605, 2.638427012816831674 ) ) ;
#86904 = CARTESIAN_POINT ( 'NONE',  ( 1.274849032794223680, 28.57228050351031001, 6.499999999999884537 ) ) ;
#86906 = VERTEX_POINT ( 'NONE', #58196 ) ;
#86907 = CARTESIAN_POINT ( 'NONE',  ( 12.91533473730993009, 41.60535201082149825, -10.88017736071109987 ) ) ;
#86908 = DIRECTION ( 'NONE',  ( 0.000000000000000000, 0.000000000000000000, 1.000000000000000000 ) ) ;
#86909 = CARTESIAN_POINT ( 'NONE',  ( 0.000000000000000000, 15.00000000000000000, 0.000000000000000000 ) ) ;
#86910 = EDGE_CURVE ( 'NONE', #10984, #79104, #97233, .T. ) ;
#86911 = CARTESIAN_POINT ( 'NONE',  ( 19.84674366389459266, 53.71726448433411605, -2.638427012816827677 ) ) ;
#86912 = CARTESIAN_POINT ( 'NONE',  ( -0.08248232600719085372, 0.1423898869303599768, 6.349449577244200782 ) ) ;
#86913 = B_SPLINE_CURVE_WITH_KNOTS ( 'NONE', 3,
 ( #42406, #72883, #81377, #80891, #43858, #27878 ),
 .UNSPECIFIED., .F., .F.,
 ( 4, 2, 4 ),
 ( 0.0002800154274984798615, 0.0006862208078247625676, 0.001092426188151045165 ),
 .UNSPECIFIED. ) ;
#86914 = CARTESIAN_POINT ( 'NONE',  ( 12.26659068614894466, 9.720415501580641049, -7.082119434687053960 ) ) ;
#86915 = CARTESIAN_POINT ( 'NONE',  ( 7.361572987183170547, 57.05059781766744464, 9.846743663894590881 ) ) ;
#86916 = DIRECTION ( 'NONE',  ( 0.000000000000000000, 1.000000000000000000, -0.000000000000000000 ) ) ;
#86917 = ORIENTED_EDGE ( 'NONE', *, *, #51498, .F. ) ;
#86918 = CARTESIAN_POINT ( 'NONE',  ( -0.3689425029237881626, 32.42874883491395366, 10.36894250292379027 ) ) ;
#86919 = DIRECTION ( 'NONE',  ( -1.927470528863119542E-16, 1.000000000000000000, 0.000000000000000000 ) ) ;
#86921 = CARTESIAN_POINT ( 'NONE',  ( -6.189644032515588812, 14.95077488074853456, -13.39157970158804645 ) ) ;
#86920 = CARTESIAN_POINT ( 'NONE',  ( -6.606690058644155705, -50.93246948813188624, -2.500000000001612044 ) ) ;
#86922 = CARTESIAN_POINT ( 'NONE',  ( 2.035157376598824452, 13.68868534415483751, 7.964842623401179544 ) ) ;
#86923 = CARTESIAN_POINT ( 'NONE',  ( -2.816281873526473856, 24.12363466993042138, 9.499525473075851096E-16 ) ) ;
#86924 = CARTESIAN_POINT ( 'NONE',  ( 0.1532563361054082862, 6.217264484334118713, 2.638427012816831674 ) ) ;
#86925 = CARTESIAN_POINT ( 'NONE',  ( 18.72515096720568906, 15.05509018479935612, 6.500000000000002665 ) ) ;
#86926 = CARTESIAN_POINT ( 'NONE',  ( 1.472469842513823179, 20.59226448433411960, -4.923371831947296329 ) ) ;
#86927 = CARTESIAN_POINT ( 'NONE',  ( -7.371420888394233373, -73.25401859617250011, 4.000000000000000888 ) ) ;
#86928 = CARTESIAN_POINT ( 'NONE',  ( 17.96484262340118221, 9.938685344154839285, 7.964842623401181321 ) ) ;
#86929 = CARTESIAN_POINT ( 'NONE',  ( -1.114591949025129258, 15.00000000000000000, 14.45709807627963706 ) ) ;
#86930 = CARTESIAN_POINT ( 'NONE',  ( 17.96484262340118221, 44.93868534415483396, 7.964842623401181321 ) ) ;
#86931 = CARTESIAN_POINT ( 'NONE',  ( -0.8801773607111009756, 33.06368534415484106, 1.068504757029289695E-15 ) ) ;
#86932 = CARTESIAN_POINT ( 'NONE',  ( 0.1532563361054083140, 66.00893115100079456, 1.131784320476157264E-15 ) ) ;
#86933 = CARTESIAN_POINT ( 'NONE',  ( 5.076628168052703671, 66.84226448433412315, 8.527530157486179263 ) ) ;
#86934 = CARTESIAN_POINT ( 'NONE',  ( -42.50369195530268485, 107.9060299417078426, -5.000000000000000888 ) ) ;
#86935 = CARTESIAN_POINT ( 'NONE',  ( 19.84674366389459266, 8.300597817667451750, 2.638427012816836559 ) ) ;
#86936 = VERTEX_POINT ( 'NONE', #4738 ) ;
#86937 = AXIS2_PLACEMENT_3D ( 'NONE', #18342, #48821, #38885 ) ;
#86938 = CARTESIAN_POINT ( 'NONE',  ( 7.084665262690076126, 27.02201867748817676, -10.88017736071110164 ) ) ;
#86939 = CARTESIAN_POINT ( 'NONE',  ( 0.6178305044545818747, 28.49863466993041783, -9.382169495545419124 ) ) ;
#86940 = EDGE_CURVE ( 'NONE', #95286, #45739, #94903, .T. ) ;
#86941 = CARTESIAN_POINT ( 'NONE',  ( 1.472469842513823179, 56.42559781766745886, 4.923371831947296329 ) ) ;
#86942 = CARTESIAN_POINT ( 'NONE',  ( 0.5774900079438590739, 62.64701867748817676, -5.440088680355550821 ) ) ;
#86943 = CARTESIAN_POINT ( 'NONE',  ( 10.00000000000000000, 14.75893115100078568, -9.846743663894594434 ) ) ;
#86944 = CARTESIAN_POINT ( 'NONE',  ( 19.38216949554541202, 35.99863466993041072, 9.382169495545424454 ) ) ;
#86945 = CARTESIAN_POINT ( 'NONE',  ( 17.20831665107776587, 4.133931151000785675, -7.208316651077762316 ) ) ;
#86946 = ORIENTED_EDGE ( 'NONE', *, *, #68204, .T. ) ;
#86947 = CARTESIAN_POINT ( 'NONE',  ( 3.420591144908486481, 14.49999999999999112, 14.60477854057964109 ) ) ;
#86948 =( NAMED_UNIT ( * ) PLANE_ANGLE_UNIT ( ) SI_UNIT ( $, .RADIAN. ) );
#86950 = CARTESIAN_POINT ( 'NONE',  ( -4.164238869374099927, 27.01208216824730357, 3.795296366450308767 ) ) ;
#86949 = CARTESIAN_POINT ( 'NONE',  ( 19.38216949554541202, 60.99863466993042493, 9.382169495545424454 ) ) ;
#86951 = CARTESIAN_POINT ( 'NONE',  ( 19.84674366389459266, 18.71726448433411960, -2.638427012816827677 ) ) ;
#86952 = CARTESIAN_POINT ( 'NONE',  ( 10.00000000000000000, 6.813685344154838397, -10.88017736071110342 ) ) ;
#86953 = CARTESIAN_POINT ( 'NONE',  ( 10.00000000000000178, 27.25893115100078390, 9.846743663894594434 ) ) ;
#86954 = CARTESIAN_POINT ( 'NONE',  ( 2.917880565312948704, 52.63708216824730357, 12.26659068614894643 ) ) ;
#86955 = ORIENTED_EDGE ( 'NONE', *, *, #41970, .F. ) ;
#86956 = CARTESIAN_POINT ( 'NONE',  ( 7.084665262690076126, 9.105352010821503583, 10.88017736071109987 ) ) ;
#86957 = CARTESIAN_POINT ( 'NONE',  ( -0.8801773607110991993, 17.85535201082150536, -2.915334737309923874 ) ) ;
#86958 = CARTESIAN_POINT ( 'NONE',  ( 0.1532563361054083140, 16.00893115100078390, 1.131784320476157264E-15 ) ) ;
#86959 = ORIENTED_EDGE ( 'NONE', *, *, #21122, .F. ) ;
#86960 = CARTESIAN_POINT ( 'NONE',  ( 12.60874940350942985, 3.897725180921639224E-16, 7.160268045227119238 ) ) ;
#86961 = CARTESIAN_POINT ( 'NONE',  ( 2.035157376598824452, 23.68868534415484461, 7.964842623401179544 ) ) ;
#86962 = CARTESIAN_POINT ( 'NONE',  ( 18.52753015748617571, 58.09226448433411605, 4.923371831947298993 ) ) ;
#86963 = DIRECTION ( 'NONE',  ( 0.000000000000000000, 0.000000000000000000, 1.000000000000000000 ) ) ;
#86964 = CARTESIAN_POINT ( 'NONE',  ( -0.8801773607111009756, 68.27201867748817676, 2.915334737309923874 ) ) ;
#86966 = CARTESIAN_POINT ( 'NONE',  ( 13.79529636645031943, 25.34541550158063572, -14.16423886937409904 ) ) ;
#86965 = PRESENTATION_LAYER_ASSIGNMENT (  '', '', ( #23104 ) ) ;
#86967 = CARTESIAN_POINT ( 'NONE',  ( 2.035157376598824452, 43.68868534415484106, 7.964842623401179544 ) ) ;
#86968 = CARTESIAN_POINT ( 'NONE',  ( 19.42250999205614193, 15.14701867748817143, 5.440088680355555262 ) ) ;
#86969 = CARTESIAN_POINT ( 'NONE',  ( 10.00000000000000178, 52.25893115100078745, 9.846743663894594434 ) ) ;
#86970 = PRESENTATION_LAYER_ASSIGNMENT (  '', '', ( #61406 ) ) ;
#86971 = CARTESIAN_POINT ( 'NONE',  ( -9.208505132027131168, -19.73424747731175088, -3.750000000000000444 ) ) ;
#86972 = CARTESIAN_POINT ( 'NONE',  ( 5.076628168052703671, 41.84226448433411605, 8.527530157486179263 ) ) ;
#86973 = AXIS2_PLACEMENT_3D ( 'NONE', #56549, #63544, #9080 ) ;
#86974 = DIRECTION ( 'NONE',  ( 0.000000000000000000, 0.000000000000000000, 1.000000000000000000 ) ) ;
#86975 = CARTESIAN_POINT ( 'NONE',  ( 19.84674366389459621, 13.50893115100078568, 7.409399052514197653E-17 ) ) ;
#86976 = CARTESIAN_POINT ( 'NONE',  ( -3.434112377981047626, -34.83469866340291077, 12.81628187352647963 ) ) ;
#86977 = VERTEX_POINT ( 'NONE', #51211 ) ;
#86978 = EDGE_CURVE ( 'NONE', #2021, #35739, #88709, .T. ) ;
#86979 = CARTESIAN_POINT ( 'NONE',  ( 15.44008868035555793, 11.39701867748817143, -9.422509992056140149 ) ) ;
#86980 = CARTESIAN_POINT ( 'NONE',  ( 2.791683348922240793, 6.633931151000785675, 7.208316651077764092 ) ) ;
#86981 = CARTESIAN_POINT ( 'NONE',  ( 2.791683348922240793, 66.63393115100079456, 7.208316651077764092 ) ) ;
#86983 = CARTESIAN_POINT ( 'NONE',  ( 4.559911319644449179, 48.89701867748817676, 9.422509992056141925 ) ) ;
#86982 = CARTESIAN_POINT ( 'NONE',  ( -0.8801773607111009756, 43.06368534415484106, 1.068504757029289695E-15 ) ) ;
#86985 = CARTESIAN_POINT ( 'NONE',  ( 10.00000000000000178, 50.37363466993042493, 12.81628187352647608 ) ) ;
#86984 = CARTESIAN_POINT ( 'NONE',  ( 17.96484262340118221, 19.93868534415484106, 7.964842623401181321 ) ) ;
#86986 = CARTESIAN_POINT ( 'NONE',  ( 17.08211943468705840, 35.13708216824730357, -12.26659068614894466 ) ) ;
#86987 = EDGE_CURVE ( 'NONE', #60992, #1556, #29707, .T. ) ;
#86988 = CARTESIAN_POINT ( 'NONE',  ( 21.92686044187657046, 12.39664270246084321, -3.195792623639524432 ) ) ;
#86989 = AXIS2_PLACEMENT_3D ( 'NONE', #18804, #78309, #86808 ) ;
#86990 = CARTESIAN_POINT ( 'NONE',  ( 6.565887622018943937, 63.08196800326376064, -12.81628187352647608 ) ) ;
#86991 = ORIENTED_EDGE ( 'NONE', *, *, #7243, .F. ) ;
#86992 = CARTESIAN_POINT ( 'NONE',  ( 19.84674366389459266, 63.71726448433412315, -2.638427012816827677 ) ) ;
#86993 = CARTESIAN_POINT ( 'NONE',  ( -0.1503990784575328643, 15.12777174578612538, 6.262539305110068177 ) ) ;
#86994 = CARTESIAN_POINT ( 'NONE',  ( 12.91533473730993009, 36.60535201082151247, -10.88017736071109987 ) ) ;
#86995 = EDGE_CURVE ( 'NONE', #62224, #2288, #76047, .T. ) ;
#86996 = EDGE_LOOP ( 'NONE', ( #7800, #5677, #3613, #47238 ) ) ;
#86998 = CARTESIAN_POINT ( 'NONE',  ( 14.97687855664609202, 14.63595249122789177, -0.8325315005900555398 ) ) ;
#86997 = CARTESIAN_POINT ( 'NONE',  ( 2.791683348922240793, 1.633931151000784565, 7.208316651077764092 ) ) ;
#86999 = CARTESIAN_POINT ( 'NONE',  ( -0.1491070598754174470, 61.94583914210339515, 4.500000000000000888 ) ) ;
#87000 = CARTESIAN_POINT ( 'NONE',  ( 14.92337183194729988, 29.34226448433411960, -8.527530157486177487 ) ) ;
#87001 = CARTESIAN_POINT ( 'NONE',  ( 2.791683348922240793, 16.63393115100078745, 7.208316651077764092 ) ) ;
#87003 = CARTESIAN_POINT ( 'NONE',  ( -4.850097797904361130, 0.04962897333335897221, 13.93319274793799600 ) ) ;
#87002 = CARTESIAN_POINT ( 'NONE',  ( 0.5774900079438590739, 62.64701867748817676, -5.440088680355550821 ) ) ;
#87004 = CARTESIAN_POINT ( 'NONE',  ( 0.5774900079438607392, 58.48035201082151247, 5.440088680355550821 ) ) ;
#87006 = EDGE_LOOP ( 'NONE', ( #10146, #40337, #38957, #31033 ) ) ;
#87005 = CARTESIAN_POINT ( 'NONE',  ( 18.52753015748617571, 23.09226448433411960, 4.923371831947298993 ) ) ;
#87007 = DIRECTION ( 'NONE',  ( -0.000000000000000000, -0.000000000000000000, -1.000000000000000000 ) ) ;
#87008 = CARTESIAN_POINT ( 'NONE',  ( 0.1532563361054083140, 51.00893115100078745, 1.131784320476157264E-15 ) ) ;
#87009 = ORIENTED_EDGE ( 'NONE', *, *, #42450, .F. ) ;
#87010 = ORIENTED_EDGE ( 'NONE', *, *, #76713, .T. ) ;
#87011 = CARTESIAN_POINT ( 'NONE',  ( 0.000000000000000000, 15.00000000000000000, 0.000000000000000000 ) ) ;
#87012 = CARTESIAN_POINT ( 'NONE',  ( 20.36894250292379738, 4.928748834913967869, -10.36894250292379027 ) ) ;
#87013 = CARTESIAN_POINT ( 'NONE',  ( 19.72487221294570858, 70.00000000000000000, -6.000000000000000000 ) ) ;
#87014 = SURFACE_STYLE_USAGE ( .BOTH. , #70054 ) ;
#87015 = CARTESIAN_POINT ( 'NONE',  ( -4.164238869374099039, 36.80374883491396787, 8.674139862899312516E-16 ) ) ;
#87016 = SURFACE_STYLE_FILL_AREA ( #27003 ) ;
#87017 = CARTESIAN_POINT ( 'NONE',  ( 7.084665262690076126, 39.10535201082150536, 10.88017736071109987 ) ) ;
#87018 = VERTEX_POINT ( 'NONE', #13207 ) ;
#87019 = CARTESIAN_POINT ( 'NONE',  ( 2.791683348922237240, 15.38393115100078212, -7.208316651077763204 ) ) ;
#87021 = CARTESIAN_POINT ( 'NONE',  ( 17.20831665107776587, 12.88393115100078390, 7.208316651077764980 ) ) ;
#87020 = CARTESIAN_POINT ( 'NONE',  ( 7.084665262690076126, 54.10535201082151247, 10.88017736071109987 ) ) ;
#87022 = CARTESIAN_POINT ( 'NONE',  ( 10.00000000000000178, 45.37363466993041783, 12.81628187352647608 ) ) ;
#87023 = CARTESIAN_POINT ( 'NONE',  ( 1.472469842513823179, 31.42559781766745530, 4.923371831947296329 ) ) ;
#87024 = CARTESIAN_POINT ( 'NONE',  ( 17.39651004071838969, 59.08210964143329846, -6.500000000000027534 ) ) ;
#87026 = ADVANCED_FACE ( 'NONE', ( #4246 ), #51711, .F. ) ;
#87025 = CARTESIAN_POINT ( 'NONE',  ( 17.96484262340118221, 54.93868534415484106, 7.964842623401181321 ) ) ;
#87027 = CARTESIAN_POINT ( 'NONE',  ( 16.40814093676323893, 25.79030133659708923, 11.09922568453595026 ) ) ;
#87028 = CARTESIAN_POINT ( 'NONE',  ( -14.16423886937410082, -33.19625116508603213, 4.336808689942017736E-15 ) ) ;
#87029 = CARTESIAN_POINT ( 'NONE',  ( 0.1532563361054082862, 26.21726448433411605, 2.638427012816831674 ) ) ;
#87030 = CARTESIAN_POINT ( 'NONE',  ( 10.00000000000000178, 18.05374883491396787, 14.16423886937410082 ) ) ;
#87031 = AXIS2_PLACEMENT_3D ( 'NONE', #82219, #28232, #49743 ) ;
#87032 = VERTEX_POINT ( 'NONE', #66201 ) ;
#87033 = EDGE_CURVE ( 'NONE', #75712, #53231, #62345, .T. ) ;
#87034 = PRESENTATION_LAYER_ASSIGNMENT (  '', '', ( #63121 ) ) ;
#87035 = CARTESIAN_POINT ( 'NONE',  ( -0.8801773607111009756, 38.06368534415484106, 1.068504757029289695E-15 ) ) ;
#87036 = CARTESIAN_POINT ( 'NONE',  ( -0.8801773607111009756, 53.06368534415484106, 1.068504757029289695E-15 ) ) ;
#87037 = CARTESIAN_POINT ( 'NONE',  ( 2.917880565312950480, 30.97041550158063572, -12.26659068614894821 ) ) ;
#87038 = CARTESIAN_POINT ( 'NONE',  ( 12.63842701281683922, 49.55059781766744464, -9.846743663894590881 ) ) ;
#87039 =( BOUNDED_CURVE ( )  B_SPLINE_CURVE ( 2, ( #14793, #75760, #61730, #82269, #74776, #92248, #52273, #76262, #37293, #82771, #15771, #38274, #97810 ),
 .UNSPECIFIED., .F., .F. ) 
 B_SPLINE_CURVE_WITH_KNOTS ( ( 3, 2, 2, 2, 2, 2, 3 ),
 ( 0.5666666666666666519, 0.5722222222222221877, 0.5777777777777777235, 0.5833333333333333703, 0.5888888888888889062, 0.5944444444444444420, 0.5999999999999999778 ),
 .UNSPECIFIED. ) 
 CURVE ( )  GEOMETRIC_REPRESENTATION_ITEM ( )  RATIONAL_B_SPLINE_CURVE ( ( 1.000000000000000000, 0.9659258262890683122, 1.000000000000000000, 0.9659258262890683122, 1.000000000000000000, 0.9659258262890683122, 1.000000000000000000, 0.9659258262890683122, 1.000000000000000000, 0.9659258262890683122, 1.000000000000000000, 0.9659258262890683122, 1.000000000000000000 ) ) 
 REPRESENTATION_ITEM ( '' )  );
#87040 = CARTESIAN_POINT ( 'NONE',  ( 17.20831665107776587, 12.88393115100078390, 7.208316651077764980 ) ) ;
#87042 = DIRECTION ( 'NONE',  ( -1.000000000000000000, 0.000000000000000000, 0.000000000000000000 ) ) ;
#87041 = CARTESIAN_POINT ( 'NONE',  ( 13.82192141328807011, 15.00000000000000000, 4.382292601468777526 ) ) ;
#87043 = CARTESIAN_POINT ( 'NONE',  ( 20.88017736071110875, 45.77201867748816966, -2.915334737309920765 ) ) ;
#87044 = CARTESIAN_POINT ( 'NONE',  ( 3.799999999999998934, 1.639999999999999014, 4.653657836759941744E-16 ) ) ;
#87045 = CARTESIAN_POINT ( 'NONE',  ( -1.099225684535947600, 23.70696800326375708, -6.408140936763238038 ) ) ;
#87046 = CARTESIAN_POINT ( 'NONE',  ( 18.52753015748617571, 48.09226448433412315, 4.923371831947298993 ) ) ;
#87047 = CARTESIAN_POINT ( 'NONE',  ( -9.422509992056145478, 12.64701867748818032, -5.440088680355541939 ) ) ;
#87048 = CARTESIAN_POINT ( 'NONE',  ( -0.8801773607111008646, 3.272018677488171434, 2.915334737309923430 ) ) ;
#87049 = EDGE_CURVE ( 'NONE', #39787, #63379, #58398, .T. ) ;
#87051 = DIRECTION ( 'NONE',  ( 0.000000000000000000, 1.000000000000000000, 0.000000000000000000 ) ) ;
#87050 = CARTESIAN_POINT ( 'NONE',  ( -11.62006642627350672, -3.693487166502375051E-15, -8.881585844847300848 ) ) ;
#87052 = CARTESIAN_POINT ( 'NONE',  ( -13.61464873478158211, 0.5000000000000004441, -6.296136897218027606 ) ) ;
#87053 = CARTESIAN_POINT ( 'NONE',  ( 1.816707512666851265, 15.10290668512023338, -6.499999999999988454 ) ) ;
#87054 = CARTESIAN_POINT ( 'NONE',  ( 15.44008868035555260, 64.73035201082151957, 9.422509992056143702 ) ) ;
#87055 = CARTESIAN_POINT ( 'NONE',  ( 7.084665262690076126, 59.10535201082150536, 10.88017736071109987 ) ) ;
#87056 = AXIS2_PLACEMENT_3D ( 'NONE', #11495, #40536, #48012 ) ;
#87058 = EDGE_CURVE ( 'NONE', #38990, #71998, #51559, .T. ) ;
#87057 = CARTESIAN_POINT ( 'NONE',  ( 0.2751277870542871984, 68.21833443783938833, 6.499999999999984901 ) ) ;
#87059 = CARTESIAN_POINT ( 'NONE',  ( 18.52753015748618282, 23.92559781766745530, -4.923371831947291888 ) ) ;
#87060 = CARTESIAN_POINT ( 'NONE',  ( 20.88017736071110519, 20.56368534415484106, 2.639326808657452039E-16 ) ) ;
#87061 = CARTESIAN_POINT ( 'NONE',  ( 12.63842701281683922, 64.55059781766745175, -9.846743663894590881 ) ) ;
#87063 = CARTESIAN_POINT ( 'NONE',  ( -7.116235062956296709, -80.68325857818734903, -3.749999999999999556 ) ) ;
#87062 = CARTESIAN_POINT ( 'NONE',  ( 20.88017736071110519, 20.56368534415484106, 2.639326808657452039E-16 ) ) ;
#87064 = CARTESIAN_POINT ( 'NONE',  ( 45.14529252227820422, 61.69856644711347826, -8.000000000000000000 ) ) ;
#87065 = CARTESIAN_POINT ( 'NONE',  ( 22.81628187352647785, 41.62363466993042493, 6.195893100308588602E-16 ) ) ;
#87066 = ORIENTED_EDGE ( 'NONE', *, *, #40200, .T. ) ;
#87067 = CARTESIAN_POINT ( 'NONE',  ( 0.5774900079438590739, 47.64701867748817676, -5.440088680355550821 ) ) ;
#87068 = EDGE_CURVE ( 'NONE', #61681, #24281, #68685, .T. ) ;
#87070 = CARTESIAN_POINT ( 'NONE',  ( 20.15039907845753220, 51.74884699246889852, 6.262539305110077059 ) ) ;
#87069 = CARTESIAN_POINT ( 'NONE',  ( 22.81628187352648496, 26.83196800326374998, -3.434112377981050290 ) ) ;
#87071 = CARTESIAN_POINT ( 'NONE',  ( 4.559911319644449179, 23.89701867748817321, 9.422509992056141925 ) ) ;
#87072 = CARTESIAN_POINT ( 'NONE',  ( 22.26659068614894466, 53.88708216824731068, 7.082119434687054849 ) ) ;
#87073 = CARTESIAN_POINT ( 'NONE',  ( 10.00000000000000000, 44.75893115100078745, -9.846743663894594434 ) ) ;
#87074 = CARTESIAN_POINT ( 'NONE',  ( 0.1532563361054100626, 5.800597817667452638, -2.638427012816831230 ) ) ;
#87075 = CARTESIAN_POINT ( 'NONE',  ( 17.96484262340118221, 49.93868534415484106, 7.964842623401181321 ) ) ;
#87076 = LINE ( 'NONE', #19564, #4351 ) ;
#87077 = CARTESIAN_POINT ( 'NONE',  ( -0.3689425029237898834, 16.17874883491396076, -10.36894250292378850 ) ) ;
#87078 = CARTESIAN_POINT ( 'NONE',  ( -5.999999999999994671, 43.00000000000000000, 6.500000000000000888 ) ) ;
#87079 = CARTESIAN_POINT ( 'NONE',  ( 12.60589901313221439, 15.00000000000000000, -8.129656208642048298 ) ) ;
#87080 = ORIENTED_EDGE ( 'NONE', *, *, #51720, .F. ) ;
#87081 = CARTESIAN_POINT ( 'NONE',  ( 24.16423886937410614, 44.30374883491397497, 8.672049930838204340E-16 ) ) ;
#87082 = CARTESIAN_POINT ( 'NONE',  ( -0.3689425029237898834, 51.17874883491397497, -10.36894250292378850 ) ) ;
#87083 = CARTESIAN_POINT ( 'NONE',  ( 18.52753015748618282, 18.92559781766745175, -4.923371831947291888 ) ) ;
#87085 = CARTESIAN_POINT ( 'NONE',  ( 6.565887622018943937, 13.08196800326374998, -12.81628187352647608 ) ) ;
#87084 = AXIS2_PLACEMENT_3D ( 'NONE', #4180, #89142, #42663 ) ;
#87086 = DIRECTION ( 'NONE',  ( 1.257568779154408793E-17, 1.000000000000000000, -0.000000000000000000 ) ) ;
#87087 = DIRECTION ( 'NONE',  ( -0.06975647374412567714, -0.9975640502598243087, 0.000000000000000000 ) ) ;
#87089 = CARTESIAN_POINT ( 'NONE',  ( 13.43411237798105340, 30.58196800326374998, 12.81628187352647963 ) ) ;
#87088 = CARTESIAN_POINT ( 'NONE',  ( 7.084665262690076126, 4.105352010821503583, 10.88017736071109987 ) ) ;
#87090 = CARTESIAN_POINT ( 'NONE',  ( 2.917880565312948704, 47.63708216824730357, 12.26659068614894643 ) ) ;
#87091 = DIRECTION ( 'NONE',  ( 0.000000000000000000, -1.000000000000000000, 0.000000000000000000 ) ) ;
#87092 = CARTESIAN_POINT ( 'NONE',  ( 12.91533473730992121, 64.52201867748817676, 10.88017736071110164 ) ) ;
#87093 = CARTESIAN_POINT ( 'NONE',  ( -9.846743663894594434, 1.008931151000792781, 3.469446951953614189E-15 ) ) ;
#87094 = ORIENTED_EDGE ( 'NONE', *, *, #33204, .F. ) ;
#87095 = CARTESIAN_POINT ( 'NONE',  ( 0.1532563361054100626, 20.80059781766744464, -2.638427012816831230 ) ) ;
#87096 = VERTEX_POINT ( 'NONE', #76666 ) ;
#87098 = CARTESIAN_POINT ( 'NONE',  ( 20.88017736071110875, 10.77201867748817143, -2.915334737309920765 ) ) ;
#87097 = CARTESIAN_POINT ( 'NONE',  ( 7.084665262690076126, 2.022018677488171434, -10.88017736071110164 ) ) ;
#87100 = CARTESIAN_POINT ( 'NONE',  ( 10.00000000000000178, 67.25893115100079456, 9.846743663894594434 ) ) ;
#87099 = CARTESIAN_POINT ( 'NONE',  ( 10.00000000000000178, 47.25893115100078745, 9.846743663894594434 ) ) ;
#87101 = CARTESIAN_POINT ( 'NONE',  ( 14.17193700899789022, -0.03417435944610275333, 1.489530601564113654 ) ) ;
#87102 = EDGE_CURVE ( 'NONE', #97319, #39036, #16174, .T. ) ;
#87104 = CARTESIAN_POINT ( 'NONE',  ( 22.81628187352647785, 21.41530133659708923, 3.434112377981063169 ) ) ;
#87103 = CIRCLE ( 'NONE', #34418, 0.5000000000000000000 ) ;
#87105 = VERTEX_POINT ( 'NONE', #14212 ) ;
#87106 = CARTESIAN_POINT ( 'NONE',  ( 2.917880565312948704, 57.63708216824731068, 12.26659068614894643 ) ) ;
#87107 = VERTEX_POINT ( 'NONE', #214 ) ;
#87108 = CARTESIAN_POINT ( 'NONE',  ( 2.917880565312950480, 55.97041550158063217, -12.26659068614894821 ) ) ;
#87109 = VERTEX_POINT ( 'NONE', #30664 ) ;
#87110 = CARTESIAN_POINT ( 'NONE',  ( 12.91533473730993009, 31.60535201082150891, -10.88017736071109987 ) ) ;
#87111 = CARTESIAN_POINT ( 'NONE',  ( 7.084665262690076126, 42.02201867748816966, -10.88017736071110164 ) ) ;
#87112 = SURFACE_STYLE_USAGE ( .BOTH. , #42606 ) ;
#87113 = CARTESIAN_POINT ( 'NONE',  ( 19.42250999205614548, 25.98035201082150891, -5.440088680355545492 ) ) ;
#87114 = DIRECTION ( 'NONE',  ( 0.000000000000000000, -1.000000000000000000, 0.000000000000000000 ) ) ;
#87115 = AXIS2_PLACEMENT_3D ( 'NONE', #94161, #79160, #39216 ) ;
#87116 = CARTESIAN_POINT ( 'NONE',  ( 0.1532563361054100626, 15.80059781766745353, -2.638427012816831230 ) ) ;
#87117 = ORIENTED_EDGE ( 'NONE', *, *, #14262, .T. ) ;
#87118 = CARTESIAN_POINT ( 'NONE',  ( 11.20666413564249453, -56.81049121600103291, 3.750000000000000000 ) ) ;
#87119 = CARTESIAN_POINT ( 'NONE',  ( 7.361572987183170547, 47.05059781766745175, 9.846743663894590881 ) ) ;
#87120 = CARTESIAN_POINT ( 'NONE',  ( 14.71525861348289865, 15.00000000000000000, -2.908807992686582633 ) ) ;
#87121 = CARTESIAN_POINT ( 'NONE',  ( 22.81628187352647785, 56.41530133659708213, 3.434112377981063169 ) ) ;
#87122 = EDGE_CURVE ( 'NONE', #90793, #54280, #25366, .T. ) ;
#87123 = DIRECTION ( 'NONE',  ( 0.000000000000000000, 1.000000000000000000, 0.000000000000000000 ) ) ;
#87124 = CARTESIAN_POINT ( 'NONE',  ( 0.1532563361054082862, 66.21726448433413736, 2.638427012816831674 ) ) ;
#87125 = CARTESIAN_POINT ( 'NONE',  ( 6.204703633549690345, 47.84541550158064638, 14.16423886937410082 ) ) ;
#87126 = CARTESIAN_POINT ( 'NONE',  ( 19.72487221294570858, 5.718334437839381224, -6.500000000000000888 ) ) ;
#87127 = ORIENTED_EDGE ( 'NONE', *, *, #84746, .T. ) ;
#87128 = FACE_OUTER_BOUND ( 'NONE', #20867, .T. ) ;
#87129 = CARTESIAN_POINT ( 'NONE',  ( 19.84674366389459266, 28.71726448433411960, -2.638427012816827677 ) ) ;
#87130 = CARTESIAN_POINT ( 'NONE',  ( -7.771322705638593398, 15.00000000000000000, 12.24159072200411380 ) ) ;
#87131 = CARTESIAN_POINT ( 'NONE',  ( 6.565887622018943937, 0.1653013365970866511, 12.81628187352647430 ) ) ;
#87132 = CARTESIAN_POINT ( 'NONE',  ( 15.44008868035555793, 66.39701867748817676, -9.422509992056140149 ) ) ;
#87133 = CARTESIAN_POINT ( 'NONE',  ( -1.820328553599896981, 0.000000000000000000, -5.140449258537809207 ) ) ;
#87134 = CARTESIAN_POINT ( 'NONE',  ( 14.92337183194729633, 52.67559781766745175, 8.527530157486181039 ) ) ;
#87135 = CIRCLE ( 'NONE', #86937, 0.4999999999999995559 ) ;
#87136 = EDGE_CURVE ( 'NONE', #55430, #32382, #31157, .T. ) ;
#87137 = EDGE_CURVE ( 'NONE', #89183, #74673, #2566, .T. ) ;
#87138 = ORIENTED_EDGE ( 'NONE', *, *, #64037, .F. ) ;
#87139 = CARTESIAN_POINT ( 'NONE',  ( 17.08211943468705130, 58.47041550158063927, 12.26659068614894998 ) ) ;
#87140 = LINE ( 'NONE', #55678, #35204 ) ;
#87141 = CARTESIAN_POINT ( 'NONE',  ( 0.5774900079438607392, 43.48035201082151247, 5.440088680355550821 ) ) ;
#87143 = CARTESIAN_POINT ( 'NONE',  ( 10.00000000000000178, 64.31368534415483396, 10.88017736071110342 ) ) ;
#87142 = CARTESIAN_POINT ( 'NONE',  ( 6.565887622018943937, 20.16530133659708213, 12.81628187352647430 ) ) ;
#87144 = CARTESIAN_POINT ( 'NONE',  ( 7.084665262690076126, 2.022018677488170990, -10.88017736071110164 ) ) ;
#87145 = DIRECTION ( 'NONE',  ( 0.000000000000000000, 0.000000000000000000, 1.000000000000000000 ) ) ;
#87146 = CARTESIAN_POINT ( 'NONE',  ( 19.39235739573469885, 59.87576471608601025, 6.499999999999986677 ) ) ;
#87147 = CARTESIAN_POINT ( 'NONE',  ( 0.1532563361054100626, 45.80059781766745886, -2.638427012816831230 ) ) ;
#87148 =( NAMED_UNIT ( * ) SI_UNIT ( $, .STERADIAN. ) SOLID_ANGLE_UNIT ( ) );
#87149 = CARTESIAN_POINT ( 'NONE',  ( -9.422509992056145478, -22.35298132251182324, -5.440088680355541939 ) ) ;
#87150 = CARTESIAN_POINT ( 'NONE',  ( 16.40814093676324603, 17.45696800326375353, -11.09922568453594671 ) ) ;
#87151 = CARTESIAN_POINT ( 'NONE',  ( -8.218815441141973821, -9.362071622911987134, -4.000000000000000000 ) ) ;
#87153 = CARTESIAN_POINT ( 'NONE',  ( 8.502626202121271959, 0.04922511925147034229, 12.05617882333543633 ) ) ;
#87152 = CARTESIAN_POINT ( 'NONE',  ( -0.8801773607111009756, 28.06368534415484106, 1.068504757029289695E-15 ) ) ;
#87154 = CARTESIAN_POINT ( 'NONE',  ( 18.00000000000000000, 84.07179676972448590, 3.750000000000000000 ) ) ;
#87155 = CARTESIAN_POINT ( 'NONE',  ( 24.16423886937409904, 34.09541550158064638, 3.795296366450317205 ) ) ;
#87156 = CARTESIAN_POINT ( 'NONE',  ( -2.266590686148945544, 27.22041550158063572, 7.082119434687048631 ) ) ;
#87157 = CARTESIAN_POINT ( 'NONE',  ( -0.8801773607111009756, 13.06368534415483929, 1.068504757029289695E-15 ) ) ;
#87158 = AXIS2_PLACEMENT_3D ( 'NONE', #52408, #67413, #82909 ) ;
#87159 = CARTESIAN_POINT ( 'NONE',  ( 14.92337183194729988, 44.34226448433412315, -8.527530157486177487 ) ) ;
#87160 = CARTESIAN_POINT ( 'NONE',  ( 21.09922568453594849, 41.20696800326375353, 6.408140936763242479 ) ) ;
#87161 = CARTESIAN_POINT ( 'NONE',  ( 0.5774900079438607392, 8.480352010821505360, 5.440088680355550821 ) ) ;
#87162 = VECTOR ( 'NONE', #45160, 1000.000000000000000 ) ;
#87163 = CARTESIAN_POINT ( 'NONE',  ( 5.076628168052704559, 40.17559781766745175, -8.527530157486179263 ) ) ;
#87164 = CARTESIAN_POINT ( 'NONE',  ( -0.8801773607110991993, 37.85535201082151247, -2.915334737309923874 ) ) ;
#87165 = CARTESIAN_POINT ( 'NONE',  ( 0.6178305044545818747, 8.498634669930421381, -9.382169495545419124 ) ) ;
#87166 = CARTESIAN_POINT ( 'NONE',  ( -4.164238869374099039, 26.80374883491397142, 8.674139862899312516E-16 ) ) ;
#87167 = FACE_OUTER_BOUND ( 'NONE', #34001, .T. ) ;
#87168 = MECHANICAL_DESIGN_GEOMETRIC_PRESENTATION_REPRESENTATION (  '', ( #5748 ), #53638 ) ;
#87169 = UNCERTAINTY_MEASURE_WITH_UNIT (LENGTH_MEASURE( 1.000000000000000082E-05 ), #814, 'distance_accuracy_value', 'NONE');
#87170 = EDGE_CURVE ( 'NONE', #83825, #26872, #74700, .T. ) ;
#87171 = CARTESIAN_POINT ( 'NONE',  ( 12.63842701281683922, 19.55059781766745175, -9.846743663894590881 ) ) ;
#87172 = CARTESIAN_POINT ( 'NONE',  ( -1.099225684535947600, 54.54030133659708923, 6.408140936763237150 ) ) ;
#87173 = CARTESIAN_POINT ( 'NONE',  ( 14.92337183194729988, 54.34226448433412315, -8.527530157486177487 ) ) ;
#87174 = VERTEX_POINT ( 'NONE', #7198 ) ;
#87175 = ADVANCED_FACE ( 'NONE', ( #37701 ), #84667, .T. ) ;
#87176 = DIRECTION ( 'NONE',  ( 0.000000000000000000, -1.000000000000000000, -0.000000000000000000 ) ) ;
#87177 = CARTESIAN_POINT ( 'NONE',  ( 4.400664535130860422, -1.180071741297640253, 3.750000000000001776 ) ) ;
#87178 = CARTESIAN_POINT ( 'NONE',  ( 20.36894250292379738, 64.92874883491397497, -10.36894250292379027 ) ) ;
#87180 = LINE ( 'NONE', #57170, #46151 ) ;
#87179 = CARTESIAN_POINT ( 'NONE',  ( 13.79529636645030344, 13.26208216824729824, 14.16423886937410614 ) ) ;
#87181 = CARTESIAN_POINT ( 'NONE',  ( 2.791683348922237240, 5.383931151000785675, -7.208316651077763204 ) ) ;
#87182 = CARTESIAN_POINT ( 'NONE',  ( 17.20831665107776587, 47.88393115100078745, 7.208316651077764980 ) ) ;
#87183 = CARTESIAN_POINT ( 'NONE',  ( 19.42250999205614193, 40.14701867748817676, 5.440088680355555262 ) ) ;
#87184 = LINE ( 'NONE', #95172, #9679 ) ;
#87185 = FACE_OUTER_BOUND ( 'NONE', #16391, .T. ) ;
#87186 = VERTEX_POINT ( 'NONE', #15698 ) ;
#87187 = FACE_OUTER_BOUND ( 'NONE', #92923, .T. ) ;
#87188 = EDGE_LOOP ( 'NONE', ( #24958, #65503, #15595, #36605, #77470, #72230 ) ) ;
#87189 = VERTEX_POINT ( 'NONE', #37218 ) ;
#87190 = FACE_OUTER_BOUND ( 'NONE', #45117, .T. ) ;
#87191 = CARTESIAN_POINT ( 'NONE',  ( 13.79529636645031943, 10.34541550158063394, -14.16423886937409904 ) ) ;
#87192 = CARTESIAN_POINT ( 'NONE',  ( 10.00000000000000178, 8.053748834913967869, 14.16423886937410082 ) ) ;
#87193 = CARTESIAN_POINT ( 'NONE',  ( 20.36894250292379738, 39.92874883491396787, -10.36894250292379027 ) ) ;
#87194 = CARTESIAN_POINT ( 'NONE',  ( 10.00000000000000178, 62.25893115100078745, 9.846743663894594434 ) ) ;
#87195 = CARTESIAN_POINT ( 'NONE',  ( 2.791683348922240793, 41.63393115100078745, 7.208316651077764092 ) ) ;
#87196 = FACE_OUTER_BOUND ( 'NONE', #33497, .T. ) ;
#87198 = CARTESIAN_POINT ( 'NONE',  ( 7.361572987183170547, 57.05059781766744464, 9.846743663894590881 ) ) ;
#87197 = CARTESIAN_POINT ( 'NONE',  ( -0.8801773607110991993, 27.85535201082150181, -2.915334737309923874 ) ) ;
#87199 = CARTESIAN_POINT ( 'NONE',  ( -2.266590686148945544, 1.387082168247301128, -7.082119434687050408 ) ) ;
#87200 = CARTESIAN_POINT ( 'NONE',  ( -0.3689425029237898834, 41.17874883491397497, -10.36894250292378850 ) ) ;
#87201 = CARTESIAN_POINT ( 'NONE',  ( 10.00000000000000000, 6.813685344154838397, -10.88017736071110342 ) ) ;
#87202 = CARTESIAN_POINT ( 'NONE',  ( 0.000000000000000000, 0.5000000000000004441, 0.000000000000000000 ) ) ;
#87203 = CARTESIAN_POINT ( 'NONE',  ( 6.715867195167361636, 15.00000000000000000, 12.85095824508331930 ) ) ;
#87204 = CARTESIAN_POINT ( 'NONE',  ( 20.88017736071110875, 65.77201867748817676, -2.915334737309920765 ) ) ;
#87205 = CARTESIAN_POINT ( 'NONE',  ( 19.84674366389459266, 28.71726448433411960, -2.638427012816827677 ) ) ;
#87206 = CARTESIAN_POINT ( 'NONE',  ( -4.923371831947292776, -38.15773551566587685, 8.527530157486181039 ) ) ;
#87207 = VERTEX_POINT ( 'NONE', #69182 ) ;
#87208 = DIRECTION ( 'NONE',  ( -1.000000000000000000, 0.000000000000000000, 0.000000000000000000 ) ) ;
#87209 = ORIENTED_EDGE ( 'NONE', *, *, #19577, .T. ) ;
#87210 = CARTESIAN_POINT ( 'NONE',  ( 1.472469842513823179, 26.42559781766745175, 4.923371831947296329 ) ) ;
#87211 = ORIENTED_EDGE ( 'NONE', *, *, #87350, .T. ) ;
#87212 = TOROIDAL_SURFACE ( 'NONE', #13779, 14.49999999999999822, 0.5000000000000000000 ) ;
#87213 = CARTESIAN_POINT ( 'NONE',  ( -2.266590686148945544, 31.38708216824730002, -7.082119434687050408 ) ) ;
#87214 = CARTESIAN_POINT ( 'NONE',  ( 5.076628168052704559, 35.17559781766745175, -8.527530157486179263 ) ) ;
#87215 = CARTESIAN_POINT ( 'NONE',  ( 20.88017736071110875, 60.77201867748817676, -2.915334737309920765 ) ) ;
#87216 =( NAMED_UNIT ( * ) SI_UNIT ( $, .STERADIAN. ) SOLID_ANGLE_UNIT ( ) );
#87217 = CARTESIAN_POINT ( 'NONE',  ( 10.00000000000000000, 36.81368534415484106, -10.88017736071110342 ) ) ;
#87218 = CARTESIAN_POINT ( 'NONE',  ( 2.791683348922240793, 46.63393115100077324, 7.208316651077764092 ) ) ;
#87219 = CARTESIAN_POINT ( 'NONE',  ( -9.382169495545413795, -10.25136533006957507, 9.382169495545428006 ) ) ;
#87220 = STYLED_ITEM ( 'NONE', ( #58928 ), #30569 ) ;
#87221 = ORIENTED_EDGE ( 'NONE', *, *, #29070, .F. ) ;
#87222 = CARTESIAN_POINT ( 'NONE',  ( 24.16423886937409904, 14.09541550158063217, 3.795296366450317205 ) ) ;
#87223 = ORIENTED_EDGE ( 'NONE', *, *, #54030, .T. ) ;
#87224 = VERTEX_POINT ( 'NONE', #83189 ) ;
#87225 =( NAMED_UNIT ( * ) PLANE_ANGLE_UNIT ( ) SI_UNIT ( $, .RADIAN. ) );
#87226 = CARTESIAN_POINT ( 'NONE',  ( -1.099225684535947600, 34.54030133659708923, 6.408140936763237150 ) ) ;
#87227 = CARTESIAN_POINT ( 'NONE',  ( 12.63842701281683922, 24.55059781766745175, -9.846743663894590881 ) ) ;
#87228 = CARTESIAN_POINT ( 'NONE',  ( 14.82629065241269473, 0.2301504708692996282, -1.844815641835253928 ) ) ;
#87229 = DIRECTION ( 'NONE',  ( 0.9723699203976742256, 0.000000000000000000, 0.2334453638559156052 ) ) ;
#87230 = CARTESIAN_POINT ( 'NONE',  ( 19.84674366389459266, 23.71726448433412315, -2.638427012816827677 ) ) ;
#87231 = B_SPLINE_CURVE_WITH_KNOTS ( 'NONE', 3,
 ( #71643, #94628, #1689, #26139 ),
 .UNSPECIFIED., .F., .F.,
 ( 4, 4 ),
 ( 7.757919228897728493E-18, 0.002392975128318426507 ),
 .UNSPECIFIED. ) ;
#87232 = ADVANCED_FACE ( 'NONE', ( #52198 ), #52071, .T. ) ;
#87233 = AXIS2_PLACEMENT_3D ( 'NONE', #79782, #41322, #11284 ) ;
#87234 = AXIS2_PLACEMENT_3D ( 'NONE', #9303, #78289, #7845 ) ;
#87235 = CARTESIAN_POINT ( 'NONE',  ( 10.00000000000000000, 61.81368534415484106, -10.88017736071110342 ) ) ;
#87236 = FACE_OUTER_BOUND ( 'NONE', #37780, .T. ) ;
#87237 = DIRECTION ( 'NONE',  ( 0.000000000000000000, 0.000000000000000000, 1.000000000000000000 ) ) ;
#87238 = AXIS2_PLACEMENT_3D ( 'NONE', #64234, #74200, #95745 ) ;
#87239 = CARTESIAN_POINT ( 'NONE',  ( 7.084665262690076126, 69.10535201082151957, 10.88017736071109987 ) ) ;
#87240 = CARTESIAN_POINT ( 'NONE',  ( 22.81628187352647785, 11.62363466993042138, 6.195893100308588602E-16 ) ) ;
#87241 = DIRECTION ( 'NONE',  ( 0.8433914458128849434, 0.000000000000000000, 0.5372996083468249973 ) ) ;
#87242 = CARTESIAN_POINT ( 'NONE',  ( 5.076628168052703671, 41.84226448433411605, 8.527530157486179263 ) ) ;
#87243 = LINE ( 'NONE', #10770, #2644 ) ;
#87244 = CARTESIAN_POINT ( 'NONE',  ( 24.16423886937409904, 14.09541550158063217, 3.795296366450317205 ) ) ;
#87245 = CARTESIAN_POINT ( 'NONE',  ( 12.63842701281683034, 37.46726448433411605, 9.846743663894596210 ) ) ;
#87246 = CARTESIAN_POINT ( 'NONE',  ( 22.81628187352648496, 31.83196800326375353, -3.434112377981050290 ) ) ;
#87248 = DIRECTION ( 'NONE',  ( -1.483861936729427615E-16, 1.000000000000000000, 0.000000000000000000 ) ) ;
#87247 = CARTESIAN_POINT ( 'NONE',  ( 1.707155281725164508, 17.90189080397290056, 6.499999999999992006 ) ) ;
#87249 = CARTESIAN_POINT ( 'NONE',  ( 4.559911319644449179, 67.23035201082150536, -9.422509992056141925 ) ) ;
#87250 = EDGE_CURVE ( 'NONE', #89676, #4865, #61649, .T. ) ;
#87251 = CARTESIAN_POINT ( 'NONE',  ( 6.565887622018943937, 5.165301336597086568, 12.81628187352647430 ) ) ;
#87252 = CARTESIAN_POINT ( 'NONE',  ( 5.500000000000000000, 60.50000000000000000, -5.000000000000000000 ) ) ;
#87253 = CARTESIAN_POINT ( 'NONE',  ( 0.1532563361054083140, 36.00893115100078745, 1.131784320476157264E-15 ) ) ;
#87254 = CARTESIAN_POINT ( 'NONE',  ( 0.5774900079438607392, 28.48035201082150891, 5.440088680355550821 ) ) ;
#87255 = CARTESIAN_POINT ( 'NONE',  ( 22.81628187352648496, 26.83196800326374998, -3.434112377981050290 ) ) ;
#87256 = CIRCLE ( 'NONE', #55367, 2.000000000000001776 ) ;
#87257 = CIRCLE ( 'NONE', #15430, 0.2500000000000002220 ) ;
#87258 = CARTESIAN_POINT ( 'NONE',  ( -11.26637474388419591, 89.93360374965293147, 6.408881440111466432 ) ) ;
#87259 = EDGE_CURVE ( 'NONE', #41402, #37243, #65881, .T. ) ;
#87260 = AXIS2_PLACEMENT_3D ( 'NONE', #82596, #30078, #12615 ) ;
#87261 = CARTESIAN_POINT ( 'NONE',  ( 4.559911319644449179, 33.89701867748817676, 9.422509992056141925 ) ) ;
#87262 = EDGE_CURVE ( 'NONE', #9146, #71617, #47268, .T. ) ;
#87263 = ORIENTED_EDGE ( 'NONE', *, *, #68208, .F. ) ;
#87264 = CARTESIAN_POINT ( 'NONE',  ( 15.44008868035555793, 61.39701867748817676, -9.422509992056140149 ) ) ;
#87265 = CARTESIAN_POINT ( 'NONE',  ( 7.084665262690076126, 4.105352010821503583, 10.88017736071109987 ) ) ;
#87267 = CARTESIAN_POINT ( 'NONE',  ( 10.00000000000000000, 36.81368534415484106, -10.88017736071110342 ) ) ;
#87266 = CARTESIAN_POINT ( 'NONE',  ( 18.52753015748617571, 43.09226448433412315, 4.923371831947298993 ) ) ;
#87268 = CARTESIAN_POINT ( 'NONE',  ( -0.8801773607110991993, 42.85535201082150536, -2.915334737309923874 ) ) ;
#87270 =( LENGTH_UNIT ( ) NAMED_UNIT ( * ) SI_UNIT ( .MILLI., .METRE. ) );
#87269 = CARTESIAN_POINT ( 'NONE',  ( 17.96484262340118221, 16.18868534415483396, -7.964842623401177768 ) ) ;
#87271 = CARTESIAN_POINT ( 'NONE',  ( 19.72487221294570858, 0.000000000000000000, -6.500000000000000888 ) ) ;
#87272 = CARTESIAN_POINT ( 'NONE',  ( 10.00000000000000000, 34.75893115100078745, -9.846743663894594434 ) ) ;
#87274 = CARTESIAN_POINT ( 'NONE',  ( 4.441314631470126173, -2.693011450497559078, 3.749999999999999556 ) ) ;
#87273 = CARTESIAN_POINT ( 'NONE',  ( 24.16423886937410614, 54.30374883491396787, 8.672049930838204340E-16 ) ) ;
#87275 = AXIS2_PLACEMENT_3D ( 'NONE', #72661, #81159, #89156 ) ;
#87276 = LINE ( 'NONE', #24340, #32180 ) ;
#87277 = CARTESIAN_POINT ( 'NONE',  ( 2.917880565312950480, 35.97041550158063217, -12.26659068614894821 ) ) ;
#87278 = DIRECTION ( 'NONE',  ( -0.000000000000000000, -0.000000000000000000, -1.000000000000000000 ) ) ;
#87279 = VERTEX_POINT ( 'NONE', #68200 ) ;
#87280 = CARTESIAN_POINT ( 'NONE',  ( 4.559911319644449179, 2.230352010821504916, -9.422509992056141925 ) ) ;
#87281 = CARTESIAN_POINT ( 'NONE',  ( 14.92337183194729988, 29.34226448433411960, -8.527530157486177487 ) ) ;
#87283 = CARTESIAN_POINT ( 'NONE',  ( -8.669785729375572458, 87.01784090252159842, -4.324025984537457568 ) ) ;
#87282 = LINE ( 'NONE', #78807, #33932 ) ;
#87284 = CARTESIAN_POINT ( 'NONE',  ( 17.96484262340118221, 64.93868534415483396, 7.964842623401181321 ) ) ;
#87285 = CARTESIAN_POINT ( 'NONE',  ( -8.439016546561676435, 15.00000000000000000, -11.79122553965791553 ) ) ;
#87286 = VECTOR ( 'NONE', #62475, 1000.000000000000000 ) ;
#87287 = CARTESIAN_POINT ( 'NONE',  ( 2.035157376598822676, 37.43868534415484106, -7.964842623401177768 ) ) ;
#87288 = CARTESIAN_POINT ( 'NONE',  ( -2.816281873526473856, 64.33196800326376774, 3.434112377981055619 ) ) ;
#87289 = CARTESIAN_POINT ( 'NONE',  ( -2.816281873526471635, 13.91530133659708746, -3.434112377981056508 ) ) ;
#87290 = CARTESIAN_POINT ( 'NONE',  ( 1.472469842513823179, 11.42559781766745175, 4.923371831947296329 ) ) ;
#87291 = ORIENTED_EDGE ( 'NONE', *, *, #59622, .F. ) ;
#87292 =( NAMED_UNIT ( * ) PLANE_ANGLE_UNIT ( ) SI_UNIT ( $, .RADIAN. ) );
#87293 = EDGE_CURVE ( 'NONE', #92445, #21081, #15333, .T. ) ;
#87294 = CARTESIAN_POINT ( 'NONE',  ( 0.2751277870542949144, 4.366073187301309666, -6.499999999999997335 ) ) ;
#87295 = CARTESIAN_POINT ( 'NONE',  ( 22.26659068614894466, 63.88708216824730357, 7.082119434687054849 ) ) ;
#87296 = CARTESIAN_POINT ( 'NONE',  ( 17.08211943468705130, 28.47041550158063572, 12.26659068614894998 ) ) ;
#87297 = CARTESIAN_POINT ( 'NONE',  ( -0.8801773607111008646, 38.27201867748816255, 2.915334737309923430 ) ) ;
#87298 = CARTESIAN_POINT ( 'NONE',  ( 4.559911319644449179, 48.89701867748817676, 9.422509992056141925 ) ) ;
#87299 = CARTESIAN_POINT ( 'NONE',  ( 0.000000000000000000, 15.00000000000000000, 0.000000000000000000 ) ) ;
#87300 = LINE ( 'NONE', #86822, #9766 ) ;
#87301 = CARTESIAN_POINT ( 'NONE',  ( 17.20831665107776587, 9.133931151000787452, -7.208316651077762316 ) ) ;
#87302 =( NAMED_UNIT ( * ) PLANE_ANGLE_UNIT ( ) SI_UNIT ( $, .RADIAN. ) );
#87303 = CARTESIAN_POINT ( 'NONE',  ( 10.00000000000000178, 27.25893115100078390, 9.846743663894594434 ) ) ;
#87304 = CARTESIAN_POINT ( 'NONE',  ( 19.72487221294570858, 56.86607318730075633, 6.500000000000000888 ) ) ;
#87305 = CARTESIAN_POINT ( 'NONE',  ( 4.469999999999999751, 0.000000000000000000, -3.750000000000000000 ) ) ;
#87306 = CARTESIAN_POINT ( 'NONE',  ( 0.1532563361054082862, 26.21726448433411605, 2.638427012816831674 ) ) ;
#87307 = CARTESIAN_POINT ( 'NONE',  ( 5.076628168052703671, 51.84226448433412315, 8.527530157486179263 ) ) ;
#87308 = CARTESIAN_POINT ( 'NONE',  ( 15.44008868035555793, 21.39701867748817321, -9.422509992056140149 ) ) ;
#87309 = EDGE_CURVE ( 'NONE', #86614, #20501, #45685, .T. ) ;
#87310 =( GEOMETRIC_REPRESENTATION_CONTEXT ( 3 ) GLOBAL_UNCERTAINTY_ASSIGNED_CONTEXT ( ( #55197 ) ) GLOBAL_UNIT_ASSIGNED_CONTEXT ( ( #63724, #87702, #18244 ) ) REPRESENTATION_CONTEXT ( 'NONE', 'WORKASPACE' ) );
#87311 = CARTESIAN_POINT ( 'NONE',  ( -1.099225684535947600, 49.54030133659708923, 6.408140936763237150 ) ) ;
#87312 = CARTESIAN_POINT ( 'NONE',  ( 4.559911319644449179, 62.23035201082150536, -9.422509992056141925 ) ) ;
#87313 = CARTESIAN_POINT ( 'NONE',  ( 19.84674366389459621, 28.50893115100078745, 7.409399052514197653E-17 ) ) ;
#87315 = CARTESIAN_POINT ( 'NONE',  ( 5.076628168052704559, 25.17559781766745175, -8.527530157486179263 ) ) ;
#87314 = CARTESIAN_POINT ( 'NONE',  ( 22.26659068614895176, 54.72041550158063217, -7.082119434687042414 ) ) ;
#87316 = FACE_OUTER_BOUND ( 'NONE', #33006, .T. ) ;
#87317 = CIRCLE ( 'NONE', #44194, 15.00000000000000000 ) ;
#87318 = CARTESIAN_POINT ( 'NONE',  ( 19.84674366389459266, 63.71726448433412315, -2.638427012816827677 ) ) ;
#87319 = CARTESIAN_POINT ( 'NONE',  ( 2.917880565312948704, 7.637082168247301794, 12.26659068614894643 ) ) ;
#87320 = CARTESIAN_POINT ( 'NONE',  ( 10.00000000000000000, 30.55374883491397142, -14.16423886937410082 ) ) ;
#87321 = CARTESIAN_POINT ( 'NONE',  ( 17.20831665107776587, 32.88393115100078745, 7.208316651077764980 ) ) ;
#87322 = CARTESIAN_POINT ( 'NONE',  ( -14.94699059465102664, 0.5000000000000004441, 1.259949270174715696 ) ) ;
#87323 = CARTESIAN_POINT ( 'NONE',  ( 7.084665262690076126, 29.10535201082150181, 10.88017736071109987 ) ) ;
#87324 = CARTESIAN_POINT ( 'NONE',  ( -0.8801773607110991993, 62.85535201082150536, -2.915334737309923874 ) ) ;
#87325 = CARTESIAN_POINT ( 'NONE',  ( 7.084665262690076126, 42.02201867748816966, -10.88017736071110164 ) ) ;
#87326 = VERTEX_POINT ( 'NONE', #83686 ) ;
#87327 = CARTESIAN_POINT ( 'NONE',  ( 19.38216949554541202, 40.99863466993042493, 9.382169495545424454 ) ) ;
#87328 = AXIS2_PLACEMENT_3D ( 'NONE', #38749, #7767, #90748 ) ;
#87329 = CARTESIAN_POINT ( 'NONE',  ( -0.8801773607110991993, 47.85535201082150536, -2.915334737309923874 ) ) ;
#87330 = VERTEX_POINT ( 'NONE', #15203 ) ;
#87331 = FILL_AREA_STYLE_COLOUR ( '', #88099 ) ;
#87332 = CIRCLE ( 'NONE', #25127, 0.2499999999999999722 ) ;
#87333 = CARTESIAN_POINT ( 'NONE',  ( -4.250000000000000000, 10.25000000000000000, -3.750000000000000000 ) ) ;
#87334 = VERTEX_POINT ( 'NONE', #76181 ) ;
#87335 = VECTOR ( 'NONE', #69616, 1000.000000000000000 ) ;
#87336 = CARTESIAN_POINT ( 'NONE',  ( -0.8801773607111009756, 68.06368534415484817, 1.068504757029289695E-15 ) ) ;
#87337 = CARTESIAN_POINT ( 'NONE',  ( 15.44008868035555793, 6.397018677488170546, -9.422509992056140149 ) ) ;
#87338 = MECHANICAL_DESIGN_GEOMETRIC_PRESENTATION_REPRESENTATION (  '', ( #10692 ), #49007 ) ;
#87339 = CARTESIAN_POINT ( 'NONE',  ( -5.204170427930422072E-15, 11.41212336850781739, -11.92686044187656513 ) ) ;
#87340 = CARTESIAN_POINT ( 'NONE',  ( -10.44999999999999751, 99.99999999999998579, 8.000000000000000000 ) ) ;
#87341 = CARTESIAN_POINT ( 'NONE',  ( 19.42250999205614548, 10.98035201082150536, -5.440088680355545492 ) ) ;
#87342 = CARTESIAN_POINT ( 'NONE',  ( 0.1532563361054083140, 11.00893115100078568, 1.131784320476157264E-15 ) ) ;
#87343 = CARTESIAN_POINT ( 'NONE',  ( 2.917880565312948704, 2.637082168247300906, 12.26659068614894643 ) ) ;
#87344 = CARTESIAN_POINT ( 'NONE',  ( 0.1532563361054100626, 5.800597817667452638, -2.638427012816831230 ) ) ;
#87345 = CARTESIAN_POINT ( 'NONE',  ( 20.88017736071110519, 5.563685344154837509, 2.639326808657452039E-16 ) ) ;
#87346 = CARTESIAN_POINT ( 'NONE',  ( 10.00000000000000178, 52.25893115100078745, 9.846743663894594434 ) ) ;
#87347 = ORIENTED_EDGE ( 'NONE', *, *, #15317, .F. ) ;
#87348 = CARTESIAN_POINT ( 'NONE',  ( 2.791683348922240793, 51.63393115100078745, 7.208316651077764092 ) ) ;
#87349 = VERTEX_POINT ( 'NONE', #7704 ) ;
#87350 = EDGE_CURVE ( 'NONE', #47878, #1561, #10527, .T. ) ;
#87351 = CARTESIAN_POINT ( 'NONE',  ( -0.8801773607110991993, 57.85535201082149825, -2.915334737309923874 ) ) ;
#87352 = CARTESIAN_POINT ( 'NONE',  ( 17.20831665107776587, 57.88393115100078745, 7.208316651077764980 ) ) ;
#87353 = MECHANICAL_DESIGN_GEOMETRIC_PRESENTATION_REPRESENTATION (  '', ( #95345 ), #57011 ) ;
#87355 = CARTESIAN_POINT ( 'NONE',  ( -9.705452947461587598, 2.500000000000008438, -5.689172442861014645 ) ) ;
#87354 = CARTESIAN_POINT ( 'NONE',  ( 2.035157376598822676, 2.438685344154837953, -7.964842623401177768 ) ) ;
#87356 = CARTESIAN_POINT ( 'NONE',  ( 15.44008868035555793, 61.39701867748817676, -9.422509992056140149 ) ) ;
#87357 = CARTESIAN_POINT ( 'NONE',  ( 4.559911319644449179, 3.897018677488171434, 9.422509992056141925 ) ) ;
#87358 = ADVANCED_FACE ( 'NONE', ( #33610 ), #26134, .F. ) ;
#87359 = CARTESIAN_POINT ( 'NONE',  ( 0.6178305044545818747, 43.49863466993042493, -9.382169495545419124 ) ) ;
#87360 = CARTESIAN_POINT ( 'NONE',  ( 19.42250999205614193, 35.14701867748816966, 5.440088680355555262 ) ) ;
#87361 = CARTESIAN_POINT ( 'NONE',  ( 0.000000000000000000, 0.5000000000000004441, 0.000000000000000000 ) ) ;
#87362 = ORIENTED_EDGE ( 'NONE', *, *, #67090, .F. ) ;
#87363 = CARTESIAN_POINT ( 'NONE',  ( 3.591859063236761518, 44.95696800326376064, 11.09922568453594849 ) ) ;
#87364 = CARTESIAN_POINT ( 'NONE',  ( 17.96484262340118221, 36.18868534415484106, -7.964842623401177768 ) ) ;
#87365 = ORIENTED_EDGE ( 'NONE', *, *, #45729, .T. ) ;
#87366 = LINE ( 'NONE', #94863, #86763 ) ;
#87367 = CARTESIAN_POINT ( 'NONE',  ( 12.63842701281683034, 57.46726448433411605, 9.846743663894596210 ) ) ;
#87369 = CARTESIAN_POINT ( 'NONE',  ( 0.1532563361054082862, 46.21726448433411605, 2.638427012816831674 ) ) ;
#87368 = CARTESIAN_POINT ( 'NONE',  ( 17.20831665107776587, 9.133931151000787452, -7.208316651077762316 ) ) ;
#87370 = CARTESIAN_POINT ( 'NONE',  ( -0.1503990784575287842, 28.10158574516642815, 6.262539305110075283 ) ) ;
#87371 = CARTESIAN_POINT ( 'NONE',  ( -6.732636091893172470, -88.11213685669366669, -4.000000000000000000 ) ) ;
#87372 = CARTESIAN_POINT ( 'NONE',  ( 14.92337183194729633, 37.67559781766745175, 8.527530157486181039 ) ) ;
#87373 = CARTESIAN_POINT ( 'NONE',  ( 13.95806775979399461, 2.168404344971008868E-16, -4.371577651620736304 ) ) ;
#87374 = LINE ( 'NONE', #3392, #27698 ) ;
#87376 = CARTESIAN_POINT ( 'NONE',  ( 1.472469842513823179, 1.425597817667451528, 4.923371831947296329 ) ) ;
#87375 = CARTESIAN_POINT ( 'NONE',  ( 19.84674366389459621, 23.50893115100078390, 7.409399052514197653E-17 ) ) ;
#87377 = CARTESIAN_POINT ( 'NONE',  ( -3.999999999999999112, 1.839999999999999636, 0.000000000000000000 ) ) ;
#87379 = ORIENTED_EDGE ( 'NONE', *, *, #98045, .F. ) ;
#87378 = CARTESIAN_POINT ( 'NONE',  ( 1.472469842513823179, 55.59226448433412315, -4.923371831947296329 ) ) ;
#87380 = EDGE_CURVE ( 'NONE', #88318, #85778, #40648, .T. ) ;
#87381 = CARTESIAN_POINT ( 'NONE',  ( 22.81628187352647785, 21.62363466993041783, 6.195893100308588602E-16 ) ) ;
#87382 = CARTESIAN_POINT ( 'NONE',  ( 1.472469842513823179, 40.59226448433411605, -4.923371831947296329 ) ) ;
#87383 = DIRECTION ( 'NONE',  ( 0.000000000000000000, -1.000000000000000000, 0.000000000000000000 ) ) ;
#87384 = VECTOR ( 'NONE', #70057, 1000.000000000000000 ) ;
#87385 = CARTESIAN_POINT ( 'NONE',  ( 22.26659068614895176, 64.72041550158064638, -7.082119434687042414 ) ) ;
#87386 = CARTESIAN_POINT ( 'NONE',  ( 19.84674366389459266, 23.30059781766745530, 2.638427012816836559 ) ) ;
#87387 = ADVANCED_FACE ( 'NONE', ( #48132 ), #70167, .T. ) ;
#87388 = CARTESIAN_POINT ( 'NONE',  ( -0.1503990784575277295, 39.24884699246889141, -6.262539305110077947 ) ) ;
#87389 = CARTESIAN_POINT ( 'NONE',  ( -4.164238869374098151, 56.59541550158063927, -3.795296366450310543 ) ) ;
#87390 = CARTESIAN_POINT ( 'NONE',  ( 19.84674366389459266, 53.71726448433411605, -2.638427012816827677 ) ) ;
#87391 = CARTESIAN_POINT ( 'NONE',  ( 4.559911319644449179, 3.897018677488171434, 9.422509992056141925 ) ) ;
#87393 = CIRCLE ( 'NONE', #39528, 0.5000000000000004441 ) ;
#87392 = CARTESIAN_POINT ( 'NONE',  ( -0.3689425029237898834, 36.17874883491396787, -10.36894250292378850 ) ) ;
#87394 = CARTESIAN_POINT ( 'NONE',  ( 6.204703633549690345, 45.76208216824729647, -14.16423886937410259 ) ) ;
#87395 = CARTESIAN_POINT ( 'NONE',  ( 0.000000000000000000, 14.49999999999999822, 0.000000000000000000 ) ) ;
#87397 = CARTESIAN_POINT ( 'NONE',  ( 5.076628168052704559, 60.17559781766745175, -8.527530157486179263 ) ) ;
#87396 = CARTESIAN_POINT ( 'NONE',  ( 14.97687855664608314, 15.00000000000000000, -0.8325315005900512100 ) ) ;
#87398 = PRESENTATION_LAYER_ASSIGNMENT (  '', '', ( #2790 ) ) ;
#87399 = VERTEX_POINT ( 'NONE', #78647 ) ;
#87400 = CARTESIAN_POINT ( 'NONE',  ( 15.44008868035555793, 51.39701867748816966, -9.422509992056140149 ) ) ;
#87401 = CARTESIAN_POINT ( 'NONE',  ( 20.00000000000000711, 92.18909449964071712, -4.886738312952714658 ) ) ;
#87402 = CARTESIAN_POINT ( 'NONE',  ( 14.92337183194729988, 54.34226448433412315, -8.527530157486177487 ) ) ;
#87403 = LINE ( 'NONE', #80398, #55429 ) ;
#87404 = B_SPLINE_CURVE_WITH_KNOTS ( 'NONE', 3,
 ( #7737, #46216, #15241, #45222 ),
 .UNSPECIFIED., .F., .F.,
 ( 4, 4 ),
 ( 0.000000000000000000, 0.0004111141682194737997 ),
 .UNSPECIFIED. ) ;
#87405 = CARTESIAN_POINT ( 'NONE',  ( 10.00000000000000178, 57.25893115100078745, 9.846743663894594434 ) ) ;
#87406 = CARTESIAN_POINT ( 'NONE',  ( 0.1532563361054083140, 66.00893115100079456, 1.131784320476157264E-15 ) ) ;
#87407 = CARTESIAN_POINT ( 'NONE',  ( 6.204703633549690345, 20.76208216824730357, -14.16423886937410259 ) ) ;
#87408 = CARTESIAN_POINT ( 'NONE',  ( -14.61146088927471176, 15.00000000000000711, 0.6660010753333497346 ) ) ;
#87409 = CARTESIAN_POINT ( 'NONE',  ( -4.259797195126492575, -13.81744876717405468, -2.750000000000806466 ) ) ;
#87410 = CARTESIAN_POINT ( 'NONE',  ( 4.559911319644449179, 17.23035201082150536, -9.422509992056141925 ) ) ;
#87411 = CARTESIAN_POINT ( 'NONE',  ( 13.43411237798105340, 20.58196800326374643, 12.81628187352647963 ) ) ;
#87412 = DIRECTION ( 'NONE',  ( -1.000000000000000000, 0.000000000000000000, 0.000000000000000000 ) ) ;
#87413 = CARTESIAN_POINT ( 'NONE',  ( 0.1532563361054082862, 11.21726448433411605, 2.638427012816831674 ) ) ;
#87414 = CARTESIAN_POINT ( 'NONE',  ( 5.930070213854097716, -28.64748318935870941, -4.000000000000000000 ) ) ;
#87415 = CARTESIAN_POINT ( 'NONE',  ( 22.26659068614895176, 24.72041550158063572, -7.082119434687042414 ) ) ;
#87416 = DIRECTION ( 'NONE',  ( -0.000000000000000000, -0.000000000000000000, -1.000000000000000000 ) ) ;
#87417 = CARTESIAN_POINT ( 'NONE',  ( 20.15039907845753930, 70.00000000000000000, -6.262539305110068177 ) ) ;
#87418 = CARTESIAN_POINT ( 'NONE',  ( 20.88017736071110875, 5.772018677488170546, -2.915334737309920765 ) ) ;
#87419 = DIRECTION ( 'NONE',  ( 0.000000000000000000, 1.000000000000000000, 0.000000000000000000 ) ) ;
#87420 = DIRECTION ( 'NONE',  ( 0.000000000000000000, 0.000000000000000000, -1.000000000000000000 ) ) ;
#87421 = CARTESIAN_POINT ( 'NONE',  ( 20.88017736071110519, 35.56368534415484106, 2.639326808657452039E-16 ) ) ;
#87422 = CARTESIAN_POINT ( 'NONE',  ( 20.88017736071110164, 40.35535201082150536, 2.915334737309930979 ) ) ;
#87423 = CARTESIAN_POINT ( 'NONE',  ( 17.20831665107776587, 64.13393115100079456, -7.208316651077762316 ) ) ;
#87424 = FILL_AREA_STYLE ('',( #27409 ) ) ;
#87425 = CARTESIAN_POINT ( 'NONE',  ( 1.941103589310612554, 1.227327784520227727, 6.500000000000002665 ) ) ;
#87426 = CARTESIAN_POINT ( 'NONE',  ( 18.52753015748618282, 8.925597817667451750, -4.923371831947291888 ) ) ;
#87427 = ORIENTED_EDGE ( 'NONE', *, *, #1974, .T. ) ;
#87428 = DIRECTION ( 'NONE',  ( -0.000000000000000000, -0.000000000000000000, 1.000000000000000000 ) ) ;
#87429 = CARTESIAN_POINT ( 'NONE',  ( 2.035157376598824452, 48.68868534415483396, 7.964842623401179544 ) ) ;
#87430 = UNCERTAINTY_MEASURE_WITH_UNIT (LENGTH_MEASURE( 1.000000000000000082E-05 ), #37746, 'distance_accuracy_value', 'NONE');
#87431 = CARTESIAN_POINT ( 'NONE',  ( 21.09922568453595559, 12.04030133659708746, -6.408140936763230044 ) ) ;
#87432 = CARTESIAN_POINT ( 'NONE',  ( 7.084665262690076126, 62.02201867748816966, -10.88017736071110164 ) ) ;
#87433 = CARTESIAN_POINT ( 'NONE',  ( 5.076628168052703671, 26.84226448433411960, 8.527530157486179263 ) ) ;
#87434 = AXIS2_PLACEMENT_3D ( 'NONE', #12355, #88358, #50347 ) ;
#87435 = CARTESIAN_POINT ( 'NONE',  ( 10.00000000000000000, 32.87363466993042493, -12.81628187352647608 ) ) ;
#87436 = CARTESIAN_POINT ( 'NONE',  ( 1.472469842513823179, 6.425597817667451750, 4.923371831947296329 ) ) ;
#87437 = VERTEX_POINT ( 'NONE', #17171 ) ;
#87438 = CARTESIAN_POINT ( 'NONE',  ( 18.00000000000000355, 77.07179676972445748, 6.500000000000000888 ) ) ;
#87439 = DIRECTION ( 'NONE',  ( 0.000000000000000000, 1.000000000000000000, 0.000000000000000000 ) ) ;
#87440 = CARTESIAN_POINT ( 'NONE',  ( 15.44008868035555260, 4.730352010821504471, 9.422509992056143702 ) ) ;
#87442 = CARTESIAN_POINT ( 'NONE',  ( -2.266590686148945544, 21.38708216824730357, -7.082119434687050408 ) ) ;
#87441 = CARTESIAN_POINT ( 'NONE',  ( 21.09922568453594849, 56.20696800326375353, 6.408140936763242479 ) ) ;
#87443 = CARTESIAN_POINT ( 'NONE',  ( 19.84674366389459621, 28.50893115100078745, 7.409399052514197653E-17 ) ) ;
#87444 = CARTESIAN_POINT ( 'NONE',  ( -0.8801773607111008646, 3.272018677488171434, 2.915334737309923430 ) ) ;
#87445 = VECTOR ( 'NONE', #90707, 1000.000000000000000 ) ;
#87446 = CARTESIAN_POINT ( 'NONE',  ( 12.91533473730992121, 9.522018677488171434, 10.88017736071110164 ) ) ;
#87447 = ORIENTED_EDGE ( 'NONE', *, *, #84512, .F. ) ;
#87448 = CARTESIAN_POINT ( 'NONE',  ( 15.44008868035555793, 16.39701867748817321, -9.422509992056140149 ) ) ;
#87449 = CARTESIAN_POINT ( 'NONE',  ( 0.5774900079438607392, 23.48035201082150536, 5.440088680355550821 ) ) ;
#87450 = CARTESIAN_POINT ( 'NONE',  ( -5.377205135395773716, 14.76930270348882068, -13.94000429068789160 ) ) ;
#87451 = AXIS2_PLACEMENT_3D ( 'NONE', #43546, #59541, #44038 ) ;
#87452 = VERTEX_POINT ( 'NONE', #69667 ) ;
#87453 = CARTESIAN_POINT ( 'NONE',  ( 5.076628168052703671, 61.84226448433412315, 8.527530157486179263 ) ) ;
#87454 = CARTESIAN_POINT ( 'NONE',  ( 15.44008868035555793, 21.39701867748817321, -9.422509992056140149 ) ) ;
#87455 = CARTESIAN_POINT ( 'NONE',  ( 1.472469842513823179, 61.42559781766745175, 4.923371831947296329 ) ) ;
#87456 = CARTESIAN_POINT ( 'NONE',  ( -6.000000000000000000, 78.07179676972447169, -6.500000000000000888 ) ) ;
#87457 = CARTESIAN_POINT ( 'NONE',  ( 3.591859063236763294, 53.29030133659708923, -11.09922568453595026 ) ) ;
#87458 = CARTESIAN_POINT ( 'NONE',  ( -1.926860441876564023, 4.688309369127507509, 1.004413902775740781E-15 ) ) ;
#87459 = CARTESIAN_POINT ( 'NONE',  ( -2.266590686148945544, 32.22041550158063927, 7.082119434687048631 ) ) ;
#87460 = CARTESIAN_POINT ( 'NONE',  ( 7.084665262690076126, 42.02201867748816966, -10.88017736071110164 ) ) ;
#87461 = CARTESIAN_POINT ( 'NONE',  ( 10.00000000000000178, 19.31368534415484106, 10.88017736071110342 ) ) ;
#87462 = CARTESIAN_POINT ( 'NONE',  ( 0.1532563361054083140, 61.00893115100078745, 1.131784320476157264E-15 ) ) ;
#87463 = CARTESIAN_POINT ( 'NONE',  ( -11.48781033751606095, -88.26659283070991080, -3.750000000000000000 ) ) ;
#87464 = CARTESIAN_POINT ( 'NONE',  ( 5.076628168052704559, 55.17559781766745175, -8.527530157486179263 ) ) ;
#87465 = DIRECTION ( 'NONE',  ( -0.000000000000000000, 1.000000000000000000, -0.000000000000000000 ) ) ;
#87466 = CARTESIAN_POINT ( 'NONE',  ( 5.076628168052703671, 6.842264484334118713, 8.527530157486179263 ) ) ;
#87467 = CARTESIAN_POINT ( 'NONE',  ( 11.09922568453595026, -33.79303199673624647, 6.408140936763232709 ) ) ;
#87468 = CIRCLE ( 'NONE', #47572, 4.250000000000001776 ) ;
#87469 = ORIENTED_EDGE ( 'NONE', *, *, #9279, .F. ) ;
#87470 = CARTESIAN_POINT ( 'NONE',  ( 19.42250999205614548, 10.98035201082150358, -5.440088680355545492 ) ) ;
#87471 = CARTESIAN_POINT ( 'NONE',  ( 0.1532563361054083140, 6.008931151000784787, 1.131784320476157264E-15 ) ) ;
#87472 = CARTESIAN_POINT ( 'NONE',  ( 21.09922568453594849, 1.206968003263753531, 6.408140936763242479 ) ) ;
#87473 = CARTESIAN_POINT ( 'NONE',  ( 15.44008868035555793, 51.39701867748816966, -9.422509992056140149 ) ) ;
#87475 = CARTESIAN_POINT ( 'NONE',  ( 13.43411237798106583, 37.66530133659708923, -12.81628187352647252 ) ) ;
#87474 = CARTESIAN_POINT ( 'NONE',  ( 4.559911319644449179, 18.89701867748817321, 9.422509992056141925 ) ) ;
#87476 = CARTESIAN_POINT ( 'NONE',  ( 2.917880565312950480, 35.97041550158063217, -12.26659068614894821 ) ) ;
#87477 = EDGE_CURVE ( 'NONE', #91030, #47550, #47652, .T. ) ;
#87478 = CIRCLE ( 'NONE', #1301, 3.500000000000003109 ) ;
#87479 = CARTESIAN_POINT ( 'NONE',  ( 21.92686044187656691, 12.18830936912750751, 4.562052436263911564E-16 ) ) ;
#87480 = CARTESIAN_POINT ( 'NONE',  ( 19.38216949554541557, 52.24863466993041072, -9.382169495545420901 ) ) ;
#87481 = ORIENTED_EDGE ( 'NONE', *, *, #72341, .F. ) ;
#87482 = CARTESIAN_POINT ( 'NONE',  ( 19.84674366389459266, 53.71726448433411605, -2.638427012816827677 ) ) ;
#87483 = CARTESIAN_POINT ( 'NONE',  ( -5.795997163830251431, 15.00000000000000000, 13.01802277140702024 ) ) ;
#87484 = CARTESIAN_POINT ( 'NONE',  ( -0.8801773607111008646, 33.27201867748817676, 2.915334737309923430 ) ) ;
#87485 = CARTESIAN_POINT ( 'NONE',  ( 18.52753015748618282, 58.92559781766745886, -4.923371831947291888 ) ) ;
#87486 = VERTEX_POINT ( 'NONE', #39177 ) ;
#87488 = CARTESIAN_POINT ( 'NONE',  ( -6.356754967080489926, -50.93964766207074035, 2.500000000000000000 ) ) ;
#87487 = CARTESIAN_POINT ( 'NONE',  ( 0.5774900079438590739, 67.64701867748817676, -5.440088680355550821 ) ) ;
#87489 = CARTESIAN_POINT ( 'NONE',  ( 14.09394518620607428, 15.00000000000000000, 3.407449058785458451 ) ) ;
#87490 = CARTESIAN_POINT ( 'NONE',  ( 14.92337183194729633, 12.67559781766745353, 8.527530157486181039 ) ) ;
#87491 = CARTESIAN_POINT ( 'NONE',  ( 18.52753015748617571, 18.09226448433411960, 4.923371831947298993 ) ) ;
#87492 = CARTESIAN_POINT ( 'NONE',  ( 2.791683348922237240, 10.38393115100078390, -7.208316651077763204 ) ) ;
#87494 = CARTESIAN_POINT ( 'NONE',  ( 0.8952175423694801459, 37.60160829253886305, -5.990408912944315212 ) ) ;
#87493 = CARTESIAN_POINT ( 'NONE',  ( 4.559911319644449179, 57.23035201082150536, -9.422509992056141925 ) ) ;
#87495 = CARTESIAN_POINT ( 'NONE',  ( 20.88017736071110519, 65.56368534415483396, 2.639326808657452039E-16 ) ) ;
#87497 = ORIENTED_EDGE ( 'NONE', *, *, #47875, .T. ) ;
#87496 = CARTESIAN_POINT ( 'NONE',  ( 18.52753015748618282, 23.92559781766745530, -4.923371831947291888 ) ) ;
#87498 = DIRECTION ( 'NONE',  ( -0.000000000000000000, -0.000000000000000000, -1.000000000000000000 ) ) ;
#87499 = ADVANCED_FACE ( 'NONE', ( #54645 ), #20224, .T. ) ;
#87500 = CARTESIAN_POINT ( 'NONE',  ( 14.92337183194729988, 59.34226448433412315, -8.527530157486177487 ) ) ;
#87501 = ORIENTED_EDGE ( 'NONE', *, *, #74680, .T. ) ;
#87502 = CARTESIAN_POINT ( 'NONE',  ( -28.94000000000001549, 93.50000000000000000, 9.500000000000000000 ) ) ;
#87503 = CARTESIAN_POINT ( 'NONE',  ( -2.266590686148945544, 21.38708216824730357, -7.082119434687050408 ) ) ;
#87504 = ADVANCED_FACE ( 'NONE', ( #55137 ), #77644, .T. ) ;
#87505 = UNCERTAINTY_MEASURE_WITH_UNIT (LENGTH_MEASURE( 1.000000000000000082E-05 ), #40885, 'distance_accuracy_value', 'NONE');
#87506 = CARTESIAN_POINT ( 'NONE',  ( 2.120353041430552921, 4.509079855230530718E-16, 14.34413130794947122 ) ) ;
#87507 = CARTESIAN_POINT ( 'NONE',  ( 10.00000000000000178, 13.05374883491396787, 14.16423886937410082 ) ) ;
#87508 = CARTESIAN_POINT ( 'NONE',  ( 20.36894250292379738, 29.92874883491396432, -10.36894250292379027 ) ) ;
#87509 = CARTESIAN_POINT ( 'NONE',  ( 12.91533473730992121, 39.52201867748817676, 10.88017736071110164 ) ) ;
#87510 = SURFACE_STYLE_USAGE ( .BOTH. , #49019 ) ;
#87511 = ORIENTED_EDGE ( 'NONE', *, *, #13948, .F. ) ;
#87512 =( BOUNDED_CURVE ( )  B_SPLINE_CURVE ( 2, ( #66543, #22540, #21548, #91517, #23034, #83029, #52039, #15043, #90513 ),
 .UNSPECIFIED., .F., .F. ) 
 B_SPLINE_CURVE_WITH_KNOTS ( ( 3, 2, 2, 2, 3 ),
 ( 0.6187123655116599785, 0.6190476190476190688, 0.6250000000000000000, 0.6309523809523809312, 0.6312876344883400215 ),
 .UNSPECIFIED. ) 
 CURVE ( )  GEOMETRIC_REPRESENTATION_ITEM ( )  RATIONAL_B_SPLINE_CURVE ( ( 0.9963778908391764944, 0.9980808541467923733, 1.000000000000000000, 0.9659258262890682012, 1.000000000000000000, 0.9659258262890682012, 1.000000000000000000, 0.9980808541467922623, 0.9963778908391764944 ) ) 
 REPRESENTATION_ITEM ( '' )  );
#87513 = CARTESIAN_POINT ( 'NONE',  ( 0.1532563361054082862, 11.21726448433411605, 2.638427012816831674 ) ) ;
#87515 = CARTESIAN_POINT ( 'NONE',  ( 12.63842701281683034, 12.46726448433411782, 9.846743663894596210 ) ) ;
#87514 = CARTESIAN_POINT ( 'NONE',  ( 20.88017736071110875, 55.77201867748816966, -2.915334737309920765 ) ) ;
#87516 = CARTESIAN_POINT ( 'NONE',  ( -1.099225684535947600, 48.70696800326375353, -6.408140936763238038 ) ) ;
#87517 = CARTESIAN_POINT ( 'NONE',  ( 17.20831665107776587, 34.13393115100078745, -7.208316651077762316 ) ) ;
#87518 = CARTESIAN_POINT ( 'NONE',  ( 0.1143410931637231370, 25.21691075486303291, 6.480892540919854561 ) ) ;
#87519 = CARTESIAN_POINT ( 'NONE',  ( 16.40814093676323893, 30.79030133659708923, 11.09922568453595026 ) ) ;
#87520 = CARTESIAN_POINT ( 'NONE',  ( 12.26659068614894821, -31.11291783175269643, 7.082119434687044190 ) ) ;
#87521 = CARTESIAN_POINT ( 'NONE',  ( 0.1532563361054100626, 30.80059781766744820, -2.638427012816831230 ) ) ;
#87522 = CARTESIAN_POINT ( 'NONE',  ( -4.164238869374099039, 16.80374883491396787, 8.674139862899312516E-16 ) ) ;
#87523 = ORIENTED_EDGE ( 'NONE', *, *, #17287, .F. ) ;
#87524 = ORIENTED_EDGE ( 'NONE', *, *, #66459, .T. ) ;
#87525 = CARTESIAN_POINT ( 'NONE',  ( 2.035157376598824452, 43.68868534415484106, 7.964842623401179544 ) ) ;
#87526 = CARTESIAN_POINT ( 'NONE',  ( 15.44008868035555260, 54.73035201082150536, 9.422509992056143702 ) ) ;
#87527 = CARTESIAN_POINT ( 'NONE',  ( 24.16423886937409904, 44.09541550158063927, 3.795296366450317205 ) ) ;
#87528 = CARTESIAN_POINT ( 'NONE',  ( 10.00000000000000000, 49.75893115100078745, -9.846743663894594434 ) ) ;
#87529 = CARTESIAN_POINT ( 'NONE',  ( 7.361572987183170547, 12.05059781766744997, 9.846743663894590881 ) ) ;
#87531 = CARTESIAN_POINT ( 'NONE',  ( 15.67879934938582664, -0.03417435944610275333, -3.170591017105818921 ) ) ;
#87530 = CARTESIAN_POINT ( 'NONE',  ( 0.6178305044545818747, 63.49863466993043204, -9.382169495545419124 ) ) ;
#87532 = CARTESIAN_POINT ( 'NONE',  ( 19.42250999205614548, 35.98035201082151247, -5.440088680355545492 ) ) ;
#87533 = FACE_OUTER_BOUND ( 'NONE', #16580, .T. ) ;
#87534 = EDGE_CURVE ( 'NONE', #71973, #55896, #93663, .T. ) ;
#87535 = CARTESIAN_POINT ( 'NONE',  ( 21.09922568453595559, 27.04030133659708568, -6.408140936763230044 ) ) ;
#87536 = CARTESIAN_POINT ( 'NONE',  ( 0.1532563361054082862, 56.21726448433411605, 2.638427012816831674 ) ) ;
#87537 = CARTESIAN_POINT ( 'NONE',  ( 9.422509992056141925, 20.98035201082151957, -5.440088680355554374 ) ) ;
#87538 = CARTESIAN_POINT ( 'NONE',  ( 15.44008868035555260, 4.730352010821504471, 9.422509992056143702 ) ) ;
#87539 = CARTESIAN_POINT ( 'NONE',  ( 10.00000000000000178, 69.31368534415484817, 10.88017736071110342 ) ) ;
#87540 = EDGE_CURVE ( 'NONE', #89266, #65919, #71145, .T. ) ;
#87541 = VECTOR ( 'NONE', #53425, 1000.000000000000000 ) ;
#87542 = CARTESIAN_POINT ( 'NONE',  ( 0.5774900079438590739, 2.647018677488170990, -5.440088680355550821 ) ) ;
#87543 = FILL_AREA_STYLE_COLOUR ( '', #38451 ) ;
#87544 = CARTESIAN_POINT ( 'NONE',  ( 7.084665262690076126, 67.02201867748817676, -10.88017736071110164 ) ) ;
#87545 = CARTESIAN_POINT ( 'NONE',  ( 14.92337183194729633, 2.675597817667451750, 8.527530157486181039 ) ) ;
#87546 = DIRECTION ( 'NONE',  ( -1.000000000000000000, 0.000000000000000000, 0.000000000000000000 ) ) ;
#87547 = CARTESIAN_POINT ( 'NONE',  ( 0.1532563361054082862, 41.21726448433411605, 2.638427012816831674 ) ) ;
#87548 = CARTESIAN_POINT ( 'NONE',  ( 20.88017736071110875, 25.77201867748816966, -2.915334737309920765 ) ) ;
#87549 = CARTESIAN_POINT ( 'NONE',  ( 22.81628187352648496, 1.831968003263753753, -3.434112377981050290 ) ) ;
#87551 = CARTESIAN_POINT ( 'NONE',  ( -12.00809552683965187, 0.5000000000000004441, 8.989195838243462688 ) ) ;
#87550 = CARTESIAN_POINT ( 'NONE',  ( -0.8801773607111009756, 33.06368534415484106, 1.068504757029289695E-15 ) ) ;
#87552 = DIRECTION ( 'NONE',  ( -0.000000000000000000, 1.000000000000000000, -0.000000000000000000 ) ) ;
#87553 = CARTESIAN_POINT ( 'NONE',  ( -2.816281873526471635, 38.91530133659708213, -3.434112377981056508 ) ) ;
#87554 = ORIENTED_EDGE ( 'NONE', *, *, #23056, .F. ) ;
#87555 = CARTESIAN_POINT ( 'NONE',  ( 19.42250999205614548, 45.98035201082150536, -5.440088680355545492 ) ) ;
#87557 =( NAMED_UNIT ( * ) SI_UNIT ( $, .STERADIAN. ) SOLID_ANGLE_UNIT ( ) );
#87556 = CARTESIAN_POINT ( 'NONE',  ( -2.816281873526471635, 23.91530133659708568, -3.434112377981056508 ) ) ;
#87558 = CARTESIAN_POINT ( 'NONE',  ( 17.96484262340118221, 26.18868534415483396, -7.964842623401177768 ) ) ;
#87559 = CARTESIAN_POINT ( 'NONE',  ( 7.084665262690076126, 2.022018677488171434, -10.88017736071110164 ) ) ;
#87560 = CARTESIAN_POINT ( 'NONE',  ( 7.361572987183170547, 42.05059781766745886, 9.846743663894590881 ) ) ;
#87561 = CARTESIAN_POINT ( 'NONE',  ( 0.1532563361054083140, 6.008931151000784787, 1.131784320476157264E-15 ) ) ;
#87562 = CARTESIAN_POINT ( 'NONE',  ( -0.8801773607111009756, 63.06368534415484106, 1.068504757029289695E-15 ) ) ;
#87563 = CARTESIAN_POINT ( 'NONE',  ( -4.862001128006864903, 4.306586084822671512E-16, 13.66056166602457012 ) ) ;
#87564 = CARTESIAN_POINT ( 'NONE',  ( 24.16423886937410614, 24.51208216824730002, -3.795296366450302550 ) ) ;
#87565 = DIRECTION ( 'NONE',  ( 0.000000000000000000, 0.000000000000000000, 1.000000000000000000 ) ) ;
#87566 =( NAMED_UNIT ( * ) SI_UNIT ( $, .STERADIAN. ) SOLID_ANGLE_UNIT ( ) );
#87567 = ORIENTED_EDGE ( 'NONE', *, *, #93846, .F. ) ;
#87568 = ORIENTED_EDGE ( 'NONE', *, *, #49280, .F. ) ;
#87569 = CARTESIAN_POINT ( 'NONE',  ( 17.08211943468705130, 43.47041550158063927, 12.26659068614894998 ) ) ;
#87570 = CARTESIAN_POINT ( 'NONE',  ( 20.36894250292379382, 53.67874883491397497, 10.36894250292379205 ) ) ;
#87571 = CARTESIAN_POINT ( 'NONE',  ( 2.791683348922240793, 16.63393115100078745, 7.208316651077764092 ) ) ;
#87572 = CARTESIAN_POINT ( 'NONE',  ( -2.816281873526473856, 14.12363466993041961, 9.499525473075851096E-16 ) ) ;
#87573 = FACE_OUTER_BOUND ( 'NONE', #79599, .T. ) ;
#87574 = DIRECTION ( 'NONE',  ( 1.000000000000000000, 0.000000000000000000, 0.000000000000000000 ) ) ;
#87575 = CARTESIAN_POINT ( 'NONE',  ( 3.591859063236763294, 28.29030133659708568, -11.09922568453595026 ) ) ;
#87576 = CARTESIAN_POINT ( 'NONE',  ( 20.36894250292379738, 44.92874883491396787, -10.36894250292379027 ) ) ;
#87577 = LINE ( 'NONE', #71118, #38106 ) ;
#87578 = CARTESIAN_POINT ( 'NONE',  ( -2.638427012816840111, -0.03273551566588039224, -9.846743663894590881 ) ) ;
#87579 = VERTEX_POINT ( 'NONE', #40152 ) ;
#87580 = AXIS2_PLACEMENT_3D ( 'NONE', #95795, #74249, #20779 ) ;
#87581 = CARTESIAN_POINT ( 'NONE',  ( 5.076628168052704559, 15.17559781766745175, -8.527530157486179263 ) ) ;
#87582 = ORIENTED_EDGE ( 'NONE', *, *, #66946, .T. ) ;
#87583 = CARTESIAN_POINT ( 'NONE',  ( -4.164238869374099039, 11.80374883491396965, 8.674139862899312516E-16 ) ) ;
#87585 = CARTESIAN_POINT ( 'NONE',  ( 7.084665262690076126, 14.10535201082150358, 10.88017736071109987 ) ) ;
#87584 = CARTESIAN_POINT ( 'NONE',  ( 7.084665262690076126, 12.02201867748817321, -10.88017736071110164 ) ) ;
#87587 = CARTESIAN_POINT ( 'NONE',  ( 19.38216949554541557, 2.248634669930420049, -9.382169495545420901 ) ) ;
#87586 = CARTESIAN_POINT ( 'NONE',  ( 5.076628168052703671, 51.84226448433412315, 8.527530157486179263 ) ) ;
#87588 = CARTESIAN_POINT ( 'NONE',  ( 19.72487221294570858, 0.000000000000000000, -6.500000000000000888 ) ) ;
#87589 = EDGE_CURVE ( 'NONE', #77672, #59059, #58551, .T. ) ;
#87590 = VECTOR ( 'NONE', #62363, 1000.000000000000000 ) ;
#87591 = CARTESIAN_POINT ( 'NONE',  ( -2.816281873526473856, 19.12363466993042138, 9.499525473075851096E-16 ) ) ;
#87592 = ORIENTED_EDGE ( 'NONE', *, *, #55233, .F. ) ;
#87593 = CARTESIAN_POINT ( 'NONE',  ( -0.3689425029237898834, 61.17874883491396076, -10.36894250292378850 ) ) ;
#87594 = ORIENTED_EDGE ( 'NONE', *, *, #85182, .F. ) ;
#87595 = CARTESIAN_POINT ( 'NONE',  ( -0.3689425029237881626, 57.42874883491397497, 10.36894250292379027 ) ) ;
#87596 = ORIENTED_EDGE ( 'NONE', *, *, #18553, .F. ) ;
#87597 = CARTESIAN_POINT ( 'NONE',  ( 4.559911319644449179, 32.23035201082150536, -9.422509992056141925 ) ) ;
#87598 = CARTESIAN_POINT ( 'NONE',  ( -0.8801773607111009756, 48.06368534415484817, 1.068504757029289695E-15 ) ) ;
#87599 = CIRCLE ( 'NONE', #14179, 0.2500000000000002220 ) ;
#87600 = CARTESIAN_POINT ( 'NONE',  ( 0.5774900079438607392, 48.48035201082150536, 5.440088680355550821 ) ) ;
#87601 = CARTESIAN_POINT ( 'NONE',  ( 10.00000000000000178, 34.31368534415484106, 10.88017736071110342 ) ) ;
#87602 = MECHANICAL_DESIGN_GEOMETRIC_PRESENTATION_REPRESENTATION (  '', ( #22188 ), #74830 ) ;
#87603 = VECTOR ( 'NONE', #90687, 1000.000000000000000 ) ;
#87604 = LINE ( 'NONE', #4625, #90443 ) ;
#87605 = EDGE_CURVE ( 'NONE', #15967, #19871, #83790, .T. ) ;
#87606 = CARTESIAN_POINT ( 'NONE',  ( 10.00000000000000000, 14.75893115100078568, -9.846743663894594434 ) ) ;
#87607 = ORIENTED_EDGE ( 'NONE', *, *, #77894, .T. ) ;
#87608 = CARTESIAN_POINT ( 'NONE',  ( 11.13639359202192303, -94.02695735605159655, 4.000000000000000000 ) ) ;
#87609 = CARTESIAN_POINT ( 'NONE',  ( 0.1532563361054083140, 46.00893115100079456, 1.131784320476157264E-15 ) ) ;
#87610 = CARTESIAN_POINT ( 'NONE',  ( 1.354709868695618935, 15.00000000000000000, -14.93870011653151586 ) ) ;
#87611 = CARTESIAN_POINT ( 'NONE',  ( 21.09922568453595559, 52.04030133659708923, -6.408140936763230044 ) ) ;
#87612 = EDGE_CURVE ( 'NONE', #89183, #62473, #2674, .T. ) ;
#87613 = CARTESIAN_POINT ( 'NONE',  ( 1.829604203029677523, 15.00000000000000000, -15.89119079541585755 ) ) ;
#87614 = CARTESIAN_POINT ( 'NONE',  ( -47.22560975609754053, 37.78048780487799263, -8.000000000000000000 ) ) ;
#87615 = CARTESIAN_POINT ( 'NONE',  ( -6.867502880612995853, -58.37510853847093983, 3.749999999999999556 ) ) ;
#87617 = CARTESIAN_POINT ( 'NONE',  ( 18.52753015748617571, 28.09226448433411960, 4.923371831947298993 ) ) ;
#87616 = CARTESIAN_POINT ( 'NONE',  ( 14.92337183194729988, 64.34226448433412315, -8.527530157486177487 ) ) ;
#87618 = CARTESIAN_POINT ( 'NONE',  ( -2.266590686148945544, 61.38708216824730357, -7.082119434687050408 ) ) ;
#87619 = CARTESIAN_POINT ( 'NONE',  ( 0.000000000000000000, 0.5000000000000004441, 0.000000000000000000 ) ) ;
#87620 = VERTEX_POINT ( 'NONE', #33126 ) ;
#87621 = CARTESIAN_POINT ( 'NONE',  ( 1.274849032794292736, 52.55509018479936856, -6.499999999999977796 ) ) ;
#87622 = CARTESIAN_POINT ( 'NONE',  ( 17.20831665107776587, 29.13393115100078390, -7.208316651077762316 ) ) ;
#87623 = CARTESIAN_POINT ( 'NONE',  ( 11.61481287315787370, -90.96947208220468895, -3.750000000000001776 ) ) ;
#87624 = CARTESIAN_POINT ( 'NONE',  ( 22.81628187352647785, 11.41530133659708390, 3.434112377981063169 ) ) ;
#87625 = CARTESIAN_POINT ( 'NONE',  ( 10.00000000000000178, 69.31368534415484817, 10.88017736071110342 ) ) ;
#87626 = PRESENTATION_LAYER_ASSIGNMENT (  '', '', ( #39768 ) ) ;
#87627 = CARTESIAN_POINT ( 'NONE',  ( 3.969999999999999751, 36.75000000000000000, 2.750000000000000000 ) ) ;
#87628 = CARTESIAN_POINT ( 'NONE',  ( 12.63842701281683922, 14.55059781766744997, -9.846743663894590881 ) ) ;
#87629 = CARTESIAN_POINT ( 'NONE',  ( 7.361572987183169658, 54.96726448433413026, -9.846743663894592657 ) ) ;
#87630 = PLANE ( 'NONE',  #96808 ) ;
#87631 = ORIENTED_EDGE ( 'NONE', *, *, #54030, .F. ) ;
#87632 = CARTESIAN_POINT ( 'NONE',  ( 13.79529636645030344, 58.26208216824728936, 14.16423886937410614 ) ) ;
#87633 = CARTESIAN_POINT ( 'NONE',  ( 10.00000000000000178, 3.053748834913967425, 14.16423886937410082 ) ) ;
#87634 = CARTESIAN_POINT ( 'NONE',  ( 0.1532563361054100626, 15.80059781766745353, -2.638427012816831230 ) ) ;
#87635 = CARTESIAN_POINT ( 'NONE',  ( 20.88017736071110875, 35.77201867748816966, -2.915334737309920765 ) ) ;
#87637 = CARTESIAN_POINT ( 'NONE',  ( 10.56735866240293653, 12.77290477899395071, -4.606545654699560899 ) ) ;
#87636 = CARTESIAN_POINT ( 'NONE',  ( 0.6178305044545818747, 23.49863466993041783, -9.382169495545419124 ) ) ;
#87638 = CARTESIAN_POINT ( 'NONE',  ( -0.8801773607111009756, 3.063685344154837509, 1.068504757029289695E-15 ) ) ;
#87639 = DIRECTION ( 'NONE',  ( -0.5224985647159436919, 0.000000000000000000, -0.8526401643540955089 ) ) ;
#87640 = AXIS2_PLACEMENT_3D ( 'NONE', #84130, #76124, #46124 ) ;
#87641 = CARTESIAN_POINT ( 'NONE',  ( 10.00000000000000000, 49.75893115100078745, -9.846743663894594434 ) ) ;
#87642 = CARTESIAN_POINT ( 'NONE',  ( 10.00000000000000000, 9.758931151000785675, -9.846743663894594434 ) ) ;
#87643 = CARTESIAN_POINT ( 'NONE',  ( -5.440088680355547268, -31.10298132251182324, 9.422509992056143702 ) ) ;
#87644 = CARTESIAN_POINT ( 'NONE',  ( 3.591859063236761518, 24.95696800326375353, 11.09922568453594849 ) ) ;
#87645 = CARTESIAN_POINT ( 'NONE',  ( 2.377183314879991460, 50.78593319516822646, -6.500000000000057732 ) ) ;
#87647 = CARTESIAN_POINT ( 'NONE',  ( 12.87930560075675324, 14.95037102969557452, -7.195887444332383254 ) ) ;
#87646 = CARTESIAN_POINT ( 'NONE',  ( 10.00000000000000178, 24.31368534415484106, 10.88017736071110342 ) ) ;
#87648 = CARTESIAN_POINT ( 'NONE',  ( -13.34343830728398927, 14.49999999999999112, -6.852200678592835104 ) ) ;
#87649 = CARTESIAN_POINT ( 'NONE',  ( 24.16423886937410614, 44.51208216824730357, -3.795296366450302550 ) ) ;
#87650 = ADVANCED_FACE ( 'NONE', ( #1192 ), #93140, .F. ) ;
#87651 = CARTESIAN_POINT ( 'NONE',  ( 17.08211943468705840, 30.13708216824730357, -12.26659068614894466 ) ) ;
#87652 = CARTESIAN_POINT ( 'NONE',  ( 14.92337183194729988, 39.34226448433412315, -8.527530157486177487 ) ) ;
#87653 = CARTESIAN_POINT ( 'NONE',  ( -1.099225684535947600, 34.54030133659708923, 6.408140936763237150 ) ) ;
#87654 = CARTESIAN_POINT ( 'NONE',  ( 20.88017736071110519, 30.56368534415484106, 2.639326808657452039E-16 ) ) ;
#87655 = CARTESIAN_POINT ( 'NONE',  ( 7.361572987183170547, 57.05059781766744464, 9.846743663894590881 ) ) ;
#87656 = CARTESIAN_POINT ( 'NONE',  ( 20.88017736071110519, 40.56368534415484106, 2.639326808657452039E-16 ) ) ;
#87657 = CARTESIAN_POINT ( 'NONE',  ( 16.40814093676324603, 7.456968003263754419, -11.09922568453594671 ) ) ;
#87658 = CARTESIAN_POINT ( 'NONE',  ( 17.08211943468705130, 23.47041550158063572, 12.26659068614894998 ) ) ;
#87659 = CARTESIAN_POINT ( 'NONE',  ( 6.138934250732054565, -0.03417435944610275333, -14.77128574976607389 ) ) ;
#87660 = CARTESIAN_POINT ( 'NONE',  ( 19.84674366389459621, 28.50893115100078745, 7.409399052514197653E-17 ) ) ;
#87661 = CARTESIAN_POINT ( 'NONE',  ( 2.791683348922240793, 61.63393115100079456, 7.208316651077764092 ) ) ;
#87662 = ORIENTED_EDGE ( 'NONE', *, *, #39906, .T. ) ;
#87663 = CARTESIAN_POINT ( 'NONE',  ( 4.326345305608651159, 0.000000000000000000, -3.319721512309584011 ) ) ;
#87664 = CARTESIAN_POINT ( 'NONE',  ( 4.474002695404426966, -3.767820133606233579, 3.750000000000001776 ) ) ;
#87665 = CARTESIAN_POINT ( 'NONE',  ( 10.00000000000000178, 19.31368534415484106, 10.88017736071110342 ) ) ;
#87666 = CARTESIAN_POINT ( 'NONE',  ( 15.44008868035555260, 59.73035201082151247, 9.422509992056143702 ) ) ;
#87667 = CARTESIAN_POINT ( 'NONE',  ( -4.164238869374099927, 7.012082168247302683, 3.795296366450308767 ) ) ;
#87668 = CARTESIAN_POINT ( 'NONE',  ( 5.076628168052703671, 6.842264484334118713, 8.527530157486179263 ) ) ;
#87669 = CARTESIAN_POINT ( 'NONE',  ( 1.472469842513823179, 51.42559781766745886, 4.923371831947296329 ) ) ;
#87670 = CARTESIAN_POINT ( 'NONE',  ( 4.559911319644449179, 32.23035201082150536, -9.422509992056141925 ) ) ;
#87671 = CARTESIAN_POINT ( 'NONE',  ( 18.95386800104995828, 13.23810908735726777, -6.500000000000000888 ) ) ;
#87672 = PLANE ( 'NONE',  #32965 ) ;
#87673 = AXIS2_PLACEMENT_3D ( 'NONE', #68053, #29534, #53031 ) ;
#87674 = ORIENTED_EDGE ( 'NONE', *, *, #81450, .F. ) ;
#87675 = CIRCLE ( 'NONE', #1502, 0.1000000000000001166 ) ;
#87676 = CARTESIAN_POINT ( 'NONE',  ( 6.660464271194117103, -84.28715080306288598, 2.499999999999999556 ) ) ;
#87677 = EDGE_LOOP ( 'NONE', ( #57930, #74814, #34117, #62547 ) ) ;
#87678 = ORIENTED_EDGE ( 'NONE', *, *, #78331, .T. ) ;
#87679 = LINE ( 'NONE', #11693, #59693 ) ;
#87680 = CARTESIAN_POINT ( 'NONE',  ( 17.08211943468705840, 5.137082168247300906, -12.26659068614894466 ) ) ;
#87681 = CARTESIAN_POINT ( 'NONE',  ( 24.16423886937410614, 14.30374883491396787, 8.672049930838204340E-16 ) ) ;
#87682 = CARTESIAN_POINT ( 'NONE',  ( 17.08211943468705840, 60.13708216824729647, -12.26659068614894466 ) ) ;
#87683 = CARTESIAN_POINT ( 'NONE',  ( 5.076628168052703671, 56.84226448433412315, 8.527530157486179263 ) ) ;
#87684 = CARTESIAN_POINT ( 'NONE',  ( 7.361572987183170547, 42.05059781766745886, 9.846743663894590881 ) ) ;
#87685 = CARTESIAN_POINT ( 'NONE',  ( -1.099225684535947600, 64.54030133659709634, 6.408140936763237150 ) ) ;
#87687 = CARTESIAN_POINT ( 'NONE',  ( 17.20831665107776587, 59.13393115100078745, -7.208316651077762316 ) ) ;
#87686 = CARTESIAN_POINT ( 'NONE',  ( 7.084665262690076126, 39.10535201082150536, 10.88017736071109987 ) ) ;
#87688 = CARTESIAN_POINT ( 'NONE',  ( 10.00000000000000000, 5.553748834913967869, -14.16423886937410082 ) ) ;
#87689 = CARTESIAN_POINT ( 'NONE',  ( 6.204703633549690345, 52.84541550158062506, 14.16423886937410082 ) ) ;
#87690 = CARTESIAN_POINT ( 'NONE',  ( 6.204703633549690345, 67.84541550158060375, 14.16423886937410082 ) ) ;
#87691 = DIRECTION ( 'NONE',  ( -0.000000000000000000, -1.000000000000000000, -0.000000000000000000 ) ) ;
#87692 = DIRECTION ( 'NONE',  ( -0.000000000000000000, -0.000000000000000000, -1.000000000000000000 ) ) ;
#87693 = CARTESIAN_POINT ( 'NONE',  ( -8.527530157486173934, -38.57440218233254825, 4.923371831947302546 ) ) ;
#87694 = VERTEX_POINT ( 'NONE', #31654 ) ;
#87695 = CARTESIAN_POINT ( 'NONE',  ( 0.000000000000000000, 15.00000000000000000, 0.000000000000000000 ) ) ;
#87696 = ORIENTED_EDGE ( 'NONE', *, *, #66191, .T. ) ;
#87697 = CARTESIAN_POINT ( 'NONE',  ( 19.84674366389459266, 23.30059781766745530, 2.638427012816836559 ) ) ;
#87698 = ORIENTED_EDGE ( 'NONE', *, *, #9489, .T. ) ;
#87699 = CARTESIAN_POINT ( 'NONE',  ( 17.08211943468705130, 38.47041550158063217, 12.26659068614894998 ) ) ;
#87700 = CARTESIAN_POINT ( 'NONE',  ( 7.361572987183170547, 32.05059781766745175, 9.846743663894590881 ) ) ;
#87701 = CARTESIAN_POINT ( 'NONE',  ( -0.8801773607111009756, 53.06368534415484106, 1.068504757029289695E-15 ) ) ;
#87702 =( NAMED_UNIT ( * ) PLANE_ANGLE_UNIT ( ) SI_UNIT ( $, .RADIAN. ) );
#87703 = EDGE_CURVE ( 'NONE', #20606, #51688, #94589, .T. ) ;
#87704 = CARTESIAN_POINT ( 'NONE',  ( 15.44008868035555260, 54.73035201082150536, 9.422509992056143702 ) ) ;
#87705 = CARTESIAN_POINT ( 'NONE',  ( 14.92337183194729988, 49.34226448433411605, -8.527530157486177487 ) ) ;
#87706 = EDGE_CURVE ( 'NONE', #66014, #91084, #7475, .T. ) ;
#87707 = EDGE_CURVE ( 'NONE', #35180, #96723, #63332, .T. ) ;
#87708 = CARTESIAN_POINT ( 'NONE',  ( -11.09922568453595382, 13.70696800326375708, -6.408140936763226492 ) ) ;
#87709 = VERTEX_POINT ( 'NONE', #95102 ) ;
#87710 = CARTESIAN_POINT ( 'NONE',  ( 10.00000000000000000, 20.55374883491396787, -14.16423886937410082 ) ) ;
#87711 = ORIENTED_EDGE ( 'NONE', *, *, #47881, .F. ) ;
#87712 = ORIENTED_EDGE ( 'NONE', *, *, #85357, .T. ) ;
#87713 = CARTESIAN_POINT ( 'NONE',  ( 6.565887622018943937, 28.08196800326375353, -12.81628187352647608 ) ) ;
#87714 = DIRECTION ( 'NONE',  ( 0.8320502943378436100, -0.5547001962252291474, 0.000000000000000000 ) ) ;
#87715 = CARTESIAN_POINT ( 'NONE',  ( 14.92337183194729633, 22.67559781766745175, 8.527530157486181039 ) ) ;
#87716 = CARTESIAN_POINT ( 'NONE',  ( 4.559911319644449179, 18.89701867748817321, 9.422509992056141925 ) ) ;
#87717 =( REPRESENTATION_RELATIONSHIP ('NONE','NONE', #61309, #57512 ) REPRESENTATION_RELATIONSHIP_WITH_TRANSFORMATION ( #15722 )SHAPE_REPRESENTATION_RELATIONSHIP( ) );
#87718 = CARTESIAN_POINT ( 'NONE',  ( -1.099225684535947600, 48.70696800326375353, -6.408140936763238038 ) ) ;
#87719 = EDGE_CURVE ( 'NONE', #93614, #89322, #88096, .T. ) ;
#87720 = DIRECTION ( 'NONE',  ( 1.000000000000000000, 0.000000000000000000, 0.000000000000000000 ) ) ;
#87721 = CARTESIAN_POINT ( 'NONE',  ( 17.20831665107776587, 27.88393115100078390, 7.208316651077764980 ) ) ;
#87722 = VECTOR ( 'NONE', #81389, 1000.000000000000114 ) ;
#87723 = CARTESIAN_POINT ( 'NONE',  ( 20.32896413005680714, 22.60497603579417714, -5.963430220938276349 ) ) ;
#87724 = EDGE_CURVE ( 'NONE', #4086, #30837, #81580, .T. ) ;
#87725 = CARTESIAN_POINT ( 'NONE',  ( 7.084665262690076126, 64.10535201082150536, 10.88017736071109987 ) ) ;
#87726 = CARTESIAN_POINT ( 'NONE',  ( 19.90229974777923161, 69.67742753483354079, 6.500000000000000000 ) ) ;
#87727 = LINE ( 'NONE', #82698, #87603 ) ;
#87728 = CARTESIAN_POINT ( 'NONE',  ( 0.1532563361054082862, 6.217264484334118713, 2.638427012816831674 ) ) ;
#87729 = CARTESIAN_POINT ( 'NONE',  ( 3.591859063236761518, 29.95696800326375708, 11.09922568453594849 ) ) ;
#87730 = ADVANCED_FACE ( 'NONE', ( #42608 ), #76113, .T. ) ;
#87731 = CARTESIAN_POINT ( 'NONE',  ( 3.384800920124170887, 0.2306972965111907803, -14.55270344038008190 ) ) ;
#87732 = CARTESIAN_POINT ( 'NONE',  ( 7.361572987183170547, 42.05059781766745886, 9.846743663894590881 ) ) ;
#87733 = CARTESIAN_POINT ( 'NONE',  ( 19.10478245763047411, 36.02576239577082617, -5.990408912944397812 ) ) ;
#87734 = CARTESIAN_POINT ( 'NONE',  ( -2.266590686148945544, 27.22041550158063572, 7.082119434687048631 ) ) ;
#87735 = CARTESIAN_POINT ( 'NONE',  ( 12.63842701281683922, 29.55059781766745175, -9.846743663894590881 ) ) ;
#87736 = CARTESIAN_POINT ( 'NONE',  ( 3.591859063236763294, 28.29030133659708568, -11.09922568453595026 ) ) ;
#87738 = CARTESIAN_POINT ( 'NONE',  ( 9.898881779040660689, 15.00000000000000000, 10.25059215482582786 ) ) ;
#87737 = FACE_OUTER_BOUND ( 'NONE', #19336, .T. ) ;
#87739 = CARTESIAN_POINT ( 'NONE',  ( 15.44008868035555793, 56.39701867748817676, -9.422509992056140149 ) ) ;
#87740 = CARTESIAN_POINT ( 'NONE',  ( 3.591859063236761518, 9.956968003263753531, 11.09922568453594849 ) ) ;
#87741 = DIRECTION ( 'NONE',  ( 0.4617486132350405170, 0.000000000000000000, -0.8870108331782183830 ) ) ;
#87742 = CARTESIAN_POINT ( 'NONE',  ( 10.00000000000000178, 37.25893115100078745, 9.846743663894594434 ) ) ;
#87743 = CARTESIAN_POINT ( 'NONE',  ( 15.44008868035555793, 31.39701867748817676, -9.422509992056140149 ) ) ;
#87744 = CARTESIAN_POINT ( 'NONE',  ( 21.09922568453594849, 26.20696800326375353, 6.408140936763242479 ) ) ;
#87745 =( NAMED_UNIT ( * ) SI_UNIT ( $, .STERADIAN. ) SOLID_ANGLE_UNIT ( ) );
#87746 = CARTESIAN_POINT ( 'NONE',  ( 14.74963345907814372, 14.95077488074853456, 0.3072669459661709346 ) ) ;
#87747 = CARTESIAN_POINT ( 'NONE',  ( 17.96484262340118221, 34.93868534415482685, 7.964842623401181321 ) ) ;
#87748 = EDGE_LOOP ( 'NONE', ( #85072, #62904, #16487, #91788 ) ) ;
#87749 = CARTESIAN_POINT ( 'NONE',  ( 7.084665262690076126, 62.02201867748816966, -10.88017736071110164 ) ) ;
#87750 = FACE_OUTER_BOUND ( 'NONE', #40962, .T. ) ;
#87752 = CARTESIAN_POINT ( 'NONE',  ( 17.96484262340118221, 34.93868534415482685, 7.964842623401181321 ) ) ;
#87751 = CARTESIAN_POINT ( 'NONE',  ( 7.361572987183169658, 54.96726448433413026, -9.846743663894592657 ) ) ;
#87753 = PLANE ( 'NONE',  #52038 ) ;
#87754 = CARTESIAN_POINT ( 'NONE',  ( 17.96484262340118221, 44.93868534415483396, 7.964842623401181321 ) ) ;
#87756 = CARTESIAN_POINT ( 'NONE',  ( 20.00000000000000711, 88.18949240714751170, -4.994480956901625746 ) ) ;
#87755 = CARTESIAN_POINT ( 'NONE',  ( -0.8801773607110991993, 22.85535201082150181, -2.915334737309923874 ) ) ;
#87757 = CARTESIAN_POINT ( 'NONE',  ( 18.52753015748618282, 3.925597817667451306, -4.923371831947291888 ) ) ;
#87758 = CARTESIAN_POINT ( 'NONE',  ( 0.000000000000000000, 40.74999999999999289, -4.250000000000000000 ) ) ;
#87759 = CARTESIAN_POINT ( 'NONE',  ( 10.00000000000000178, 57.25893115100078745, 9.846743663894594434 ) ) ;
#87761 = CARTESIAN_POINT ( 'NONE',  ( -12.00809552683965720, 0.3640475087720476677, 8.989195838243462688 ) ) ;
#87760 = CARTESIAN_POINT ( 'NONE',  ( 2.917880565312948704, 57.63708216824731068, 12.26659068614894643 ) ) ;
#87762 = DIRECTION ( 'NONE',  ( -1.000000000000000000, -1.483861936729430326E-16, 0.000000000000000000 ) ) ;
#87763 = DIRECTION ( 'NONE',  ( 0.000000000000000000, 0.000000000000000000, 1.000000000000000000 ) ) ;
#87764 = EDGE_CURVE ( 'NONE', #71459, #27523, #38457, .T. ) ;
#87765 = CARTESIAN_POINT ( 'NONE',  ( 20.36894250292379738, 34.92874883491396076, -10.36894250292379027 ) ) ;
#87766 = CARTESIAN_POINT ( 'NONE',  ( 10.00000000000000178, 5.373634669930420493, 12.81628187352647608 ) ) ;
#87767 = CARTESIAN_POINT ( 'NONE',  ( -3.888677573129737830, -8.267510245829294391, 2.750000000000000444 ) ) ;
#87768 = ORIENTED_EDGE ( 'NONE', *, *, #9402, .F. ) ;
#87769 = CARTESIAN_POINT ( 'NONE',  ( 10.00000000000000178, 63.05374883491396076, 14.16423886937410082 ) ) ;
#87770 = CARTESIAN_POINT ( 'NONE',  ( 10.00000000000000178, 32.25893115100078745, 9.846743663894594434 ) ) ;
#87772 = CARTESIAN_POINT ( 'NONE',  ( -11.93818897418494984, 90.30657785595315090, -6.860068911468413688 ) ) ;
#87771 = CARTESIAN_POINT ( 'NONE',  ( 3.640395162852214650, 89.00000000000000000, -9.500000000000000000 ) ) ;
#87773 = CARTESIAN_POINT ( 'NONE',  ( 20.88017736071110519, 65.56368534415483396, 2.639326808657452039E-16 ) ) ;
#87774 = CARTESIAN_POINT ( 'NONE',  ( 5.056330833731640162, 15.00000000000000000, 13.58983143750701394 ) ) ;
#87775 = CARTESIAN_POINT ( 'NONE',  ( 4.559911319644449179, 28.89701867748817321, 9.422509992056141925 ) ) ;
#87776 = CARTESIAN_POINT ( 'NONE',  ( 3.591859063236763294, 58.29030133659708923, -11.09922568453595026 ) ) ;
#87777 = CARTESIAN_POINT ( 'NONE',  ( 22.81628187352647785, 11.41530133659708390, 3.434112377981063169 ) ) ;
#87778 = CARTESIAN_POINT ( 'NONE',  ( 14.92337183194729633, 32.67559781766745175, 8.527530157486181039 ) ) ;
#87779 = ORIENTED_EDGE ( 'NONE', *, *, #6348, .T. ) ;
#87780 =( NAMED_UNIT ( * ) PLANE_ANGLE_UNIT ( ) SI_UNIT ( $, .RADIAN. ) );
#87781 = CARTESIAN_POINT ( 'NONE',  ( 17.39651004071841811, 2.935752660568277328, 6.500000000000002665 ) ) ;
#87782 = CARTESIAN_POINT ( 'NONE',  ( 10.00000000000000178, 63.05374883491396076, 14.16423886937410082 ) ) ;
#87783 = CARTESIAN_POINT ( 'NONE',  ( 13.79529636645030344, 33.26208216824730357, 14.16423886937410614 ) ) ;
#87784 = CARTESIAN_POINT ( 'NONE',  ( 20.88017736071110875, 35.77201867748816966, -2.915334737309920765 ) ) ;
#87785 = CARTESIAN_POINT ( 'NONE',  ( 10.00000000000000178, 54.31368534415484106, 10.88017736071110342 ) ) ;
#87786 = DIRECTION ( 'NONE',  ( 0.000000000000000000, 0.000000000000000000, -1.000000000000000000 ) ) ;
#87787 = CARTESIAN_POINT ( 'NONE',  ( 9.261738776912691762, -15.50721619310700028, -4.000000000000000888 ) ) ;
#87788 = CARTESIAN_POINT ( 'NONE',  ( 0.1532563361054082862, 6.217264484334118713, 2.638427012816831674 ) ) ;
#87789 = SURFACE_STYLE_FILL_AREA ( #49304 ) ;
#87790 = PRESENTATION_STYLE_ASSIGNMENT (( #33790 ) ) ;
#87791 = CARTESIAN_POINT ( 'NONE',  ( 18.52753015748618282, 18.92559781766745175, -4.923371831947291888 ) ) ;
#87792 = CARTESIAN_POINT ( 'NONE',  ( 10.00000000000000000, 44.75893115100078745, -9.846743663894594434 ) ) ;
#87793 = CARTESIAN_POINT ( 'NONE',  ( 10.00000000000000178, 45.37363466993041783, 12.81628187352647608 ) ) ;
#87794 = CARTESIAN_POINT ( 'NONE',  ( -4.431036607602373500, 0.5000000000000004441, -14.33059365769916838 ) ) ;
#87795 = CARTESIAN_POINT ( 'NONE',  ( -0.8801773607111008646, 68.27201867748817676, 2.915334737309923430 ) ) ;
#87796 = CARTESIAN_POINT ( 'NONE',  ( 7.361572987183169658, 34.96726448433411605, -9.846743663894592657 ) ) ;
#87798 = CARTESIAN_POINT ( 'NONE',  ( 14.92337183194729988, 19.34226448433411960, -8.527530157486177487 ) ) ;
#87797 = CARTESIAN_POINT ( 'NONE',  ( 20.36894250292379738, 59.92874883491397497, -10.36894250292379027 ) ) ;
#87799 = LINE ( 'NONE', #20306, #27830 ) ;
#87800 = CARTESIAN_POINT ( 'NONE',  ( 17.20831665107776587, 64.13393115100079456, -7.208316651077762316 ) ) ;
#87801 = CARTESIAN_POINT ( 'NONE',  ( -4.164238869374098151, 31.59541550158063927, -3.795296366450310543 ) ) ;
#87802 = CARTESIAN_POINT ( 'NONE',  ( 19.84674366389459266, 43.30059781766744464, 2.638427012816836559 ) ) ;
#87803 = CARTESIAN_POINT ( 'NONE',  ( 19.72487221294570858, 12.80223176428831167, -6.500000000000000888 ) ) ;
#87804 = CARTESIAN_POINT ( 'NONE',  ( 20.88017736071110164, 30.35535201082151247, 2.915334737309930979 ) ) ;
#87805 = B_SPLINE_CURVE_WITH_KNOTS ( 'NONE', 3,
 ( #92362, #46854, #93344, #63330 ),
 .UNSPECIFIED., .F., .F.,
 ( 4, 4 ),
 ( 0.000000000000000000, 0.001036303429213365507 ),
 .UNSPECIFIED. ) ;
#87806 = CARTESIAN_POINT ( 'NONE',  ( 0.5774900079438607392, 63.48035201082149825, 5.440088680355550821 ) ) ;
#87807 = CARTESIAN_POINT ( 'NONE',  ( 19.10478245763052740, 51.02576239577081907, -5.990408912944300113 ) ) ;
#87808 = ORIENTED_EDGE ( 'NONE', *, *, #11199, .T. ) ;
#87809 = CARTESIAN_POINT ( 'NONE',  ( 19.38216949554541202, 45.99863466993041072, 9.382169495545424454 ) ) ;
#87810 = EDGE_CURVE ( 'NONE', #24577, #9027, #79625, .T. ) ;
#87811 = CARTESIAN_POINT ( 'NONE',  ( 0.5774900079438590739, 57.64701867748817676, -5.440088680355550821 ) ) ;
#87812 = ORIENTED_EDGE ( 'NONE', *, *, #81442, .F. ) ;
#87813 = CARTESIAN_POINT ( 'NONE',  ( 18.52753015748618282, 63.92559781766745886, -4.923371831947291888 ) ) ;
#87814 = CARTESIAN_POINT ( 'NONE',  ( 10.00000000000000000, 66.81368534415484817, -10.88017736071110342 ) ) ;
#87815 = ORIENTED_EDGE ( 'NONE', *, *, #92072, .T. ) ;
#87817 = EDGE_CURVE ( 'NONE', #21605, #11587, #87604, .T. ) ;
#87816 = CARTESIAN_POINT ( 'NONE',  ( 12.91533473730992121, 64.52201867748817676, 10.88017736071110164 ) ) ;
#87818 = CARTESIAN_POINT ( 'NONE',  ( 0.5774900079438590739, 12.64701867748817143, -5.440088680355550821 ) ) ;
#87819 = CARTESIAN_POINT ( 'NONE',  ( 1.958556081791334780, 0.5155005897679896254, -5.765297895236029646 ) ) ;
#87820 = DIRECTION ( 'NONE',  ( 1.000000000000000000, 0.000000000000000000, 0.000000000000000000 ) ) ;
#87821 = CARTESIAN_POINT ( 'NONE',  ( 15.44008868035555260, 4.730352010821505360, 9.422509992056143702 ) ) ;
#87822 = CARTESIAN_POINT ( 'NONE',  ( 0.1532563361054100626, 5.800597817667452638, -2.638427012816831230 ) ) ;
#87823 = CARTESIAN_POINT ( 'NONE',  ( -2.266590686148945544, 12.22041550158063394, 7.082119434687048631 ) ) ;
#87824 = ADVANCED_FACE ( 'NONE', ( #41643 ), #35088, .T. ) ;
#87825 = EDGE_CURVE ( 'NONE', #34926, #94118, #23398, .T. ) ;
#87826 = CARTESIAN_POINT ( 'NONE',  ( 19.42250999205614193, 25.14701867748817321, 5.440088680355555262 ) ) ;
#87827 = CARTESIAN_POINT ( 'NONE',  ( 18.52753015748618282, 58.92559781766745886, -4.923371831947291888 ) ) ;
#87828 = ORIENTED_EDGE ( 'NONE', *, *, #46732, .F. ) ;
#87829 = AXIS2_PLACEMENT_3D ( 'NONE', #25352, #63798, #32815 ) ;
#87830 = CARTESIAN_POINT ( 'NONE',  ( 2.791683348922237240, 55.38393115100078745, -7.208316651077763204 ) ) ;
#87831 = ORIENTED_EDGE ( 'NONE', *, *, #88779, .T. ) ;
#87832 = CARTESIAN_POINT ( 'NONE',  ( -0.8801773607111008646, 48.27201867748816966, 2.915334737309923430 ) ) ;
#87833 = CARTESIAN_POINT ( 'NONE',  ( 1.472469842513823179, 45.59226448433412315, -4.923371831947296329 ) ) ;
#87835 = CARTESIAN_POINT ( 'NONE',  ( -13.61912076658538240, 15.00000000000000711, -5.334594295381093865 ) ) ;
#87834 = CARTESIAN_POINT ( 'NONE',  ( 19.42250999205614548, 10.98035201082150358, -5.440088680355545492 ) ) ;
#87836 = CARTESIAN_POINT ( 'NONE',  ( 20.88017736071110164, 65.35535201082150536, 2.915334737309930979 ) ) ;
#87837 = VECTOR ( 'NONE', #10756, 1000.000000000000000 ) ;
#87838 = CARTESIAN_POINT ( 'NONE',  ( 17.96484262340118221, 4.938685344154837509, 7.964842623401181321 ) ) ;
#87839 = EDGE_CURVE ( 'NONE', #44176, #93746, #57599, .T. ) ;
#87840 = CIRCLE ( 'NONE', #89419, 2.000000000000000888 ) ;
#87841 = CARTESIAN_POINT ( 'NONE',  ( 19.38216949554541202, 35.99863466993041072, 9.382169495545424454 ) ) ;
#87842 = CARTESIAN_POINT ( 'NONE',  ( 15.44008868035555793, 36.39701867748816966, -9.422509992056140149 ) ) ;
#87843 = CARTESIAN_POINT ( 'NONE',  ( -3.897244926436033374, 15.00000000000000000, -13.96644127841335958 ) ) ;
#87844 = ORIENTED_EDGE ( 'NONE', *, *, #25585, .T. ) ;
#87845 = CARTESIAN_POINT ( 'NONE',  ( 0.6178305044545838731, 39.74863466993041072, 9.382169495545420901 ) ) ;
#87846 = CARTESIAN_POINT ( 'NONE',  ( 7.084665262690076126, 37.02201867748817676, -10.88017736071110164 ) ) ;
#87847 = CARTESIAN_POINT ( 'NONE',  ( 18.52753015748618282, 58.92559781766745886, -4.923371831947291888 ) ) ;
#87849 = VERTEX_POINT ( 'NONE', #19608 ) ;
#87848 = EDGE_CURVE ( 'NONE', #82789, #981, #21819, .T. ) ;
#87850 = CARTESIAN_POINT ( 'NONE',  ( 17.75000000000000000, 78.80384757729335377, -3.750000000000000444 ) ) ;
#87851 = CARTESIAN_POINT ( 'NONE',  ( 17.20831665107776587, 57.88393115100078745, 7.208316651077764980 ) ) ;
#87853 = CARTESIAN_POINT ( 'NONE',  ( 5.076628168052703671, 51.84226448433412315, 8.527530157486179263 ) ) ;
#87852 = CARTESIAN_POINT ( 'NONE',  ( -9.898881779040587858, 15.00000000000000000, -10.25059215482589714 ) ) ;
#87854 = CARTESIAN_POINT ( 'NONE',  ( 7.084665262690076126, 17.02201867748817676, -10.88017736071110164 ) ) ;
#87855 = CARTESIAN_POINT ( 'NONE',  ( -28.94000000000001549, 93.50000000000000000, -10.09898361729590199 ) ) ;
#87856 = CARTESIAN_POINT ( 'NONE',  ( 1.472469842513823179, 35.59226448433412315, -4.923371831947296329 ) ) ;
#87857 = DIRECTION ( 'NONE',  ( 0.000000000000000000, 0.000000000000000000, 1.000000000000000000 ) ) ;
#87858 = CARTESIAN_POINT ( 'NONE',  ( 0.2751277870542909176, 60.30223176428830101, 6.499999999999992006 ) ) ;
#87860 = CARTESIAN_POINT ( 'NONE',  ( 5.076628168052704559, 15.17559781766745175, -8.527530157486179263 ) ) ;
#87859 = CARTESIAN_POINT ( 'NONE',  ( 1.472469842513823179, 46.42559781766745175, 4.923371831947296329 ) ) ;
#87861 = CARTESIAN_POINT ( 'NONE',  ( 0.9413316022086116730, 8.455083851089586489, 6.499999999999963585 ) ) ;
#87863 = EDGE_LOOP ( 'NONE', ( #94732, #85936, #11591, #74571 ) ) ;
#87862 = CARTESIAN_POINT ( 'NONE',  ( 0.1532563361054083140, 66.00893115100079456, 1.131784320476157264E-15 ) ) ;
#87864 = PRESENTATION_STYLE_ASSIGNMENT (( #88368 ) ) ;
#87865 = CARTESIAN_POINT ( 'NONE',  ( 6.565887622018943937, 45.16530133659708923, 12.81628187352647430 ) ) ;
#87866 = CARTESIAN_POINT ( 'NONE',  ( 19.84674366389459266, 38.71726448433412315, -2.638427012816827677 ) ) ;
#87867 = PRESENTATION_STYLE_ASSIGNMENT (( #64858 ) ) ;
#87868 = CARTESIAN_POINT ( 'NONE',  ( 6.204703633549690345, 65.76208216824731778, -14.16423886937410259 ) ) ;
#87869 = CARTESIAN_POINT ( 'NONE',  ( 19.84674366389459621, 33.50893115100078745, 7.409399052514197653E-17 ) ) ;
#87870 = CARTESIAN_POINT ( 'NONE',  ( 8.564643372776618691, 14.63595249122790598, -12.31449893000741369 ) ) ;
#87871 = CARTESIAN_POINT ( 'NONE',  ( -4.164238869374099039, 56.80374883491397497, 8.674139862899312516E-16 ) ) ;
#87872 = DIRECTION ( 'NONE',  ( -1.000000000000000000, 0.000000000000000000, 0.000000000000000000 ) ) ;
#87873 = CARTESIAN_POINT ( 'NONE',  ( -0.8801773607111009756, 3.063685344154838397, 1.068504757029289695E-15 ) ) ;
#87874 = CARTESIAN_POINT ( 'NONE',  ( 17.08211943468705840, 35.13708216824730357, -12.26659068614894466 ) ) ;
#87875 = CARTESIAN_POINT ( 'NONE',  ( 22.26659068614895176, 39.72041550158063217, -7.082119434687042414 ) ) ;
#87876 = DIRECTION ( 'NONE',  ( -0.5547001962252290364, -0.8320502943378437211, 0.000000000000000000 ) ) ;
#87877 = CARTESIAN_POINT ( 'NONE',  ( 5.076628168052703671, 16.84226448433411960, 8.527530157486179263 ) ) ;
#87879 = CARTESIAN_POINT ( 'NONE',  ( 0.1532563361054082862, 61.21726448433412315, 2.638427012816831674 ) ) ;
#87878 = CARTESIAN_POINT ( 'NONE',  ( 6.935134328217578137, -80.57830137131843173, 2.750000000001609823 ) ) ;
#87880 = CARTESIAN_POINT ( 'NONE',  ( 0.5774900079438607392, 48.48035201082150536, 5.440088680355550821 ) ) ;
#87881 = DIRECTION ( 'NONE',  ( 0.000000000000000000, 1.000000000000000000, 0.000000000000000000 ) ) ;
#87882 = CARTESIAN_POINT ( 'NONE',  ( 2.791683348922237240, 50.38393115100078035, -7.208316651077763204 ) ) ;
#87883 = CARTESIAN_POINT ( 'NONE',  ( 6.565887622018943937, 65.16530133659709634, 12.81628187352647430 ) ) ;
#87884 = CARTESIAN_POINT ( 'NONE',  ( 2.791683348922240793, 56.63393115100078035, 7.208316651077764092 ) ) ;
#87885 = CIRCLE ( 'NONE', #44787, 14.49999999999999822 ) ;
#87886 = ORIENTED_EDGE ( 'NONE', *, *, #74975, .F. ) ;
#87887 = CARTESIAN_POINT ( 'NONE',  ( -4.164238869374098151, 21.59541550158063217, -3.795296366450310543 ) ) ;
#87888 = CARTESIAN_POINT ( 'NONE',  ( 6.000000000000000000, 60.50000000000000711, 5.000000000000000000 ) ) ;
#87890 = FACE_OUTER_BOUND ( 'NONE', #94003, .T. ) ;
#87889 = SURFACE_STYLE_FILL_AREA ( #41449 ) ;
#87891 = CARTESIAN_POINT ( 'NONE',  ( 12.91533473730992121, 24.52201867748816966, 10.88017736071110164 ) ) ;
#87892 = CARTESIAN_POINT ( 'NONE',  ( -2.816281873526473856, 19.33196800326375708, 3.434112377981055619 ) ) ;
#87893 = FACE_OUTER_BOUND ( 'NONE', #65815, .T. ) ;
#87894 = CARTESIAN_POINT ( 'NONE',  ( 17.20831665107776587, 7.883931151000784787, 7.208316651077764980 ) ) ;
#87895 = CIRCLE ( 'NONE', #86272, 0.5000000000000004441 ) ;
#87896 = CARTESIAN_POINT ( 'NONE',  ( 6.565887622018943937, 48.08196800326375353, -12.81628187352647608 ) ) ;
#87897 = VERTEX_POINT ( 'NONE', #27597 ) ;
#87898 = CARTESIAN_POINT ( 'NONE',  ( 7.079515573063597245, -88.00917032380698402, -4.000000000000000000 ) ) ;
#87899 = AXIS2_PLACEMENT_3D ( 'NONE', #36025, #45002, #68017 ) ;
#87900 = CARTESIAN_POINT ( 'NONE',  ( -4.164238869374098151, 26.59541550158063217, -3.795296366450310543 ) ) ;
#87901 = LINE ( 'NONE', #57409, #61170 ) ;
#87902 = ADVANCED_FACE ( 'NONE', ( #34593 ), #65086, .F. ) ;
#87903 = CARTESIAN_POINT ( 'NONE',  ( 19.72487221294570858, 61.86607318730076344, 6.500000000000000888 ) ) ;
#87904 = CARTESIAN_POINT ( 'NONE',  ( 0.5774900079438607392, 13.48035201082150358, 5.440088680355550821 ) ) ;
#87905 = FACE_OUTER_BOUND ( 'NONE', #77142, .T. ) ;
#87906 = CARTESIAN_POINT ( 'NONE',  ( 4.431036607602565347, 0.3640475087720985159, -14.33059365769911864 ) ) ;
#87907 = CARTESIAN_POINT ( 'NONE',  ( 20.88017736071110519, 45.56368534415484106, 2.639326808657452039E-16 ) ) ;
#87908 = CARTESIAN_POINT ( 'NONE',  ( 4.559911319644449179, 47.23035201082150536, -9.422509992056141925 ) ) ;
#87909 = CARTESIAN_POINT ( 'NONE',  ( 21.09922568453595559, 12.04030133659708746, -6.408140936763230044 ) ) ;
#87910 = CARTESIAN_POINT ( 'NONE',  ( 1.472469842513823179, 60.59226448433412315, -4.923371831947296329 ) ) ;
#87911 = DIRECTION ( 'NONE',  ( 1.000000000000000000, 1.636349903325072848E-16, -0.000000000000000000 ) ) ;
#87912 = CARTESIAN_POINT ( 'NONE',  ( 2.791683348922237240, 5.383931151000785675, -7.208316651077763204 ) ) ;
#87913 = AXIS2_PLACEMENT_3D ( 'NONE', #93241, #33709, #24767 ) ;
#87914 = CARTESIAN_POINT ( 'NONE',  ( 17.84635730667658393, 48.63791097397317031, 6.499999999999931610 ) ) ;
#87915 = ADVANCED_FACE ( 'NONE', ( #67085 ), #82077, .F. ) ;
#87916 = CARTESIAN_POINT ( 'NONE',  ( 15.44008868035555260, 49.73035201082150536, 9.422509992056143702 ) ) ;
#87917 = CARTESIAN_POINT ( 'NONE',  ( 6.565887622018943937, 5.165301336597086568, 12.81628187352647430 ) ) ;
#87918 = CARTESIAN_POINT ( 'NONE',  ( 20.88017736071110519, 65.56368534415483396, 2.639326808657452039E-16 ) ) ;
#87919 = CARTESIAN_POINT ( 'NONE',  ( 2.791683348922240793, 31.63393115100078745, 7.208316651077764092 ) ) ;
#87920 = CARTESIAN_POINT ( 'NONE',  ( -2.816281873526473856, 49.33196800326374643, 3.434112377981055619 ) ) ;
#87922 = CARTESIAN_POINT ( 'NONE',  ( -4.838527690343710219, 14.49999999999999112, 14.19819177887730355 ) ) ;
#87921 = CARTESIAN_POINT ( 'NONE',  ( 10.00000000000000000, 4.758931151000784787, -9.846743663894594434 ) ) ;
#87923 = ORIENTED_EDGE ( 'NONE', *, *, #12207, .T. ) ;
#87924 = CARTESIAN_POINT ( 'NONE',  ( 1.274849032794278747, 57.55509018479938277, -6.499999999999960032 ) ) ;
#87925 = CARTESIAN_POINT ( 'NONE',  ( 10.19513985507828302, 14.49999999999999112, 11.00268709613230200 ) ) ;
#87926 = CARTESIAN_POINT ( 'NONE',  ( 17.96484262340118221, 14.93868534415483751, 7.964842623401181321 ) ) ;
#87927 = CARTESIAN_POINT ( 'NONE',  ( 16.40814093676324603, 57.45696800326375353, -11.09922568453594671 ) ) ;
#87928 = CARTESIAN_POINT ( 'NONE',  ( 12.63842701281683922, 34.55059781766745886, -9.846743663894590881 ) ) ;
#87929 = CARTESIAN_POINT ( 'NONE',  ( -0.8801773607110991993, 17.85535201082150536, -2.915334737309923874 ) ) ;
#87930 = CARTESIAN_POINT ( 'NONE',  ( 20.88017736071110164, 5.355352010821503583, 2.915334737309930979 ) ) ;
#87931 = ORIENTED_EDGE ( 'NONE', *, *, #60181, .F. ) ;
#87932 = VECTOR ( 'NONE', #7624, 1000.000000000000000 ) ;
#87933 = CARTESIAN_POINT ( 'NONE',  ( 10.00000000000000178, 14.31368534415483751, 10.88017736071110342 ) ) ;
#87934 = CARTESIAN_POINT ( 'NONE',  ( 19.42250999205614548, 25.98035201082150891, -5.440088680355545492 ) ) ;
#87936 = CARTESIAN_POINT ( 'NONE',  ( 4.559911319644449179, 22.23035201082150536, -9.422509992056141925 ) ) ;
#87935 = DIRECTION ( 'NONE',  ( 0.000000000000000000, 0.000000000000000000, -1.000000000000000000 ) ) ;
#87937 = VERTEX_POINT ( 'NONE', #15583 ) ;
#87938 = DIRECTION ( 'NONE',  ( 0.000000000000000000, 1.000000000000000000, 0.000000000000000000 ) ) ;
#87940 = EDGE_CURVE ( 'NONE', #70662, #57827, #13480, .T. ) ;
#87939 = CARTESIAN_POINT ( 'NONE',  ( 15.44008868035555793, 26.39701867748817321, -9.422509992056140149 ) ) ;
#87941 = CARTESIAN_POINT ( 'NONE',  ( 0.1532563361054082862, 51.21726448433412315, 2.638427012816831674 ) ) ;
#87942 = AXIS2_PLACEMENT_3D ( 'NONE', #60204, #7217, #91696 ) ;
#87943 = CARTESIAN_POINT ( 'NONE',  ( -8.439016546559974685, 15.00000000000000000, 11.79122553964965014 ) ) ;
#87944 = PRESENTATION_STYLE_ASSIGNMENT (( #74412 ) ) ;
#87945 = CARTESIAN_POINT ( 'NONE',  ( 0.5774900079438590739, 67.64701867748817676, -5.440088680355550821 ) ) ;
#87946 = CARTESIAN_POINT ( 'NONE',  ( -2.266590686148945544, 31.38708216824730002, -7.082119434687050408 ) ) ;
#87947 = CARTESIAN_POINT ( 'NONE',  ( 19.42250999205614193, 45.14701867748817676, 5.440088680355555262 ) ) ;
#87948 = CARTESIAN_POINT ( 'NONE',  ( 4.559911319644449179, 22.23035201082150536, -9.422509992056141925 ) ) ;
#87949 = CARTESIAN_POINT ( 'NONE',  ( 5.795997163830165277, 0.000000000000000000, -13.01802277140705932 ) ) ;
#87950 = ADVANCED_FACE ( 'NONE', ( #8070 ), #98097, .T. ) ;
#87951 = CARTESIAN_POINT ( 'NONE',  ( -8.029120018247418500, -1.061548449190519605, -3.750000000000000444 ) ) ;
#87952 = CARTESIAN_POINT ( 'NONE',  ( 17.20831665107776587, 47.88393115100078745, 7.208316651077764980 ) ) ;
#87953 = CARTESIAN_POINT ( 'NONE',  ( 17.20831665107776587, 7.883931151000784787, 7.208316651077764980 ) ) ;
#87954 = CARTESIAN_POINT ( 'NONE',  ( -11.09922568453595382, -31.29303199673623936, -6.408140936763226492 ) ) ;
#87955 = CARTESIAN_POINT ( 'NONE',  ( 20.88017736071110875, 15.77201867748817143, -2.915334737309920765 ) ) ;
#87956 = CARTESIAN_POINT ( 'NONE',  ( 0.1532563361054082862, 6.217264484334118713, 2.638427012816831674 ) ) ;
#87957 = CARTESIAN_POINT ( 'NONE',  ( 3.591859063236763294, 8.290301336597087456, -11.09922568453595026 ) ) ;
#87958 = CARTESIAN_POINT ( 'NONE',  ( 17.96484262340118221, 61.18868534415482685, -7.964842623401177768 ) ) ;
#87960 = CARTESIAN_POINT ( 'NONE',  ( -1.099225684535947600, 59.54030133659708923, 6.408140936763237150 ) ) ;
#87959 = CARTESIAN_POINT ( 'NONE',  ( 2.035157376598824452, 18.68868534415484106, 7.964842623401179544 ) ) ;
#87961 = CARTESIAN_POINT ( 'NONE',  ( 2.917880565312948704, 32.63708216824730357, 12.26659068614894643 ) ) ;
#87963 = FILL_AREA_STYLE_COLOUR ( '', #49080 ) ;
#87962 = B_SPLINE_CURVE_WITH_KNOTS ( 'NONE', 3,
 ( #13559, #5583, #81551, #44046, #96083, #36566, #13060, #83046, #58555, #66560 ),
 .UNSPECIFIED., .F., .F.,
 ( 4, 3, 3, 4 ),
 ( 5.003707553108400597E-17, 0.0006253016069560918136, 0.001250604074564953165, 0.002501455912506547405 ),
 .UNSPECIFIED. ) ;
#87964 = AXIS2_PLACEMENT_3D ( 'NONE', #19540, #97047, #59014 ) ;
#87965 = CARTESIAN_POINT ( 'NONE',  ( -2.816281873526473856, 54.12363466993041783, 9.499525473075851096E-16 ) ) ;
#87966 = VERTEX_POINT ( 'NONE', #53056 ) ;
#87967 = CARTESIAN_POINT ( 'NONE',  ( -1.099225684535947600, 4.540301336597087456, 6.408140936763237150 ) ) ;
#87968 = DIRECTION ( 'NONE',  ( -0.000000000000000000, 0.000000000000000000, 1.000000000000000000 ) ) ;
#87969 = CARTESIAN_POINT ( 'NONE',  ( 20.88017736071110875, 50.77201867748817676, -2.915334737309920765 ) ) ;
#87970 = CARTESIAN_POINT ( 'NONE',  ( -0.8801773607111009756, 33.06368534415484106, 1.068504757029289695E-15 ) ) ;
#87971 = AXIS2_PLACEMENT_3D ( 'NONE', #98291, #14281, #60255 ) ;
#87972 = CARTESIAN_POINT ( 'NONE',  ( 0.1532563361054082862, 66.21726448433413736, 2.638427012816831674 ) ) ;
#87974 = EDGE_LOOP ( 'NONE', ( #72089, #75784, #23363, #14713, #29345, #64760 ) ) ;
#87973 = EDGE_CURVE ( 'NONE', #59795, #54039, #68079, .T. ) ;
#87975 = CARTESIAN_POINT ( 'NONE',  ( 2.791683348922237240, 15.38393115100078212, -7.208316651077763204 ) ) ;
#87976 = STYLED_ITEM ( 'NONE', ( #27421 ), #21696 ) ;
#87977 = CARTESIAN_POINT ( 'NONE',  ( 0.1532563361054082862, 16.21726448433411960, 2.638427012816831674 ) ) ;
#87978 = CARTESIAN_POINT ( 'NONE',  ( 10.00000000000000178, 12.25893115100078568, 9.846743663894594434 ) ) ;
#87980 = CARTESIAN_POINT ( 'NONE',  ( 0.000000000000000000, 0.5000000000000004441, 0.000000000000000000 ) ) ;
#87979 = CARTESIAN_POINT ( 'NONE',  ( 7.084665262690076126, 59.10535201082150536, 10.88017736071109987 ) ) ;
#87981 = CARTESIAN_POINT ( 'NONE',  ( 1.472469842513823179, 10.59226448433411782, -4.923371831947296329 ) ) ;
#87983 = ORIENTED_EDGE ( 'NONE', *, *, #77791, .F. ) ;
#87982 = CARTESIAN_POINT ( 'NONE',  ( 0.1532563361054100626, 20.80059781766744464, -2.638427012816831230 ) ) ;
#87984 = DIRECTION ( 'NONE',  ( 0.6225146366376183016, 0.000000000000000000, -0.7826081568524148047 ) ) ;
#87985 = CARTESIAN_POINT ( 'NONE',  ( 22.81628187352648496, 1.831968003263753753, -3.434112377981050290 ) ) ;
#87986 = ORIENTED_EDGE ( 'NONE', *, *, #51090, .F. ) ;
#87987 = ORIENTED_EDGE ( 'NONE', *, *, #55694, .F. ) ;
#87988 = CARTESIAN_POINT ( 'NONE',  ( -0.8801773607111008646, 3.272018677488171434, 2.915334737309923430 ) ) ;
#87989 = CARTESIAN_POINT ( 'NONE',  ( 17.08211943468705840, 15.13708216824730179, -12.26659068614894466 ) ) ;
#87990 = CARTESIAN_POINT ( 'NONE',  ( 2.361121941889016362, 0.2301505397289888843, 14.75287579053850706 ) ) ;
#87991 = CARTESIAN_POINT ( 'NONE',  ( 17.08211943468705130, 18.47041550158063572, 12.26659068614894998 ) ) ;
#87992 = B_SPLINE_CURVE_WITH_KNOTS ( 'NONE', 3,
 ( #19996, #81977, #82473, #72993, #73479, #13489 ),
 .UNSPECIFIED., .F., .F.,
 ( 4, 2, 4 ),
 ( 3.409110551421259754E-05, 0.0004400426677360415621, 0.0008459942299578705402 ),
 .UNSPECIFIED. ) ;
#87993 = CARTESIAN_POINT ( 'NONE',  ( -0.3689425029237881626, 27.42874883491397142, 10.36894250292379027 ) ) ;
#87994 =( NAMED_UNIT ( * ) PLANE_ANGLE_UNIT ( ) SI_UNIT ( $, .RADIAN. ) );
#87995 = CARTESIAN_POINT ( 'NONE',  ( 24.16423886937410614, 4.512082168247300906, -3.795296366450302550 ) ) ;
#87996 = CARTESIAN_POINT ( 'NONE',  ( 12.91533473730993009, 31.60535201082150891, -10.88017736071109987 ) ) ;
#87997 = CARTESIAN_POINT ( 'NONE',  ( 8.629999999999991900, 70.25000000000000000, 6.500000000000000888 ) ) ;
#87998 = ORIENTED_EDGE ( 'NONE', *, *, #48567, .F. ) ;
#87999 = CARTESIAN_POINT ( 'NONE',  ( 17.20831665107776587, 17.88393115100078745, 7.208316651077764980 ) ) ;
#88001 = CARTESIAN_POINT ( 'NONE',  ( 12.63842701281683922, 9.550597817667449974, -9.846743663894590881 ) ) ;
#88000 = CARTESIAN_POINT ( 'NONE',  ( 20.88017736071110875, 60.77201867748817676, -2.915334737309920765 ) ) ;
#88002 = VECTOR ( 'NONE', #82358, 1000.000000000000000 ) ;
#88003 = VECTOR ( 'NONE', #55305, 1000.000000000000000 ) ;
#88004 = CARTESIAN_POINT ( 'NONE',  ( 0.5774900079438590739, 17.64701867748817321, -5.440088680355550821 ) ) ;
#88005 = CARTESIAN_POINT ( 'NONE',  ( 22.81628187352647785, 51.41530133659708923, 3.434112377981063169 ) ) ;
#88006 = CARTESIAN_POINT ( 'NONE',  ( 12.63842701281683922, 49.55059781766744464, -9.846743663894590881 ) ) ;
#88007 = LINE ( 'NONE', #42516, #84148 ) ;
#88008 = CARTESIAN_POINT ( 'NONE',  ( 3.591859063236763294, 23.29030133659708568, -11.09922568453595026 ) ) ;
#88009 = CARTESIAN_POINT ( 'NONE',  ( -3.795296366450322534, -39.23791783175269643, -14.16423886937409904 ) ) ;
#88010 = CARTESIAN_POINT ( 'NONE',  ( 19.84674366389459266, 43.71726448433410894, -2.638427012816827677 ) ) ;
#88011 = VECTOR ( 'NONE', #91477, 1000.000000000000000 ) ;
#88012 = CARTESIAN_POINT ( 'NONE',  ( -4.164238869374098151, 11.59541550158063217, -3.795296366450310543 ) ) ;
#88013 = VERTEX_POINT ( 'NONE', #38567 ) ;
#88014 = DIRECTION ( 'NONE',  ( -0.9943711317468825195, -0.1059530667249610481, 0.000000000000000000 ) ) ;
#88015 = CARTESIAN_POINT ( 'NONE',  ( 17.96484262340118221, 46.18868534415484106, -7.964842623401177768 ) ) ;
#88016 = CARTESIAN_POINT ( 'NONE',  ( 15.44008868035555793, 56.39701867748817676, -9.422509992056140149 ) ) ;
#88017 = CARTESIAN_POINT ( 'NONE',  ( -0.3689425029237898834, 51.17874883491397497, -10.36894250292378850 ) ) ;
#88018 = CARTESIAN_POINT ( 'NONE',  ( 7.361572987183169658, 59.96726448433410894, -9.846743663894592657 ) ) ;
#88019 = CARTESIAN_POINT ( 'NONE',  ( -2.816281873526471635, 63.91530133659708923, -3.434112377981056508 ) ) ;
#88020 = CARTESIAN_POINT ( 'NONE',  ( 15.44008868035555260, 34.73035201082151247, 9.422509992056143702 ) ) ;
#88021 = CYLINDRICAL_SURFACE ( 'NONE', #56578, 0.2500000000000002220 ) ;
#88022 = CARTESIAN_POINT ( 'NONE',  ( 5.076628168052704559, 50.17559781766745886, -8.527530157486179263 ) ) ;
#88023 = CARTESIAN_POINT ( 'NONE',  ( -2.915334737309934532, 17.02201867748817321, -10.88017736071109987 ) ) ;
#88024 = CARTESIAN_POINT ( 'NONE',  ( -12.00809552683946357, 0.5000000000000004441, -8.989195838243713155 ) ) ;
#88025 = AXIS2_PLACEMENT_3D ( 'NONE', #43721, #36225, #21227 ) ;
#88026 = ADVANCED_FACE ( 'NONE', ( #31043 ), #32401, .T. ) ;
#88027 = CARTESIAN_POINT ( 'NONE',  ( -0.8801773607111009756, 8.063685344154837509, 1.068504757029289695E-15 ) ) ;
#88028 = CARTESIAN_POINT ( 'NONE',  ( 0.000000000000000000, 15.00000000000000000, 0.000000000000000000 ) ) ;
#88029 = CARTESIAN_POINT ( 'NONE',  ( 7.361572987183169658, -0.03273551566588185635, -9.846743663894592657 ) ) ;
#88030 = CIRCLE ( 'NONE', #76827, 14.49999999999999822 ) ;
#88031 = CARTESIAN_POINT ( 'NONE',  ( 19.84674366389459266, 3.717264484334118713, -2.638427012816827677 ) ) ;
#88032 = CARTESIAN_POINT ( 'NONE',  ( 18.00000000000000000, 78.20644475923673156, -3.828778322547003121 ) ) ;
#88033 = CARTESIAN_POINT ( 'NONE',  ( 14.92337183194729633, 32.67559781766745175, 8.527530157486181039 ) ) ;
#88034 = CARTESIAN_POINT ( 'NONE',  ( 19.42250999205614548, 25.98035201082150891, -5.440088680355545492 ) ) ;
#88035 = CARTESIAN_POINT ( 'NONE',  ( 0.6178305044545838731, 14.74863466993041783, 9.382169495545420901 ) ) ;
#88037 = CARTESIAN_POINT ( 'NONE',  ( -18.89999999999999503, 92.00000000000000000, 7.750000000000000000 ) ) ;
#88036 = CARTESIAN_POINT ( 'NONE',  ( 7.084665262690076126, 39.10535201082150536, 10.88017736071109987 ) ) ;
#88038 = CARTESIAN_POINT ( 'NONE',  ( -8.000000000000000000, 83.99999999999994316, -2.900000000000000799 ) ) ;
#88039 = AXIS2_PLACEMENT_3D ( 'NONE', #36536, #90012, #42 ) ;
#88040 = CARTESIAN_POINT ( 'NONE',  ( 6.565887622018943937, 45.16530133659708923, 12.81628187352647430 ) ) ;
#88041 = VERTEX_POINT ( 'NONE', #55781 ) ;
#88042 = CARTESIAN_POINT ( 'NONE',  ( -0.8801773607111009756, 48.06368534415484817, 1.068504757029289695E-15 ) ) ;
#88044 = DIRECTION ( 'NONE',  ( -0.3987490689252404241, 0.000000000000000000, -0.9170600743851266001 ) ) ;
#88043 = CARTESIAN_POINT ( 'NONE',  ( -2.816281873526471635, 18.91530133659708213, -3.434112377981056508 ) ) ;
#88045 = DIRECTION ( 'NONE',  ( -0.5547001962252291474, -0.8320502943378437211, -0.000000000000000000 ) ) ;
#88046 = CARTESIAN_POINT ( 'NONE',  ( 19.42250999205614548, 30.98035201082150536, -5.440088680355545492 ) ) ;
#88047 = CARTESIAN_POINT ( 'NONE',  ( -4.164238869374099039, 66.80374883491396076, 8.674139862899312516E-16 ) ) ;
#88048 = CARTESIAN_POINT ( 'NONE',  ( 2.791683348922237240, 55.38393115100078745, -7.208316651077763204 ) ) ;
#88049 = CARTESIAN_POINT ( 'NONE',  ( 17.20831665107776587, 9.133931151000787452, -7.208316651077762316 ) ) ;
#88050 = CARTESIAN_POINT ( 'NONE',  ( 19.42250999205614193, 65.14701867748817676, 5.440088680355555262 ) ) ;
#88051 = LINE ( 'NONE', #19073, #26660 ) ;
#88052 = CARTESIAN_POINT ( 'NONE',  ( -0.3689425029237898834, 36.17874883491396787, -10.36894250292378850 ) ) ;
#88053 = AXIS2_PLACEMENT_3D ( 'NONE', #81648, #43166, #90629 ) ;
#88054 = LINE ( 'NONE', #72072, #11612 ) ;
#88055 = FACE_OUTER_BOUND ( 'NONE', #477, .T. ) ;
#88056 = ORIENTED_EDGE ( 'NONE', *, *, #61415, .T. ) ;
#88057 = CARTESIAN_POINT ( 'NONE',  ( -4.164238869374099039, 51.80374883491396787, 8.674139862899312516E-16 ) ) ;
#88059 = EDGE_CURVE ( 'NONE', #27809, #90918, #2369, .T. ) ;
#88058 = CARTESIAN_POINT ( 'NONE',  ( 2.917880565312950480, 45.97041550158063927, -12.26659068614894821 ) ) ;
#88060 = CARTESIAN_POINT ( 'NONE',  ( 10.00000000000000000, 14.75893115100078568, -9.846743663894594434 ) ) ;
#88061 = CARTESIAN_POINT ( 'NONE',  ( -13.22853281710847284, 91.00000000000000000, 7.999999999999996447 ) ) ;
#88062 = LINE ( 'NONE', #65052, #51440 ) ;
#88063 = FACE_OUTER_BOUND ( 'NONE', #62206, .T. ) ;
#88064 = CARTESIAN_POINT ( 'NONE',  ( 22.26659068614895176, 39.72041550158063217, -7.082119434687042414 ) ) ;
#88065 = EDGE_CURVE ( 'NONE', #40449, #45767, #17785, .T. ) ;
#88066 = CARTESIAN_POINT ( 'NONE',  ( 0.000000000000000000, 15.00000000000000000, 0.000000000000000000 ) ) ;
#88067 = CARTESIAN_POINT ( 'NONE',  ( 18.52753015748617571, 3.092264484334118269, 4.923371831947298993 ) ) ;
#88068 = CARTESIAN_POINT ( 'NONE',  ( -4.923371831947302546, 5.175597817667458855, -8.527530157486173934 ) ) ;
#88069 = ORIENTED_EDGE ( 'NONE', *, *, #20020, .F. ) ;
#88070 = DIRECTION ( 'NONE',  ( 0.000000000000000000, 0.000000000000000000, -1.000000000000000000 ) ) ;
#88071 = ORIENTED_EDGE ( 'NONE', *, *, #78811, .F. ) ;
#88072 = SURFACE_SIDE_STYLE ('',( #58064 ) ) ;
#88073 = ORIENTED_EDGE ( 'NONE', *, *, #21271, .T. ) ;
#88075 = CARTESIAN_POINT ( 'NONE',  ( 17.96484262340118221, 21.18868534415483396, -7.964842623401177768 ) ) ;
#88074 = CARTESIAN_POINT ( 'NONE',  ( 2.035157376598824452, 23.68868534415484461, 7.964842623401179544 ) ) ;
#88077 = CARTESIAN_POINT ( 'NONE',  ( -1.099225684535947600, 23.70696800326375708, -6.408140936763238038 ) ) ;
#88076 = CARTESIAN_POINT ( 'NONE',  ( 5.076628168052704559, 50.17559781766745886, -8.527530157486179263 ) ) ;
#88078 = SURFACE_SIDE_STYLE ('',( #33593 ) ) ;
#88079 = VECTOR ( 'NONE', #44236, 1000.000000000000000 ) ;
#88080 = CARTESIAN_POINT ( 'NONE',  ( 15.94536257719940409, 15.00000000000000000, 1.273895096820067296 ) ) ;
#88081 = STYLED_ITEM ( 'NONE', ( #18328 ), #80489 ) ;
#88082 = CARTESIAN_POINT ( 'NONE',  ( -1.099225684535947600, 23.70696800326375708, -6.408140936763238038 ) ) ;
#88083 = ORIENTED_EDGE ( 'NONE', *, *, #71498, .F. ) ;
#88084 = CARTESIAN_POINT ( 'NONE',  ( 0.1532563361054100626, 35.80059781766745175, -2.638427012816831230 ) ) ;
#88085 = CARTESIAN_POINT ( 'NONE',  ( 24.16423886937410614, 64.51208216824728936, -3.795296366450302550 ) ) ;
#88086 = ORIENTED_EDGE ( 'NONE', *, *, #27641, .F. ) ;
#88087 = CARTESIAN_POINT ( 'NONE',  ( 17.08211943468705130, 63.47041550158063927, 12.26659068614894998 ) ) ;
#88088 = ORIENTED_EDGE ( 'NONE', *, *, #47195, .T. ) ;
#88089 = CARTESIAN_POINT ( 'NONE',  ( 20.88017736071110164, 30.35535201082151247, 2.915334737309930979 ) ) ;
#88090 = CARTESIAN_POINT ( 'NONE',  ( 12.91533473730992121, 49.52201867748817676, 10.88017736071110164 ) ) ;
#88091 = CARTESIAN_POINT ( 'NONE',  ( 7.084665262690076126, 54.10535201082151247, 10.88017736071109987 ) ) ;
#88092 = SURFACE_STYLE_USAGE ( .BOTH. , #95099 ) ;
#88093 = CARTESIAN_POINT ( 'NONE',  ( 19.42250999205614193, 40.14701867748817676, 5.440088680355555262 ) ) ;
#88094 = CARTESIAN_POINT ( 'NONE',  ( 1.354709868695531894, 0.3639309939382489034, 14.93870011653156027 ) ) ;
#88095 = ADVANCED_FACE ( 'NONE', ( #24798 ), #68131, .T. ) ;
#88098 = ORIENTED_EDGE ( 'NONE', *, *, #85467, .F. ) ;
#88097 = AXIS2_PLACEMENT_3D ( 'NONE', #16005, #1019, #30499 ) ;
#88096 = LINE ( 'NONE', #12106, #72887 ) ;
#88099 = COLOUR_RGB ( '', 0.31764706, 0.68627451, 0.89019608) ;
#88100 = CARTESIAN_POINT ( 'NONE',  ( 1.472469842513823179, 20.59226448433411960, -4.923371831947296329 ) ) ;
#88101 = ORIENTED_EDGE ( 'NONE', *, *, #92324, .T. ) ;
#88102 = CARTESIAN_POINT ( 'NONE',  ( 11.13639359160540288, -94.02695735602790705, 3.750000000000000000 ) ) ;
#88103 = CARTESIAN_POINT ( 'NONE',  ( 14.92337183194729633, 62.67559781766745886, 8.527530157486181039 ) ) ;
#88104 = CARTESIAN_POINT ( 'NONE',  ( 12.07856007377828078, 15.00000000000000000, -8.022367888854837759 ) ) ;
#88105 = AXIS2_PLACEMENT_3D ( 'NONE', #8777, #334, #39294 ) ;
#88106 = CARTESIAN_POINT ( 'NONE',  ( -7.045329894599615450, -66.66420243593404393, 2.750000000000000000 ) ) ;
#88107 = FACE_OUTER_BOUND ( 'NONE', #97674, .T. ) ;
#88108 = PLANE ( 'NONE',  #96906 ) ;
#88110 = CARTESIAN_POINT ( 'NONE',  ( 7.361572987183170547, 27.05059781766745175, 9.846743663894590881 ) ) ;
#88109 = CARTESIAN_POINT ( 'NONE',  ( 10.00000000000000178, 62.25893115100078745, 9.846743663894594434 ) ) ;
#88111 = CARTESIAN_POINT ( 'NONE',  ( 22.26659068614894466, 58.88708216824729647, 7.082119434687054849 ) ) ;
#88112 = ORIENTED_EDGE ( 'NONE', *, *, #95985, .F. ) ;
#88114 = VECTOR ( 'NONE', #24573, 1000.000000000000000 ) ;
#88113 = CARTESIAN_POINT ( 'NONE',  ( -7.264948169187551485, 0.2306972965111897256, 13.05597881399713955 ) ) ;
#88115 = CARTESIAN_POINT ( 'NONE',  ( 18.52753015748618282, 33.92559781766745886, -4.923371831947291888 ) ) ;
#88116 = CARTESIAN_POINT ( 'NONE',  ( 13.43411237798105340, 60.58196800326376064, 12.81628187352647963 ) ) ;
#88117 = CARTESIAN_POINT ( 'NONE',  ( 13.43411237798106583, 2.665301336597086568, -12.81628187352647252 ) ) ;
#88118 = CARTESIAN_POINT ( 'NONE',  ( 0.1532563361054100626, 5.800597817667452638, -2.638427012816831230 ) ) ;
#88119 = CARTESIAN_POINT ( 'NONE',  ( 0.1129803114748722526, 4.294273331840908980, -6.480634945678659165 ) ) ;
#88120 = CARTESIAN_POINT ( 'NONE',  ( 19.84674366389459621, 3.508931151000785231, 7.409399052514197653E-17 ) ) ;
#88121 = CARTESIAN_POINT ( 'NONE',  ( 18.52753015748618282, 63.92559781766745886, -4.923371831947291888 ) ) ;
#88122 = DIRECTION ( 'NONE',  ( 0.000000000000000000, -1.000000000000000000, 0.000000000000000000 ) ) ;
#88123 = VERTEX_POINT ( 'NONE', #56750 ) ;
#88124 = CARTESIAN_POINT ( 'NONE',  ( 10.00000000000000178, 9.313685344154839285, 10.88017736071110342 ) ) ;
#88125 = CARTESIAN_POINT ( 'NONE',  ( -4.164238869374098151, 6.595415501580634832, -3.795296366450310543 ) ) ;
#88126 = CARTESIAN_POINT ( 'NONE',  ( 2.791683348922240793, 16.63393115100078745, 7.208316651077764092 ) ) ;
#88127 = CARTESIAN_POINT ( 'NONE',  ( 4.559911319644449179, 47.23035201082150536, -9.422509992056141925 ) ) ;
#88129 = CARTESIAN_POINT ( 'NONE',  ( 11.32537994190320418, 12.61453919175019678, -1.000888968711507676 ) ) ;
#88128 = CARTESIAN_POINT ( 'NONE',  ( 0.6178305044545818747, 33.49863466993042493, -9.382169495545419124 ) ) ;
#88130 = DIRECTION ( 'NONE',  ( 0.000000000000000000, -1.000000000000000000, 0.000000000000000000 ) ) ;
#88131 = CARTESIAN_POINT ( 'NONE',  ( 19.88565890683628368, 17.71691075486302935, -6.480892540919849232 ) ) ;
#88132 = CARTESIAN_POINT ( 'NONE',  ( -4.431036607602414357, 14.49999999999999112, -14.33059365769922167 ) ) ;
#88133 = CARTESIAN_POINT ( 'NONE',  ( 19.84674366389459266, 58.30059781766745886, 2.638427012816836559 ) ) ;
#88134 = CARTESIAN_POINT ( 'NONE',  ( 5.076628168052704559, 20.17559781766745175, -8.527530157486179263 ) ) ;
#88135 = CARTESIAN_POINT ( 'NONE',  ( 7.964842623401181321, -20.06131465584516249, 7.964842623401174215 ) ) ;
#88136 = CARTESIAN_POINT ( 'NONE',  ( 21.09922568453595559, 17.04030133659708923, -6.408140936763230044 ) ) ;
#88137 = DIRECTION ( 'NONE',  ( -6.938893903907222067E-15, 1.000000000000000000, 0.000000000000000000 ) ) ;
#88138 = CARTESIAN_POINT ( 'NONE',  ( 4.559911319644449179, 22.23035201082150536, -9.422509992056141925 ) ) ;
#88139 = CARTESIAN_POINT ( 'NONE',  ( -4.746257547686163925, 0.000000000000000000, -2.685303318749144186 ) ) ;
#88140 = CARTESIAN_POINT ( 'NONE',  ( 2.917880565312950480, 50.97041550158064638, -12.26659068614894821 ) ) ;
#88141 = ADVANCED_FACE ( 'NONE', ( #32267 ), #49251, .T. ) ;
#88142 = CARTESIAN_POINT ( 'NONE',  ( 6.905582103719410725, -69.44843085160002261, -3.750000000000002220 ) ) ;
#88143 = CARTESIAN_POINT ( 'NONE',  ( 7.361572987183170547, 47.05059781766745175, 9.846743663894590881 ) ) ;
#88144 = CARTESIAN_POINT ( 'NONE',  ( 19.38216949554541557, 37.24863466993041783, -9.382169495545420901 ) ) ;
#88145 = CARTESIAN_POINT ( 'NONE',  ( 12.91533473730993009, 31.60535201082150891, -10.88017736071109987 ) ) ;
#88146 = AXIS2_PLACEMENT_3D ( 'NONE', #47732, #33695, #79710 ) ;
#88147 = CARTESIAN_POINT ( 'NONE',  ( 5.076628168052704559, 55.17559781766745175, -8.527530157486179263 ) ) ;
#88148 = CARTESIAN_POINT ( 'NONE',  ( 0.5774900079438607392, 48.48035201082150536, 5.440088680355550821 ) ) ;
#88149 = CARTESIAN_POINT ( 'NONE',  ( 16.40814093676323893, 0.7903013365970867898, 11.09922568453595026 ) ) ;
#88150 = CARTESIAN_POINT ( 'NONE',  ( 17.08211943468705130, 33.47041550158063927, 12.26659068614894998 ) ) ;
#88151 = CARTESIAN_POINT ( 'NONE',  ( -8.375939845167600595, 15.00000000000000000, -11.52849216984310310 ) ) ;
#88152 = CARTESIAN_POINT ( 'NONE',  ( 5.076628168052703671, 21.84226448433411960, 8.527530157486179263 ) ) ;
#88153 = CARTESIAN_POINT ( 'NONE',  ( -2.816281873526473856, 64.33196800326376774, 3.434112377981055619 ) ) ;
#88154 = B_SPLINE_CURVE_WITH_KNOTS ( 'NONE', 3,
 ( #22537, #45513, #31969, #91515 ),
 .UNSPECIFIED., .F., .F.,
 ( 4, 4 ),
 ( 6.942281208919283290E-19, 7.431658353028133043E-05 ),
 .UNSPECIFIED. ) ;
#88155 = CARTESIAN_POINT ( 'NONE',  ( 0.1532563361054082862, 66.21726448433413736, 2.638427012816831674 ) ) ;
#88156 = ORIENTED_EDGE ( 'NONE', *, *, #35042, .F. ) ;
#88157 = DIRECTION ( 'NONE',  ( 0.000000000000000000, 0.000000000000000000, 1.000000000000000000 ) ) ;
#88158 = CARTESIAN_POINT ( 'NONE',  ( 7.084665262690076126, 12.02201867748817321, -10.88017736071110164 ) ) ;
#88159 = CARTESIAN_POINT ( 'NONE',  ( 24.16423886937410614, 24.51208216824730002, -3.795296366450302550 ) ) ;
#88160 = CARTESIAN_POINT ( 'NONE',  ( 18.52753015748618282, 13.92559781766745175, -4.923371831947291888 ) ) ;
#88161 = CARTESIAN_POINT ( 'NONE',  ( 7.361572987183169658, 54.96726448433413026, -9.846743663894592657 ) ) ;
#88162 = CARTESIAN_POINT ( 'NONE',  ( 2.035157376598822676, 27.43868534415483396, -7.964842623401177768 ) ) ;
#88163 = CARTESIAN_POINT ( 'NONE',  ( -13.55255535720598026, 15.00000000000000000, 4.403492169842870396 ) ) ;
#88164 = CARTESIAN_POINT ( 'NONE',  ( 7.882504294823946545, 2.625802136488331051E-16, -12.32089577884791787 ) ) ;
#88165 = ORIENTED_EDGE ( 'NONE', *, *, #32285, .T. ) ;
#88166 = TOROIDAL_SURFACE ( 'NONE', #45064, 14.49999999999999822, 0.5000000000000000000 ) ;
#88167 = CARTESIAN_POINT ( 'NONE',  ( 6.655501998723816648, -69.44085999572126866, 2.500000000000000000 ) ) ;
#88168 = CARTESIAN_POINT ( 'NONE',  ( 7.361572987183170547, 52.05059781766745175, 9.846743663894590881 ) ) ;
#88169 = ORIENTED_EDGE ( 'NONE', *, *, #80502, .T. ) ;
#88170 = VERTEX_POINT ( 'NONE', #62776 ) ;
#88171 = CARTESIAN_POINT ( 'NONE',  ( 3.014428414850127691, 11.46346884451820713, -11.25000000000000000 ) ) ;
#88172 = CARTESIAN_POINT ( 'NONE',  ( 20.36894250292379382, 13.67874883491396965, 10.36894250292379205 ) ) ;
#88174 = EDGE_CURVE ( 'NONE', #93746, #15284, #87243, .T. ) ;
#88173 = CARTESIAN_POINT ( 'NONE',  ( 24.16423886937410614, 4.303748834913967869, 8.672049930838204340E-16 ) ) ;
#88175 = CARTESIAN_POINT ( 'NONE',  ( 4.559911319644449179, 43.89701867748816966, 9.422509992056141925 ) ) ;
#88176 = CARTESIAN_POINT ( 'NONE',  ( 2.917880565312950480, 60.97041550158063927, -12.26659068614894821 ) ) ;
#88177 = CARTESIAN_POINT ( 'NONE',  ( 17.20831665107776587, 59.13393115100078745, -7.208316651077762316 ) ) ;
#88178 = CARTESIAN_POINT ( 'NONE',  ( 14.92337183194729988, 29.34226448433411960, -8.527530157486177487 ) ) ;
#88180 = CARTESIAN_POINT ( 'NONE',  ( -2.816281873526471635, 8.915301336597083903, -3.434112377981056508 ) ) ;
#88179 = CARTESIAN_POINT ( 'NONE',  ( 20.88017736071110164, 35.35535201082150536, 2.915334737309930979 ) ) ;
#88181 = CARTESIAN_POINT ( 'NONE',  ( 10.00000000000000178, 3.053748834913967425, 14.16423886937410082 ) ) ;
#88182 = CARTESIAN_POINT ( 'NONE',  ( 10.00000000000000000, 50.55374883491396787, -14.16423886937410082 ) ) ;
#88183 = CARTESIAN_POINT ( 'NONE',  ( 15.44008868035555260, 9.730352010821505360, 9.422509992056143702 ) ) ;
#88184 = CARTESIAN_POINT ( 'NONE',  ( -2.815433093576926282, 0.3640475087720981828, -14.73340885523754196 ) ) ;
#88185 = PRESENTATION_LAYER_ASSIGNMENT (  '', '', ( #19531 ) ) ;
#88186 = CARTESIAN_POINT ( 'NONE',  ( 0.8218345515129070744, 14.95077488074852923, -14.72992491912910573 ) ) ;
#88187 = EDGE_CURVE ( 'NONE', #76621, #88425, #40943, .T. ) ;
#88188 = PRESENTATION_LAYER_ASSIGNMENT (  '', '', ( #97791 ) ) ;
#88189 = CARTESIAN_POINT ( 'NONE',  ( -9.846743663894594434, -33.99106884899921255, 3.469446951953614189E-15 ) ) ;
#88190 = ORIENTED_EDGE ( 'NONE', *, *, #63670, .T. ) ;
#88191 = CYLINDRICAL_SURFACE ( 'NONE', #36362, 6.349999999999995204 ) ;
#88192 = CIRCLE ( 'NONE', #70654, 2.999999999999999112 ) ;
#88193 = EDGE_LOOP ( 'NONE', ( #9979, #18128, #14818, #55325 ) ) ;
#88194 = CARTESIAN_POINT ( 'NONE',  ( 19.84674366389459266, 28.71726448433411960, -2.638427012816827677 ) ) ;
#88195 = ORIENTED_EDGE ( 'NONE', *, *, #68784, .T. ) ;
#88196 = CARTESIAN_POINT ( 'NONE',  ( 24.16423886937410614, 34.51208216824731068, -3.795296366450302550 ) ) ;
#88197 = CARTESIAN_POINT ( 'NONE',  ( 10.00000000000000000, 39.75893115100078745, -9.846743663894594434 ) ) ;
#88198 = CARTESIAN_POINT ( 'NONE',  ( 2.035157376598822676, 52.43868534415483396, -7.964842623401177768 ) ) ;
#88199 = DIRECTION ( 'NONE',  ( 0.000000000000000000, 1.000000000000000000, -0.000000000000000000 ) ) ;
#88200 = AXIS2_PLACEMENT_3D ( 'NONE', #94774, #970, #64261 ) ;
#88201 = CARTESIAN_POINT ( 'NONE',  ( 15.44008868035555260, 49.73035201082150536, 9.422509992056143702 ) ) ;
#88202 = CARTESIAN_POINT ( 'NONE',  ( 6.565887622018943937, 63.08196800326376064, -12.81628187352647608 ) ) ;
#88203 = CARTESIAN_POINT ( 'NONE',  ( 6.408140936763243367, 5.790301336597095450, 11.09922568453594494 ) ) ;
#88204 = ORIENTED_EDGE ( 'NONE', *, *, #71251, .T. ) ;
#88205 = CARTESIAN_POINT ( 'NONE',  ( 20.36894250292379382, 18.67874883491397142, 10.36894250292379205 ) ) ;
#88206 = ORIENTED_EDGE ( 'NONE', *, *, #7616, .T. ) ;
#88207 = CARTESIAN_POINT ( 'NONE',  ( 6.565887622018943937, 50.16530133659708213, 12.81628187352647430 ) ) ;
#88208 = EDGE_CURVE ( 'NONE', #10227, #59535, #11249, .T. ) ;
#88209 = CARTESIAN_POINT ( 'NONE',  ( 17.96484262340118221, 21.18868534415483396, -7.964842623401177768 ) ) ;
#88210 = CARTESIAN_POINT ( 'NONE',  ( 19.84674366389459266, 23.30059781766745530, 2.638427012816836559 ) ) ;
#88211 = CARTESIAN_POINT ( 'NONE',  ( 12.91533473730993009, 16.60535201082150891, -10.88017736071109987 ) ) ;
#88212 = CARTESIAN_POINT ( 'NONE',  ( -2.816281873526473856, 49.12363466993042493, 9.499525473075851096E-16 ) ) ;
#88213 = DIRECTION ( 'NONE',  ( -0.000000000000000000, -0.000000000000000000, 1.000000000000000000 ) ) ;
#88214 = CARTESIAN_POINT ( 'NONE',  ( 0.1532563361054100626, 40.80059781766745886, -2.638427012816831230 ) ) ;
#88215 = EDGE_CURVE ( 'NONE', #65562, #23769, #32764, .T. ) ;
#88216 = CARTESIAN_POINT ( 'NONE',  ( -12.79448242979012562, 14.76930270348881002, 7.716169648622011046 ) ) ;
#88217 = AXIS2_PLACEMENT_3D ( 'NONE', #76904, #24419, #37947 ) ;
#88218 = CARTESIAN_POINT ( 'NONE',  ( 10.00000000000000000, 66.81368534415484817, -10.88017736071110342 ) ) ;
#88219 = DIRECTION ( 'NONE',  ( 0.000000000000000000, 0.000000000000000000, -1.000000000000000000 ) ) ;
#88220 = CARTESIAN_POINT ( 'NONE',  ( 0.000000000000000000, 35.00000000000000000, 0.000000000000000000 ) ) ;
#88221 = CARTESIAN_POINT ( 'NONE',  ( 2.791683348922240793, 21.63393115100078745, 7.208316651077764092 ) ) ;
#88222 =( BOUNDED_CURVE ( )  B_SPLINE_CURVE ( 3, ( #39082, #46088, #8092, #40558 ),
 .UNSPECIFIED., .F., .F. ) 
 B_SPLINE_CURVE_WITH_KNOTS ( ( 4, 4 ),
 ( 3.141592653589793116, 4.712388980384689674 ),
 .UNSPECIFIED. ) 
 CURVE ( )  GEOMETRIC_REPRESENTATION_ITEM ( )  RATIONAL_B_SPLINE_CURVE ( ( 1.000000000000000000, 0.8047378541243649375, 0.8047378541243649375, 1.000000000000000000 ) ) 
 REPRESENTATION_ITEM ( '' )  );
#88223 = CARTESIAN_POINT ( 'NONE',  ( -2.816281873526471635, 18.91530133659708213, -3.434112377981056508 ) ) ;
#88224 = CARTESIAN_POINT ( 'NONE',  ( -6.982525766850297799, -88.11956318484570261, 3.750000000000000000 ) ) ;
#88225 = EDGE_CURVE ( 'NONE', #76195, #73208, #3771, .T. ) ;
#88226 = CARTESIAN_POINT ( 'NONE',  ( 1.472469842513823179, 46.42559781766745175, 4.923371831947296329 ) ) ;
#88227 = CARTESIAN_POINT ( 'NONE',  ( -14.93928340878672323, 0.2306972965111904195, 0.2363597353048689786 ) ) ;
#88228 = CARTESIAN_POINT ( 'NONE',  ( -4.164238869374099039, 16.80374883491396787, 8.674139862899312516E-16 ) ) ;
#88229 = CARTESIAN_POINT ( 'NONE',  ( 19.84674366389459266, 38.30059781766745175, 2.638427012816836559 ) ) ;
#88230 = CARTESIAN_POINT ( 'NONE',  ( 21.09922568453595559, 37.04030133659708923, -6.408140936763230044 ) ) ;
#88232 = CARTESIAN_POINT ( 'NONE',  ( 0.8952175423694819223, 23.52576239577082262, 5.990408912944316100 ) ) ;
#88231 = CARTESIAN_POINT ( 'NONE',  ( 0.000000000000000000, 15.00000000000000000, 0.000000000000000000 ) ) ;
#88233 = CARTESIAN_POINT ( 'NONE',  ( 0.5774900079438590739, 57.64701867748817676, -5.440088680355550821 ) ) ;
#88234 = CARTESIAN_POINT ( 'NONE',  ( 16.40814093676323893, 5.790301336597087456, 11.09922568453595026 ) ) ;
#88235 = DIRECTION ( 'NONE',  ( 0.000000000000000000, 0.000000000000000000, -1.000000000000000000 ) ) ;
#88236 = ORIENTED_EDGE ( 'NONE', *, *, #65798, .F. ) ;
#88237 = CARTESIAN_POINT ( 'NONE',  ( 0.1532563361054100626, 35.80059781766745175, -2.638427012816831230 ) ) ;
#88238 = CARTESIAN_POINT ( 'NONE',  ( 12.91533473730993009, 31.60535201082150891, -10.88017736071109987 ) ) ;
#88239 = CARTESIAN_POINT ( 'NONE',  ( -1.099225684535947600, 34.54030133659708923, 6.408140936763237150 ) ) ;
#88240 = PRESENTATION_LAYER_ASSIGNMENT (  '', '', ( #37163 ) ) ;
#88241 = CARTESIAN_POINT ( 'NONE',  ( 1.472469842513823179, 35.59226448433412315, -4.923371831947296329 ) ) ;
#88242 = CARTESIAN_POINT ( 'NONE',  ( -2.393480905993250918, 0.5000000000000004441, 14.80781041047749724 ) ) ;
#88243 = CARTESIAN_POINT ( 'NONE',  ( 4.559911319644449179, 37.23035201082150536, -9.422509992056141925 ) ) ;
#88244 = TOROIDAL_SURFACE ( 'NONE', #33990, 4.190000000000001279, 0.2500000000000000000 ) ;
#88245 = VERTEX_POINT ( 'NONE', #33733 ) ;
#88246 = CARTESIAN_POINT ( 'NONE',  ( -9.742785792574931492, 5.534700295649322754, 5.625000000000008882 ) ) ;
#88247 = DIRECTION ( 'NONE',  ( 0.8070303256584299145, -0.5905099943842175847, 0.000000000000000000 ) ) ;
#88249 = CARTESIAN_POINT ( 'NONE',  ( 17.96484262340118221, 31.18868534415483751, -7.964842623401177768 ) ) ;
#88248 = CARTESIAN_POINT ( 'NONE',  ( 0.1532563361054082862, 56.21726448433411605, 2.638427012816831674 ) ) ;
#88250 = LINE ( 'NONE', #80758, #31253 ) ;
#88251 = CARTESIAN_POINT ( 'NONE',  ( 20.88017736071110164, 65.35535201082150536, 2.915334737309930979 ) ) ;
#88253 = DIRECTION ( 'NONE',  ( -0.000000000000000000, -0.000000000000000000, -1.000000000000000000 ) ) ;
#88252 = CARTESIAN_POINT ( 'NONE',  ( 10.00000000000000000, 21.81368534415484106, -10.88017736071110342 ) ) ;
#88254 = CARTESIAN_POINT ( 'NONE',  ( 1.472469842513823179, 6.425597817667451750, 4.923371831947296329 ) ) ;
#88255 = CARTESIAN_POINT ( 'NONE',  ( -3.750000000000000000, 10.00000000000000000, -2.500000000000000000 ) ) ;
#88256 = VECTOR ( 'NONE', #2345, 1000.000000000000000 ) ;
#88257 = CARTESIAN_POINT ( 'NONE',  ( 0.1532563361054083140, 56.00893115100078745, 1.131784320476157264E-15 ) ) ;
#88259 = CARTESIAN_POINT ( 'NONE',  ( 5.679672690684601122, -28.64560013356482315, 3.750000000000000000 ) ) ;
#88258 = CARTESIAN_POINT ( 'NONE',  ( 6.204703633549690345, 57.84541550158063927, 14.16423886937410082 ) ) ;
#88260 = DIRECTION ( 'NONE',  ( -0.000000000000000000, -0.000000000000000000, -1.000000000000000000 ) ) ;
#88261 = CARTESIAN_POINT ( 'NONE',  ( 13.79529636645031943, 15.34541550158063750, -14.16423886937409904 ) ) ;
#88262 = EDGE_CURVE ( 'NONE', #46930, #44781, #66473, .T. ) ;
#88263 = CARTESIAN_POINT ( 'NONE',  ( 13.79529636645031943, 40.34541550158063217, -14.16423886937409904 ) ) ;
#88264 = CARTESIAN_POINT ( 'NONE',  ( -1.099225684535947600, 8.706968003263753531, -6.408140936763238038 ) ) ;
#88265 = B_SPLINE_CURVE_WITH_KNOTS ( 'NONE', 3,
 ( #65541, #41601, #95056, #4081, #48578, #64060 ),
 .UNSPECIFIED., .F., .F.,
 ( 4, 2, 4 ),
 ( 0.0002800065468475842123, 0.0006862118402974218614, 0.001092417133747259619 ),
 .UNSPECIFIED. ) ;
#88266 = CARTESIAN_POINT ( 'NONE',  ( -6.030735014468242561, -39.80307827768279338, 2.750000000000000444 ) ) ;
#88267 = CARTESIAN_POINT ( 'NONE',  ( 2.035157376598824452, 3.688685344154837953, 7.964842623401179544 ) ) ;
#88268 = EDGE_CURVE ( 'NONE', #38312, #41376, #43038, .T. ) ;
#88269 = CARTESIAN_POINT ( 'NONE',  ( 1.472469842513823179, 41.42559781766745886, 4.923371831947296329 ) ) ;
#88271 = CARTESIAN_POINT ( 'NONE',  ( -12.83294900548052730, 0.5000000000000004441, -7.766300266068542513 ) ) ;
#88270 =( NAMED_UNIT ( * ) PLANE_ANGLE_UNIT ( ) SI_UNIT ( $, .RADIAN. ) );
#88272 = CARTESIAN_POINT ( 'NONE',  ( 4.559911319644449179, 57.23035201082150536, -9.422509992056141925 ) ) ;
#88273 = LINE ( 'NONE', #11783, #67577 ) ;
#88274 = UNCERTAINTY_MEASURE_WITH_UNIT (LENGTH_MEASURE( 1.000000000000000082E-05 ), #41169, 'distance_accuracy_value', 'NONE');
#88275 = CARTESIAN_POINT ( 'NONE',  ( 22.81628187352647785, 61.41530133659709634, 3.434112377981063169 ) ) ;
#88276 = CARTESIAN_POINT ( 'NONE',  ( -1.099225684535947600, 19.54030133659708568, 6.408140936763237150 ) ) ;
#88277 = CARTESIAN_POINT ( 'NONE',  ( 0.1532563361054082862, 31.21726448433412315, 2.638427012816831674 ) ) ;
#88278 = ORIENTED_EDGE ( 'NONE', *, *, #77829, .F. ) ;
#88279 = CARTESIAN_POINT ( 'NONE',  ( 2.791683348922240793, 1.633931151000784565, 7.208316651077764092 ) ) ;
#88280 = CARTESIAN_POINT ( 'NONE',  ( 18.06765999051785343, 3.991275129254488796, 6.500000000000000888 ) ) ;
#88281 = CARTESIAN_POINT ( 'NONE',  ( 2.917880565312948704, 67.63708216824730357, 12.26659068614894643 ) ) ;
#88282 = CARTESIAN_POINT ( 'NONE',  ( 7.084665262690076126, 12.02201867748817143, -10.88017736071110164 ) ) ;
#88283 = AXIS2_PLACEMENT_3D ( 'NONE', #93363, #26339, #16394 ) ;
#88284 = CARTESIAN_POINT ( 'NONE',  ( 6.204703633549690345, 45.76208216824729647, -14.16423886937410259 ) ) ;
#88285 = CARTESIAN_POINT ( 'NONE',  ( 15.44008868035555793, 26.39701867748817321, -9.422509992056140149 ) ) ;
#88286 = CARTESIAN_POINT ( 'NONE',  ( 0.5774900079438607392, 68.48035201082150536, 5.440088680355550821 ) ) ;
#88287 = CARTESIAN_POINT ( 'NONE',  ( 2.962741594153077251, 15.00000000000000000, -13.93860331045673107 ) ) ;
#88288 = CARTESIAN_POINT ( 'NONE',  ( 18.04007052943773459, 49.00257860105350005, -5.767676674365834089 ) ) ;
#88289 = CARTESIAN_POINT ( 'NONE',  ( 0.1532563361054082862, 16.21726448433411960, 2.638427012816831674 ) ) ;
#88290 = DIRECTION ( 'NONE',  ( 0.1927083333333330095, -0.9812560818990572198, 0.000000000000000000 ) ) ;
#88291 = CARTESIAN_POINT ( 'NONE',  ( 12.63842701281683922, 9.550597817667449974, -9.846743663894590881 ) ) ;
#88292 = CARTESIAN_POINT ( 'NONE',  ( 18.52753015748618282, 43.92559781766745175, -4.923371831947291888 ) ) ;
#88293 = CARTESIAN_POINT ( 'NONE',  ( 7.361572987183170547, 62.05059781766745886, 9.846743663894590881 ) ) ;
#88294 = CARTESIAN_POINT ( 'NONE',  ( 12.91533473730992121, 29.52201867748817321, 10.88017736071110164 ) ) ;
#88295 = UNCERTAINTY_MEASURE_WITH_UNIT (LENGTH_MEASURE( 1.000000000000000082E-05 ), #32216, 'distance_accuracy_value', 'NONE');
#88296 = TOROIDAL_SURFACE ( 'NONE', #11639, 1.750000000000000888, 0.2500000000000000000 ) ;
#88297 = ORIENTED_EDGE ( 'NONE', *, *, #26710, .T. ) ;
#88298 = CARTESIAN_POINT ( 'NONE',  ( 13.43411237798106583, 42.66530133659707502, -12.81628187352647252 ) ) ;
#88300 = EDGE_CURVE ( 'NONE', #82789, #25872, #50221, .T. ) ;
#88299 = DIRECTION ( 'NONE',  ( 0.000000000000000000, 0.000000000000000000, 1.000000000000000000 ) ) ;
#88301 = CARTESIAN_POINT ( 'NONE',  ( -0.8801773607111008646, 63.27201867748817676, 2.915334737309923430 ) ) ;
#88302 = CARTESIAN_POINT ( 'NONE',  ( -2.816281873526473856, 39.12363466993041783, 9.499525473075851096E-16 ) ) ;
#88304 = CARTESIAN_POINT ( 'NONE',  ( 14.92337183194729988, 24.34226448433411960, -8.527530157486177487 ) ) ;
#88303 = CARTESIAN_POINT ( 'NONE',  ( -2.266590686148945544, 57.22041550158063217, 7.082119434687048631 ) ) ;
#88305 = DIRECTION ( 'NONE',  ( -0.000000000000000000, -1.000000000000000000, -0.000000000000000000 ) ) ;
#88306 = DIRECTION ( 'NONE',  ( -0.000000000000000000, -0.000000000000000000, -1.000000000000000000 ) ) ;
#88307 = CARTESIAN_POINT ( 'NONE',  ( -2.266590686148945544, 16.38708216824730357, -7.082119434687050408 ) ) ;
#88308 = CARTESIAN_POINT ( 'NONE',  ( -2.266590686148945544, 31.38708216824730002, -7.082119434687050408 ) ) ;
#88309 = CARTESIAN_POINT ( 'NONE',  ( 12.63842701281683034, 47.46726448433412315, 9.846743663894596210 ) ) ;
#88310 = CARTESIAN_POINT ( 'NONE',  ( 4.145753578647971338, -0.8370341202350775056, -2.500000000000000000 ) ) ;
#88311 = CARTESIAN_POINT ( 'NONE',  ( 20.88017736071110164, 20.35535201082150891, 2.915334737309930979 ) ) ;
#88312 = EDGE_CURVE ( 'NONE', #34886, #65300, #27621, .T. ) ;
#88313 = CARTESIAN_POINT ( 'NONE',  ( 10.00000000000000178, 59.31368534415484106, 10.88017736071110342 ) ) ;
#88314 = VERTEX_POINT ( 'NONE', #73220 ) ;
#88315 = CARTESIAN_POINT ( 'NONE',  ( 16.40814093676323893, 45.79030133659708923, 11.09922568453595026 ) ) ;
#88316 = VERTEX_POINT ( 'NONE', #4748 ) ;
#88317 = CARTESIAN_POINT ( 'NONE',  ( 12.91533473730992121, 54.52201867748816255, 10.88017736071110164 ) ) ;
#88318 = VERTEX_POINT ( 'NONE', #65718 ) ;
#88319 =( LENGTH_UNIT ( ) NAMED_UNIT ( * ) SI_UNIT ( .MILLI., .METRE. ) );
#88320 = DIRECTION ( 'NONE',  ( -0.000000000000000000, -1.000000000000000000, -0.000000000000000000 ) ) ;
#88321 = DIRECTION ( 'NONE',  ( 0.6093027842603870869, 0.6796026999251361111, 0.4085220769395525586 ) ) ;
#88322 = ORIENTED_EDGE ( 'NONE', *, *, #69692, .F. ) ;
#88323 = CARTESIAN_POINT ( 'NONE',  ( 2.035157376598822676, 62.43868534415483396, -7.964842623401177768 ) ) ;
#88324 = CARTESIAN_POINT ( 'NONE',  ( 19.42250999205614193, 15.14701867748817143, 5.440088680355555262 ) ) ;
#88325 = CARTESIAN_POINT ( 'NONE',  ( -10.32896413005680536, 12.24545670184114243, -5.963430220938272797 ) ) ;
#88326 = CARTESIAN_POINT ( 'NONE',  ( 3.558677480090427725, 70.40124509038875544, 5.000000000000000000 ) ) ;
#88327 = CARTESIAN_POINT ( 'NONE',  ( 0.5774900079438590739, 7.647018677488171434, -5.440088680355550821 ) ) ;
#88328 = CARTESIAN_POINT ( 'NONE',  ( 10.00000000000000178, 27.25893115100078390, 9.846743663894594434 ) ) ;
#88329 = CARTESIAN_POINT ( 'NONE',  ( 22.26659068614895176, 19.72041550158063572, -7.082119434687042414 ) ) ;
#88330 = AXIS2_PLACEMENT_3D ( 'NONE', #84196, #68692, #39185 ) ;
#88331 = CARTESIAN_POINT ( 'NONE',  ( 10.00000000000000178, 19.31368534415484106, 10.88017736071110342 ) ) ;
#88332 = CARTESIAN_POINT ( 'NONE',  ( 5.076628168052704559, 65.17559781766745175, -8.527530157486179263 ) ) ;
#88333 = VERTEX_POINT ( 'NONE', #43716 ) ;
#88334 = CARTESIAN_POINT ( 'NONE',  ( 6.565887622018943937, -1.918031996736246692, -12.81628187352647608 ) ) ;
#88335 = ORIENTED_EDGE ( 'NONE', *, *, #25755, .T. ) ;
#88336 = CIRCLE ( 'NONE', #93115, 15.00000000000000000 ) ;
#88337 = CARTESIAN_POINT ( 'NONE',  ( 20.88017736071110519, 50.56368534415484106, 2.639326808657452039E-16 ) ) ;
#88338 = DIRECTION ( 'NONE',  ( -0.000000000000000000, -1.000000000000000000, -0.000000000000000000 ) ) ;
#88339 = CARTESIAN_POINT ( 'NONE',  ( 3.591859063236763294, 38.29030133659708923, -11.09922568453595026 ) ) ;
#88340 = DIRECTION ( 'NONE',  ( -0.000000000000000000, 0.000000000000000000, -1.000000000000000000 ) ) ;
#88341 = CARTESIAN_POINT ( 'NONE',  ( 2.035157376598822676, 57.43868534415484106, -7.964842623401177768 ) ) ;
#88342 = CARTESIAN_POINT ( 'NONE',  ( 0.5774900079438590739, 17.64701867748817321, -5.440088680355550821 ) ) ;
#88343 = EDGE_CURVE ( 'NONE', #47253, #14084, #81297, .T. ) ;
#88344 = CARTESIAN_POINT ( 'NONE',  ( -2.816281873526471635, 43.91530133659708923, -3.434112377981056508 ) ) ;
#88345 = CARTESIAN_POINT ( 'NONE',  ( 4.559911319644449179, 32.23035201082150536, -9.422509992056141925 ) ) ;
#88346 = CARTESIAN_POINT ( 'NONE',  ( -8.564643372776702179, 0.5000000000000004441, 12.31449893000734797 ) ) ;
#88347 = CARTESIAN_POINT ( 'NONE',  ( 6.565887622018943937, 38.08196800326376064, -12.81628187352647608 ) ) ;
#88348 = CARTESIAN_POINT ( 'NONE',  ( 12.91533473730992121, 34.52201867748817676, 10.88017736071110164 ) ) ;
#88349 = CARTESIAN_POINT ( 'NONE',  ( 17.20831665107776587, 57.88393115100078745, 7.208316651077764980 ) ) ;
#88350 = B_SPLINE_CURVE_WITH_KNOTS ( 'NONE', 3,
 ( #82593, #52100, #7100, #58606, #44592, #36100 ),
 .UNSPECIFIED., .F., .F.,
 ( 4, 2, 4 ),
 ( 3.409110551496223525E-05, 0.0004400426677367995820, 0.0008459942299586368543 ),
 .UNSPECIFIED. ) ;
#88351 = ORIENTED_EDGE ( 'NONE', *, *, #63202, .T. ) ;
#88352 = DIRECTION ( 'NONE',  ( 0.000000000000000000, 0.000000000000000000, 1.000000000000000000 ) ) ;
#88353 = CARTESIAN_POINT ( 'NONE',  ( 19.84674366389459266, 8.300597817667451750, 2.638427012816836559 ) ) ;
#88354 = CARTESIAN_POINT ( 'NONE',  ( 7.361572987183169658, 64.96726448433412315, -9.846743663894592657 ) ) ;
#88356 = CARTESIAN_POINT ( 'NONE',  ( 17.20831665107776587, 47.88393115100078745, 7.208316651077764980 ) ) ;
#88355 = LINE ( 'NONE', #87852, #86708 ) ;
#88357 = CARTESIAN_POINT ( 'NONE',  ( 7.084665262690076126, 29.10535201082150181, 10.88017736071109987 ) ) ;
#88358 = DIRECTION ( 'NONE',  ( -0.000000000000000000, -1.000000000000000000, -0.000000000000000000 ) ) ;
#88359 = CARTESIAN_POINT ( 'NONE',  ( -0.1038446121089068586, 39.24302437010792488, -6.337995344473776882 ) ) ;
#88360 = DIRECTION ( 'NONE',  ( 0.000000000000000000, -1.000000000000000000, 0.000000000000000000 ) ) ;
#88361 = PRESENTATION_LAYER_ASSIGNMENT (  '', '', ( #14950 ) ) ;
#88363 = CARTESIAN_POINT ( 'NONE',  ( 19.84674366389459266, 3.717264484334118713, -2.638427012816827677 ) ) ;
#88362 = CARTESIAN_POINT ( 'NONE',  ( 17.20831665107776587, 39.13393115100079456, -7.208316651077762316 ) ) ;
#88364 = LINE ( 'NONE', #21349, #93623 ) ;
#88366 = VERTEX_POINT ( 'NONE', #11744 ) ;
#88365 = CARTESIAN_POINT ( 'NONE',  ( 14.92337183194729988, 64.34226448433412315, -8.527530157486177487 ) ) ;
#88367 = VECTOR ( 'NONE', #10400, 1000.000000000000000 ) ;
#88368 = SURFACE_STYLE_USAGE ( .BOTH. , #4393 ) ;
#88369 = CARTESIAN_POINT ( 'NONE',  ( -2.816281873526473856, 34.33196800326376064, 3.434112377981055619 ) ) ;
#88370 = CARTESIAN_POINT ( 'NONE',  ( 17.20831665107776587, 44.13393115100078745, -7.208316651077762316 ) ) ;
#88371 = CARTESIAN_POINT ( 'NONE',  ( 9.742785792574933268, 8.034700295649317425, -5.625000000000003553 ) ) ;
#88372 = CARTESIAN_POINT ( 'NONE',  ( -4.164238869374098151, 56.59541550158063927, -3.795296366450310543 ) ) ;
#88373 = CARTESIAN_POINT ( 'NONE',  ( 12.63842701281683922, 34.55059781766745886, -9.846743663894590881 ) ) ;
#88374 = B_SPLINE_CURVE_WITH_KNOTS ( 'NONE', 3,
 ( #77657, #70670, #48634, #94634, #18157, #63630 ),
 .UNSPECIFIED., .F., .F.,
 ( 4, 2, 4 ),
 ( 0.0002800518438628033847, 0.0006862575805706614372, 0.001092463317278519544 ),
 .UNSPECIFIED. ) ;
#88375 = DIRECTION ( 'NONE',  ( 0.6087614290087186575, 0.000000000000000000, 0.7933533402912366084 ) ) ;
#88376 = CARTESIAN_POINT ( 'NONE',  ( 10.00000000000000178, 58.05374883491397497, 14.16423886937410082 ) ) ;
#88377 = CARTESIAN_POINT ( 'NONE',  ( 12.79448242979007411, 14.76930270348881002, -7.716169648622100752 ) ) ;
#88378 = CARTESIAN_POINT ( 'NONE',  ( 2.035157376598824452, 18.68868534415484106, 7.964842623401179544 ) ) ;
#88379 = CARTESIAN_POINT ( 'NONE',  ( 20.36894250292379738, 29.92874883491396432, -10.36894250292379027 ) ) ;
#88381 = DIRECTION ( 'NONE',  ( -0.4924235601034587240, 0.000000000000000000, -0.8703556959399044723 ) ) ;
#88380 = CARTESIAN_POINT ( 'NONE',  ( -4.164238869374099039, 46.80374883491397497, 8.674139862899312516E-16 ) ) ;
#88382 = CARTESIAN_POINT ( 'NONE',  ( 2.791683348922240793, 16.63393115100078745, 7.208316651077764092 ) ) ;
#88384 = CARTESIAN_POINT ( 'NONE',  ( 19.84674366389459266, 63.30059781766745886, 2.638427012816836559 ) ) ;
#88383 = FACE_BOUND ( 'NONE', #80702, .T. ) ;
#88385 = ORIENTED_EDGE ( 'NONE', *, *, #19659, .T. ) ;
#88386 = CARTESIAN_POINT ( 'NONE',  ( 10.00000000000000178, 44.31368534415484106, 10.88017736071110342 ) ) ;
#88387 = CARTESIAN_POINT ( 'NONE',  ( 0.1955144967548739787, 64.32703681773342907, -6.500000000002695622 ) ) ;
#88388 = CARTESIAN_POINT ( 'NONE',  ( 17.20831665107776587, 54.13393115100079456, -7.208316651077762316 ) ) ;
#88389 = DIRECTION ( 'NONE',  ( 0.6093027842603860877, 0.6796026999251382206, -0.4085220769395505602 ) ) ;
#88390 = CARTESIAN_POINT ( 'NONE',  ( 10.00000000000000000, 54.75893115100078745, -9.846743663894594434 ) ) ;
#88391 = CARTESIAN_POINT ( 'NONE',  ( 10.00000000000000000, 0.5537488349139675359, -14.16423886937410082 ) ) ;
#88392 = AXIS2_PLACEMENT_3D ( 'NONE', #25465, #54451, #53969 ) ;
#88393 = CARTESIAN_POINT ( 'NONE',  ( 2.917880565312950480, 20.97041550158063217, -12.26659068614894821 ) ) ;
#88394 = EDGE_CURVE ( 'NONE', #48000, #56218, #33064, .T. ) ;
#88395 = EDGE_CURVE ( 'NONE', #30537, #55012, #85763, .T. ) ;
#88396 = FILL_AREA_STYLE_COLOUR ( '', #21529 ) ;
#88398 = CARTESIAN_POINT ( 'NONE',  ( -2.393480905992944496, 0.5000000000000004441, -14.80781041047754520 ) ) ;
#88397 = CARTESIAN_POINT ( 'NONE',  ( -3.377759596008065746, -3.629459927035739497, -2.500000000000000000 ) ) ;
#88399 = CARTESIAN_POINT ( 'NONE',  ( 4.559911319644449179, 18.89701867748817321, 9.422509992056141925 ) ) ;
#88400 = CARTESIAN_POINT ( 'NONE',  ( 22.81628187352647785, 41.41530133659708923, 3.434112377981063169 ) ) ;
#88401 = CARTESIAN_POINT ( 'NONE',  ( 21.92686044187656336, 61.97997603579418069, 3.195792623639536423 ) ) ;
#88402 = CARTESIAN_POINT ( 'NONE',  ( 14.92337183194729988, 14.34226448433411782, -8.527530157486177487 ) ) ;
#88403 = DIRECTION ( 'NONE',  ( 0.1132032137679171296, 0.000000000000000000, -0.9935718556765863463 ) ) ;
#88404 = ORIENTED_EDGE ( 'NONE', *, *, #38181, .F. ) ;
#88405 = VECTOR ( 'NONE', #90456, 1000.000000000000000 ) ;
#88406 = CARTESIAN_POINT ( 'NONE',  ( 5.680373670945877862, -28.65980262290164049, -3.999999999987121413 ) ) ;
#88407 = CARTESIAN_POINT ( 'NONE',  ( 17.08211943468705840, 30.13708216824730357, -12.26659068614894466 ) ) ;
#88408 = CARTESIAN_POINT ( 'NONE',  ( 2.035157376598822676, 7.438685344154837509, -7.964842623401177768 ) ) ;
#88409 = LINE ( 'NONE', #42422, #36682 ) ;
#88410 = DIRECTION ( 'NONE',  ( 0.000000000000000000, 0.000000000000000000, -1.000000000000000000 ) ) ;
#88411 = CARTESIAN_POINT ( 'NONE',  ( 4.559911319644449179, 37.23035201082150536, -9.422509992056141925 ) ) ;
#88412 = CARTESIAN_POINT ( 'NONE',  ( 0.5774900079438590739, 47.64701867748817676, -5.440088680355550821 ) ) ;
#88413 = CARTESIAN_POINT ( 'NONE',  ( -2.816281873526473856, 14.33196800326375531, 3.434112377981055619 ) ) ;
#88414 = CARTESIAN_POINT ( 'NONE',  ( 14.92337183194729633, 62.67559781766745886, 8.527530157486181039 ) ) ;
#88415 = CARTESIAN_POINT ( 'NONE',  ( -0.8801773607111009756, 3.063685344154838397, 1.068504757029289695E-15 ) ) ;
#88416 = CARTESIAN_POINT ( 'NONE',  ( 0.1532563361054100626, 5.800597817667452638, -2.638427012816831230 ) ) ;
#88417 = CARTESIAN_POINT ( 'NONE',  ( -3.750000000000000000, 10.25000000000000000, 2.750000000000000000 ) ) ;
#88418 = CARTESIAN_POINT ( 'NONE',  ( 19.42250999205614193, 50.14701867748817676, 5.440088680355555262 ) ) ;
#88420 = EDGE_CURVE ( 'NONE', #91650, #27523, #4256, .T. ) ;
#88419 = CARTESIAN_POINT ( 'NONE',  ( 3.591859063236763294, 8.290301336597087456, -11.09922568453595026 ) ) ;
#88421 = CARTESIAN_POINT ( 'NONE',  ( 7.084665262690076126, 64.10535201082150536, 10.88017736071109987 ) ) ;
#88422 = CARTESIAN_POINT ( 'NONE',  ( 5.076628168052704559, 25.17559781766745175, -8.527530157486179263 ) ) ;
#88423 = CARTESIAN_POINT ( 'NONE',  ( 13.43411237798106583, 47.66530133659709634, -12.81628187352647252 ) ) ;
#88424 = CARTESIAN_POINT ( 'NONE',  ( 19.84674366389459621, 3.508931151000785231, 7.409399052514197653E-17 ) ) ;
#88425 = VERTEX_POINT ( 'NONE', #21222 ) ;
#88426 = CARTESIAN_POINT ( 'NONE',  ( 13.21236992757673789, 15.00000000000000000, -5.338143956176714333 ) ) ;
#88427 = CARTESIAN_POINT ( 'NONE',  ( 0.9413316022086073431, 28.45508385108958649, 6.499999999999968914 ) ) ;
#88428 = CARTESIAN_POINT ( 'NONE',  ( 20.88017736071110164, 20.35535201082150891, 2.915334737309930979 ) ) ;
#88429 = CARTESIAN_POINT ( 'NONE',  ( -1.099225684535947600, 64.54030133659709634, 6.408140936763237150 ) ) ;
#88430 = EDGE_CURVE ( 'NONE', #20387, #88013, #15607, .T. ) ;
#88431 = CARTESIAN_POINT ( 'NONE',  ( 10.00000000000000000, 24.75893115100078745, -9.846743663894594434 ) ) ;
#88432 = CARTESIAN_POINT ( 'NONE',  ( 15.44008868035555260, 24.73035201082150891, 9.422509992056143702 ) ) ;
#88433 = CARTESIAN_POINT ( 'NONE',  ( 20.88017736071110519, 5.563685344154838397, 2.639326808657452039E-16 ) ) ;
#88434 = ORIENTED_EDGE ( 'NONE', *, *, #17779, .F. ) ;
#88435 = CARTESIAN_POINT ( 'NONE',  ( -0.8801773607111008646, 13.27201867748817143, 2.915334737309923430 ) ) ;
#88436 = CARTESIAN_POINT ( 'NONE',  ( 20.88017736071110519, 30.56368534415484106, 2.639326808657452039E-16 ) ) ;
#88438 = CARTESIAN_POINT ( 'NONE',  ( 10.00000000000000178, 39.31368534415484106, 10.88017736071110342 ) ) ;
#88437 = CARTESIAN_POINT ( 'NONE',  ( -12.07856007377833407, 15.00000000000000000, 8.022367888854752493 ) ) ;
#88439 = ORIENTED_EDGE ( 'NONE', *, *, #90792, .F. ) ;
#88440 = CARTESIAN_POINT ( 'NONE',  ( 5.076628168052704559, 65.17559781766745175, -8.527530157486179263 ) ) ;
#88441 = CARTESIAN_POINT ( 'NONE',  ( 12.91533473730992121, 29.52201867748817321, 10.88017736071110164 ) ) ;
#88442 = CARTESIAN_POINT ( 'NONE',  ( 4.573751236700658751, -6.413519960483383464, 3.750000000000000000 ) ) ;
#88443 = CARTESIAN_POINT ( 'NONE',  ( -8.549892366338930572, 14.76930270348881002, 12.25305656628349382 ) ) ;
#88444 = CARTESIAN_POINT ( 'NONE',  ( 13.99999999999999822, 10.49999999999999822, 6.500000000000000888 ) ) ;
#88445 = CARTESIAN_POINT ( 'NONE',  ( 22.26659068614894466, 33.88708216824730357, 7.082119434687054849 ) ) ;
#88446 = CARTESIAN_POINT ( 'NONE',  ( -0.8801773607111008646, 33.27201867748817676, 2.915334737309923430 ) ) ;
#88447 = CARTESIAN_POINT ( 'NONE',  ( 4.559911319644449179, 28.89701867748817321, 9.422509992056141925 ) ) ;
#88448 = CARTESIAN_POINT ( 'NONE',  ( 17.20831665107776587, 64.13393115100079456, -7.208316651077762316 ) ) ;
#88449 = CYLINDRICAL_SURFACE ( 'NONE', #47718, 0.4999999999999995559 ) ;
#88450 = CARTESIAN_POINT ( 'NONE',  ( 0.1532563361054083140, 51.00893115100078745, 1.131784320476157264E-15 ) ) ;
#88451 = CARTESIAN_POINT ( 'NONE',  ( 0.2751277870542913062, 29.36607318730131411, -6.499999999999992006 ) ) ;
#88452 = CARTESIAN_POINT ( 'NONE',  ( 17.20831665107776587, 17.88393115100078745, 7.208316651077764980 ) ) ;
#88453 = CARTESIAN_POINT ( 'NONE',  ( 9.382169495545415572, -27.75136533006957862, -9.382169495545422677 ) ) ;
#88454 = CARTESIAN_POINT ( 'NONE',  ( -0.8801773607111008646, 13.27201867748817143, 2.915334737309923430 ) ) ;
#88455 = CARTESIAN_POINT ( 'NONE',  ( 19.84674366389459266, 28.71726448433411960, -2.638427012816827677 ) ) ;
#88456 = CARTESIAN_POINT ( 'NONE',  ( 16.40814093676324603, 12.45696800326375353, -11.09922568453594671 ) ) ;
#88457 = CARTESIAN_POINT ( 'NONE',  ( 7.084665262690076126, 57.02201867748817676, -10.88017736071110164 ) ) ;
#88459 = CARTESIAN_POINT ( 'NONE',  ( 21.09922568453595559, 57.04030133659708923, -6.408140936763230044 ) ) ;
#88458 = CARTESIAN_POINT ( 'NONE',  ( -0.8801773607111009756, 13.06368534415483929, 1.068504757029289695E-15 ) ) ;
#88460 = CARTESIAN_POINT ( 'NONE',  ( 20.36894250292379738, 29.92874883491396432, -10.36894250292379027 ) ) ;
#88461 = COLOUR_RGB ( '', 0.66274510, 0.83137255, 0.94901961) ;
#88462 = ORIENTED_EDGE ( 'NONE', *, *, #52392, .F. ) ;
#88463 = CARTESIAN_POINT ( 'NONE',  ( 0.6178305044545818747, 8.498634669930421381, -9.382169495545419124 ) ) ;
#88464 = FILL_AREA_STYLE ('',( #72470 ) ) ;
#88465 = CARTESIAN_POINT ( 'NONE',  ( 2.035157376598822676, 27.43868534415483396, -7.964842623401177768 ) ) ;
#88466 = CARTESIAN_POINT ( 'NONE',  ( 7.361572987183170547, 62.05059781766745886, 9.846743663894590881 ) ) ;
#88467 = ORIENTED_EDGE ( 'NONE', *, *, #17682, .T. ) ;
#88468 = CARTESIAN_POINT ( 'NONE',  ( 17.20831665107776587, 12.88393115100078390, 7.208316651077764980 ) ) ;
#88469 = CARTESIAN_POINT ( 'NONE',  ( 7.361572987183169658, 14.96726448433411960, -9.846743663894592657 ) ) ;
#88470 = CARTESIAN_POINT ( 'NONE',  ( 19.84674366389459621, 18.50893115100078745, 7.409399052514197653E-17 ) ) ;
#88471 = CARTESIAN_POINT ( 'NONE',  ( 17.20831665107776587, 14.13393115100078568, -7.208316651077762316 ) ) ;
#88472 = B_SPLINE_CURVE_WITH_KNOTS ( 'NONE', 3,
 ( #7711, #92178, #37707, #8193, #29686, #23704 ),
 .UNSPECIFIED., .F., .F.,
 ( 4, 2, 4 ),
 ( 0.0002800011564896245269, 0.0006862063972211604468, 0.001092411637952696475 ),
 .UNSPECIFIED. ) ;
#88473 = FILL_AREA_STYLE ('',( #11988 ) ) ;
#88474 = EDGE_CURVE ( 'NONE', #51046, #59600, #2528, .T. ) ;
#88475 = CARTESIAN_POINT ( 'NONE',  ( -4.535014064373548592, -17.52590857053363393, 2.750000000000806466 ) ) ;
#88477 = DIRECTION ( 'NONE',  ( 1.000000000000000000, 0.000000000000000000, 0.000000000000000000 ) ) ;
#88476 = CARTESIAN_POINT ( 'NONE',  ( 0.5774900079438607392, 68.48035201082150536, 5.440088680355550821 ) ) ;
#88478 = CARTESIAN_POINT ( 'NONE',  ( 7.361572987183169658, 4.967264484334119601, -9.846743663894592657 ) ) ;
#88480 = VERTEX_POINT ( 'NONE', #13718 ) ;
#88479 = CARTESIAN_POINT ( 'NONE',  ( 5.076628168052703671, 16.84226448433411960, 8.527530157486179263 ) ) ;
#88481 = DIRECTION ( 'NONE',  ( 0.000000000000000000, 0.000000000000000000, -1.000000000000000000 ) ) ;
#88482 = CARTESIAN_POINT ( 'NONE',  ( 2.791683348922237240, 65.38393115100078035, -7.208316651077763204 ) ) ;
#88483 = ORIENTED_EDGE ( 'NONE', *, *, #9513, .F. ) ;
#88484 = ORIENTED_EDGE ( 'NONE', *, *, #92124, .T. ) ;
#88485 = CARTESIAN_POINT ( 'NONE',  ( 4.559911319644449179, 2.230352010821504471, -9.422509992056141925 ) ) ;
#88486 = CARTESIAN_POINT ( 'NONE',  ( 2.917880565312950480, 25.97041550158063572, -12.26659068614894821 ) ) ;
#88487 = PRODUCT_DEFINITION_CONTEXT ( 'detailed design', #83209, 'design' ) ;
#88488 = LINE ( 'NONE', #34488, #71123 ) ;
#88489 = CARTESIAN_POINT ( 'NONE',  ( -2.266590686148945544, 17.22041550158063572, 7.082119434687048631 ) ) ;
#88490 = CARTESIAN_POINT ( 'NONE',  ( 17.08211943468705130, 38.47041550158063217, 12.26659068614894998 ) ) ;
#88491 = CARTESIAN_POINT ( 'NONE',  ( -4.164238869374099039, 16.80374883491396787, 8.674139862899312516E-16 ) ) ;
#88492 = CARTESIAN_POINT ( 'NONE',  ( 10.00000000000000000, 36.81368534415484106, -10.88017736071110342 ) ) ;
#88493 = CARTESIAN_POINT ( 'NONE',  ( 6.878063601867475008, -66.29791949882819324, -3.750000000000000888 ) ) ;
#88494 = ORIENTED_EDGE ( 'NONE', *, *, #1082, .F. ) ;
#88495 = CARTESIAN_POINT ( 'NONE',  ( 2.791683348922237240, 20.38393115100078745, -7.208316651077763204 ) ) ;
#88496 = ADVANCED_FACE ( 'NONE', ( #27724 ), #65218, .F. ) ;
#88498 = CARTESIAN_POINT ( 'NONE',  ( 2.791683348922237240, 25.38393115100078390, -7.208316651077763204 ) ) ;
#88497 = CARTESIAN_POINT ( 'NONE',  ( 15.44008868035555793, 56.39701867748817676, -9.422509992056140149 ) ) ;
#88499 = ORIENTED_EDGE ( 'NONE', *, *, #93931, .F. ) ;
#88500 = CARTESIAN_POINT ( 'NONE',  ( 12.91533473730993009, 16.60535201082150891, -10.88017736071109987 ) ) ;
#88501 = CARTESIAN_POINT ( 'NONE',  ( -2.816281873526471635, 38.91530133659708213, -3.434112377981056508 ) ) ;
#88502 = CARTESIAN_POINT ( 'NONE',  ( 7.361572987183169658, 54.96726448433413026, -9.846743663894592657 ) ) ;
#88503 = CARTESIAN_POINT ( 'NONE',  ( -27.43587634952537968, 22.49999999999998934, -9.500000000000000000 ) ) ;
#88504 = CARTESIAN_POINT ( 'NONE',  ( 10.00000000000000000, 47.87363466993042493, -12.81628187352647608 ) ) ;
#88505 = CARTESIAN_POINT ( 'NONE',  ( -12.26659068614894110, -37.77958449841936783, 7.082119434687058401 ) ) ;
#88506 = CARTESIAN_POINT ( 'NONE',  ( 12.63842701281683922, 34.55059781766745886, -9.846743663894590881 ) ) ;
#88507 = EDGE_CURVE ( 'NONE', #85704, #81651, #47810, .T. ) ;
#88508 = CARTESIAN_POINT ( 'NONE',  ( 20.36894250292379382, 28.67874883491396787, 10.36894250292379205 ) ) ;
#88509 = ORIENTED_EDGE ( 'NONE', *, *, #49890, .F. ) ;
#88510 = SPHERICAL_SURFACE ( 'NONE', #55581, 0.2500000000000000000 ) ;
#88511 = EDGE_CURVE ( 'NONE', #1901, #32046, #59205, .T. ) ;
#88512 = CARTESIAN_POINT ( 'NONE',  ( 20.88017736071110164, 55.35535201082149825, 2.915334737309930979 ) ) ;
#88513 = CARTESIAN_POINT ( 'NONE',  ( 17.96484262340118221, 49.93868534415484106, 7.964842623401181321 ) ) ;
#88514 = CARTESIAN_POINT ( 'NONE',  ( 24.16423886937410614, 39.51208216824731068, -3.795296366450302550 ) ) ;
#88515 = CARTESIAN_POINT ( 'NONE',  ( 0.6178305044545838731, 4.748634669930420493, 9.382169495545420901 ) ) ;
#88516 = B_SPLINE_CURVE_WITH_KNOTS ( 'NONE', 3,
 ( #91102, #641, #7638, #98143, #75118, #45107 ),
 .UNSPECIFIED., .F., .F.,
 ( 4, 2, 4 ),
 ( 9.220181747203676555E-18, 0.0002605067024380944827, 0.0005210134048761797497 ),
 .UNSPECIFIED. ) ;
#88517 = CARTESIAN_POINT ( 'NONE',  ( 0.2751277870542868098, 57.28217586085237656, -6.499999999999985789 ) ) ;
#88518 = CARTESIAN_POINT ( 'NONE',  ( 0.5774900079438607392, 38.48035201082150536, 5.440088680355550821 ) ) ;
#88519 = CARTESIAN_POINT ( 'NONE',  ( -6.822555938877875370, -84.39442183841866552, -2.500000000000000000 ) ) ;
#88520 = CARTESIAN_POINT ( 'NONE',  ( 12.63842701281683922, 59.55059781766744464, -9.846743663894590881 ) ) ;
#88521 = CARTESIAN_POINT ( 'NONE',  ( 9.422509992056141925, 20.14701867748818032, 5.440088680355547268 ) ) ;
#88522 = DIRECTION ( 'NONE',  ( -0.000000000000000000, 0.000000000000000000, 1.000000000000000000 ) ) ;
#88523 = CARTESIAN_POINT ( 'NONE',  ( 20.88017736071110875, 65.77201867748817676, -2.915334737309920765 ) ) ;
#88524 = ORIENTED_EDGE ( 'NONE', *, *, #19770, .T. ) ;
#88525 = CARTESIAN_POINT ( 'NONE',  ( 19.42250999205614548, 5.980352010821504471, -5.440088680355545492 ) ) ;
#88526 = CARTESIAN_POINT ( 'NONE',  ( 19.80777595082616926, 65.68878173731739878, -6.499999999999942268 ) ) ;
#88527 = CARTESIAN_POINT ( 'NONE',  ( -0.8801773607111009756, 68.06368534415484817, 1.068504757029289695E-15 ) ) ;
#88528 = CARTESIAN_POINT ( 'NONE',  ( 17.20831665107776587, 2.883931151000785231, 7.208316651077764980 ) ) ;
#88529 = CARTESIAN_POINT ( 'NONE',  ( 20.15039907845753575, 36.74884699246889141, 6.262539305110075283 ) ) ;
#88530 = VECTOR ( 'NONE', #66969, 1000.000000000000000 ) ;
#88531 = CARTESIAN_POINT ( 'NONE',  ( 12.63842701281683922, 34.55059781766745886, -9.846743663894590881 ) ) ;
#88532 = CARTESIAN_POINT ( 'NONE',  ( 2.035157376598824452, 28.68868534415484106, 7.964842623401179544 ) ) ;
#88533 = VECTOR ( 'NONE', #55224, 1000.000000000000000 ) ;
#88534 = CARTESIAN_POINT ( 'NONE',  ( 0.6178305044545838731, 4.748634669930420493, 9.382169495545420901 ) ) ;
#88535 = CARTESIAN_POINT ( 'NONE',  ( 4.559911319644449179, 32.23035201082150536, -9.422509992056141925 ) ) ;
#88536 = DIRECTION ( 'NONE',  ( 0.000000000000000000, 0.000000000000000000, 1.000000000000000000 ) ) ;
#88537 = CARTESIAN_POINT ( 'NONE',  ( 6.565887622018943937, 33.08196800326374643, -12.81628187352647608 ) ) ;
#88538 = ORIENTED_EDGE ( 'NONE', *, *, #48083, .F. ) ;
#88539 = CARTESIAN_POINT ( 'NONE',  ( -0.8801773607111008646, 58.27201867748816966, 2.915334737309923430 ) ) ;
#88541 = DIRECTION ( 'NONE',  ( -0.9170600743851266001, 0.000000000000000000, 0.3987490689252404241 ) ) ;
#88540 = CARTESIAN_POINT ( 'NONE',  ( 0.6178305044545838731, 19.74863466993042138, 9.382169495545420901 ) ) ;
#88542 = EDGE_CURVE ( 'NONE', #84080, #95213, #71736, .T. ) ;
#88543 = SURFACE_STYLE_FILL_AREA ( #5055 ) ;
#88544 = CARTESIAN_POINT ( 'NONE',  ( 12.91533473730993009, 26.60535201082150536, -10.88017736071109987 ) ) ;
#88545 = CARTESIAN_POINT ( 'NONE',  ( 2.917880565312948704, 62.63708216824730357, 12.26659068614894643 ) ) ;
#88546 = CARTESIAN_POINT ( 'NONE',  ( 1.472469842513823179, 56.42559781766745886, 4.923371831947296329 ) ) ;
#88547 = CARTESIAN_POINT ( 'NONE',  ( 5.076628168052704559, 10.17559781766745175, -8.527530157486179263 ) ) ;
#88548 = CARTESIAN_POINT ( 'NONE',  ( 12.91533473730993009, 66.60535201082150536, -10.88017736071109987 ) ) ;
#88549 = CARTESIAN_POINT ( 'NONE',  ( 13.55157833323634797, 0.2306972965111905305, -6.292279346205384094 ) ) ;
#88550 = CARTESIAN_POINT ( 'NONE',  ( 24.16423886937410614, 34.30374883491396787, 8.672049930838204340E-16 ) ) ;
#88551 =( LENGTH_UNIT ( ) NAMED_UNIT ( * ) SI_UNIT ( .MILLI., .METRE. ) );
#88552 = ORIENTED_EDGE ( 'NONE', *, *, #20098, .T. ) ;
#88553 = ORIENTED_EDGE ( 'NONE', *, *, #88511, .F. ) ;
#88554 = CARTESIAN_POINT ( 'NONE',  ( 17.08211943468705130, 58.47041550158063927, 12.26659068614894998 ) ) ;
#88555 = CARTESIAN_POINT ( 'NONE',  ( -2.266590686148945544, 47.22041550158063927, 7.082119434687048631 ) ) ;
#88556 = CARTESIAN_POINT ( 'NONE',  ( 12.63842701281683922, 24.55059781766745175, -9.846743663894590881 ) ) ;
#88557 = CIRCLE ( 'NONE', #7200, 1.249999999999987121 ) ;
#88558 = CARTESIAN_POINT ( 'NONE',  ( 13.43411237798106583, 22.66530133659708923, -12.81628187352647252 ) ) ;
#88559 = FACE_OUTER_BOUND ( 'NONE', #56240, .T. ) ;
#88560 = DIRECTION ( 'NONE',  ( 0.000000000000000000, 1.000000000000000000, -0.000000000000000000 ) ) ;
#88561 = CARTESIAN_POINT ( 'NONE',  ( -2.266590686148945544, 46.38708216824730357, -7.082119434687050408 ) ) ;
#88562 = CARTESIAN_POINT ( 'NONE',  ( -8.099999999999999645, 75.73428692542562146, 2.900000000000000355 ) ) ;
#88563 = CARTESIAN_POINT ( 'NONE',  ( 0.1532563361054082862, 6.217264484334118713, 2.638427012816831674 ) ) ;
#88564 = DIRECTION ( 'NONE',  ( 0.9762960071199360268, 0.000000000000000000, -0.2164396139380906636 ) ) ;
#88565 = CARTESIAN_POINT ( 'NONE',  ( -2.638427012816824124, 7.050597817667457079, 9.846743663894596210 ) ) ;
#88566 = EDGE_LOOP ( 'NONE', ( #58797, #11875, #88961, #84192 ) ) ;
#88567 = ORIENTED_EDGE ( 'NONE', *, *, #65569, .T. ) ;
#88568 = FILL_AREA_STYLE_COLOUR ( '', #70149 ) ;
#88569 = ORIENTED_EDGE ( 'NONE', *, *, #98157, .T. ) ;
#88571 = CARTESIAN_POINT ( 'NONE',  ( 15.44008868035555260, 24.73035201082150891, 9.422509992056143702 ) ) ;
#88570 = CARTESIAN_POINT ( 'NONE',  ( 19.42250999205614193, 15.14701867748817143, 5.440088680355555262 ) ) ;
#88573 = CARTESIAN_POINT ( 'NONE',  ( 3.591859063236761518, 19.95696800326375353, 11.09922568453594849 ) ) ;
#88572 = CARTESIAN_POINT ( 'NONE',  ( 2.791683348922237240, 50.38393115100078035, -7.208316651077763204 ) ) ;
#88574 = CARTESIAN_POINT ( 'NONE',  ( 15.00000000000000000, 11.50000000000000000, 6.000000000000000000 ) ) ;
#88575 = COLOUR_RGB ( '', 0.66274510, 0.83137255, 0.94901961) ;
#88576 = CARTESIAN_POINT ( 'NONE',  ( 3.591859063236763294, 13.29030133659708746, -11.09922568453595026 ) ) ;
#88577 = ORIENTED_EDGE ( 'NONE', *, *, #13361, .F. ) ;
#88578 = CARTESIAN_POINT ( 'NONE',  ( 7.361572987183169658, 29.96726448433411960, -9.846743663894592657 ) ) ;
#88579 = CARTESIAN_POINT ( 'NONE',  ( 13.79529636645031943, 55.34541550158062506, -14.16423886937409904 ) ) ;
#88580 = ORIENTED_EDGE ( 'NONE', *, *, #76164, .T. ) ;
#88581 = CARTESIAN_POINT ( 'NONE',  ( 10.00000000000000178, 4.313685344154837509, 10.88017736071110342 ) ) ;
#88582 = EDGE_LOOP ( 'NONE', ( #24898, #33870, #24885 ) ) ;
#88583 = CARTESIAN_POINT ( 'NONE',  ( 12.91533473730993009, 41.60535201082149825, -10.88017736071109987 ) ) ;
#88584 = CARTESIAN_POINT ( 'NONE',  ( 2.035157376598824452, 38.68868534415483396, 7.964842623401179544 ) ) ;
#88585 = CARTESIAN_POINT ( 'NONE',  ( 17.96484262340118221, 44.93868534415483396, 7.964842623401181321 ) ) ;
#88586 = CARTESIAN_POINT ( 'NONE',  ( 19.80777595082615861, 5.688781737317405884, -6.500000000000003553 ) ) ;
#88587 = CARTESIAN_POINT ( 'NONE',  ( 0.5774900079438607392, 38.48035201082150536, 5.440088680355550821 ) ) ;
#88588 = CARTESIAN_POINT ( 'NONE',  ( -4.250000000000000000, 78.07179676972445748, 6.500000000000000888 ) ) ;
#88589 = EDGE_CURVE ( 'NONE', #32382, #92377, #13882, .T. ) ;
#88590 = DIRECTION ( 'NONE',  ( 1.927470528863119542E-16, -1.000000000000000000, -0.000000000000000000 ) ) ;
#88591 = CARTESIAN_POINT ( 'NONE',  ( 17.20831665107776587, 24.13393115100078035, -7.208316651077762316 ) ) ;
#88592 = ORIENTED_EDGE ( 'NONE', *, *, #11238, .F. ) ;
#88593 = CARTESIAN_POINT ( 'NONE',  ( 19.84674366389459266, 63.71726448433412315, -2.638427012816827677 ) ) ;
#88594 = DIRECTION ( 'NONE',  ( 0.000000000000000000, 0.000000000000000000, -1.000000000000000000 ) ) ;
#88595 = CARTESIAN_POINT ( 'NONE',  ( 0.000000000000000000, 0.5000000000000004441, 0.000000000000000000 ) ) ;
#88596 = DIRECTION ( 'NONE',  ( -0.000000000000000000, -1.000000000000000000, -0.000000000000000000 ) ) ;
#88597 = DIRECTION ( 'NONE',  ( 6.938893903907221278E-15, -1.000000000000000000, 0.000000000000000000 ) ) ;
#88599 = CARTESIAN_POINT ( 'NONE',  ( 1.472469842513823179, 35.59226448433412315, -4.923371831947296329 ) ) ;
#88598 = CARTESIAN_POINT ( 'NONE',  ( -3.115783986955370732, 3.816680036666981737E-16, -14.16128137375401685 ) ) ;
#88600 = CARTESIAN_POINT ( 'NONE',  ( 6.204703633549690345, 60.76208216824730357, -14.16423886937410259 ) ) ;
#88601 = DIRECTION ( 'NONE',  ( 0.02617694830786938473, 0.000000000000000000, 0.9996573249755574819 ) ) ;
#88602 = ORIENTED_EDGE ( 'NONE', *, *, #56558, .F. ) ;
#88603 = CARTESIAN_POINT ( 'NONE',  ( 5.129999999999995453, 43.00000000000000000, 6.250000000000000000 ) ) ;
#88604 = CARTESIAN_POINT ( 'NONE',  ( 2.791683348922240793, 26.63393115100078745, 7.208316651077764092 ) ) ;
#88605 = CARTESIAN_POINT ( 'NONE',  ( 6.728956594450806072, 15.00000000000000888, -12.98689685418140627 ) ) ;
#88606 = VERTEX_POINT ( 'NONE', #7716 ) ;
#88607 = CARTESIAN_POINT ( 'NONE',  ( 22.81628187352648496, 6.831968003263753531, -3.434112377981050290 ) ) ;
#88608 = CARTESIAN_POINT ( 'NONE',  ( 2.791683348922240793, 11.63393115100078568, 7.208316651077764092 ) ) ;
#88609 = DIRECTION ( 'NONE',  ( -0.9799247046208282574, 0.000000000000000000, -0.1993679344172039347 ) ) ;
#88610 = CARTESIAN_POINT ( 'NONE',  ( 1.472469842513823179, 6.425597817667451750, 4.923371831947296329 ) ) ;
#88611 = CARTESIAN_POINT ( 'NONE',  ( 17.20831665107776587, 52.88393115100078035, 7.208316651077764980 ) ) ;
#88612 = CARTESIAN_POINT ( 'NONE',  ( 20.88017736071110164, 20.35535201082150536, 2.915334737309930979 ) ) ;
#88613 = EDGE_CURVE ( 'NONE', #28657, #6038, #39441, .T. ) ;
#88614 = AXIS2_PLACEMENT_3D ( 'NONE', #60242, #8718, #44742 ) ;
#88615 = ORIENTED_EDGE ( 'NONE', *, *, #58593, .F. ) ;
#88616 = ADVANCED_FACE ( 'NONE', ( #23211 ), #37875, .T. ) ;
#88617 = CARTESIAN_POINT ( 'NONE',  ( -0.8801773607111008646, 13.27201867748817321, 2.915334737309923430 ) ) ;
#88618 = CARTESIAN_POINT ( 'NONE',  ( 10.00000000000000000, 5.553748834913967869, -14.16423886937410082 ) ) ;
#88619 = CARTESIAN_POINT ( 'NONE',  ( 18.52753015748617571, 18.09226448433411960, 4.923371831947298993 ) ) ;
#88620 = CARTESIAN_POINT ( 'NONE',  ( 15.44008868035555260, 54.73035201082150536, 9.422509992056143702 ) ) ;
#88622 = DIRECTION ( 'NONE',  ( 0.000000000000000000, 0.000000000000000000, 1.000000000000000000 ) ) ;
#88621 = CARTESIAN_POINT ( 'NONE',  ( 22.81628187352648496, 26.83196800326374998, -3.434112377981050290 ) ) ;
#88623 = CARTESIAN_POINT ( 'NONE',  ( 12.91533473730992121, 4.522018677488169658, 10.88017736071110164 ) ) ;
#88624 = CARTESIAN_POINT ( 'NONE',  ( 20.03447792253738768, 17.65514106990690379, -6.401564815979731371 ) ) ;
#88625 = CARTESIAN_POINT ( 'NONE',  ( 19.72487221294570858, 0.5000000000000000000, -6.500000000000000888 ) ) ;
#88626 = CARTESIAN_POINT ( 'NONE',  ( 7.361572987183169658, 59.96726448433410894, -9.846743663894592657 ) ) ;
#88627 = CARTESIAN_POINT ( 'NONE',  ( 17.20831665107776587, 7.883931151000784787, 7.208316651077764980 ) ) ;
#88628 = CARTESIAN_POINT ( 'NONE',  ( 2.915334737309921209, -28.39464798917849819, -10.88017736071110164 ) ) ;
#88629 = CARTESIAN_POINT ( 'NONE',  ( -2.816281873526471635, 18.91530133659708213, -3.434112377981056508 ) ) ;
#88630 = CARTESIAN_POINT ( 'NONE',  ( -10.60841303226387033, -98.07605699796263821, -3.999999999999994671 ) ) ;
#88632 = DIRECTION ( 'NONE',  ( 0.000000000000000000, 1.000000000000000000, 0.000000000000000000 ) ) ;
#88631 = CARTESIAN_POINT ( 'NONE',  ( 15.44008868035555793, 26.39701867748817321, -9.422509992056140149 ) ) ;
#88633 = DIRECTION ( 'NONE',  ( -1.000000000000000000, 0.000000000000000000, 0.000000000000000000 ) ) ;
#88634 = AXIS2_PLACEMENT_3D ( 'NONE', #35862, #66855, #66350 ) ;
#88635 = CARTESIAN_POINT ( 'NONE',  ( -2.266590686148945544, 52.22041550158064638, 7.082119434687048631 ) ) ;
#88636 = SURFACE_STYLE_USAGE ( .BOTH. , #27642 ) ;
#88637 = B_SPLINE_CURVE_WITH_KNOTS ( 'NONE', 3,
 ( #67622, #83105, #98640, #60093, #8104, #632 ),
 .UNSPECIFIED., .F., .F.,
 ( 4, 2, 4 ),
 ( 0.0002800671705680388059, 0.0006862730573397204763, 0.001092478944111402147 ),
 .UNSPECIFIED. ) ;
#88638 = CARTESIAN_POINT ( 'NONE',  ( 4.559911319644449179, 27.23035201082150536, -9.422509992056141925 ) ) ;
#88639 = CARTESIAN_POINT ( 'NONE',  ( 0.1532563361054100626, 55.80059781766745175, -2.638427012816831230 ) ) ;
#88640 = CARTESIAN_POINT ( 'NONE',  ( 15.44008868035555260, 54.73035201082150536, 9.422509992056143702 ) ) ;
#88641 = VECTOR ( 'NONE', #40208, 1000.000000000000000 ) ;
#88643 = EDGE_CURVE ( 'NONE', #62748, #98433, #96718, .T. ) ;
#88642 = CARTESIAN_POINT ( 'NONE',  ( 6.204703633549690345, 32.84541550158063927, 14.16423886937410082 ) ) ;
#88644 = CARTESIAN_POINT ( 'NONE',  ( 17.35999999999999943, 37.99999999999997868, 7.000000000000000000 ) ) ;
#88645 = CARTESIAN_POINT ( 'NONE',  ( 0.1532563361054082862, 36.21726448433410894, 2.638427012816831674 ) ) ;
#88646 = CARTESIAN_POINT ( 'NONE',  ( -1.099225684535947600, 63.70696800326376774, -6.408140936763238038 ) ) ;
#88647 = CARTESIAN_POINT ( 'NONE',  ( -1.099225684535947600, 4.540301336597087456, 6.408140936763237150 ) ) ;
#88648 = ORIENTED_EDGE ( 'NONE', *, *, #31026, .F. ) ;
#88649 = CARTESIAN_POINT ( 'NONE',  ( 12.91533473730993009, 26.60535201082150536, -10.88017736071109987 ) ) ;
#88650 = CARTESIAN_POINT ( 'NONE',  ( 20.32896413005680714, 7.604976035794174472, -5.963430220938276349 ) ) ;
#88651 = CARTESIAN_POINT ( 'NONE',  ( 4.903136312256997087, -13.39483660680936339, 2.750000000000000000 ) ) ;
#88652 = CARTESIAN_POINT ( 'NONE',  ( 4.559911319644449179, 8.897018677488173211, 9.422509992056141925 ) ) ;
#88653 = CARTESIAN_POINT ( 'NONE',  ( 4.559911319644449179, 68.89701867748817676, 9.422509992056141925 ) ) ;
#88654 = CARTESIAN_POINT ( 'NONE',  ( 24.16423886937410614, 24.30374883491396787, 8.672049930838204340E-16 ) ) ;
#88655 = CARTESIAN_POINT ( 'NONE',  ( 10.00000000000000000, 14.75893115100078568, -9.846743663894594434 ) ) ;
#88656 = CARTESIAN_POINT ( 'NONE',  ( 19.84674366389459621, 63.50893115100078745, 7.409399052514197653E-17 ) ) ;
#88657 = CARTESIAN_POINT ( 'NONE',  ( 4.559911319644449179, 27.23035201082150536, -9.422509992056141925 ) ) ;
#88658 = VECTOR ( 'NONE', #96005, 1000.000000000000000 ) ;
#88659 = DIRECTION ( 'NONE',  ( -0.000000000000000000, -1.000000000000000000, -0.000000000000000000 ) ) ;
#88660 = CARTESIAN_POINT ( 'NONE',  ( 7.771322705631503069, 4.156677014937179135E-16, -12.24159072199917375 ) ) ;
#88661 = ORIENTED_EDGE ( 'NONE', *, *, #39854, .F. ) ;
#88662 = LINE ( 'NONE', #33680, #53084 ) ;
#88663 = CARTESIAN_POINT ( 'NONE',  ( 7.361572987183170547, 42.05059781766745886, 9.846743663894590881 ) ) ;
#88664 = ORIENTED_EDGE ( 'NONE', *, *, #64320, .F. ) ;
#88665 = ORIENTED_EDGE ( 'NONE', *, *, #71910, .F. ) ;
#88666 = CARTESIAN_POINT ( 'NONE',  ( 0.000000000000000000, 0.5000000000000004441, 0.000000000000000000 ) ) ;
#88667 = CARTESIAN_POINT ( 'NONE',  ( 24.16423886937410614, 4.512082168247300906, -3.795296366450302550 ) ) ;
#88668 = CARTESIAN_POINT ( 'NONE',  ( -4.164238869374099927, 12.01208216824730357, 3.795296366450308767 ) ) ;
#88669 = CARTESIAN_POINT ( 'NONE',  ( 19.42250999205614548, 45.98035201082150536, -5.440088680355545492 ) ) ;
#88670 = PRODUCT_DEFINITION_FORMATION_WITH_SPECIFIED_SOURCE ( 'ANY', '', #36462, .NOT_KNOWN. ) ;
#88671 = CARTESIAN_POINT ( 'NONE',  ( -2.266590686148945544, 52.22041550158064638, 7.082119434687048631 ) ) ;
#88672 = CARTESIAN_POINT ( 'NONE',  ( 22.81628187352647785, 6.415301336597088344, 3.434112377981063169 ) ) ;
#88673 = CARTESIAN_POINT ( 'NONE',  ( 14.92337183194729633, 37.67559781766745175, 8.527530157486181039 ) ) ;
#88674 = SURFACE_SIDE_STYLE ('',( #27678 ) ) ;
#88676 = CARTESIAN_POINT ( 'NONE',  ( 19.38216949554541557, 2.248634669930420049, -9.382169495545420901 ) ) ;
#88675 = CARTESIAN_POINT ( 'NONE',  ( 10.00000000000000000, 36.81368534415484106, -10.88017736071110342 ) ) ;
#88677 = CARTESIAN_POINT ( 'NONE',  ( 2.917880565312948704, 7.637082168247301794, 12.26659068614894643 ) ) ;
#88678 = CARTESIAN_POINT ( 'NONE',  ( -2.266590686148945544, 56.38708216824731068, -7.082119434687050408 ) ) ;
#88679 = VECTOR ( 'NONE', #30974, 1000.000000000000000 ) ;
#88680 = CARTESIAN_POINT ( 'NONE',  ( 7.084665262690076126, 22.02201867748817321, -10.88017736071110164 ) ) ;
#88681 = CARTESIAN_POINT ( 'NONE',  ( -2.815433093576927170, 0.5000000000000004441, -14.73340885523753663 ) ) ;
#88682 = CARTESIAN_POINT ( 'NONE',  ( 0.7575892234031803563, 14.76930270348881535, -14.92193396517713566 ) ) ;
#88683 = CARTESIAN_POINT ( 'NONE',  ( 8.776446609406717059, 70.10355339059326241, -6.500000000000001776 ) ) ;
#88684 = ORIENTED_EDGE ( 'NONE', *, *, #5334, .F. ) ;
#88685 = SURFACE_STYLE_USAGE ( .BOTH. , #11216 ) ;
#88686 = VERTEX_POINT ( 'NONE', #15710 ) ;
#88687 = VERTEX_POINT ( 'NONE', #37713 ) ;
#88688 = CARTESIAN_POINT ( 'NONE',  ( 24.16423886937410614, 44.51208216824730357, -3.795296366450302550 ) ) ;
#88689 = CARTESIAN_POINT ( 'NONE',  ( 10.00000000000000178, 52.25893115100078745, 9.846743663894594434 ) ) ;
#88690 = CARTESIAN_POINT ( 'NONE',  ( 20.88017736071110519, 50.56368534415484106, 2.639326808657452039E-16 ) ) ;
#88691 = CARTESIAN_POINT ( 'NONE',  ( -41.94000000000001194, 93.50000000000000000, -10.09898361729590199 ) ) ;
#88692 = CARTESIAN_POINT ( 'NONE',  ( 4.559911319644449179, 57.23035201082150536, -9.422509992056141925 ) ) ;
#88693 = AXIS2_PLACEMENT_3D ( 'NONE', #59609, #76956, #69465 ) ;
#88694 = CARTESIAN_POINT ( 'NONE',  ( 19.38216949554541557, 57.24863466993042493, -9.382169495545420901 ) ) ;
#88695 = CARTESIAN_POINT ( 'NONE',  ( -9.382169495545413795, 4.748634669930419605, 9.382169495545428006 ) ) ;
#88696 = VERTEX_POINT ( 'NONE', #61664 ) ;
#88697 = CARTESIAN_POINT ( 'NONE',  ( 24.16423886937410614, 24.51208216824730002, -3.795296366450302550 ) ) ;
#88698 = ORIENTED_EDGE ( 'NONE', *, *, #48034, .F. ) ;
#88699 = CARTESIAN_POINT ( 'NONE',  ( 16.40814093676323893, 30.79030133659708923, 11.09922568453595026 ) ) ;
#88700 = EDGE_LOOP ( 'NONE', ( #64351, #77002, #96467, #70543 ) ) ;
#88701 = CARTESIAN_POINT ( 'NONE',  ( 13.43411237798105340, 40.58196800326375353, 12.81628187352647963 ) ) ;
#88702 = CARTESIAN_POINT ( 'NONE',  ( 17.20831665107776587, 42.88393115100077324, 7.208316651077764980 ) ) ;
#88703 = CARTESIAN_POINT ( 'NONE',  ( 12.91533473730993009, 11.60535201082150536, -10.88017736071109987 ) ) ;
#88704 = CARTESIAN_POINT ( 'NONE',  ( 16.40814093676324603, 52.45696800326375353, -11.09922568453594671 ) ) ;
#88705 = DIRECTION ( 'NONE',  ( -0.4924235601034586685, 0.000000000000000000, -0.8703556959399044723 ) ) ;
#88706 = CARTESIAN_POINT ( 'NONE',  ( 5.076628168052704559, 45.17559781766745175, -8.527530157486179263 ) ) ;
#88707 = CIRCLE ( 'NONE', #946, 0.2500000000000002220 ) ;
#88708 = EDGE_CURVE ( 'NONE', #65339, #61713, #60688, .T. ) ;
#88710 = ORIENTED_EDGE ( 'NONE', *, *, #34885, .F. ) ;
#88709 = LINE ( 'NONE', #89207, #26504 ) ;
#88711 = AXIS2_PLACEMENT_3D ( 'NONE', #24722, #18199, #25709 ) ;
#88712 = FILL_AREA_STYLE_COLOUR ( '', #67084 ) ;
#88713 = DIRECTION ( 'NONE',  ( 0.000000000000000000, 0.000000000000000000, -1.000000000000000000 ) ) ;
#88714 = FACE_OUTER_BOUND ( 'NONE', #35091, .T. ) ;
#88715 = CARTESIAN_POINT ( 'NONE',  ( 1.881370533971287617, 15.00000000000000888, -14.50512983964826574 ) ) ;
#88716 = CARTESIAN_POINT ( 'NONE',  ( 12.63842701281683034, 22.46726448433411605, 9.846743663894596210 ) ) ;
#88717 = CARTESIAN_POINT ( 'NONE',  ( 22.81628187352648496, 21.83196800326374643, -3.434112377981050290 ) ) ;
#88718 = CARTESIAN_POINT ( 'NONE',  ( 24.35999999999999233, 44.99999999999999289, -7.000000000000000000 ) ) ;
#88719 = ORIENTED_EDGE ( 'NONE', *, *, #27686, .F. ) ;
#88720 = CARTESIAN_POINT ( 'NONE',  ( 7.361572987183170547, 62.05059781766745886, 9.846743663894590881 ) ) ;
#88721 = CARTESIAN_POINT ( 'NONE',  ( 18.95386800105009328, 28.23810908735718783, -6.499999999999990230 ) ) ;
#88722 = CARTESIAN_POINT ( 'NONE',  ( 6.204703633549690345, 17.84541550158063217, 14.16423886937410082 ) ) ;
#88723 = CARTESIAN_POINT ( 'NONE',  ( 17.20831665107776587, 29.13393115100078390, -7.208316651077762316 ) ) ;
#88724 = CARTESIAN_POINT ( 'NONE',  ( 13.43411237798105340, 45.58196800326374643, 12.81628187352647963 ) ) ;
#88726 = DIRECTION ( 'NONE',  ( 1.000000000000000000, 0.000000000000000000, 0.000000000000000000 ) ) ;
#88725 = DIRECTION ( 'NONE',  ( -0.000000000000000000, -0.000000000000000000, -1.000000000000000000 ) ) ;
#88727 = CARTESIAN_POINT ( 'NONE',  ( 0.5774900079438607392, 58.48035201082151247, 5.440088680355550821 ) ) ;
#88728 = CARTESIAN_POINT ( 'NONE',  ( 0.6178305044545818747, 13.49863466993041783, -9.382169495545419124 ) ) ;
#88729 = CARTESIAN_POINT ( 'NONE',  ( 13.48255862861923937, 4.031870098369226268E-16, 5.335786055104250636 ) ) ;
#88730 = CARTESIAN_POINT ( 'NONE',  ( 17.20831665107776587, 32.88393115100078745, 7.208316651077764980 ) ) ;
#88731 = CARTESIAN_POINT ( 'NONE',  ( 15.44008868035555260, 44.73035201082151247, 9.422509992056143702 ) ) ;
#88732 = CARTESIAN_POINT ( 'NONE',  ( 22.81628187352648496, 41.83196800326375353, -3.434112377981050290 ) ) ;
#88733 = CIRCLE ( 'NONE', #12088, 0.5000000000000000000 ) ;
#88734 = CARTESIAN_POINT ( 'NONE',  ( 0.1532563361054083140, 36.00893115100078745, 1.131784320476157264E-15 ) ) ;
#88735 = CARTESIAN_POINT ( 'NONE',  ( -9.000000000000001776, 80.99999999999994316, 0.000000000000000000 ) ) ;
#88736 = VECTOR ( 'NONE', #12321, 1000.000000000000000 ) ;
#88737 = CIRCLE ( 'NONE', #55188, 14.49999999999999822 ) ;
#88738 = ADVANCED_FACE ( 'NONE', ( #29690 ), #52210, .T. ) ;
#88739 = CARTESIAN_POINT ( 'NONE',  ( -0.8801773607111008646, 28.27201867748817321, 2.915334737309923430 ) ) ;
#88740 = AXIS2_PLACEMENT_3D ( 'NONE', #44190, #43702, #35711 ) ;
#88741 = ORIENTED_EDGE ( 'NONE', *, *, #21596, .F. ) ;
#88742 = CARTESIAN_POINT ( 'NONE',  ( -8.235571585149862983, 5.743033628982648686, 8.235571585149875418 ) ) ;
#88743 = CARTESIAN_POINT ( 'NONE',  ( 19.42250999205614193, 15.14701867748817143, 5.440088680355555262 ) ) ;
#88745 = CARTESIAN_POINT ( 'NONE',  ( 7.084665262690076126, 32.02201867748816966, -10.88017736071110164 ) ) ;
#88744 = CARTESIAN_POINT ( 'NONE',  ( 10.00000000000000000, 54.75893115100078745, -9.846743663894594434 ) ) ;
#88746 = DIRECTION ( 'NONE',  ( 0.000000000000000000, -0.000000000000000000, 1.000000000000000000 ) ) ;
#88747 = CARTESIAN_POINT ( 'NONE',  ( 12.91533473730992121, 54.52201867748816255, 10.88017736071110164 ) ) ;
#88749 = CARTESIAN_POINT ( 'NONE',  ( -0.000000000000000000, 77.78215977002660964, -8.385699614948331160 ) ) ;
#88748 = CARTESIAN_POINT ( 'NONE',  ( 4.559911319644449179, 27.23035201082150536, -9.422509992056141925 ) ) ;
#88750 = SURFACE_STYLE_USAGE ( .BOTH. , #35748 ) ;
#88751 = CARTESIAN_POINT ( 'NONE',  ( 12.63842701281683922, 19.55059781766745175, -9.846743663894590881 ) ) ;
#88752 =( NAMED_UNIT ( * ) PLANE_ANGLE_UNIT ( ) SI_UNIT ( $, .RADIAN. ) );
#88753 = CARTESIAN_POINT ( 'NONE',  ( 7.082119434687047743, 0.1370821682473086223, -12.26659068614894821 ) ) ;
#88754 = CARTESIAN_POINT ( 'NONE',  ( 5.076628168052703671, 51.84226448433412315, 8.527530157486179263 ) ) ;
#88756 = CARTESIAN_POINT ( 'NONE',  ( 20.24186590665278018, 20.59014588040357197, -6.114288769123027656 ) ) ;
#88755 = CARTESIAN_POINT ( 'NONE',  ( -4.164238869374098151, 51.59541550158063217, -3.795296366450310543 ) ) ;
#88757 = CARTESIAN_POINT ( 'NONE',  ( -2.266590686148945544, 7.220415501580634832, 7.082119434687048631 ) ) ;
#88758 = CARTESIAN_POINT ( 'NONE',  ( 17.08211943468705130, 33.47041550158063927, 12.26659068614894998 ) ) ;
#88759 = CARTESIAN_POINT ( 'NONE',  ( -1.099225684535947600, -0.4596986634029132657, 6.408140936763237150 ) ) ;
#88760 = CARTESIAN_POINT ( 'NONE',  ( -7.116235074765046242, -80.68325706346374204, 2.750000000000000888 ) ) ;
#88761 = ORIENTED_EDGE ( 'NONE', *, *, #76553, .F. ) ;
#88762 = CIRCLE ( 'NONE', #55217, 14.49999999999999822 ) ;
#88763 = CARTESIAN_POINT ( 'NONE',  ( 19.42250999205614193, 15.14701867748817143, 5.440088680355555262 ) ) ;
#88764 = CARTESIAN_POINT ( 'NONE',  ( 19.84674366389459621, 33.50893115100078745, 7.409399052514197653E-17 ) ) ;
#88766 = CARTESIAN_POINT ( 'NONE',  ( -13.39911793698190223, 90.87255582226813999, -7.784798940734470207 ) ) ;
#88765 =( LENGTH_UNIT ( ) NAMED_UNIT ( * ) SI_UNIT ( .MILLI., .METRE. ) );
#88767 = CARTESIAN_POINT ( 'NONE',  ( 5.076628168052703671, 1.842264484334118047, 8.527530157486179263 ) ) ;
#88768 = CARTESIAN_POINT ( 'NONE',  ( 16.40814093676323893, 20.79030133659708923, 11.09922568453595026 ) ) ;
#88769 = CARTESIAN_POINT ( 'NONE',  ( 1.472469842513823179, 26.42559781766745175, 4.923371831947296329 ) ) ;
#88770 = ORIENTED_EDGE ( 'NONE', *, *, #60727, .T. ) ;
#88771 = PRESENTATION_STYLE_ASSIGNMENT (( #41336 ) ) ;
#88772 = CARTESIAN_POINT ( 'NONE',  ( -12.83294900548052730, 0.5000000000000004441, -7.766300266068542513 ) ) ;
#88773 = CARTESIAN_POINT ( 'NONE',  ( -4.164238869374099039, 61.80374883491397497, 8.674139862899312516E-16 ) ) ;
#88774 = CARTESIAN_POINT ( 'NONE',  ( 15.44008868035555793, 16.39701867748817321, -9.422509992056140149 ) ) ;
#88775 = CARTESIAN_POINT ( 'NONE',  ( 2.917880565312950480, 35.97041550158063217, -12.26659068614894821 ) ) ;
#88776 = CARTESIAN_POINT ( 'NONE',  ( 0.5774900079438590739, 37.64701867748817676, -5.440088680355550821 ) ) ;
#88777 = CARTESIAN_POINT ( 'NONE',  ( 20.88017736071110519, 60.56368534415484106, 2.639326808657452039E-16 ) ) ;
#88778 = CARTESIAN_POINT ( 'NONE',  ( -0.7375392941516041301, 14.63606910178966913, -14.98185688723475906 ) ) ;
#88779 = EDGE_CURVE ( 'NONE', #94453, #52640, #69679, .T. ) ;
#88780 = CARTESIAN_POINT ( 'NONE',  ( 20.15039907845753575, 39.72266099184919597, 6.262539305110075283 ) ) ;
#88781 = CARTESIAN_POINT ( 'NONE',  ( 17.20831665107776587, 29.13393115100078390, -7.208316651077762316 ) ) ;
#88782 = DIRECTION ( 'NONE',  ( 0.9812560818990571088, 0.1927083333333329818, 0.000000000000000000 ) ) ;
#88783 = CARTESIAN_POINT ( 'NONE',  ( 7.361572987183169658, 9.967264484334119601, -9.846743663894592657 ) ) ;
#88784 =( NAMED_UNIT ( * ) PLANE_ANGLE_UNIT ( ) SI_UNIT ( $, .RADIAN. ) );
#88785 = CARTESIAN_POINT ( 'NONE',  ( 1.472469842513823179, 41.42559781766745886, 4.923371831947296329 ) ) ;
#88786 = CARTESIAN_POINT ( 'NONE',  ( 14.92337183194729988, 59.34226448433412315, -8.527530157486177487 ) ) ;
#88787 = COLOUR_RGB ( '', 0.09019608, 0.27058824, 0.51372549) ;
#88788 = VECTOR ( 'NONE', #96636, 1000.000000000000000 ) ;
#88789 = ADVANCED_FACE ( 'NONE', ( #1210 ), #71351, .T. ) ;
#88790 = CARTESIAN_POINT ( 'NONE',  ( -0.8801773607110991993, 32.85535201082151247, -2.915334737309923874 ) ) ;
#88791 = ORIENTED_EDGE ( 'NONE', *, *, #67868, .F. ) ;
#88792 = CARTESIAN_POINT ( 'NONE',  ( 19.38216949554541557, 47.24863466993041783, -9.382169495545420901 ) ) ;
#88793 = CARTESIAN_POINT ( 'NONE',  ( -0.3329122712636025105, 0.000000000000000000, 5.443067521379386875 ) ) ;
#88794 = CARTESIAN_POINT ( 'NONE',  ( 2.791683348922237240, 0.3839311510007847872, -7.208316651077763204 ) ) ;
#88795 = CARTESIAN_POINT ( 'NONE',  ( -1.099225684535947600, 38.70696800326375353, -6.408140936763238038 ) ) ;
#88797 = CARTESIAN_POINT ( 'NONE',  ( 2.791683348922237240, 35.38393115100079456, -7.208316651077763204 ) ) ;
#88796 = CARTESIAN_POINT ( 'NONE',  ( 10.00000000000000178, 58.05374883491397497, 14.16423886937410082 ) ) ;
#88798 = CARTESIAN_POINT ( 'NONE',  ( 8.979999999999991545, 21.00000000000000000, -2.899999999999999911 ) ) ;
#88799 = CARTESIAN_POINT ( 'NONE',  ( 2.791683348922240793, 61.63393115100079456, 7.208316651077764092 ) ) ;
#88800 = CARTESIAN_POINT ( 'NONE',  ( -0.3689425029237898834, 26.17874883491396432, -10.36894250292378850 ) ) ;
#88801 = CARTESIAN_POINT ( 'NONE',  ( 12.63842701281683922, 39.55059781766744464, -9.846743663894590881 ) ) ;
#88802 = CARTESIAN_POINT ( 'NONE',  ( 19.88565890683628368, 12.71691075486302580, -6.480892540919847455 ) ) ;
#88803 = CARTESIAN_POINT ( 'NONE',  ( 0.5774900079438607392, 38.48035201082150536, 5.440088680355550821 ) ) ;
#88804 = CARTESIAN_POINT ( 'NONE',  ( 15.44008868035555260, 54.73035201082150536, 9.422509992056143702 ) ) ;
#88805 = DIRECTION ( 'NONE',  ( -0.000000000000000000, -1.000000000000000000, -0.000000000000000000 ) ) ;
#88806 = VERTEX_POINT ( 'NONE', #77171 ) ;
#88807 = CARTESIAN_POINT ( 'NONE',  ( 0.6178305044545838731, 44.74863466993042493, 9.382169495545420901 ) ) ;
#88808 = CARTESIAN_POINT ( 'NONE',  ( 17.20831665107776587, 2.883931151000785231, 7.208316651077764980 ) ) ;
#88809 = ORIENTED_EDGE ( 'NONE', *, *, #74957, .F. ) ;
#88810 = CARTESIAN_POINT ( 'NONE',  ( 2.917880565312948704, 12.63708216824730179, 12.26659068614894643 ) ) ;
#88811 = CARTESIAN_POINT ( 'NONE',  ( 14.92337183194729988, 4.342264484334117824, -8.527530157486177487 ) ) ;
#88812 = CARTESIAN_POINT ( 'NONE',  ( 1.250199848463767305, 0.007464128780085518312, -6.094592771028128020 ) ) ;
#88813 = VECTOR ( 'NONE', #9421, 1000.000000000000000 ) ;
#88814 = ORIENTED_EDGE ( 'NONE', *, *, #34080, .F. ) ;
#88815 = CARTESIAN_POINT ( 'NONE',  ( 64.56412365047461321, 44.99999999999998579, 7.000000000000000000 ) ) ;
#88816 = CARTESIAN_POINT ( 'NONE',  ( 4.559911319644449179, 8.897018677488171434, 9.422509992056141925 ) ) ;
#88817 = CARTESIAN_POINT ( 'NONE',  ( -11.92686044187656869, 12.45379003517447636, -3.195792623639521768 ) ) ;
#88818 = CARTESIAN_POINT ( 'NONE',  ( 22.26659068614894466, 18.88708216824730002, 7.082119434687054849 ) ) ;
#88819 = COLOUR_RGB ( '', 0.09019608, 0.27058824, 0.51372549) ;
#88820 = CARTESIAN_POINT ( 'NONE',  ( 15.44008868035555260, 24.73035201082150891, 9.422509992056143702 ) ) ;
#88821 = CARTESIAN_POINT ( 'NONE',  ( 10.00000000000000178, 62.25893115100078745, 9.846743663894594434 ) ) ;
#88822 = VERTEX_POINT ( 'NONE', #60199 ) ;
#88823 = CARTESIAN_POINT ( 'NONE',  ( 12.63842701281683922, 59.55059781766744464, -9.846743663894590881 ) ) ;
#88824 = ORIENTED_EDGE ( 'NONE', *, *, #2294, .T. ) ;
#88825 = CARTESIAN_POINT ( 'NONE',  ( 17.96484262340118221, 66.18868534415483396, -7.964842623401177768 ) ) ;
#88826 = CARTESIAN_POINT ( 'NONE',  ( 18.52753015748617571, 63.09226448433412315, 4.923371831947298993 ) ) ;
#88827 = CARTESIAN_POINT ( 'NONE',  ( 13.43411237798106583, 37.66530133659708923, -12.81628187352647252 ) ) ;
#88829 = CARTESIAN_POINT ( 'NONE',  ( -7.551349515323269479, -0.03417435944610275333, 12.08468537022900868 ) ) ;
#88828 = CARTESIAN_POINT ( 'NONE',  ( 4.559911319644449179, 2.230352010821504471, -9.422509992056141925 ) ) ;
#88830 = CARTESIAN_POINT ( 'NONE',  ( 2.791683348922240793, 1.633931151000784565, 7.208316651077764092 ) ) ;
#88831 = CARTESIAN_POINT ( 'NONE',  ( 0.5774900079438607392, 18.48035201082150536, 5.440088680355550821 ) ) ;
#88832 = ADVANCED_FACE ( 'NONE', ( #82704 ), #12305, .T. ) ;
#88833 = AXIS2_PLACEMENT_3D ( 'NONE', #65460, #27468, #29924 ) ;
#88834 = AXIS2_PLACEMENT_3D ( 'NONE', #28830, #89348, #80864 ) ;
#88835 = EDGE_LOOP ( 'NONE', ( #50066, #26115, #11001, #79347, #63414, #18811 ) ) ;
#88836 = AXIS2_PLACEMENT_3D ( 'NONE', #9555, #69084, #76571 ) ;
#88837 = CARTESIAN_POINT ( 'NONE',  ( 21.09922568453595559, 52.04030133659708923, -6.408140936763230044 ) ) ;
#88838 = CARTESIAN_POINT ( 'NONE',  ( 0.5774900079438607392, 28.48035201082150891, 5.440088680355550821 ) ) ;
#88839 = CARTESIAN_POINT ( 'NONE',  ( -46.94000000000000483, 100.6164469616018238, -8.719320056940125241 ) ) ;
#88840 = CARTESIAN_POINT ( 'NONE',  ( 13.43411237798106583, 37.66530133659708923, -12.81628187352647252 ) ) ;
#88841 = CARTESIAN_POINT ( 'NONE',  ( 4.559911319644449179, 53.89701867748817676, 9.422509992056141925 ) ) ;
#88842 = CARTESIAN_POINT ( 'NONE',  ( 17.20831665107776587, 52.88393115100078035, 7.208316651077764980 ) ) ;
#88843 = ORIENTED_EDGE ( 'NONE', *, *, #9359, .T. ) ;
#88844 = CARTESIAN_POINT ( 'NONE',  ( -0.1038446121089038471, 49.24302437010793909, -6.337995344473782211 ) ) ;
#88845 = CARTESIAN_POINT ( 'NONE',  ( 7.361572987183169658, 9.967264484334119601, -9.846743663894592657 ) ) ;
#88846 = CARTESIAN_POINT ( 'NONE',  ( 22.81628187352647785, 11.62363466993042138, 6.195893100308588602E-16 ) ) ;
#88848 = CARTESIAN_POINT ( 'NONE',  ( 2.791683348922240793, 51.63393115100078745, 7.208316651077764092 ) ) ;
#88847 = DIRECTION ( 'NONE',  ( -0.000000000000000000, 1.000000000000000000, -0.000000000000000000 ) ) ;
#88849 = CARTESIAN_POINT ( 'NONE',  ( 4.559911319644449179, 27.23035201082150536, -9.422509992056141925 ) ) ;
#88850 = CARTESIAN_POINT ( 'NONE',  ( 14.92337183194729988, 49.34226448433411605, -8.527530157486177487 ) ) ;
#88851 = CARTESIAN_POINT ( 'NONE',  ( -10.64017930668216749, 14.63606904708525747, 10.57291749337210085 ) ) ;
#88852 = PRESENTATION_LAYER_ASSIGNMENT (  '', '', ( #53747 ) ) ;
#88853 = DIRECTION ( 'NONE',  ( 0.8949343616020259962, 0.000000000000000000, 0.4461978131098069955 ) ) ;
#88854 = CARTESIAN_POINT ( 'NONE',  ( 2.791683348922240793, 6.633931151000785675, 7.208316651077764092 ) ) ;
#88856 = VERTEX_POINT ( 'NONE', #15218 ) ;
#88855 = CARTESIAN_POINT ( 'NONE',  ( 12.63842701281683034, 57.46726448433411605, 9.846743663894596210 ) ) ;
#88857 = VECTOR ( 'NONE', #54155, 1000.000000000000000 ) ;
#88858 = CYLINDRICAL_SURFACE ( 'NONE', #75829, 15.00000000000000000 ) ;
#88859 = CARTESIAN_POINT ( 'NONE',  ( 0.6178305044545818747, 43.49863466993042493, -9.382169495545419124 ) ) ;
#88860 = EDGE_CURVE ( 'NONE', #10376, #9175, #66556, .T. ) ;
#88861 = CARTESIAN_POINT ( 'NONE',  ( 12.63842701281683922, 29.55059781766745175, -9.846743663894590881 ) ) ;
#88862 = CARTESIAN_POINT ( 'NONE',  ( -0.1503990784575407469, 12.22266099184918531, -6.262539305110056631 ) ) ;
#88863 = CARTESIAN_POINT ( 'NONE',  ( 10.00000000000000000, 60.55374883491397497, -14.16423886937410082 ) ) ;
#88864 = CARTESIAN_POINT ( 'NONE',  ( 18.52753015748617571, 33.09226448433411605, 4.923371831947298993 ) ) ;
#88865 = AXIS2_PLACEMENT_3D ( 'NONE', #11954, #42948, #35434 ) ;
#88866 = ORIENTED_EDGE ( 'NONE', *, *, #10097, .F. ) ;
#88867 = CARTESIAN_POINT ( 'NONE',  ( 19.64232630867105556, 84.97379543201886065, 5.304930624720102017 ) ) ;
#88868 = ADVANCED_FACE ( 'NONE', ( #61186 ), #28212, .T. ) ;
#88869 = CARTESIAN_POINT ( 'NONE',  ( 20.36894250292379382, 58.67874883491396076, 10.36894250292379205 ) ) ;
#88870 = DIRECTION ( 'NONE',  ( -0.000000000000000000, -0.000000000000000000, -1.000000000000000000 ) ) ;
#88871 = CARTESIAN_POINT ( 'NONE',  ( 20.88017736071110875, 15.77201867748817143, -2.915334737309920765 ) ) ;
#88872 = CARTESIAN_POINT ( 'NONE',  ( -4.164238869374098151, 41.59541550158061796, -3.795296366450310543 ) ) ;
#88874 = CARTESIAN_POINT ( 'NONE',  ( 3.541595367958660479, 0.000000000000000000, 4.146675399920616734 ) ) ;
#88873 = CARTESIAN_POINT ( 'NONE',  ( 2.917880565312950480, 55.97041550158063217, -12.26659068614894821 ) ) ;
#88875 = CARTESIAN_POINT ( 'NONE',  ( 20.88017736071110875, 5.772018677488170546, -2.915334737309920321 ) ) ;
#88876 = CARTESIAN_POINT ( 'NONE',  ( 0.1532563361054082862, 6.217264484334118713, 2.638427012816831674 ) ) ;
#88877 = CARTESIAN_POINT ( 'NONE',  ( 0.6178305044545818747, -1.501365330069579951, -9.382169495545419124 ) ) ;
#88878 = CARTESIAN_POINT ( 'NONE',  ( 17.62281668512002852, 13.28593319516822469, 6.499999999999993783 ) ) ;
#88879 = CARTESIAN_POINT ( 'NONE',  ( -0.8801773607111009756, 48.06368534415484817, 1.068504757029289695E-15 ) ) ;
#88880 = DIRECTION ( 'NONE',  ( 1.000000000000000000, 0.000000000000000000, 0.000000000000000000 ) ) ;
#88881 = CARTESIAN_POINT ( 'NONE',  ( 14.92337183194729988, 49.34226448433411605, -8.527530157486177487 ) ) ;
#88882 = DIRECTION ( 'NONE',  ( 0.5075383629606904368, 0.000000000000000000, 0.8616291604415338146 ) ) ;
#88883 = CIRCLE ( 'NONE', #17033, 19.99999999999999645 ) ;
#88884 = CARTESIAN_POINT ( 'NONE',  ( 67.06412365047464164, 22.49999999999998934, -10.00000000000000000 ) ) ;
#88885 =( NAMED_UNIT ( * ) PLANE_ANGLE_UNIT ( ) SI_UNIT ( $, .RADIAN. ) );
#88886 = ORIENTED_EDGE ( 'NONE', *, *, #12492, .F. ) ;
#88887 = CARTESIAN_POINT ( 'NONE',  ( -2.266590686148945544, 36.38708216824730357, -7.082119434687050408 ) ) ;
#88888 = AXIS2_PLACEMENT_3D ( 'NONE', #59578, #21595, #14091 ) ;
#88889 = CARTESIAN_POINT ( 'NONE',  ( 0.9408516040111475354, 37.46693863883976405, -6.499999999999953815 ) ) ;
#88891 = DIRECTION ( 'NONE',  ( 0.3007057995042832221, 0.000000000000000000, -0.9537169507482238240 ) ) ;
#88890 = CARTESIAN_POINT ( 'NONE',  ( -12.34086200392816757, -0.03417435944610275333, -7.125000000000143885 ) ) ;
#88892 = CARTESIAN_POINT ( 'NONE',  ( 17.96484262340118221, 21.18868534415483396, -7.964842623401177768 ) ) ;
#88893 = CARTESIAN_POINT ( 'NONE',  ( -1.099225684535947600, 43.70696800326375353, -6.408140936763238038 ) ) ;
#88894 = CARTESIAN_POINT ( 'NONE',  ( -8.731067818237029599, 10.31330936912750396, 8.731067818237042033 ) ) ;
#88895 = CARTESIAN_POINT ( 'NONE',  ( 10.00000000000000178, 20.37363466993042138, 12.81628187352647608 ) ) ;
#88896 = CARTESIAN_POINT ( 'NONE',  ( 3.591859063236761518, 64.95696800326376774, 11.09922568453594849 ) ) ;
#88897 = ORIENTED_EDGE ( 'NONE', *, *, #74390, .T. ) ;
#88898 = DIRECTION ( 'NONE',  ( 1.049065152435176504E-16, -1.000000000000000000, 0.000000000000000000 ) ) ;
#88899 = CARTESIAN_POINT ( 'NONE',  ( -10.77974636252767482, -96.52223143589499443, -4.000000000000000888 ) ) ;
#88900 = CARTESIAN_POINT ( 'NONE',  ( 17.08211943468705130, 28.47041550158063572, 12.26659068614894998 ) ) ;
#88901 = CARTESIAN_POINT ( 'NONE',  ( -7.330068351210570654, -69.53589943318685584, 4.000000000000000000 ) ) ;
#88902 = CARTESIAN_POINT ( 'NONE',  ( 10.00000000000000178, 24.31368534415484106, 10.88017736071110342 ) ) ;
#88903 = CARTESIAN_POINT ( 'NONE',  ( 19.72487221294570858, 70.00000000000000000, 6.500000000000000888 ) ) ;
#88904 = CARTESIAN_POINT ( 'NONE',  ( 19.42250999205614193, 40.14701867748817676, 5.440088680355555262 ) ) ;
#88905 = CARTESIAN_POINT ( 'NONE',  ( 10.00000000000000000, 46.81368534415484106, -10.88017736071110342 ) ) ;
#88906 = CARTESIAN_POINT ( 'NONE',  ( -1.099225684535947600, 14.54030133659708568, 6.408140936763237150 ) ) ;
#88907 = CARTESIAN_POINT ( 'NONE',  ( -5.817157072110893168, 0.5000000000000004441, 13.82608706751082828 ) ) ;
#88908 = DIRECTION ( 'NONE',  ( 0.9170600743851238246, 0.000000000000000000, -0.3987490689252466414 ) ) ;
#88909 = CARTESIAN_POINT ( 'NONE',  ( 17.20831665107776587, 17.88393115100078745, 7.208316651077764980 ) ) ;
#88910 = CARTESIAN_POINT ( 'NONE',  ( -18.89999999999999147, 99.74999999999998579, -8.000000000000000000 ) ) ;
#88911 = CARTESIAN_POINT ( 'NONE',  ( 17.96484262340118221, 46.18868534415484106, -7.964842623401177768 ) ) ;
#88912 = EDGE_CURVE ( 'NONE', #91250, #38990, #87317, .T. ) ;
#88913 = CIRCLE ( 'NONE', #45809, 1.499999999999996669 ) ;
#88914 = TOROIDAL_SURFACE ( 'NONE', #5912, 14.49999999999999822, 0.5000000000000000000 ) ;
#88915 = CARTESIAN_POINT ( 'NONE',  ( -1.099225684535947600, -0.4596986634029132657, 6.408140936763237150 ) ) ;
#88916 = CARTESIAN_POINT ( 'NONE',  ( 1.274849032794278747, 42.55509018479936856, -6.499999999999960032 ) ) ;
#88917 = CARTESIAN_POINT ( 'NONE',  ( 10.00000000000000178, 27.25893115100078390, 9.846743663894594434 ) ) ;
#88918 = CARTESIAN_POINT ( 'NONE',  ( 10.00000000000000000, 52.87363466993041783, -12.81628187352647608 ) ) ;
#88919 = CARTESIAN_POINT ( 'NONE',  ( 2.791683348922240793, 11.63393115100078568, 7.208316651077764092 ) ) ;
#88920 = ORIENTED_EDGE ( 'NONE', *, *, #21152, .T. ) ;
#88921 = CARTESIAN_POINT ( 'NONE',  ( 2.603489959281582777, 31.58210964143329136, 6.499999999999995559 ) ) ;
#88922 = CARTESIAN_POINT ( 'NONE',  ( 4.559911319644449179, 18.89701867748817321, 9.422509992056141925 ) ) ;
#88923 = DIRECTION ( 'NONE',  ( 0.000000000000000000, -1.000000000000000000, 0.000000000000000000 ) ) ;
#88924 = CARTESIAN_POINT ( 'NONE',  ( 2.791683348922237240, 30.38393115100078390, -7.208316651077763204 ) ) ;
#88925 = CARTESIAN_POINT ( 'NONE',  ( 12.91533473730993009, 21.60535201082150536, -10.88017736071109987 ) ) ;
#88926 = CARTESIAN_POINT ( 'NONE',  ( 19.42250999205614548, 5.980352010821504471, -5.440088680355545492 ) ) ;
#88927 = ORIENTED_EDGE ( 'NONE', *, *, #47675, .T. ) ;
#88928 = CARTESIAN_POINT ( 'NONE',  ( 0.5774900079438590739, 32.64701867748816966, -5.440088680355550821 ) ) ;
#88929 = CARTESIAN_POINT ( 'NONE',  ( 19.42250999205614548, 40.98035201082150536, -5.440088680355545492 ) ) ;
#88931 = CARTESIAN_POINT ( 'NONE',  ( 12.91533473730993009, 41.60535201082149825, -10.88017736071109987 ) ) ;
#88930 = CARTESIAN_POINT ( 'NONE',  ( -5.240416992896607340, 14.95077488074853811, -13.79072622793306913 ) ) ;
#88932 = ORIENTED_EDGE ( 'NONE', *, *, #8490, .T. ) ;
#88933 = CARTESIAN_POINT ( 'NONE',  ( 14.92337183194729633, 62.67559781766745886, 8.527530157486181039 ) ) ;
#88934 = CARTESIAN_POINT ( 'NONE',  ( 2.035157376598824452, 38.68868534415483396, 7.964842623401179544 ) ) ;
#88935 = CARTESIAN_POINT ( 'NONE',  ( 4.395886033851783559, -0.8422402087859571784, 3.750000000000000000 ) ) ;
#88936 = DIRECTION ( 'NONE',  ( 5.329070518200751394E-14, 0.000000000000000000, 1.000000000000000000 ) ) ;
#88937 = CARTESIAN_POINT ( 'NONE',  ( 13.43411237798105340, 60.58196800326376064, 12.81628187352647963 ) ) ;
#88938 = CARTESIAN_POINT ( 'NONE',  ( 0.000000000000000000, 14.49999999999999822, 0.000000000000000000 ) ) ;
#88939 = CARTESIAN_POINT ( 'NONE',  ( 17.08211943468705840, 30.13708216824730357, -12.26659068614894466 ) ) ;
#88940 = CARTESIAN_POINT ( 'NONE',  ( 10.00000000000000000, 51.81368534415484106, -10.88017736071110342 ) ) ;
#88941 = CARTESIAN_POINT ( 'NONE',  ( 20.88017736071110164, 30.35535201082151247, 2.915334737309930979 ) ) ;
#88942 = CARTESIAN_POINT ( 'NONE',  ( 0.000000000000000000, 15.00000000000000000, 0.000000000000000000 ) ) ;
#88943 = CARTESIAN_POINT ( 'NONE',  ( 20.15039907845753220, 27.62777174578613071, -6.262539305110077947 ) ) ;
#88945 = EDGE_CURVE ( 'NONE', #84166, #37561, #21623, .T. ) ;
#88944 = CARTESIAN_POINT ( 'NONE',  ( 0.1532563361054083140, 56.00893115100078745, 1.131784320476157264E-15 ) ) ;
#88946 = ORIENTED_EDGE ( 'NONE', *, *, #44801, .F. ) ;
#88947 = DIRECTION ( 'NONE',  ( -1.000000000000000000, 0.000000000000000000, 0.000000000000000000 ) ) ;
#88948 = CARTESIAN_POINT ( 'NONE',  ( 17.20831665107776587, 19.13393115100078035, -7.208316651077762316 ) ) ;
#88949 = CARTESIAN_POINT ( 'NONE',  ( -3.434112377981067610, -16.91803199673624647, -12.81628187352647252 ) ) ;
#88950 = CARTESIAN_POINT ( 'NONE',  ( 17.96484262340118221, 9.938685344154837509, 7.964842623401181321 ) ) ;
#88951 = CARTESIAN_POINT ( 'NONE',  ( 0.1532563361054100626, 30.80059781766744820, -2.638427012816831230 ) ) ;
#88952 = CARTESIAN_POINT ( 'NONE',  ( 13.43411237798105340, 10.58196800326375353, 12.81628187352647963 ) ) ;
#88953 = CARTESIAN_POINT ( 'NONE',  ( 0.5774900079438590739, 62.64701867748817676, -5.440088680355550821 ) ) ;
#88955 = CARTESIAN_POINT ( 'NONE',  ( 3.591859063236763294, 58.29030133659708923, -11.09922568453595026 ) ) ;
#88954 = CARTESIAN_POINT ( 'NONE',  ( -0.8801773607110991993, 32.85535201082151247, -2.915334737309923874 ) ) ;
#88956 = CARTESIAN_POINT ( 'NONE',  ( -4.164238869374098151, 51.59541550158063217, -3.795296366450310543 ) ) ;
#88957 = EDGE_CURVE ( 'NONE', #60892, #42806, #41653, .T. ) ;
#88959 = DIRECTION ( 'NONE',  ( 1.000000000000000000, 0.000000000000000000, 0.000000000000000000 ) ) ;
#88958 = AXIS2_PLACEMENT_3D ( 'NONE', #45574, #6589, #7597 ) ;
#88960 = EDGE_CURVE ( 'NONE', #78529, #31207, #46432, .T. ) ;
#88961 = ORIENTED_EDGE ( 'NONE', *, *, #26094, .T. ) ;
#88962 = CARTESIAN_POINT ( 'NONE',  ( 7.361572987183169658, 64.96726448433412315, -9.846743663894592657 ) ) ;
#88963 = CARTESIAN_POINT ( 'NONE',  ( 19.42250999205614193, 10.14701867748816966, 5.440088680355555262 ) ) ;
#88964 = CARTESIAN_POINT ( 'NONE',  ( 15.44008868035555793, 41.39701867748817676, -9.422509992056140149 ) ) ;
#88965 = CARTESIAN_POINT ( 'NONE',  ( 12.63842701281683922, 64.55059781766745175, -9.846743663894590881 ) ) ;
#88966 = ORIENTED_EDGE ( 'NONE', *, *, #69829, .T. ) ;
#88967 = CARTESIAN_POINT ( 'NONE',  ( 10.00000000000000178, 22.25893115100078745, 9.846743663894594434 ) ) ;
#88968 = AXIS2_PLACEMENT_3D ( 'NONE', #7324, #45308, #37827 ) ;
#88969 = CARTESIAN_POINT ( 'NONE',  ( 2.791683348922240793, 11.63393115100078568, 7.208316651077764092 ) ) ;
#88970 = CARTESIAN_POINT ( 'NONE',  ( 14.92337183194729633, 17.67559781766745175, 8.527530157486181039 ) ) ;
#88971 = CARTESIAN_POINT ( 'NONE',  ( 14.92337183194729633, 12.67559781766745353, 8.527530157486181039 ) ) ;
#88972 = CARTESIAN_POINT ( 'NONE',  ( 17.20831665107776587, 4.133931151000785675, -7.208316651077762316 ) ) ;
#88973 = CARTESIAN_POINT ( 'NONE',  ( -7.116252256210342964, -80.68108970088772480, 2.499999999998790745 ) ) ;
#88976 = CARTESIAN_POINT ( 'NONE',  ( 17.35999999999999943, 37.99999999999997868, 7.000000000000000000 ) ) ;
#88975 = CIRCLE ( 'NONE', #92194, 0.2500000000000002220 ) ;
#88974 = CARTESIAN_POINT ( 'NONE',  ( 5.076628168052703671, 6.842264484334118713, 8.527530157486179263 ) ) ;
#88977 = CARTESIAN_POINT ( 'NONE',  ( 12.63842701281683922, 9.550597817667449974, -9.846743663894590881 ) ) ;
#88979 = VERTEX_POINT ( 'NONE', #56638 ) ;
#88978 = CARTESIAN_POINT ( 'NONE',  ( 0.1532563361054082862, 16.21726448433411960, 2.638427012816831674 ) ) ;
#88980 = AXIS2_PLACEMENT_3D ( 'NONE', #65295, #12309, #65792 ) ;
#88981 = DIRECTION ( 'NONE',  ( 0.8070303256584298035, -0.5905099943842175847, 0.000000000000000000 ) ) ;
#88983 = ADVANCED_FACE ( 'NONE', ( #85664 ), #34620, .T. ) ;
#88982 = CARTESIAN_POINT ( 'NONE',  ( 10.00000000000000178, 0.3736346699304200492, 12.81628187352647608 ) ) ;
#88984 = ORIENTED_EDGE ( 'NONE', *, *, #45293, .F. ) ;
#88985 = CARTESIAN_POINT ( 'NONE',  ( 0.2751277870542980231, 14.36607318730130878, -6.500000000000002665 ) ) ;
#88986 = CARTESIAN_POINT ( 'NONE',  ( 2.917880565312948704, 17.63708216824730357, 12.26659068614894643 ) ) ;
#88987 = FACE_OUTER_BOUND ( 'NONE', #59930, .T. ) ;
#88988 = EDGE_CURVE ( 'NONE', #1670, #76760, #41015, .T. ) ;
#88989 = CARTESIAN_POINT ( 'NONE',  ( -2.266590686148945544, 21.38708216824730357, -7.082119434687050408 ) ) ;
#88990 = CARTESIAN_POINT ( 'NONE',  ( 24.16423886937410614, 49.51208216824730357, -3.795296366450302550 ) ) ;
#88991 = LINE ( 'NONE', #26510, #90167 ) ;
#88992 = CARTESIAN_POINT ( 'NONE',  ( -2.266590686148945544, 7.220415501580634832, 7.082119434687048631 ) ) ;
#88993 = CARTESIAN_POINT ( 'NONE',  ( 4.559911319644449179, 38.89701867748817676, 9.422509992056141925 ) ) ;
#88994 = DIRECTION ( 'NONE',  ( -1.000000000000000000, 0.000000000000000000, 0.000000000000000000 ) ) ;
#88995 = ORIENTED_EDGE ( 'NONE', *, *, #87136, .F. ) ;
#88996 = CARTESIAN_POINT ( 'NONE',  ( 14.92337183194729633, 22.67559781766745175, 8.527530157486181039 ) ) ;
#88998 = CARTESIAN_POINT ( 'NONE',  ( 7.361572987183169658, 34.96726448433411605, -9.846743663894592657 ) ) ;
#88997 = CARTESIAN_POINT ( 'NONE',  ( -0.8801773607110991993, 57.85535201082149825, -2.915334737309923874 ) ) ;
#88999 = CARTESIAN_POINT ( 'NONE',  ( 7.084665262690076126, 9.105352010821503583, 10.88017736071109987 ) ) ;
#89000 = CARTESIAN_POINT ( 'NONE',  ( 22.81628187352647785, 61.62363466993041783, 6.195893100308588602E-16 ) ) ;
#89001 = CARTESIAN_POINT ( 'NONE',  ( 12.63842701281683034, 47.46726448433412315, 9.846743663894596210 ) ) ;
#89002 = DIRECTION ( 'NONE',  ( 1.000000000000000000, 0.000000000000000000, 0.000000000000000000 ) ) ;
#89003 = CARTESIAN_POINT ( 'NONE',  ( 6.565887622018943937, 43.08196800326374643, -12.81628187352647608 ) ) ;
#89004 = CARTESIAN_POINT ( 'NONE',  ( -7.082119434687058401, -24.02958449841936073, -12.26659068614894110 ) ) ;
#89005 = CARTESIAN_POINT ( 'NONE',  ( -0.8801773607111008646, 48.27201867748816966, 2.915334737309923430 ) ) ;
#89006 = CARTESIAN_POINT ( 'NONE',  ( 1.472469842513823179, 41.42559781766745886, 4.923371831947296329 ) ) ;
#89007 = CARTESIAN_POINT ( 'NONE',  ( -4.164238869374099039, 31.80374883491396432, 8.674139862899312516E-16 ) ) ;
#89008 = ORIENTED_EDGE ( 'NONE', *, *, #27556, .F. ) ;
#89009 = VECTOR ( 'NONE', #62834, 1000.000000000000000 ) ;
#89010 = CARTESIAN_POINT ( 'NONE',  ( 12.91533473730992121, 54.52201867748816255, 10.88017736071110164 ) ) ;
#89011 = CARTESIAN_POINT ( 'NONE',  ( 17.96484262340118221, 61.18868534415482685, -7.964842623401177768 ) ) ;
#89012 = CARTESIAN_POINT ( 'NONE',  ( -4.164238869374098151, 51.59541550158063217, -3.795296366450310543 ) ) ;
#89013 = CARTESIAN_POINT ( 'NONE',  ( 6.565887622018943937, -1.918031996736246692, -12.81628187352647608 ) ) ;
#89014 = CARTESIAN_POINT ( 'NONE',  ( 6.000000000000000000, 61.00000000000000711, -5.000000000000000000 ) ) ;
#89015 = CARTESIAN_POINT ( 'NONE',  ( 7.084665262690076126, 39.10535201082150536, 10.88017736071109987 ) ) ;
#89016 = DIRECTION ( 'NONE',  ( -1.000000000000000000, 0.000000000000000000, 0.000000000000000000 ) ) ;
#89017 = CARTESIAN_POINT ( 'NONE',  ( 17.20831665107776587, 47.88393115100078745, 7.208316651077764980 ) ) ;
#89018 = CARTESIAN_POINT ( 'NONE',  ( 7.964842623401181321, 9.938685344154839285, 7.964842623401174215 ) ) ;
#89019 = PRESENTATION_STYLE_ASSIGNMENT (( #66011 ) ) ;
#89020 = CARTESIAN_POINT ( 'NONE',  ( 19.42250999205614193, 15.14701867748817143, 5.440088680355555262 ) ) ;
#89021 = EDGE_LOOP ( 'NONE', ( #76073, #63401, #41476, #445 ) ) ;
#89022 = COLOUR_RGB ( '', 0.72549020, 0.75294118, 0.79215686) ;
#89023 = CARTESIAN_POINT ( 'NONE',  ( 10.00000000000000178, 4.313685344154837509, 10.88017736071110342 ) ) ;
#89024 = FACE_OUTER_BOUND ( 'NONE', #84299, .T. ) ;
#89025 = CARTESIAN_POINT ( 'NONE',  ( -0.8801773607111008646, 68.27201867748817676, 2.915334737309923430 ) ) ;
#89026 = TOROIDAL_SURFACE ( 'NONE', #96978, 14.49999999999999822, 0.5000000000000000000 ) ;
#89027 = CARTESIAN_POINT ( 'NONE',  ( 10.00000000000000178, 69.31368534415484817, 10.88017736071110342 ) ) ;
#89028 = CARTESIAN_POINT ( 'NONE',  ( 14.92337183194729988, 29.34226448433411960, -8.527530157486177487 ) ) ;
#89029 = CARTESIAN_POINT ( 'NONE',  ( 12.91533473730993009, 16.60535201082150891, -10.88017736071109987 ) ) ;
#89030 = CARTESIAN_POINT ( 'NONE',  ( 21.09922568453594849, 11.20696800326375531, 6.408140936763242479 ) ) ;
#89032 = CARTESIAN_POINT ( 'NONE',  ( 8.731067818237038480, 10.78712336850781739, -8.731067818237040257 ) ) ;
#89031 = CARTESIAN_POINT ( 'NONE',  ( 7.084665262690076126, 37.02201867748817676, -10.88017736071110164 ) ) ;
#89033 = CARTESIAN_POINT ( 'NONE',  ( 10.00000000000000178, 35.37363466993042493, 12.81628187352647608 ) ) ;
#89034 = ORIENTED_EDGE ( 'NONE', *, *, #53620, .F. ) ;
#89035 = CARTESIAN_POINT ( 'NONE',  ( 20.88017736071110164, 60.35535201082151957, 2.915334737309930979 ) ) ;
#89037 = FILL_AREA_STYLE_COLOUR ( '', #57384 ) ;
#89036 = CARTESIAN_POINT ( 'NONE',  ( 6.565887622018943937, 25.16530133659708213, 12.81628187352647430 ) ) ;
#89038 = CARTESIAN_POINT ( 'NONE',  ( 21.92686044187656691, 32.18830936912750929, 4.562052436263911564E-16 ) ) ;
#89039 = CARTESIAN_POINT ( 'NONE',  ( 0.5774900079438607392, 33.48035201082150536, 5.440088680355550821 ) ) ;
#89040 = CARTESIAN_POINT ( 'NONE',  ( 0.2751277870542979120, 15.30223176428831344, 6.500000000000003553 ) ) ;
#89041 = CARTESIAN_POINT ( 'NONE',  ( 2.917880565312948704, 67.63708216824730357, 12.26659068614894643 ) ) ;
#89042 = CARTESIAN_POINT ( 'NONE',  ( 10.00000000000000178, 52.25893115100078745, 9.846743663894594434 ) ) ;
#89043 = CARTESIAN_POINT ( 'NONE',  ( 10.00000000000000000, -0.2410688489992152128, -9.846743663894594434 ) ) ;
#89044 = CARTESIAN_POINT ( 'NONE',  ( 4.559911319644449179, 58.89701867748817676, 9.422509992056141925 ) ) ;
#89045 = CARTESIAN_POINT ( 'NONE',  ( 13.79529636645030344, 28.26208216824729647, 14.16423886937410614 ) ) ;
#89046 = PRESENTATION_LAYER_ASSIGNMENT (  '', '', ( #47580 ) ) ;
#89047 =( NAMED_UNIT ( * ) PLANE_ANGLE_UNIT ( ) SI_UNIT ( $, .RADIAN. ) );
#89048 = CARTESIAN_POINT ( 'NONE',  ( 19.65595853167378948, 85.79736161466001931, -5.361990343729008401 ) ) ;
#89049 = VERTEX_POINT ( 'NONE', #24189 ) ;
#89050 = VERTEX_POINT ( 'NONE', #2684 ) ;
#89051 = CARTESIAN_POINT ( 'NONE',  ( -2.266590686148945544, 61.38708216824730357, -7.082119434687050408 ) ) ;
#89052 = CARTESIAN_POINT ( 'NONE',  ( 6.204703633549690345, 47.84541550158064638, 14.16423886937410082 ) ) ;
#89053 = CARTESIAN_POINT ( 'NONE',  ( 17.20831665107776587, 24.13393115100078035, -7.208316651077762316 ) ) ;
#89054 = CARTESIAN_POINT ( 'NONE',  ( 14.99999999999997868, 80.07179676972448590, 4.250000000000000000 ) ) ;
#89055 = DIRECTION ( 'NONE',  ( -0.000000000000000000, -0.000000000000000000, -1.000000000000000000 ) ) ;
#89056 = CARTESIAN_POINT ( 'NONE',  ( 17.96484262340118221, 11.18868534415483929, -7.964842623401177768 ) ) ;
#89057 = CARTESIAN_POINT ( 'NONE',  ( 17.08211943468705130, 53.47041550158063217, 12.26659068614894998 ) ) ;
#89058 = CARTESIAN_POINT ( 'NONE',  ( 12.63842701281683034, 22.46726448433411605, 9.846743663894596210 ) ) ;
#89059 = CARTESIAN_POINT ( 'NONE',  ( -14.49154782522702867, 0.04962890019108593537, 2.766288502466858201 ) ) ;
#89060 = CARTESIAN_POINT ( 'NONE',  ( 5.076628168052703671, 6.842264484334118713, 8.527530157486179263 ) ) ;
#89061 = CARTESIAN_POINT ( 'NONE',  ( 19.84674366389459266, 3.717264484334118713, -2.638427012816827677 ) ) ;
#89062 = CARTESIAN_POINT ( 'NONE',  ( -2.638427012816824124, -2.949402182332543365, 9.846743663894596210 ) ) ;
#89063 = VERTEX_POINT ( 'NONE', #25665 ) ;
#89064 = ORIENTED_EDGE ( 'NONE', *, *, #87973, .T. ) ;
#89065 = EDGE_CURVE ( 'NONE', #76154, #56374, #55662, .T. ) ;
#89066 = VERTEX_POINT ( 'NONE', #18644 ) ;
#89067 = CARTESIAN_POINT ( 'NONE',  ( 20.36894250292379738, 14.92874883491396432, -10.36894250292379027 ) ) ;
#89069 = CARTESIAN_POINT ( 'NONE',  ( 17.96484262340118221, 29.93868534415484106, 7.964842623401181321 ) ) ;
#89068 = CARTESIAN_POINT ( 'NONE',  ( 2.035157376598824452, 18.68868534415484106, 7.964842623401179544 ) ) ;
#89071 = CARTESIAN_POINT ( 'NONE',  ( 19.38216949554541202, 20.99863466993042138, 9.382169495545424454 ) ) ;
#89070 = CARTESIAN_POINT ( 'NONE',  ( 0.1532563361054082862, 46.21726448433411605, 2.638427012816831674 ) ) ;
#89072 = CARTESIAN_POINT ( 'NONE',  ( 6.204703633549690345, 10.76208216824729824, -14.16423886937410259 ) ) ;
#89073 = EDGE_CURVE ( 'NONE', #52137, #80996, #9171, .T. ) ;
#89074 = CARTESIAN_POINT ( 'NONE',  ( -2.816281873526473856, 29.33196800326376064, 3.434112377981055619 ) ) ;
#89075 = EDGE_CURVE ( 'NONE', #86688, #74051, #88374, .T. ) ;
#89076 = VERTEX_POINT ( 'NONE', #9668 ) ;
#89077 = CARTESIAN_POINT ( 'NONE',  ( 1.472469842513823179, 25.59226448433412315, -4.923371831947296329 ) ) ;
#89078 = CARTESIAN_POINT ( 'NONE',  ( -0.3689425029237898834, 66.17874883491396076, -10.36894250292378850 ) ) ;
#89079 = ORIENTED_EDGE ( 'NONE', *, *, #61081, .T. ) ;
#89080 = CARTESIAN_POINT ( 'NONE',  ( -0.3689425029237898834, 66.17874883491396076, -10.36894250292378850 ) ) ;
#89081 = ORIENTED_EDGE ( 'NONE', *, *, #35903, .T. ) ;
#89082 = CARTESIAN_POINT ( 'NONE',  ( -0.8801773607111009756, 53.06368534415484106, 1.068504757029289695E-15 ) ) ;
#89083 = CARTESIAN_POINT ( 'NONE',  ( 19.42250999205614548, 40.98035201082150536, -5.440088680355545492 ) ) ;
#89084 = CARTESIAN_POINT ( 'NONE',  ( -0.8801773607111009756, 53.06368534415484106, 1.068504757029289695E-15 ) ) ;
#89085 = LINE ( 'NONE', #64591, #2675 ) ;
#89086 = CARTESIAN_POINT ( 'NONE',  ( 15.44008868035555793, 41.39701867748817676, -9.422509992056140149 ) ) ;
#89087 = CARTESIAN_POINT ( 'NONE',  ( 1.383448333479233794, 47.37718327197428891, -6.499999999999977796 ) ) ;
#89090 = ORIENTED_EDGE ( 'NONE', *, *, #25107, .F. ) ;
#89089 = CIRCLE ( 'NONE', #66690, 0.09999999999999939493 ) ;
#89088 = DIRECTION ( 'NONE',  ( 0.000000000000000000, -1.000000000000000000, 0.000000000000000000 ) ) ;
#89091 = CARTESIAN_POINT ( 'NONE',  ( 19.84674366389459621, 33.50893115100078745, 7.409399052514197653E-17 ) ) ;
#89092 = ORIENTED_EDGE ( 'NONE', *, *, #77420, .T. ) ;
#89093 = CARTESIAN_POINT ( 'NONE',  ( 18.52753015748618282, 63.92559781766745886, -4.923371831947291888 ) ) ;
#89094 = CARTESIAN_POINT ( 'NONE',  ( -0.1038446121089049989, 24.24302437010794264, -6.337995344473780435 ) ) ;
#89095 = EDGE_CURVE ( 'NONE', #37098, #40499, #47664, .T. ) ;
#89096 = CARTESIAN_POINT ( 'NONE',  ( 2.917880565312948704, 7.637082168247301794, 12.26659068614894643 ) ) ;
#89097 = VECTOR ( 'NONE', #64116, 999.9999999999998863 ) ;
#89098 = VERTEX_POINT ( 'NONE', #2190 ) ;
#89099 =( NAMED_UNIT ( * ) SI_UNIT ( $, .STERADIAN. ) SOLID_ANGLE_UNIT ( ) );
#89100 = LINE ( 'NONE', #50111, #72960 ) ;
#89101 = CARTESIAN_POINT ( 'NONE',  ( -46.91881431881006392, 103.2388046827858545, -5.912160981969285523 ) ) ;
#89102 = CARTESIAN_POINT ( 'NONE',  ( 17.08211943468705840, 65.13708216824730357, -12.26659068614894466 ) ) ;
#89103 = DIRECTION ( 'NONE',  ( -0.8870108331782182720, 0.000000000000000000, -0.4617486132350404615 ) ) ;
#89104 = EDGE_LOOP ( 'NONE', ( #46070, #40229, #77145, #96527, #33223, #14625 ) ) ;
#89105 = DIRECTION ( 'NONE',  ( 0.7808688094430307203, -0.6246950475544238435, 0.000000000000000000 ) ) ;
#89106 = CARTESIAN_POINT ( 'NONE',  ( 19.84674366389459266, 28.30059781766745886, 2.638427012816836559 ) ) ;
#89107 = PLANE ( 'NONE',  #10036 ) ;
#89108 = VERTEX_POINT ( 'NONE', #32149 ) ;
#89109 = CARTESIAN_POINT ( 'NONE',  ( 3.591859063236763294, 8.290301336597087456, -11.09922568453595026 ) ) ;
#89110 = CARTESIAN_POINT ( 'NONE',  ( 1.472469842513823179, 10.59226448433411782, -4.923371831947296329 ) ) ;
#89111 = AXIS2_PLACEMENT_3D ( 'NONE', #67282, #23278, #59765 ) ;
#89112 = CARTESIAN_POINT ( 'NONE',  ( 18.52753015748617571, 8.092264484334117824, 4.923371831947298993 ) ) ;
#89113 = CARTESIAN_POINT ( 'NONE',  ( 22.81628187352648496, 6.831968003263753531, -3.434112377981050290 ) ) ;
#89114 = ADVANCED_FACE ( 'NONE', ( #71159 ), #32999, .T. ) ;
#89115 = CYLINDRICAL_SURFACE ( 'NONE', #45684, 62.50000000000000000 ) ;
#89116 = ORIENTED_EDGE ( 'NONE', *, *, #35308, .F. ) ;
#89117 = CARTESIAN_POINT ( 'NONE',  ( 7.084665262690076126, 12.02201867748817321, -10.88017736071110164 ) ) ;
#89118 = CARTESIAN_POINT ( 'NONE',  ( -2.266590686148945544, 6.387082168247300906, -7.082119434687050408 ) ) ;
#89119 = CARTESIAN_POINT ( 'NONE',  ( 12.63842701281683034, 27.46726448433411250, 9.846743663894596210 ) ) ;
#89120 = CARTESIAN_POINT ( 'NONE',  ( 7.084665262690076126, 57.02201867748817676, -10.88017736071110164 ) ) ;
#89122 = CARTESIAN_POINT ( 'NONE',  ( 0.000000000000000000, 0.000000000000000000, -4.000000000000000000 ) ) ;
#89121 = CARTESIAN_POINT ( 'NONE',  ( 6.565887622018943937, 25.16530133659708213, 12.81628187352647430 ) ) ;
#89123 = CARTESIAN_POINT ( 'NONE',  ( 17.96484262340118221, 4.938685344154837509, 7.964842623401181321 ) ) ;
#89124 = DIRECTION ( 'NONE',  ( 0.000000000000000000, 0.000000000000000000, -1.000000000000000000 ) ) ;
#89125 = CARTESIAN_POINT ( 'NONE',  ( -13.75801628063882909, 15.00000000000000000, 4.578972376164350599 ) ) ;
#89126 = CARTESIAN_POINT ( 'NONE',  ( 18.52753015748618282, 63.92559781766745886, -4.923371831947291888 ) ) ;
#89127 = CARTESIAN_POINT ( 'NONE',  ( 18.52753015748617571, 18.09226448433411960, 4.923371831947298993 ) ) ;
#89128 = B_SPLINE_CURVE_WITH_KNOTS ( 'NONE', 3,
 ( #28946, #82951, #58458, #58967 ),
 .UNSPECIFIED., .F., .F.,
 ( 4, 4 ),
 ( 0.000000000000000000, 0.002657014572711325923 ),
 .UNSPECIFIED. ) ;
#89129 = CARTESIAN_POINT ( 'NONE',  ( 10.88017736071109987, -29.22798132251182679, -2.915334737309928315 ) ) ;
#89130 = CARTESIAN_POINT ( 'NONE',  ( 16.40814093676323893, 25.79030133659708923, 11.09922568453595026 ) ) ;
#89131 = CARTESIAN_POINT ( 'NONE',  ( -11.48880622970674636, -88.23206844530574244, -3.750000000000000000 ) ) ;
#89132 = B_SPLINE_CURVE_WITH_KNOTS ( 'NONE', 3,
 ( #63579, #65043, #57068, #10108, #48084, #19077 ),
 .UNSPECIFIED., .F., .F.,
 ( 4, 2, 4 ),
 ( 0.0002800111042666545411, 0.0006862164423004639587, 0.001092421780334273214 ),
 .UNSPECIFIED. ) ;
#89134 = CARTESIAN_POINT ( 'NONE',  ( 14.88640444357869796, 14.76930270348881180, 1.277895705730344833 ) ) ;
#89133 = CARTESIAN_POINT ( 'NONE',  ( 15.44008868035555260, 44.73035201082151247, 9.422509992056143702 ) ) ;
#89135 = CARTESIAN_POINT ( 'NONE',  ( -3.750000000000000000, 36.75000000000000000, -2.750000000000000000 ) ) ;
#89136 = CARTESIAN_POINT ( 'NONE',  ( 20.36894250292379738, 54.92874883491396076, -10.36894250292379027 ) ) ;
#89137 = CARTESIAN_POINT ( 'NONE',  ( 1.780824192092392400, 14.63606913465075365, 14.89391369643518637 ) ) ;
#89138 = CARTESIAN_POINT ( 'NONE',  ( -0.8801773607111009756, 28.06368534415484106, 1.068504757029289695E-15 ) ) ;
#89139 = CARTESIAN_POINT ( 'NONE',  ( 17.20831665107776587, 49.13393115100078745, -7.208316651077762316 ) ) ;
#89140 = CARTESIAN_POINT ( 'NONE',  ( 0.5774900079438607392, 53.48035201082151247, 5.440088680355550821 ) ) ;
#89141 = CARTESIAN_POINT ( 'NONE',  ( 17.08211943468705130, 28.47041550158063572, 12.26659068614894998 ) ) ;
#89142 = DIRECTION ( 'NONE',  ( 0.000000000000000000, 1.000000000000000000, 0.000000000000000000 ) ) ;
#89143 = CARTESIAN_POINT ( 'NONE',  ( 19.84674366389459621, 43.50893115100078745, 7.409399052514197653E-17 ) ) ;
#89144 = CARTESIAN_POINT ( 'NONE',  ( 3.591859063236763294, -1.709698663402913210, -11.09922568453595026 ) ) ;
#89145 = EDGE_LOOP ( 'NONE', ( #32925, #95, #87808, #29073 ) ) ;
#89146 = CARTESIAN_POINT ( 'NONE',  ( -0.8801773607110991993, 27.85535201082150181, -2.915334737309923874 ) ) ;
#89147 = CARTESIAN_POINT ( 'NONE',  ( 20.24186590665275887, 7.616331881023276296, -6.114288769123074729 ) ) ;
#89148 = CARTESIAN_POINT ( 'NONE',  ( 4.559911319644449179, 17.23035201082150536, -9.422509992056141925 ) ) ;
#89149 = CARTESIAN_POINT ( 'NONE',  ( 17.20831665107776587, 4.133931151000785675, -7.208316651077762316 ) ) ;
#89150 = CARTESIAN_POINT ( 'NONE',  ( 17.08211943468705130, 23.47041550158063572, 12.26659068614894998 ) ) ;
#89151 = EDGE_CURVE ( 'NONE', #22386, #32242, #66092, .T. ) ;
#89152 = CARTESIAN_POINT ( 'NONE',  ( 19.84674366389459266, 18.71726448433411960, -2.638427012816827677 ) ) ;
#89153 = CARTESIAN_POINT ( 'NONE',  ( 19.84674366389459621, 58.50893115100078745, 7.409399052514197653E-17 ) ) ;
#89154 = CARTESIAN_POINT ( 'NONE',  ( -0.8801773607111009756, 28.06368534415484106, 1.068504757029289695E-15 ) ) ;
#89155 = CARTESIAN_POINT ( 'NONE',  ( 13.78891971893204271, 15.00000000000000000, 5.904717858191622426 ) ) ;
#89156 = DIRECTION ( 'NONE',  ( 0.000000000000000000, 1.000000000000000000, 0.000000000000000000 ) ) ;
#89157 = EDGE_CURVE ( 'NONE', #3713, #61040, #47410, .T. ) ;
#89158 = ORIENTED_EDGE ( 'NONE', *, *, #52734, .T. ) ;
#89159 = STYLED_ITEM ( 'NONE', ( #54013 ), #16060 ) ;
#89160 = CARTESIAN_POINT ( 'NONE',  ( 4.191187596055478082, -2.692365942001591517, 2.500000000000000000 ) ) ;
#89161 = CARTESIAN_POINT ( 'NONE',  ( 10.00000000000000000, 39.75893115100078745, -9.846743663894594434 ) ) ;
#89162 = ORIENTED_EDGE ( 'NONE', *, *, #66853, .T. ) ;
#89163 = ORIENTED_EDGE ( 'NONE', *, *, #60292, .T. ) ;
#89164 = LINE ( 'NONE', #13162, #62907 ) ;
#89165 = CARTESIAN_POINT ( 'NONE',  ( 2.917880565312948704, 27.63708216824730357, 12.26659068614894643 ) ) ;
#89166 = CARTESIAN_POINT ( 'NONE',  ( 20.36894250292379738, 14.92874883491396432, -10.36894250292379027 ) ) ;
#89167 = CARTESIAN_POINT ( 'NONE',  ( 17.96484262340118221, 56.18868534415484817, -7.964842623401177768 ) ) ;
#89168 = CARTESIAN_POINT ( 'NONE',  ( -0.3689425029237898834, 51.17874883491397497, -10.36894250292378850 ) ) ;
#89169 = CARTESIAN_POINT ( 'NONE',  ( 10.00000000000000000, 64.75893115100078035, -9.846743663894594434 ) ) ;
#89170 = CARTESIAN_POINT ( 'NONE',  ( 10.00000000000000000, 29.75893115100078745, -9.846743663894594434 ) ) ;
#89171 = CARTESIAN_POINT ( 'NONE',  ( -1.028725271592155099, -1.208271517246092823E-15, 4.540618777627624780 ) ) ;
#89173 = CARTESIAN_POINT ( 'NONE',  ( 22.81628187352648496, 6.831968003263753531, -3.434112377981050290 ) ) ;
#89172 = CARTESIAN_POINT ( 'NONE',  ( 15.44008868035555793, 31.39701867748817676, -9.422509992056140149 ) ) ;
#89174 = CARTESIAN_POINT ( 'NONE',  ( -4.164238869374098151, 21.59541550158063217, -3.795296366450310543 ) ) ;
#89175 = CARTESIAN_POINT ( 'NONE',  ( -0.8801773607111008646, 23.27201867748817676, 2.915334737309923430 ) ) ;
#89176 = DIRECTION ( 'NONE',  ( 0.000000000000000000, 1.000000000000000000, 0.000000000000000000 ) ) ;
#89177 = CARTESIAN_POINT ( 'NONE',  ( -12.98685442714190508, 15.00000000000000000, -6.449155920601135072 ) ) ;
#89178 = CARTESIAN_POINT ( 'NONE',  ( 15.44008868035555260, 44.73035201082151247, 9.422509992056143702 ) ) ;
#89179 = COLOUR_RGB ( '', 0.09019608, 0.27058824, 0.51372549) ;
#89180 = CARTESIAN_POINT ( 'NONE',  ( 8.879999999999991900, 69.99999999999998579, -6.250000000000000000 ) ) ;
#89181 = ORIENTED_EDGE ( 'NONE', *, *, #77642, .F. ) ;
#89182 = CARTESIAN_POINT ( 'NONE',  ( 13.07751017357379730, 4.171195230237741069E-16, 6.263284095430596388 ) ) ;
#89183 = VERTEX_POINT ( 'NONE', #81103 ) ;
#89184 = ORIENTED_EDGE ( 'NONE', *, *, #98249, .T. ) ;
#89185 = CARTESIAN_POINT ( 'NONE',  ( -0.3689425029237898834, 51.17874883491397497, -10.36894250292378850 ) ) ;
#89186 = CARTESIAN_POINT ( 'NONE',  ( 19.84674366389459266, 53.71726448433411605, -2.638427012816827677 ) ) ;
#89187 = CARTESIAN_POINT ( 'NONE',  ( 17.96484262340118221, 59.93868534415484106, 7.964842623401181321 ) ) ;
#89188 = VECTOR ( 'NONE', #25630, 1000.000000000000114 ) ;
#89189 = DIRECTION ( 'NONE',  ( -0.000000000000000000, 0.000000000000000000, 1.000000000000000000 ) ) ;
#89190 = CIRCLE ( 'NONE', #70005, 0.5000000000000004441 ) ;
#89191 = CARTESIAN_POINT ( 'NONE',  ( -0.8801773607111009756, 53.06368534415484106, 1.068504757029289695E-15 ) ) ;
#89192 = EDGE_CURVE ( 'NONE', #47751, #18983, #4330, .T. ) ;
#89193 = CARTESIAN_POINT ( 'NONE',  ( 10.00000000000000000, 57.87363466993042493, -12.81628187352647608 ) ) ;
#89194 = CARTESIAN_POINT ( 'NONE',  ( -11.09922568453594316, 9.540301336597091009, 6.408140936763246920 ) ) ;
#89195 = EDGE_CURVE ( 'NONE', #77740, #73794, #89100, .T. ) ;
#89196 = ORIENTED_EDGE ( 'NONE', *, *, #60187, .T. ) ;
#89197 = CARTESIAN_POINT ( 'NONE',  ( 17.08211943468705840, 25.13708216824730357, -12.26659068614894466 ) ) ;
#89198 = CARTESIAN_POINT ( 'NONE',  ( 10.00000000000000000, 17.87363466993041783, -12.81628187352647608 ) ) ;
#89199 = VERTEX_POINT ( 'NONE', #20613 ) ;
#89200 = CARTESIAN_POINT ( 'NONE',  ( 22.81628187352647785, 41.41530133659708923, 3.434112377981063169 ) ) ;
#89201 = CARTESIAN_POINT ( 'NONE',  ( -0.8801773607111008646, 18.27201867748817321, 2.915334737309923430 ) ) ;
#89202 = CARTESIAN_POINT ( 'NONE',  ( 12.63842701281683922, 34.55059781766745886, -9.846743663894590881 ) ) ;
#89203 = CARTESIAN_POINT ( 'NONE',  ( 7.084665262690076126, 14.10535201082150358, 10.88017736071109987 ) ) ;
#89204 = CARTESIAN_POINT ( 'NONE',  ( 0.6178305044545818747, 58.49863466993042493, -9.382169495545419124 ) ) ;
#89205 = CARTESIAN_POINT ( 'NONE',  ( -0.1503990784575328643, 70.00000000000000000, 6.262539305110068177 ) ) ;
#89206 = CARTESIAN_POINT ( 'NONE',  ( 7.361572987183170547, 37.05059781766744464, 9.846743663894590881 ) ) ;
#89208 = ORIENTED_EDGE ( 'NONE', *, *, #27761, .T. ) ;
#89207 = CARTESIAN_POINT ( 'NONE',  ( -19.96637108136584260, 47.61387035396268885, -3.000000000000000000 ) ) ;
#89209 = LINE ( 'NONE', #36210, #66860 ) ;
#89210 = CARTESIAN_POINT ( 'NONE',  ( 1.707155281725185381, 32.90189080397284016, 6.499999999999955591 ) ) ;
#89211 = DIRECTION ( 'NONE',  ( -1.000000000000000000, 0.000000000000000000, 0.000000000000000000 ) ) ;
#89212 = EDGE_CURVE ( 'NONE', #33986, #1529, #83599, .T. ) ;
#89213 = CARTESIAN_POINT ( 'NONE',  ( 1.780824192092484326, 14.49999999999999112, -14.89391369643520058 ) ) ;
#89214 = CARTESIAN_POINT ( 'NONE',  ( 0.1532563361054082862, 16.21726448433411960, 2.638427012816831674 ) ) ;
#89215 = CARTESIAN_POINT ( 'NONE',  ( 10.00000000000000000, 17.87363466993041783, -12.81628187352647608 ) ) ;
#89216 = FACE_OUTER_BOUND ( 'NONE', #11017, .T. ) ;
#89217 = B_SPLINE_CURVE_WITH_KNOTS ( 'NONE', 3,
 ( #1314, #76295, #61282, #44795, #37328, #23312 ),
 .UNSPECIFIED., .F., .F.,
 ( 4, 2, 4 ),
 ( 3.409110551479961170E-05, 0.0004400426677366258386, 0.0008459942299584519978 ),
 .UNSPECIFIED. ) ;
#89218 = ADVANCED_FACE ( 'NONE', ( #35099 ), #88108, .F. ) ;
#89219 = ORIENTED_EDGE ( 'NONE', *, *, #49726, .F. ) ;
#89220 = STYLED_ITEM ( 'NONE', ( #15147 ), #3431 ) ;
#89221 = CARTESIAN_POINT ( 'NONE',  ( 0.1532563361054082862, 51.21726448433412315, 2.638427012816831674 ) ) ;
#89222 = CARTESIAN_POINT ( 'NONE',  ( -10.84451454130513426, 4.265732461173792237E-16, 9.625305416630759225 ) ) ;
#89223 = CARTESIAN_POINT ( 'NONE',  ( -0.3689425029237881626, 17.42874883491397142, 10.36894250292379027 ) ) ;
#89224 = CARTESIAN_POINT ( 'NONE',  ( 1.472469842513823179, 41.42559781766745886, 4.923371831947296329 ) ) ;
#89225 = CARTESIAN_POINT ( 'NONE',  ( 6.565887622018943937, 48.08196800326375353, -12.81628187352647608 ) ) ;
#89226 = DIRECTION ( 'NONE',  ( 0.000000000000000000, -0.000000000000000000, 1.000000000000000000 ) ) ;
#89227 = CARTESIAN_POINT ( 'NONE',  ( -0.8801773607110991993, 57.85535201082149825, -2.915334737309923874 ) ) ;
#89228 = CARTESIAN_POINT ( 'NONE',  ( -10.70613742633244669, 4.850979303660538556E-16, -9.778988772285387654 ) ) ;
#89229 = CARTESIAN_POINT ( 'NONE',  ( 7.361572987183169658, 39.96726448433411605, -9.846743663894592657 ) ) ;
#89230 = CARTESIAN_POINT ( 'NONE',  ( 4.559911319644449179, 38.89701867748817676, 9.422509992056141925 ) ) ;
#89231 = CARTESIAN_POINT ( 'NONE',  ( 13.43411237798105340, 45.58196800326374643, 12.81628187352647963 ) ) ;
#89232 = CARTESIAN_POINT ( 'NONE',  ( 0.1532563361054082862, 31.21726448433412315, 2.638427012816831674 ) ) ;
#89233 = DIRECTION ( 'NONE',  ( 1.000000000000000000, 0.000000000000000000, 0.000000000000000000 ) ) ;
#89234 = DIRECTION ( 'NONE',  ( -0.000000000000000000, 1.000000000000000000, -0.000000000000000000 ) ) ;
#89235 = CARTESIAN_POINT ( 'NONE',  ( 12.91533473730992121, 44.52201867748816966, 10.88017736071110164 ) ) ;
#89236 = B_SPLINE_CURVE_WITH_KNOTS ( 'NONE', 3,
 ( #26652, #19650, #57148, #35130, #52123, #82617 ),
 .UNSPECIFIED., .F., .F.,
 ( 4, 2, 4 ),
 ( 3.409110551496096132E-05, 0.0004400426677367866800, 0.0008459942299586124597 ),
 .UNSPECIFIED. ) ;
#89237 = VERTEX_POINT ( 'NONE', #4140 ) ;
#89238 = CARTESIAN_POINT ( 'NONE',  ( -9.742785792574940373, 4.701366962315984388, -5.624999999999991118 ) ) ;
#89239 = CARTESIAN_POINT ( 'NONE',  ( 4.559911319644449179, 12.23035201082150536, -9.422509992056141925 ) ) ;
#89241 = CARTESIAN_POINT ( 'NONE',  ( -0.8801773607111009756, 43.06368534415484106, 1.068504757029289695E-15 ) ) ;
#89240 = CARTESIAN_POINT ( 'NONE',  ( 5.076628168052703671, 51.84226448433412315, 8.527530157486179263 ) ) ;
#89242 = LINE ( 'NONE', #13241, #77572 ) ;
#89243 = CARTESIAN_POINT ( 'NONE',  ( 0.5774900079438607392, 63.48035201082149825, 5.440088680355550821 ) ) ;
#89245 = FACE_OUTER_BOUND ( 'NONE', #58202, .T. ) ;
#89244 = CARTESIAN_POINT ( 'NONE',  ( 4.559911319644449179, 32.23035201082150536, -9.422509992056141925 ) ) ;
#89246 = CARTESIAN_POINT ( 'NONE',  ( 2.791683348922237240, 25.38393115100078390, -7.208316651077763204 ) ) ;
#89247 = CARTESIAN_POINT ( 'NONE',  ( 12.99999999999999822, 75.00000000000000000, -8.525133428036872019 ) ) ;
#89248 = CARTESIAN_POINT ( 'NONE',  ( 3.795296366450306547, 0.3454155015806399942, -14.16423886937410259 ) ) ;
#89249 = CARTESIAN_POINT ( 'NONE',  ( 2.791683348922237240, 55.38393115100078745, -7.208316651077763204 ) ) ;
#89250 = CARTESIAN_POINT ( 'NONE',  ( 13.79529636645031943, 50.34541550158064638, -14.16423886937409904 ) ) ;
#89251 = CARTESIAN_POINT ( 'NONE',  ( 12.79448242979001371, 0.2306972965111889762, 7.716169648622186905 ) ) ;
#89253 = CARTESIAN_POINT ( 'NONE',  ( 22.26659068614894466, 3.887082168247300906, 7.082119434687054849 ) ) ;
#89252 =( GEOMETRIC_REPRESENTATION_CONTEXT ( 3 ) GLOBAL_UNCERTAINTY_ASSIGNED_CONTEXT ( ( #12296 ) ) GLOBAL_UNIT_ASSIGNED_CONTEXT ( ( #72569, #51064, #5587 ) ) REPRESENTATION_CONTEXT ( 'NONE', 'WORKASPACE' ) );
#89254 = CIRCLE ( 'NONE', #76491, 15.00000000000000000 ) ;
#89255 = CARTESIAN_POINT ( 'NONE',  ( 13.79529636645031943, 35.34541550158063927, -14.16423886937409904 ) ) ;
#89256 = CARTESIAN_POINT ( 'NONE',  ( 3.591859063236761518, -0.04303199673624671928, 11.09922568453594849 ) ) ;
#89257 = ORIENTED_EDGE ( 'NONE', *, *, #15294, .T. ) ;
#89258 = CARTESIAN_POINT ( 'NONE',  ( 20.88017736071110519, 20.56368534415484106, 2.639326808657452039E-16 ) ) ;
#89259 = CARTESIAN_POINT ( 'NONE',  ( 17.20831665107776587, 52.88393115100078035, 7.208316651077764980 ) ) ;
#89261 = DIRECTION ( 'NONE',  ( -0.000000000000000000, -1.000000000000000000, -0.000000000000000000 ) ) ;
#89260 = CARTESIAN_POINT ( 'NONE',  ( 2.831191079880678085, 79.91181047996344944, -9.500000000000000000 ) ) ;
#89262 = DIRECTION ( 'NONE',  ( -2.569960705150826877E-16, 1.000000000000000000, -0.000000000000000000 ) ) ;
#89263 = SURFACE_STYLE_FILL_AREA ( #45243 ) ;
#89264 = CARTESIAN_POINT ( 'NONE',  ( 10.00000000000000000, 27.87363466993042138, -12.81628187352647608 ) ) ;
#89265 = CARTESIAN_POINT ( 'NONE',  ( 10.00000000000000178, 22.25893115100078745, 9.846743663894594434 ) ) ;
#89266 = VERTEX_POINT ( 'NONE', #66600 ) ;
#89267 = CARTESIAN_POINT ( 'NONE',  ( 19.84674366389459621, 3.508931151000785231, 7.409399052514197653E-17 ) ) ;
#89268 = CARTESIAN_POINT ( 'NONE',  ( -12.79448242978996220, 0.2306972965111912799, -7.716169648622273947 ) ) ;
#89269 = DIRECTION ( 'NONE',  ( -0.000000000000000000, -1.000000000000000000, -0.000000000000000000 ) ) ;
#89270 = CARTESIAN_POINT ( 'NONE',  ( 12.91533473730992121, 9.522018677488171434, 10.88017736071110164 ) ) ;
#89271 = CARTESIAN_POINT ( 'NONE',  ( -4.164238869374098151, 36.59541550158063217, -3.795296366450310543 ) ) ;
#89272 = CARTESIAN_POINT ( 'NONE',  ( 2.035157376598822676, 47.43868534415484817, -7.964842623401177768 ) ) ;
#89273 = CARTESIAN_POINT ( 'NONE',  ( 10.00000000000000000, 61.81368534415484106, -10.88017736071110342 ) ) ;
#89274 = CARTESIAN_POINT ( 'NONE',  ( -0.7577696756369834974, 14.76984978199062581, -14.92139465029885237 ) ) ;
#89275 = CARTESIAN_POINT ( 'NONE',  ( 19.72487221294570858, 16.86607318730074567, 6.500000000000000888 ) ) ;
#89276 = CARTESIAN_POINT ( 'NONE',  ( 17.20831665107776587, 24.13393115100078035, -7.208316651077762316 ) ) ;
#89277 = DIRECTION ( 'NONE',  ( 0.000000000000000000, -1.000000000000000000, -0.000000000000000000 ) ) ;
#89278 = CARTESIAN_POINT ( 'NONE',  ( 14.92337183194729988, 9.342264484334119601, -8.527530157486177487 ) ) ;
#89279 =( BOUNDED_CURVE ( )  B_SPLINE_CURVE ( 2, ( #58084, #68570, #29069, #37584, #90563, #74576, #75073, #84062, #46063 ),
 .UNSPECIFIED., .F., .F. ) 
 B_SPLINE_CURVE_WITH_KNOTS ( ( 3, 2, 2, 2, 3 ),
 ( 0.2258552226545170460, 0.2261904761904761640, 0.2321428571428572063, 0.2380952380952381375, 0.2384304916311972555 ),
 .UNSPECIFIED. ) 
 CURVE ( )  GEOMETRIC_REPRESENTATION_ITEM ( )  RATIONAL_B_SPLINE_CURVE ( ( 0.9963778908391762723, 0.9980808541467921513, 1.000000000000000000, 0.9659258262890682012, 1.000000000000000000, 0.9659258262890682012, 1.000000000000000000, 0.9980808541467921513, 0.9963778908391762723 ) ) 
 REPRESENTATION_ITEM ( '' )  );
#89280 = CARTESIAN_POINT ( 'NONE',  ( 5.817157072110704874, 15.00000000000000000, 13.82608706751090821 ) ) ;
#89281 = CARTESIAN_POINT ( 'NONE',  ( 12.63842701281683922, 34.55059781766745886, -9.846743663894590881 ) ) ;
#89282 = CARTESIAN_POINT ( 'NONE',  ( 18.52753015748618282, 58.92559781766745886, -4.923371831947291888 ) ) ;
#89283 = EDGE_CURVE ( 'NONE', #15070, #26787, #29849, .T. ) ;
#89284 = CARTESIAN_POINT ( 'NONE',  ( 7.084665262690076126, 37.02201867748817676, -10.88017736071110164 ) ) ;
#89285 = UNCERTAINTY_MEASURE_WITH_UNIT (LENGTH_MEASURE( 1.000000000000000082E-05 ), #10368, 'distance_accuracy_value', 'NONE');
#89286 = ORIENTED_EDGE ( 'NONE', *, *, #20028, .F. ) ;
#89287 = CARTESIAN_POINT ( 'NONE',  ( 22.81628187352647785, 61.41530133659709634, 3.434112377981063169 ) ) ;
#89288 = CARTESIAN_POINT ( 'NONE',  ( 2.062412797813223616E-17, 1.639999999999999014, 0.000000000000000000 ) ) ;
#89289 = CARTESIAN_POINT ( 'NONE',  ( 0.1532563361054082862, 1.217264484334117824, 2.638427012816831674 ) ) ;
#89290 = CARTESIAN_POINT ( 'NONE',  ( 3.591859063236761518, 39.95696800326375353, 11.09922568453594849 ) ) ;
#89292 = CARTESIAN_POINT ( 'NONE',  ( 0.1532563361054100626, 40.80059781766745886, -2.638427012816831230 ) ) ;
#89291 = CARTESIAN_POINT ( 'NONE',  ( 17.08211943468705840, 65.13708216824730357, -12.26659068614894466 ) ) ;
#89293 = CARTESIAN_POINT ( 'NONE',  ( 0.2751277870542909731, 47.28217586085238366, -6.499999999999992006 ) ) ;
#89294 = CARTESIAN_POINT ( 'NONE',  ( 1.472469842513823179, 1.425597817667451528, 4.923371831947296329 ) ) ;
#89295 = CARTESIAN_POINT ( 'NONE',  ( -0.3689425029237898834, 21.17874883491396432, -10.36894250292378850 ) ) ;
#89296 = CARTESIAN_POINT ( 'NONE',  ( 20.36894250292379382, 48.67874883491396076, 10.36894250292379205 ) ) ;
#89297 = CARTESIAN_POINT ( 'NONE',  ( 17.20831665107776587, 37.88393115100078745, 7.208316651077764980 ) ) ;
#89298 = FACE_OUTER_BOUND ( 'NONE', #59903, .T. ) ;
#89299 = CARTESIAN_POINT ( 'NONE',  ( 19.42250999205614193, 40.14701867748817676, 5.440088680355555262 ) ) ;
#89300 = CARTESIAN_POINT ( 'NONE',  ( 19.42250999205614193, 55.14701867748817676, 5.440088680355555262 ) ) ;
#89301 = VECTOR ( 'NONE', #61929, 1000.000000000000000 ) ;
#89302 = FILL_AREA_STYLE_COLOUR ( '', #11023 ) ;
#89303 = ORIENTED_EDGE ( 'NONE', *, *, #72914, .F. ) ;
#89304 = CARTESIAN_POINT ( 'NONE',  ( 21.09922568453594849, 46.20696800326376064, 6.408140936763242479 ) ) ;
#89305 = VERTEX_POINT ( 'NONE', #5119 ) ;
#89306 = CARTESIAN_POINT ( 'NONE',  ( 7.361572987183169658, -0.03273551566588185635, -9.846743663894592657 ) ) ;
#89307 = VERTEX_POINT ( 'NONE', #19128 ) ;
#89308 = CARTESIAN_POINT ( 'NONE',  ( 13.79529636645030344, 8.262082168247300018, 14.16423886937410614 ) ) ;
#89309 = CARTESIAN_POINT ( 'NONE',  ( 5.076628168052704559, 5.175597817667451750, -8.527530157486179263 ) ) ;
#89310 = DIRECTION ( 'NONE',  ( 0.000000000000000000, 1.000000000000000000, 0.000000000000000000 ) ) ;
#89311 = ORIENTED_EDGE ( 'NONE', *, *, #72450, .F. ) ;
#89312 = CARTESIAN_POINT ( 'NONE',  ( 2.035157376598824452, 18.68868534415484106, 7.964842623401179544 ) ) ;
#89313 = EDGE_CURVE ( 'NONE', #18983, #24454, #9762, .T. ) ;
#89314 = CARTESIAN_POINT ( 'NONE',  ( 11.81378540890936080, -0.03417435944610275333, -7.968498874458115999 ) ) ;
#89315 = CARTESIAN_POINT ( 'NONE',  ( 2.917880565312948704, 12.63708216824730179, 12.26659068614894643 ) ) ;
#89316 = ADVANCED_FACE ( 'NONE', ( #95113 ), #68205, .T. ) ;
#89317 = EDGE_LOOP ( 'NONE', ( #31769, #11117, #76672, #47022 ) ) ;
#89318 = CARTESIAN_POINT ( 'NONE',  ( 19.42250999205614548, 20.98035201082150891, -5.440088680355545492 ) ) ;
#89319 = CARTESIAN_POINT ( 'NONE',  ( 17.20831665107776587, 62.88393115100078745, 7.208316651077764980 ) ) ;
#89320 = EDGE_LOOP ( 'NONE', ( #605, #89742, #3698, #84242 ) ) ;
#89321 = CARTESIAN_POINT ( 'NONE',  ( 18.52753015748618282, 58.92559781766745886, -4.923371831947291888 ) ) ;
#89322 = VERTEX_POINT ( 'NONE', #49607 ) ;
#89323 = CARTESIAN_POINT ( 'NONE',  ( 2.035157376598824452, 63.68868534415484106, 7.964842623401179544 ) ) ;
#89324 = CARTESIAN_POINT ( 'NONE',  ( 2.361121941889117171, 14.76984946027100420, -14.75287579053849463 ) ) ;
#89326 = CARTESIAN_POINT ( 'NONE',  ( -13.75503023589401863, 14.95077488074853811, -5.333408231410926348 ) ) ;
#89325 = CARTESIAN_POINT ( 'NONE',  ( -0.8801773607110991993, 12.85535201082150358, -2.915334737309923874 ) ) ;
#89327 = CARTESIAN_POINT ( 'NONE',  ( 18.52753015748617571, 8.092264484334117824, 4.923371831947298993 ) ) ;
#89328 = CARTESIAN_POINT ( 'NONE',  ( 4.559911319644449179, 13.89701867748817321, 9.422509992056141925 ) ) ;
#89329 = B_SPLINE_CURVE_WITH_KNOTS ( 'NONE', 3,
 ( #97451, #6421, #12939, #74417, #28916, #43433 ),
 .UNSPECIFIED., .F., .F.,
 ( 4, 2, 4 ),
 ( 0.0002800065468392932098, 0.0006862118402932773902, 0.001092417133747261571 ),
 .UNSPECIFIED. ) ;
#89330 = EDGE_LOOP ( 'NONE', ( #27088, #69077, #83202, #64315 ) ) ;
#89331 = CARTESIAN_POINT ( 'NONE',  ( 4.559911319644449179, 47.23035201082150536, -9.422509992056141925 ) ) ;
#89332 = CARTESIAN_POINT ( 'NONE',  ( 19.54819611545892144, 96.99629728834725029, 4.999999999999999112 ) ) ;
#89333 = CARTESIAN_POINT ( 'NONE',  ( 3.591859063236763294, 43.29030133659708923, -11.09922568453595026 ) ) ;
#89334 = CARTESIAN_POINT ( 'NONE',  ( 7.084665262690076126, 42.02201867748816966, -10.88017736071110164 ) ) ;
#89335 = CARTESIAN_POINT ( 'NONE',  ( 5.076628168052704559, 60.17559781766745175, -8.527530157486179263 ) ) ;
#89336 = EDGE_LOOP ( 'NONE', ( #34363, #73822, #77036, #43187 ) ) ;
#89337 = TOROIDAL_SURFACE ( 'NONE', #51083, 14.49999999999999822, 0.5000000000000000000 ) ;
#89338 = CARTESIAN_POINT ( 'NONE',  ( 2.791683348922240793, 11.63393115100078568, 7.208316651077764092 ) ) ;
#89339 = CARTESIAN_POINT ( 'NONE',  ( -1.099225684535947600, 4.540301336597087456, 6.408140936763237150 ) ) ;
#89341 = CARTESIAN_POINT ( 'NONE',  ( 2.791683348922237240, 60.38393115100078745, -7.208316651077763204 ) ) ;
#89340 = CARTESIAN_POINT ( 'NONE',  ( -13.77612262535527954, 90.93158326518027934, -7.883772450803742338 ) ) ;
#89342 = CARTESIAN_POINT ( 'NONE',  ( 2.035157376598824452, 23.68868534415484461, 7.964842623401179544 ) ) ;
#89343 = CARTESIAN_POINT ( 'NONE',  ( 10.00000000000000178, 47.25893115100078745, 9.846743663894594434 ) ) ;
#89344 = CARTESIAN_POINT ( 'NONE',  ( -10.39692778084947022, 14.95037106203290733, 10.46714871971192018 ) ) ;
#89345 = EDGE_CURVE ( 'NONE', #15452, #14809, #34701, .T. ) ;
#89346 = AXIS2_PLACEMENT_3D ( 'NONE', #70982, #63461, #86475 ) ;
#89347 = CARTESIAN_POINT ( 'NONE',  ( 5.076628168052703671, 11.84226448433411960, 8.527530157486179263 ) ) ;
#89348 = DIRECTION ( 'NONE',  ( 0.9025852843498648470, 0.000000000000000000, -0.4305110968082862533 ) ) ;
#89350 = ORIENTED_EDGE ( 'NONE', *, *, #58920, .F. ) ;
#89349 = CARTESIAN_POINT ( 'NONE',  ( 0.6178305044545818747, -1.501365330069579951, -9.382169495545419124 ) ) ;
#89351 =( LENGTH_UNIT ( ) NAMED_UNIT ( * ) SI_UNIT ( .MILLI., .METRE. ) );
#89352 = CARTESIAN_POINT ( 'NONE',  ( 10.00000000000000178, 40.37363466993042493, 12.81628187352647608 ) ) ;
#89353 = CARTESIAN_POINT ( 'NONE',  ( 0.1532563361054083140, 36.00893115100078745, 1.131784320476157264E-15 ) ) ;
#89354 = CARTESIAN_POINT ( 'NONE',  ( -4.838527690343713772, 0.5000000000000004441, 14.19819177887723605 ) ) ;
#89355 = CARTESIAN_POINT ( 'NONE',  ( 22.26659068614895176, 54.72041550158063217, -7.082119434687042414 ) ) ;
#89356 = CARTESIAN_POINT ( 'NONE',  ( 0.1532563361054082862, 26.21726448433411605, 2.638427012816831674 ) ) ;
#89357 = CARTESIAN_POINT ( 'NONE',  ( 0.000000000000000000, 15.00000000000000000, 0.000000000000000000 ) ) ;
#89358 = CARTESIAN_POINT ( 'NONE',  ( 0.5774900079438607392, 8.480352010821505360, 5.440088680355550821 ) ) ;
#89359 = CARTESIAN_POINT ( 'NONE',  ( -11.80960303780298482, 90.32667112043513669, -7.004222671090198027 ) ) ;
#89360 = CARTESIAN_POINT ( 'NONE',  ( 17.96484262340118221, 14.93868534415484106, 7.964842623401181321 ) ) ;
#89361 = CARTESIAN_POINT ( 'NONE',  ( -0.3689425029237881626, 47.42874883491396787, 10.36894250292379027 ) ) ;
#89363 = DIRECTION ( 'NONE',  ( 0.000000000000000000, 0.000000000000000000, 1.000000000000000000 ) ) ;
#89362 = CARTESIAN_POINT ( 'NONE',  ( -4.164238869374099927, 47.01208216824729647, 3.795296366450308767 ) ) ;
#89364 = CARTESIAN_POINT ( 'NONE',  ( 0.000000000000000000, 15.00000000000000000, 0.000000000000000000 ) ) ;
#89365 = CARTESIAN_POINT ( 'NONE',  ( 14.92337183194729988, 14.34226448433411782, -8.527530157486177487 ) ) ;
#89366 = CARTESIAN_POINT ( 'NONE',  ( 10.00000000000000000, 64.75893115100078035, -9.846743663894594434 ) ) ;
#89367 = ORIENTED_EDGE ( 'NONE', *, *, #47800, .F. ) ;
#89368 = CARTESIAN_POINT ( 'NONE',  ( 19.42250999205614193, 50.14701867748817676, 5.440088680355555262 ) ) ;
#89369 = CARTESIAN_POINT ( 'NONE',  ( 0.5774900079438590739, 17.64701867748817321, -5.440088680355550821 ) ) ;
#89370 = CARTESIAN_POINT ( 'NONE',  ( 10.00000000000000000, 54.75893115100078745, -9.846743663894594434 ) ) ;
#89371 = DIRECTION ( 'NONE',  ( -0.000000000000000000, -1.000000000000000000, -0.000000000000000000 ) ) ;
#89372 = CARTESIAN_POINT ( 'NONE',  ( 17.20831665107776587, 62.88393115100078745, 7.208316651077764980 ) ) ;
#89373 = CARTESIAN_POINT ( 'NONE',  ( 20.36894250292379382, 3.678748834913967869, 10.36894250292379205 ) ) ;
#89374 = CARTESIAN_POINT ( 'NONE',  ( 10.00000000000000178, 32.25893115100078745, 9.846743663894594434 ) ) ;
#89375 = FACE_OUTER_BOUND ( 'NONE', #44375, .T. ) ;
#89376 = ORIENTED_EDGE ( 'NONE', *, *, #14001, .T. ) ;
#89377 = CARTESIAN_POINT ( 'NONE',  ( 13.79529636645030344, 43.26208216824730357, 14.16423886937410614 ) ) ;
#89378 = CARTESIAN_POINT ( 'NONE',  ( 10.00000000000000000, -0.2410688489992152128, -9.846743663894594434 ) ) ;
#89380 = CARTESIAN_POINT ( 'NONE',  ( 10.00000000000000178, 70.00000000000000000, 0.000000000000000000 ) ) ;
#89379 = CARTESIAN_POINT ( 'NONE',  ( -7.116252256160142231, -80.68108970088715637, -2.749999999999193978 ) ) ;
#89381 = CARTESIAN_POINT ( 'NONE',  ( 17.96484262340118221, 29.93868534415484106, 7.964842623401181321 ) ) ;
#89382 = CARTESIAN_POINT ( 'NONE',  ( 19.38216949554541202, 40.99863466993042493, 9.382169495545424454 ) ) ;
#89383 = CARTESIAN_POINT ( 'NONE',  ( 15.44008868035555793, 6.397018677488170546, -9.422509992056140149 ) ) ;
#89384 = CARTESIAN_POINT ( 'NONE',  ( 0.6178305044545818747, 38.49863466993042493, -9.382169495545419124 ) ) ;
#89385 = CARTESIAN_POINT ( 'NONE',  ( 6.565887622018943937, 58.08196800326376064, -12.81628187352647608 ) ) ;
#89386 = EDGE_LOOP ( 'NONE', ( #77862, #45869, #48943, #49782 ) ) ;
#89387 = DIRECTION ( 'NONE',  ( 0.000000000000000000, 1.000000000000000000, -0.000000000000000000 ) ) ;
#89388 = CARTESIAN_POINT ( 'NONE',  ( -11.26386101273689988, -65.37750071423508302, -4.000000000000000888 ) ) ;
#89389 = CARTESIAN_POINT ( 'NONE',  ( 20.36894250292379738, 29.92874883491396432, -10.36894250292379027 ) ) ;
#89390 = CARTESIAN_POINT ( 'NONE',  ( 0.5774900079438607392, 18.48035201082150536, 5.440088680355550821 ) ) ;
#89391 = DIRECTION ( 'NONE',  ( -0.5547001962252291474, -0.8320502943378437211, -0.000000000000000000 ) ) ;
#89392 = DIRECTION ( 'NONE',  ( -1.000000000000000000, 0.000000000000000000, 0.000000000000000000 ) ) ;
#89393 = CARTESIAN_POINT ( 'NONE',  ( -0.8801773607111009756, 48.06368534415484817, 1.068504757029289695E-15 ) ) ;
#89394 = CARTESIAN_POINT ( 'NONE',  ( 12.91533473730993009, 51.60535201082149825, -10.88017736071109987 ) ) ;
#89395 = CARTESIAN_POINT ( 'NONE',  ( 21.09922568453595559, 7.040301336597086568, -6.408140936763230044 ) ) ;
#89396 =( NAMED_UNIT ( * ) SI_UNIT ( $, .STERADIAN. ) SOLID_ANGLE_UNIT ( ) );
#89397 = CARTESIAN_POINT ( 'NONE',  ( 2.603489959281588106, 1.582109641433292690, 6.500000000000000888 ) ) ;
#89398 = CARTESIAN_POINT ( 'NONE',  ( 14.92337183194729633, 22.67559781766745175, 8.527530157486181039 ) ) ;
#89399 = CARTESIAN_POINT ( 'NONE',  ( 12.91533473730993009, 41.60535201082149825, -10.88017736071109987 ) ) ;
#89400 = EDGE_CURVE ( 'NONE', #92653, #72857, #90572, .T. ) ;
#89401 = CARTESIAN_POINT ( 'NONE',  ( 6.565887622018943937, 10.16530133659708746, 12.81628187352647430 ) ) ;
#89402 = CARTESIAN_POINT ( 'NONE',  ( 10.00000000000000000, -0.2410688489992152128, -9.846743663894594434 ) ) ;
#89403 = CARTESIAN_POINT ( 'NONE',  ( 7.361572987183169658, 29.96726448433411960, -9.846743663894592657 ) ) ;
#89404 = CARTESIAN_POINT ( 'NONE',  ( 6.565887622018943937, 55.16530133659709634, 12.81628187352647430 ) ) ;
#89405 = CARTESIAN_POINT ( 'NONE',  ( 18.52753015748617571, 23.09226448433411960, 4.923371831947298993 ) ) ;
#89406 = VERTEX_POINT ( 'NONE', #76562 ) ;
#89407 = CARTESIAN_POINT ( 'NONE',  ( 20.36894250292379738, 4.928748834913967869, -10.36894250292379027 ) ) ;
#89408 = DIRECTION ( 'NONE',  ( 1.000000000000000000, 0.000000000000000000, 0.000000000000000000 ) ) ;
#89409 = CARTESIAN_POINT ( 'NONE',  ( 15.44008868035555260, 19.73035201082150536, 9.422509992056143702 ) ) ;
#89411 = CARTESIAN_POINT ( 'NONE',  ( -4.164238869374099039, 36.80374883491396787, 8.674139862899312516E-16 ) ) ;
#89410 = CARTESIAN_POINT ( 'NONE',  ( 10.00000000000000000, 1.813685344154837731, -10.88017736071110342 ) ) ;
#89412 = CARTESIAN_POINT ( 'NONE',  ( 14.92337183194729988, 34.34226448433411605, -8.527530157486177487 ) ) ;
#89413 = CIRCLE ( 'NONE', #8064, 15.00000000000000000 ) ;
#89414 = CARTESIAN_POINT ( 'NONE',  ( 7.084665262690076126, 22.02201867748817321, -10.88017736071110164 ) ) ;
#89415 = CARTESIAN_POINT ( 'NONE',  ( -0.8801773607111008646, 18.27201867748817321, 2.915334737309923430 ) ) ;
#89416 = ORIENTED_EDGE ( 'NONE', *, *, #35734, .T. ) ;
#89417 = CIRCLE ( 'NONE', #94193, 15.00000000000000000 ) ;
#89418 = CARTESIAN_POINT ( 'NONE',  ( 20.88017736071110164, 20.35535201082150891, 2.915334737309930979 ) ) ;
#89419 = AXIS2_PLACEMENT_3D ( 'NONE', #14914, #7414, #30375 ) ;
#89420 = CARTESIAN_POINT ( 'NONE',  ( -2.816281873526473856, 44.12363466993042493, 9.499525473075851096E-16 ) ) ;
#89421 = CARTESIAN_POINT ( 'NONE',  ( 10.00000000000000178, 39.31368534415484106, 10.88017736071110342 ) ) ;
#89423 = CARTESIAN_POINT ( 'NONE',  ( 7.084665262690076126, 42.02201867748816966, -10.88017736071110164 ) ) ;
#89422 = PLANE ( 'NONE',  #52068 ) ;
#89424 = ORIENTED_EDGE ( 'NONE', *, *, #51385, .F. ) ;
#89425 = CARTESIAN_POINT ( 'NONE',  ( 0.1532563361054100626, 55.80059781766745175, -2.638427012816831230 ) ) ;
#89426 = CARTESIAN_POINT ( 'NONE',  ( -0.8801773607111008646, 38.27201867748816255, 2.915334737309923430 ) ) ;
#89427 = PRESENTATION_STYLE_ASSIGNMENT (( #81918 ) ) ;
#89428 = EDGE_CURVE ( 'NONE', #96626, #71776, #84113, .T. ) ;
#89429 = DIRECTION ( 'NONE',  ( 0.000000000000000000, -1.000000000000000000, 0.000000000000000000 ) ) ;
#89430 = DIRECTION ( 'NONE',  ( -0.000000000000000000, -1.000000000000000000, -0.000000000000000000 ) ) ;
#89431 = CARTESIAN_POINT ( 'NONE',  ( -4.164238869374098151, 51.59541550158063217, -3.795296366450310543 ) ) ;
#89432 = CARTESIAN_POINT ( 'NONE',  ( -0.8801773607110991993, 57.85535201082149825, -2.915334737309923874 ) ) ;
#89433 = DIRECTION ( 'NONE',  ( -0.9935718556765871234, 0.000000000000000000, -0.1132032137679106348 ) ) ;
#89434 = B_SPLINE_CURVE_WITH_KNOTS ( 'NONE', 3,
 ( #56905, #95405, #94906, #19406, #87408, #64397 ),
 .UNSPECIFIED., .F., .F.,
 ( 4, 2, 4 ),
 ( 3.409110551494641268E-05, 0.0004400426677367945405, 0.0008459942299586426006 ),
 .UNSPECIFIED. ) ;
#89435 = DIRECTION ( 'NONE',  ( -0.000000000000000000, 0.000000000000000000, -1.000000000000000000 ) ) ;
#89436 = CARTESIAN_POINT ( 'NONE',  ( 19.84674366389459266, 53.71726448433411605, -2.638427012816827677 ) ) ;
#89437 = CARTESIAN_POINT ( 'NONE',  ( 19.84674366389459621, 3.508931151000785231, 7.409399052514197653E-17 ) ) ;
#89438 = CARTESIAN_POINT ( 'NONE',  ( 1.472469842513823179, 20.59226448433411960, -4.923371831947296329 ) ) ;
#89439 = EDGE_CURVE ( 'NONE', #92463, #48349, #7288, .T. ) ;
#89440 = CARTESIAN_POINT ( 'NONE',  ( 1.472469842513823179, 25.59226448433412315, -4.923371831947296329 ) ) ;
#89441 = CARTESIAN_POINT ( 'NONE',  ( -12.81628187352647963, -21.08469866340291432, -3.434112377981046293 ) ) ;
#89442 = AXIS2_PLACEMENT_3D ( 'NONE', #6245, #14751, #46218 ) ;
#89443 = CARTESIAN_POINT ( 'NONE',  ( 0.5774900079438607392, 23.48035201082150536, 5.440088680355550821 ) ) ;
#89444 = CARTESIAN_POINT ( 'NONE',  ( 5.076628168052704559, 20.17559781766745175, -8.527530157486179263 ) ) ;
#89445 = CARTESIAN_POINT ( 'NONE',  ( 22.81628187352648496, 11.83196800326375531, -3.434112377981050290 ) ) ;
#89447 = CARTESIAN_POINT ( 'NONE',  ( 17.96484262340118221, 51.18868534415483396, -7.964842623401177768 ) ) ;
#89446 = CARTESIAN_POINT ( 'NONE',  ( -0.8801773607110991993, 62.85535201082150536, -2.915334737309923874 ) ) ;
#89449 = CARTESIAN_POINT ( 'NONE',  ( 3.591859063236761518, 59.95696800326375353, 11.09922568453594849 ) ) ;
#89448 = CARTESIAN_POINT ( 'NONE',  ( 0.5774900079438590739, 27.64701867748817676, -5.440088680355550821 ) ) ;
#89450 = CARTESIAN_POINT ( 'NONE',  ( -4.164238869374099039, 46.80374883491397497, 8.674139862899312516E-16 ) ) ;
#89451 = CARTESIAN_POINT ( 'NONE',  ( 6.879999999999995453, 70.25000000000000000, 6.250000000000000000 ) ) ;
#89452 = VERTEX_POINT ( 'NONE', #31053 ) ;
#89453 = CARTESIAN_POINT ( 'NONE',  ( 3.591859063236763294, -1.709698663402913210, -11.09922568453595026 ) ) ;
#89454 = CARTESIAN_POINT ( 'NONE',  ( 12.91533473730993009, 11.60535201082150536, -10.88017736071109987 ) ) ;
#89455 = CARTESIAN_POINT ( 'NONE',  ( 0.5774900079438607392, 48.48035201082150536, 5.440088680355550821 ) ) ;
#89456 = CARTESIAN_POINT ( 'NONE',  ( 10.00000000000000000, 0.5537488349139675359, -14.16423886937410082 ) ) ;
#89457 = VERTEX_POINT ( 'NONE', #36607 ) ;
#89458 = CARTESIAN_POINT ( 'NONE',  ( 14.92337183194729988, 19.34226448433411960, -8.527530157486177487 ) ) ;
#89459 = CARTESIAN_POINT ( 'NONE',  ( 0.5774900079438590739, 62.64701867748817676, -5.440088680355550821 ) ) ;
#89460 = CARTESIAN_POINT ( 'NONE',  ( 17.20831665107776587, 32.88393115100078745, 7.208316651077764980 ) ) ;
#89461 = CARTESIAN_POINT ( 'NONE',  ( 10.00000000000000000, 24.75893115100078745, -9.846743663894594434 ) ) ;
#89462 = CARTESIAN_POINT ( 'NONE',  ( 1.472469842513823179, 15.59226448433411960, -4.923371831947296329 ) ) ;
#89463 = DIRECTION ( 'NONE',  ( 0.8141155183563186792, 0.000000000000000000, -0.5807029557109404383 ) ) ;
#89464 = EDGE_CURVE ( 'NONE', #25008, #64876, #18660, .T. ) ;
#89466 = DIRECTION ( 'NONE',  ( 1.000000000000000000, 0.000000000000000000, 0.000000000000000000 ) ) ;
#89465 = CARTESIAN_POINT ( 'NONE',  ( 0.5774900079438590739, 67.64701867748817676, -5.440088680355550821 ) ) ;
#89468 = EDGE_LOOP ( 'NONE', ( #29774, #27362, #33451, #96453 ) ) ;
#89467 = CARTESIAN_POINT ( 'NONE',  ( 2.791683348922237240, 35.38393115100079456, -7.208316651077763204 ) ) ;
#89469 = AXIS2_PLACEMENT_3D ( 'NONE', #17238, #62217, #78211 ) ;
#89470 = CARTESIAN_POINT ( 'NONE',  ( 13.43411237798105340, 50.58196800326375353, 12.81628187352647963 ) ) ;
#89471 = CARTESIAN_POINT ( 'NONE',  ( 7.079515573063599021, -88.00917032380691296, 4.000000000000000000 ) ) ;
#89472 = CARTESIAN_POINT ( 'NONE',  ( 1.472469842513823179, 66.42559781766745175, 4.923371831947296329 ) ) ;
#89473 = DIRECTION ( 'NONE',  ( -1.000000000000000000, 0.000000000000000000, 0.000000000000000000 ) ) ;
#89474 = CARTESIAN_POINT ( 'NONE',  ( 13.79529636645031943, 20.34541550158063572, -14.16423886937409904 ) ) ;
#89475 = AXIS2_PLACEMENT_3D ( 'NONE', #28399, #74882, #97409 ) ;
#89476 = UNCERTAINTY_MEASURE_WITH_UNIT (LENGTH_MEASURE( 1.000000000000000082E-05 ), #86410, 'distance_accuracy_value', 'NONE');
#89477 = CARTESIAN_POINT ( 'NONE',  ( 1.492507162822248157, 42.19955587570481725, -6.500000000000035527 ) ) ;
#89478 = CARTESIAN_POINT ( 'NONE',  ( -4.164238869374098151, 16.59541550158063927, -3.795296366450310543 ) ) ;
#89479 = ADVANCED_FACE ( 'NONE', ( #45076 ), #22099, .T. ) ;
#89480 = AXIS2_PLACEMENT_3D ( 'NONE', #26303, #24850, #49300 ) ;
#89481 = CARTESIAN_POINT ( 'NONE',  ( 17.08211943468705840, 45.13708216824730357, -12.26659068614894466 ) ) ;
#89482 = CARTESIAN_POINT ( 'NONE',  ( -0.3689425029237881626, 2.428748834913967869, 10.36894250292379027 ) ) ;
#89483 = CARTESIAN_POINT ( 'NONE',  ( -0.3689425029237881626, 12.42874883491396609, 10.36894250292379027 ) ) ;
#89484 = CARTESIAN_POINT ( 'NONE',  ( 19.42250999205614193, 45.14701867748817676, 5.440088680355555262 ) ) ;
#89485 = CARTESIAN_POINT ( 'NONE',  ( 6.930493939446634499, -71.55570417525920845, -3.750000000000000888 ) ) ;
#89486 = ORIENTED_EDGE ( 'NONE', *, *, #41696, .T. ) ;
#89487 = CARTESIAN_POINT ( 'NONE',  ( 14.92337183194729633, 27.67559781766745530, 8.527530157486181039 ) ) ;
#89490 = VECTOR ( 'NONE', #51209, 1000.000000000000000 ) ;
#89489 = CARTESIAN_POINT ( 'NONE',  ( 2.791683348922240793, 31.63393115100078745, 7.208316651077764092 ) ) ;
#89488 = CARTESIAN_POINT ( 'NONE',  ( 19.72487221294570858, 61.86607318730076344, 6.500000000000000888 ) ) ;
#89491 = CARTESIAN_POINT ( 'NONE',  ( -0.8801773607111008646, 13.27201867748817321, 2.915334737309923430 ) ) ;
#89492 = CARTESIAN_POINT ( 'NONE',  ( 13.43411237798106583, 52.66530133659708213, -12.81628187352647252 ) ) ;
#89493 = CARTESIAN_POINT ( 'NONE',  ( 18.52753015748617571, 53.09226448433412315, 4.923371831947298993 ) ) ;
#89494 =( LENGTH_UNIT ( ) NAMED_UNIT ( * ) SI_UNIT ( .MILLI., .METRE. ) );
#89495 = CARTESIAN_POINT ( 'NONE',  ( 22.81628187352647785, 46.41530133659708213, 3.434112377981063169 ) ) ;
#89496 = CARTESIAN_POINT ( 'NONE',  ( 7.082119434687054849, -26.52958449841936428, 12.26659068614894288 ) ) ;
#89497 = CARTESIAN_POINT ( 'NONE',  ( 12.91533473730992121, 44.52201867748816966, 10.88017736071110164 ) ) ;
#89498 = CARTESIAN_POINT ( 'NONE',  ( 5.076628168052703671, 41.84226448433411605, 8.527530157486179263 ) ) ;
#89499 = CARTESIAN_POINT ( 'NONE',  ( -0.3689425029237881626, 22.42874883491397142, 10.36894250292379027 ) ) ;
#89500 = ORIENTED_EDGE ( 'NONE', *, *, #73027, .T. ) ;
#89501 = CARTESIAN_POINT ( 'NONE',  ( -4.164238869374098151, 6.595415501580634832, -3.795296366450310543 ) ) ;
#89502 = CARTESIAN_POINT ( 'NONE',  ( 15.44008868035555260, 44.73035201082151247, 9.422509992056143702 ) ) ;
#89503 = CARTESIAN_POINT ( 'NONE',  ( 20.88017736071110519, 65.56368534415483396, 2.639326808657452039E-16 ) ) ;
#89504 = CARTESIAN_POINT ( 'NONE',  ( -4.164238869374099927, 42.01208216824728936, 3.795296366450308767 ) ) ;
#89505 = CARTESIAN_POINT ( 'NONE',  ( 12.63842701281683922, 64.55059781766745175, -9.846743663894590881 ) ) ;
#89506 = DIRECTION ( 'NONE',  ( -0.9304175679820231304, 0.000000000000000000, -0.3665012267243009103 ) ) ;
#89507 = CARTESIAN_POINT ( 'NONE',  ( 15.44008868035555260, 54.73035201082150536, 9.422509992056143702 ) ) ;
#89508 = CARTESIAN_POINT ( 'NONE',  ( -0.8649609010934330433, 15.00000000000000888, 14.60103384664008885 ) ) ;
#89509 = AXIS2_PLACEMENT_3D ( 'NONE', #74622, #97162, #37627 ) ;
#89510 = CARTESIAN_POINT ( 'NONE',  ( 3.591859063236763294, 23.29030133659708568, -11.09922568453595026 ) ) ;
#89511 = CARTESIAN_POINT ( 'NONE',  ( 10.00000000000000000, 2.873634669930420049, -12.81628187352647608 ) ) ;
#89512 = CARTESIAN_POINT ( 'NONE',  ( -2.915334737309917656, 34.10535201082151957, 10.88017736071110164 ) ) ;
#89513 = CARTESIAN_POINT ( 'NONE',  ( 2.035157376598822676, 17.43868534415483751, -7.964842623401177768 ) ) ;
#89514 = CARTESIAN_POINT ( 'NONE',  ( 20.88017736071110164, 5.355352010821503583, 2.915334737309930979 ) ) ;
#89515 = CYLINDRICAL_SURFACE ( 'NONE', #7328, 0.2500000000000002220 ) ;
#89516 = ORIENTED_EDGE ( 'NONE', *, *, #6116, .F. ) ;
#89517 = B_SPLINE_CURVE_WITH_KNOTS ( 'NONE', 3,
 ( #48755, #93772, #94756, #77287, #79263, #26257 ),
 .UNSPECIFIED., .F., .F.,
 ( 4, 2, 4 ),
 ( 0.0002800056097769411802, 0.0006862108940652274832, 0.001092416178353513949 ),
 .UNSPECIFIED. ) ;
#89518 = VECTOR ( 'NONE', #26534, 1000.000000000000000 ) ;
#89519 = EDGE_CURVE ( 'NONE', #22589, #72372, #84074, .T. ) ;
#89520 = CARTESIAN_POINT ( 'NONE',  ( 10.00000000000000000, 4.758931151000784787, -9.846743663894594434 ) ) ;
#89521 = AXIS2_PLACEMENT_3D ( 'NONE', #49612, #89105, #80627 ) ;
#89522 = CARTESIAN_POINT ( 'NONE',  ( 7.361572987183169658, 39.96726448433411605, -9.846743663894592657 ) ) ;
#89523 = EDGE_CURVE ( 'NONE', #85047, #97286, #37100, .T. ) ;
#89524 = CARTESIAN_POINT ( 'NONE',  ( 7.084665262690076126, 42.02201867748816966, -10.88017736071110164 ) ) ;
#89525 = CARTESIAN_POINT ( 'NONE',  ( -1.099225684535947600, 9.540301336597087456, 6.408140936763237150 ) ) ;
#89527 = CARTESIAN_POINT ( 'NONE',  ( 14.11874224319628013, 14.76984899115444527, 4.887061453530134436 ) ) ;
#89526 = CARTESIAN_POINT ( 'NONE',  ( 12.91533473730992121, 34.52201867748817676, 10.88017736071110164 ) ) ;
#89528 = CYLINDRICAL_SURFACE ( 'NONE', #76837, 0.2500000000000002220 ) ;
#89529 = CARTESIAN_POINT ( 'NONE',  ( 0.6178305044545818747, 48.49863466993042493, -9.382169495545419124 ) ) ;
#89530 = ORIENTED_EDGE ( 'NONE', *, *, #75635, .F. ) ;
#89531 = CARTESIAN_POINT ( 'NONE',  ( 17.96484262340118221, 59.93868534415484106, 7.964842623401181321 ) ) ;
#89533 = CARTESIAN_POINT ( 'NONE',  ( 22.26659068614895176, 4.720415501580633943, -7.082119434687042414 ) ) ;
#89532 = CARTESIAN_POINT ( 'NONE',  ( 3.591859063236761518, 29.95696800326375708, 11.09922568453594849 ) ) ;
#89534 =( NAMED_UNIT ( * ) SI_UNIT ( $, .STERADIAN. ) SOLID_ANGLE_UNIT ( ) );
#89535 = CARTESIAN_POINT ( 'NONE',  ( 2.035157376598822676, 42.43868534415483396, -7.964842623401177768 ) ) ;
#89536 = CARTESIAN_POINT ( 'NONE',  ( 18.52753015748617571, 63.09226448433412315, 4.923371831947298993 ) ) ;
#89537 = CARTESIAN_POINT ( 'NONE',  ( 17.20831665107776587, 47.88393115100078745, 7.208316651077764980 ) ) ;
#89538 = CARTESIAN_POINT ( 'NONE',  ( 12.63842701281683922, 19.55059781766745175, -9.846743663894590881 ) ) ;
#89539 = CARTESIAN_POINT ( 'NONE',  ( 19.42250999205614548, 60.98035201082151247, -5.440088680355545492 ) ) ;
#89540 = CARTESIAN_POINT ( 'NONE',  ( 24.16423886937410614, 29.51208216824729647, -3.795296366450302550 ) ) ;
#89541 = ADVANCED_FACE ( 'NONE', ( #44584 ), #15098, .F. ) ;
#89542 = CARTESIAN_POINT ( 'NONE',  ( 20.15039907845753930, 70.00000000000000000, 6.262539305110068177 ) ) ;
#89543 = CARTESIAN_POINT ( 'NONE',  ( -4.262581422817185661, -13.85606188144533846, -4.000000000000000888 ) ) ;
#89544 = AXIS2_PLACEMENT_3D ( 'NONE', #88028, #73512, #13523 ) ;
#89545 = VERTEX_POINT ( 'NONE', #75580 ) ;
#89546 = VERTEX_POINT ( 'NONE', #14101 ) ;
#89547 = CARTESIAN_POINT ( 'NONE',  ( 24.16423886937410614, 64.30374883491396076, 8.672049930838204340E-16 ) ) ;
#89548 = CARTESIAN_POINT ( 'NONE',  ( 22.26659068614894466, 63.88708216824730357, 7.082119434687054849 ) ) ;
#89549 = CARTESIAN_POINT ( 'NONE',  ( 18.52753015748618282, 33.92559781766745886, -4.923371831947291888 ) ) ;
#89550 = PRESENTATION_STYLE_ASSIGNMENT (( #67047 ) ) ;
#89551 = CARTESIAN_POINT ( 'NONE',  ( 10.00000000000000178, 14.31368534415483751, 10.88017736071110342 ) ) ;
#89552 = CARTESIAN_POINT ( 'NONE',  ( 2.917880565312950480, 55.97041550158063217, -12.26659068614894821 ) ) ;
#89553 = CARTESIAN_POINT ( 'NONE',  ( 10.00000000000000000, 34.75893115100078745, -9.846743663894594434 ) ) ;
#89554 = DIRECTION ( 'NONE',  ( 0.000000000000000000, 0.000000000000000000, -1.000000000000000000 ) ) ;
#89555 = CARTESIAN_POINT ( 'NONE',  ( 1.472469842513823179, 10.59226448433411782, -4.923371831947296329 ) ) ;
#89556 = AXIS2_PLACEMENT_3D ( 'NONE', #70848, #2361, #60863 ) ;
#89557 = EDGE_CURVE ( 'NONE', #84748, #3599, #7561, .T. ) ;
#89558 = CIRCLE ( 'NONE', #86354, 0.09999999999999982514 ) ;
#89559 = CARTESIAN_POINT ( 'NONE',  ( 0.000000000000000000, 15.00000000000000000, 0.000000000000000000 ) ) ;
#89560 = CARTESIAN_POINT ( 'NONE',  ( 9.846743663894594434, 13.50893115100078923, -2.168404344971008868E-15 ) ) ;
#89561 = ORIENTED_EDGE ( 'NONE', *, *, #96999, .T. ) ;
#89562 = ORIENTED_EDGE ( 'NONE', *, *, #61852, .T. ) ;
#89563 = ORIENTED_EDGE ( 'NONE', *, *, #58707, .F. ) ;
#89564 = CARTESIAN_POINT ( 'NONE',  ( 18.52753015748617571, 43.09226448433412315, 4.923371831947298993 ) ) ;
#89566 = CARTESIAN_POINT ( 'NONE',  ( 15.44008868035555793, 21.39701867748817321, -9.422509992056140149 ) ) ;
#89565 = CARTESIAN_POINT ( 'NONE',  ( 20.88017736071110875, 15.77201867748817143, -2.915334737309920765 ) ) ;
#89567 = CARTESIAN_POINT ( 'NONE',  ( 22.81628187352647785, 21.62363466993041783, 6.195893100308588602E-16 ) ) ;
#89568 = CARTESIAN_POINT ( 'NONE',  ( -4.164238869374099927, 2.012082168247300906, 3.795296366450308767 ) ) ;
#89569 = CARTESIAN_POINT ( 'NONE',  ( -1.099225684535947600, 34.54030133659708923, 6.408140936763237150 ) ) ;
#89570 = ORIENTED_EDGE ( 'NONE', *, *, #64952, .F. ) ;
#89571 = CARTESIAN_POINT ( 'NONE',  ( 0.1532563361054083140, 31.00893115100078390, 1.131784320476157264E-15 ) ) ;
#89572 = CARTESIAN_POINT ( 'NONE',  ( 10.00000000000000178, 68.05374883491397497, 14.16423886937410082 ) ) ;
#89573 = ORIENTED_EDGE ( 'NONE', *, *, #85707, .T. ) ;
#89574 = CARTESIAN_POINT ( 'NONE',  ( -0.3689425029237881626, 67.42874883491396076, 10.36894250292379027 ) ) ;
#89575 = VERTEX_POINT ( 'NONE', #23091 ) ;
#89576 = CARTESIAN_POINT ( 'NONE',  ( 20.88017736071110164, 50.35535201082151247, 2.915334737309930979 ) ) ;
#89577 = CARTESIAN_POINT ( 'NONE',  ( -0.8801773607111008646, 63.27201867748817676, 2.915334737309923430 ) ) ;
#89578 = CARTESIAN_POINT ( 'NONE',  ( 17.96484262340118221, 56.18868534415484817, -7.964842623401177768 ) ) ;
#89579 = CARTESIAN_POINT ( 'NONE',  ( 2.791683348922240793, 1.633931151000784565, 7.208316651077764092 ) ) ;
#89580 = CARTESIAN_POINT ( 'NONE',  ( 19.42250999205614193, 45.14701867748817676, 5.440088680355555262 ) ) ;
#89581 = AXIS2_PLACEMENT_3D ( 'NONE', #93801, #40814, #62309 ) ;
#89582 = AXIS2_PLACEMENT_3D ( 'NONE', #32792, #18300, #79779 ) ;
#89583 = CARTESIAN_POINT ( 'NONE',  ( 24.35999999999999233, 44.99999999999999289, 7.000000000000000000 ) ) ;
#89584 = EDGE_CURVE ( 'NONE', #31232, #6963, #31166, .T. ) ;
#89585 = EDGE_LOOP ( 'NONE', ( #82809, #35924, #45695, #51724 ) ) ;
#89586 = AXIS2_PLACEMENT_3D ( 'NONE', #36613, #76568, #44590 ) ;
#89587 = CARTESIAN_POINT ( 'NONE',  ( 7.361572987183170547, 27.05059781766745175, 9.846743663894590881 ) ) ;
#89588 = VERTEX_POINT ( 'NONE', #54054 ) ;
#89589 = CARTESIAN_POINT ( 'NONE',  ( 18.52753015748617571, 53.09226448433412315, 4.923371831947298993 ) ) ;
#89590 = CARTESIAN_POINT ( 'NONE',  ( -2.614810775378867191, 35.00346125376525919, 10.00000000000000000 ) ) ;
#89591 = B_SPLINE_CURVE_WITH_KNOTS ( 'NONE', 3,
 ( #45913, #69395, #29902, #52903 ),
 .UNSPECIFIED., .F., .F.,
 ( 4, 4 ),
 ( 0.000000000000000000, 0.001036303429213365507 ),
 .UNSPECIFIED. ) ;
#89592 = CARTESIAN_POINT ( 'NONE',  ( -4.164238869374099039, 11.80374883491396965, 8.674139862899312516E-16 ) ) ;
#89593 = ORIENTED_EDGE ( 'NONE', *, *, #5682, .F. ) ;
#89594 = CARTESIAN_POINT ( 'NONE',  ( 19.72487221294571569, 50.71833443783938122, -6.499999999999983125 ) ) ;
#89595 = CARTESIAN_POINT ( 'NONE',  ( -6.607088789283611874, -50.94270388117418946, 3.750000000000000000 ) ) ;
#89597 = CARTESIAN_POINT ( 'NONE',  ( 5.076628168052703671, 36.84226448433412315, 8.527530157486179263 ) ) ;
#89596 = FACE_OUTER_BOUND ( 'NONE', #48621, .T. ) ;
#89598 = CARTESIAN_POINT ( 'NONE',  ( 10.00000000000000178, 63.05374883491396076, 14.16423886937410082 ) ) ;
#89599 = DIRECTION ( 'NONE',  ( -0.000000000000000000, -1.000000000000000000, -0.000000000000000000 ) ) ;
#89600 = ORIENTED_EDGE ( 'NONE', *, *, #26972, .T. ) ;
#89601 = CARTESIAN_POINT ( 'NONE',  ( 20.15039907845753575, 62.62777174578612716, -6.262539305110073506 ) ) ;
#89602 = CARTESIAN_POINT ( 'NONE',  ( 17.20831665107776587, 42.88393115100077324, 7.208316651077764980 ) ) ;
#89603 = DIRECTION ( 'NONE',  ( -0.000000000000000000, 1.000000000000000000, -0.000000000000000000 ) ) ;
#89604 = CARTESIAN_POINT ( 'NONE',  ( 13.43411237798106583, 22.66530133659708923, -12.81628187352647252 ) ) ;
#89605 = CARTESIAN_POINT ( 'NONE',  ( 5.076628168052704559, 10.17559781766745175, -8.527530157486179263 ) ) ;
#89606 = DIRECTION ( 'NONE',  ( 0.000000000000000000, -1.000000000000000000, 0.000000000000000000 ) ) ;
#89607 = CARTESIAN_POINT ( 'NONE',  ( 0.1532563361054100626, 5.800597817667452638, -2.638427012816831230 ) ) ;
#89608 = CARTESIAN_POINT ( 'NONE',  ( -2.816281873526471635, 8.915301336597083903, -3.434112377981056508 ) ) ;
#89609 = CARTESIAN_POINT ( 'NONE',  ( 1.472469842513823179, 25.59226448433412315, -4.923371831947296329 ) ) ;
#89610 = ORIENTED_EDGE ( 'NONE', *, *, #16528, .F. ) ;
#89611 = CARTESIAN_POINT ( 'NONE',  ( 2.035157376598822676, 12.43868534415483751, -7.964842623401177768 ) ) ;
#89612 = CARTESIAN_POINT ( 'NONE',  ( 17.08211943468705840, 10.13708216824730179, -12.26659068614894466 ) ) ;
#89613 = CARTESIAN_POINT ( 'NONE',  ( 1.472469842513823179, 31.42559781766745530, 4.923371831947296329 ) ) ;
#89614 = CARTESIAN_POINT ( 'NONE',  ( 19.42250999205614193, 60.14701867748817676, 5.440088680355555262 ) ) ;
#89615 = AXIS2_PLACEMENT_3D ( 'NONE', #45501, #8010, #38019 ) ;
#89617 = FACE_OUTER_BOUND ( 'NONE', #69956, .T. ) ;
#89616 = CARTESIAN_POINT ( 'NONE',  ( 22.81628187352647785, 21.41530133659708923, 3.434112377981063169 ) ) ;
#89618 = CARTESIAN_POINT ( 'NONE',  ( 4.559911319644449179, 8.897018677488171434, 9.422509992056141925 ) ) ;
#89619 = CARTESIAN_POINT ( 'NONE',  ( 8.880000000000020322, 80.32179676972448590, -4.250000000000000000 ) ) ;
#89620 = CARTESIAN_POINT ( 'NONE',  ( 14.24131928502211331, 15.00000000000000000, 0.4973178280106892446 ) ) ;
#89621 = CARTESIAN_POINT ( 'NONE',  ( 14.92337183194729988, 64.34226448433412315, -8.527530157486177487 ) ) ;
#89622 = CARTESIAN_POINT ( 'NONE',  ( 18.52753015748618282, 33.92559781766745886, -4.923371831947291888 ) ) ;
#89623 = CARTESIAN_POINT ( 'NONE',  ( -5.204170427930421283E-15, -8.186314655845155386, -10.88017736071110342 ) ) ;
#89624 = CARTESIAN_POINT ( 'NONE',  ( 13.43411237798106583, 37.66530133659708923, -12.81628187352647252 ) ) ;
#89625 = STYLED_ITEM ( 'NONE', ( #69133 ), #74243 ) ;
#89627 = CARTESIAN_POINT ( 'NONE',  ( 12.74414838903278557, 6.606856988583540673E-16, -7.178093659841974450 ) ) ;
#89626 = CARTESIAN_POINT ( 'NONE',  ( 19.42250999205614193, 40.14701867748817676, 5.440088680355555262 ) ) ;
#89628 = CARTESIAN_POINT ( 'NONE',  ( -2.283843307429720415, 13.12729635533385597, 9.500000000000000000 ) ) ;
#89629 = CARTESIAN_POINT ( 'NONE',  ( 20.88017736071110519, 25.56368534415483751, 2.639326808657452039E-16 ) ) ;
#89630 = ADVANCED_FACE ( 'NONE', ( #59585 ), #84567, .T. ) ;
#89631 = CARTESIAN_POINT ( 'NONE',  ( 19.42250999205614548, 35.98035201082151247, -5.440088680355545492 ) ) ;
#89632 = CARTESIAN_POINT ( 'NONE',  ( 14.92337183194729633, 52.67559781766745175, 8.527530157486181039 ) ) ;
#89633 = CARTESIAN_POINT ( 'NONE',  ( 7.084665262690076126, 59.10535201082150536, 10.88017736071109987 ) ) ;
#89634 = CARTESIAN_POINT ( 'NONE',  ( 13.79529636645031943, 30.34541550158063927, -14.16423886937409904 ) ) ;
#89635 = ADVANCED_FACE ( 'NONE', ( #21607 ), #52093, .T. ) ;
#89636 = EDGE_CURVE ( 'NONE', #59040, #7312, #79331, .T. ) ;
#89637 = CARTESIAN_POINT ( 'NONE',  ( 18.52753015748617571, 43.09226448433412315, 4.923371831947298993 ) ) ;
#89638 = CARTESIAN_POINT ( 'NONE',  ( 19.38216949554541202, 0.9986346699304200492, 9.382169495545424454 ) ) ;
#89639 = ORIENTED_EDGE ( 'NONE', *, *, #25653, .F. ) ;
#89640 = CARTESIAN_POINT ( 'NONE',  ( 19.42250999205614548, 20.98035201082150891, -5.440088680355545492 ) ) ;
#89641 = CARTESIAN_POINT ( 'NONE',  ( -9.876730923139145801, 15.00000000000000000, -11.28938378619076843 ) ) ;
#89642 = CARTESIAN_POINT ( 'NONE',  ( 2.035157376598824452, 18.68868534415484106, 7.964842623401179544 ) ) ;
#89643 = CARTESIAN_POINT ( 'NONE',  ( 12.63842701281683034, 2.467264484334118269, 9.846743663894596210 ) ) ;
#89644 = CARTESIAN_POINT ( 'NONE',  ( 17.08211943468705840, 30.13708216824730357, -12.26659068614894466 ) ) ;
#89645 = CARTESIAN_POINT ( 'NONE',  ( 5.076628168052703671, 11.84226448433411960, 8.527530157486179263 ) ) ;
#89646 = CARTESIAN_POINT ( 'NONE',  ( 14.92337183194729988, 64.34226448433412315, -8.527530157486177487 ) ) ;
#89647 = CARTESIAN_POINT ( 'NONE',  ( 12.91533473730993009, 46.60535201082150536, -10.88017736071109987 ) ) ;
#89648 = CARTESIAN_POINT ( 'NONE',  ( 18.17884179759845509, 38.66688879859523098, -6.500000000000054179 ) ) ;
#89649 = CARTESIAN_POINT ( 'NONE',  ( 0.000000000000000000, 0.5000000000000004441, 0.000000000000000000 ) ) ;
#89650 = EDGE_CURVE ( 'NONE', #63634, #38758, #97783, .T. ) ;
#89651 = CIRCLE ( 'NONE', #89582, 0.2500000000000002220 ) ;
#89652 = EDGE_LOOP ( 'NONE', ( #79390, #2699, #4186, #98631, #98597, #53211 ) ) ;
#89653 = CARTESIAN_POINT ( 'NONE',  ( -10.44999999999999751, 99.99999999999998579, -8.000000000000000000 ) ) ;
#89654 = CARTESIAN_POINT ( 'NONE',  ( 19.84674366389459621, 48.50893115100078745, 7.409399052514197653E-17 ) ) ;
#89655 = ORIENTED_EDGE ( 'NONE', *, *, #40114, .F. ) ;
#89656 = ORIENTED_EDGE ( 'NONE', *, *, #66158, .F. ) ;
#89657 = SURFACE_SIDE_STYLE ('',( #81653 ) ) ;
#89658 = CARTESIAN_POINT ( 'NONE',  ( -2.266590686148945544, 16.38708216824730357, -7.082119434687050408 ) ) ;
#89659 = CARTESIAN_POINT ( 'NONE',  ( 22.26659068614894466, 28.88708216824730357, 7.082119434687054849 ) ) ;
#89660 = CARTESIAN_POINT ( 'NONE',  ( 15.44008868035555260, 54.73035201082150536, 9.422509992056143702 ) ) ;
#89661 = CARTESIAN_POINT ( 'NONE',  ( 2.917880565312948704, 52.63708216824730357, 12.26659068614894643 ) ) ;
#89662 = CARTESIAN_POINT ( 'NONE',  ( 1.472469842513823179, 66.42559781766745175, 4.923371831947296329 ) ) ;
#89663 = CARTESIAN_POINT ( 'NONE',  ( 14.92337183194729633, 42.67559781766745886, 8.527530157486181039 ) ) ;
#89665 = CARTESIAN_POINT ( 'NONE',  ( 13.43411237798106583, 7.665301336597086568, -12.81628187352647252 ) ) ;
#89664 = CARTESIAN_POINT ( 'NONE',  ( 4.559911319644449179, 48.89701867748817676, 9.422509992056141925 ) ) ;
#89666 = CARTESIAN_POINT ( 'NONE',  ( -2.266590686148945544, 22.22041550158063572, 7.082119434687048631 ) ) ;
#89667 = CARTESIAN_POINT ( 'NONE',  ( -2.266590686148945544, 46.38708216824730357, -7.082119434687050408 ) ) ;
#89668 = CARTESIAN_POINT ( 'NONE',  ( 10.00000000000000000, 21.81368534415484106, -10.88017736071110342 ) ) ;
#89669 = CARTESIAN_POINT ( 'NONE',  ( 19.84674366389459266, 53.71726448433411605, -2.638427012816827677 ) ) ;
#89670 = CARTESIAN_POINT ( 'NONE',  ( 2.035157376598822676, 37.43868534415484106, -7.964842623401177768 ) ) ;
#89671 = EDGE_CURVE ( 'NONE', #44083, #77740, #1579, .T. ) ;
#89672 = CARTESIAN_POINT ( 'NONE',  ( 19.38216949554541202, 50.99863466993042493, 9.382169495545424454 ) ) ;
#89673 = CARTESIAN_POINT ( 'NONE',  ( 2.638427012816835227, -17.53273551566588040, 9.846743663894590881 ) ) ;
#89674 = VERTEX_POINT ( 'NONE', #17063 ) ;
#89675 = FACE_OUTER_BOUND ( 'NONE', #1043, .T. ) ;
#89676 = VERTEX_POINT ( 'NONE', #25062 ) ;
#89677 = ORIENTED_EDGE ( 'NONE', *, *, #58336, .T. ) ;
#89678 = CARTESIAN_POINT ( 'NONE',  ( 13.79529636645031943, 45.34541550158062506, -14.16423886937409904 ) ) ;
#89679 = CARTESIAN_POINT ( 'NONE',  ( 12.63842701281683034, 47.46726448433412315, 9.846743663894596210 ) ) ;
#89680 = CARTESIAN_POINT ( 'NONE',  ( 15.44008868035555260, 64.73035201082151957, 9.422509992056143702 ) ) ;
#89681 = DIRECTION ( 'NONE',  ( -0.4617486132350466788, -0.000000000000000000, 0.8870108331782150524 ) ) ;
#89682 = CARTESIAN_POINT ( 'NONE',  ( 2.035157376598824452, 53.68868534415484817, 7.964842623401179544 ) ) ;
#89683 = AXIS2_PLACEMENT_3D ( 'NONE', #71367, #35310, #80818 ) ;
#89684 = CARTESIAN_POINT ( 'NONE',  ( 12.81628187352647252, 11.83196800326375708, -3.434112377981059172 ) ) ;
#89685 = ORIENTED_EDGE ( 'NONE', *, *, #67641, .T. ) ;
#89686 = COLOUR_RGB ( '', 0.09019608, 0.27058824, 0.51372549) ;
#89687 = CARTESIAN_POINT ( 'NONE',  ( -2.266590686148945544, 27.22041550158063572, 7.082119434687048631 ) ) ;
#89688 = CARTESIAN_POINT ( 'NONE',  ( 0.6178305044545838731, 24.74863466993042493, 9.382169495545420901 ) ) ;
#89689 = ORIENTED_EDGE ( 'NONE', *, *, #29282, .T. ) ;
#89690 = CARTESIAN_POINT ( 'NONE',  ( -1.099225684535947600, 38.70696800326375353, -6.408140936763238038 ) ) ;
#89691 = CARTESIAN_POINT ( 'NONE',  ( 12.91533473730993009, 16.60535201082150891, -10.88017736071109987 ) ) ;
#89692 = CARTESIAN_POINT ( 'NONE',  ( 18.52753015748617571, 38.09226448433412315, 4.923371831947298993 ) ) ;
#89693 = CARTESIAN_POINT ( 'NONE',  ( 20.88017736071110164, 15.35535201082150358, 2.915334737309930979 ) ) ;
#89694 = AXIS2_PLACEMENT_3D ( 'NONE', #42032, #96008, #41543 ) ;
#89695 = CARTESIAN_POINT ( 'NONE',  ( 3.591859063236761518, 64.95696800326376774, 11.09922568453594849 ) ) ;
#89696 = DIRECTION ( 'NONE',  ( 0.000000000000000000, 0.000000000000000000, 1.000000000000000000 ) ) ;
#89697 = CARTESIAN_POINT ( 'NONE',  ( 18.52753015748618282, 43.92559781766745175, -4.923371831947291888 ) ) ;
#89698 = ORIENTED_EDGE ( 'NONE', *, *, #78535, .T. ) ;
#89699 = CARTESIAN_POINT ( 'NONE',  ( -0.2074183518478776300, 0.04876363957840557789, -14.75075219811622596 ) ) ;
#89700 = FACE_OUTER_BOUND ( 'NONE', #39746, .T. ) ;
#89701 = CARTESIAN_POINT ( 'NONE',  ( -3.836325488036278930, 0.5000000000000004441, 14.50112432709419785 ) ) ;
#89702 = CARTESIAN_POINT ( 'NONE',  ( 0.2751277870542868098, 57.28217586085237656, -6.499999999999985789 ) ) ;
#89703 = CARTESIAN_POINT ( 'NONE',  ( 7.361572987183170547, 12.05059781766744997, 9.846743663894590881 ) ) ;
#89704 = CARTESIAN_POINT ( 'NONE',  ( 21.09922568453594849, 21.20696800326375353, 6.408140936763242479 ) ) ;
#89705 = FACE_OUTER_BOUND ( 'NONE', #40202, .T. ) ;
#89706 = ORIENTED_EDGE ( 'NONE', *, *, #96135, .T. ) ;
#89707 = CARTESIAN_POINT ( 'NONE',  ( 10.00000000000000178, 57.25893115100078745, 9.846743663894594434 ) ) ;
#89708 = CARTESIAN_POINT ( 'NONE',  ( -11.35178980618980304, 0.5000000000000004441, 9.804941009311846756 ) ) ;
#89709 = CARTESIAN_POINT ( 'NONE',  ( 13.79529636645031943, 20.34541550158063572, -14.16423886937409904 ) ) ;
#89710 = CARTESIAN_POINT ( 'NONE',  ( 5.076628168052703671, 41.84226448433411605, 8.527530157486179263 ) ) ;
#89711 = CARTESIAN_POINT ( 'NONE',  ( 6.565887622018943937, 40.16530133659708923, 12.81628187352647430 ) ) ;
#89713 = DIRECTION ( 'NONE',  ( -0.000000000000000000, -0.000000000000000000, -1.000000000000000000 ) ) ;
#89712 = LINE ( 'NONE', #73718, #34078 ) ;
#89714 = CARTESIAN_POINT ( 'NONE',  ( 7.361572987183169658, 4.967264484334119601, -9.846743663894592657 ) ) ;
#89715 = CARTESIAN_POINT ( 'NONE',  ( 21.92686044187656691, 47.18830936912750929, 4.562052436263911564E-16 ) ) ;
#89716 = EDGE_CURVE ( 'NONE', #87186, #51568, #1200, .T. ) ;
#89717 = CARTESIAN_POINT ( 'NONE',  ( 19.84674366389459266, 48.30059781766745175, 2.638427012816836559 ) ) ;
#89718 = CARTESIAN_POINT ( 'NONE',  ( 17.96484262340118221, 46.18868534415484106, -7.964842623401177768 ) ) ;
#89719 = PRODUCT_CONTEXT ( 'NONE', #42329, 'mechanical' ) ;
#89720 = CARTESIAN_POINT ( 'NONE',  ( -18.89999999999999503, 92.00000000000000000, 8.000000000000000000 ) ) ;
#89721 = AXIS2_PLACEMENT_3D ( 'NONE', #31989, #83542, #68049 ) ;
#89722 = CARTESIAN_POINT ( 'NONE',  ( 12.91533473730993009, 41.60535201082149825, -10.88017736071109987 ) ) ;
#89723 = ORIENTED_EDGE ( 'NONE', *, *, #36933, .T. ) ;
#89724 = CARTESIAN_POINT ( 'NONE',  ( -11.35178980618980304, 15.00000000000000000, 9.804941009311846756 ) ) ;
#89725 = CARTESIAN_POINT ( 'NONE',  ( 15.44008868035555793, 11.39701867748817143, -9.422509992056140149 ) ) ;
#89727 = CARTESIAN_POINT ( 'NONE',  ( -0.8801773607110991993, 47.85535201082150536, -2.915334737309923874 ) ) ;
#89726 = CARTESIAN_POINT ( 'NONE',  ( 10.00000000000000178, 57.25893115100078745, 9.846743663894594434 ) ) ;
#89728 = DIRECTION ( 'NONE',  ( 0.000000000000000000, 0.000000000000000000, 1.000000000000000000 ) ) ;
#89729 = CARTESIAN_POINT ( 'NONE',  ( 7.084665262690076126, 59.10535201082150536, 10.88017736071109987 ) ) ;
#89730 = CARTESIAN_POINT ( 'NONE',  ( 19.42250999205614548, 20.98035201082150891, -5.440088680355545492 ) ) ;
#89731 = CARTESIAN_POINT ( 'NONE',  ( 19.84674366389459621, 3.508931151000785231, 7.409399052514197653E-17 ) ) ;
#89732 = CARTESIAN_POINT ( 'NONE',  ( 7.361572987183170547, 22.05059781766745530, 9.846743663894590881 ) ) ;
#89733 = CARTESIAN_POINT ( 'NONE',  ( -12.26659068614894110, 2.220415501580634388, 7.082119434687058401 ) ) ;
#89734 = CARTESIAN_POINT ( 'NONE',  ( 1.472469842513823179, 56.42559781766745886, 4.923371831947296329 ) ) ;
#89735 = EDGE_CURVE ( 'NONE', #76019, #61376, #31499, .T. ) ;
#89736 = CARTESIAN_POINT ( 'NONE',  ( 6.204703633549690345, 62.84541550158063927, 14.16423886937410082 ) ) ;
#89737 = CARTESIAN_POINT ( 'NONE',  ( 69.60148758828984228, 0.4999999999999982792, 10.00000000000000000 ) ) ;
#89738 = CARTESIAN_POINT ( 'NONE',  ( 10.00000000000000000, 5.553748834913967869, -14.16423886937410082 ) ) ;
#89739 = CARTESIAN_POINT ( 'NONE',  ( -4.164238869374098151, 51.59541550158063217, -3.795296366450310543 ) ) ;
#89740 = CARTESIAN_POINT ( 'NONE',  ( 19.38216949554541557, 7.248634669930421381, -9.382169495545420901 ) ) ;
#89741 = EDGE_CURVE ( 'NONE', #27523, #84834, #10743, .T. ) ;
#89742 = ORIENTED_EDGE ( 'NONE', *, *, #60295, .F. ) ;
#89743 = CARTESIAN_POINT ( 'NONE',  ( -0.8801773607111008646, 18.27201867748817321, 2.915334737309923430 ) ) ;
#89744 = CARTESIAN_POINT ( 'NONE',  ( 12.63842701281683034, 47.46726448433412315, 9.846743663894596210 ) ) ;
#89746 = CARTESIAN_POINT ( 'NONE',  ( -10.17588876012473520, 89.26462023800682744, -5.905476706514950713 ) ) ;
#89745 = SURFACE_STYLE_USAGE ( .BOTH. , #65759 ) ;
#89747 = EDGE_CURVE ( 'NONE', #65595, #30124, #58429, .T. ) ;
#89748 = AXIS2_PLACEMENT_3D ( 'NONE', #55036, #15101, #45577 ) ;
#89749 = SURFACE_STYLE_USAGE ( .BOTH. , #66254 ) ;
#89750 = CARTESIAN_POINT ( 'NONE',  ( 21.09922568453595559, 22.04030133659708923, -6.408140936763230044 ) ) ;
#89751 = CARTESIAN_POINT ( 'NONE',  ( 19.84674366389459266, 28.30059781766745886, 2.638427012816836559 ) ) ;
#89752 = ORIENTED_EDGE ( 'NONE', *, *, #16662, .F. ) ;
#89753 = CARTESIAN_POINT ( 'NONE',  ( 5.076628168052704559, 10.17559781766745175, -8.527530157486179263 ) ) ;
#89754 = VECTOR ( 'NONE', #80324, 999.9999999999998863 ) ;
#89755 = CARTESIAN_POINT ( 'NONE',  ( 10.93147959982391448, -92.98161664597374454, -4.000000000000000000 ) ) ;
#89756 = CARTESIAN_POINT ( 'NONE',  ( -46.78784730906664180, 100.7327625268226825, -9.217559165526038711 ) ) ;
#89757 = CARTESIAN_POINT ( 'NONE',  ( 10.00000000000000178, 14.31368534415483751, 10.88017736071110342 ) ) ;
#89758 = CARTESIAN_POINT ( 'NONE',  ( 17.08211943468705840, 35.13708216824730357, -12.26659068614894466 ) ) ;
#89759 = CARTESIAN_POINT ( 'NONE',  ( 10.00000000000000000, 41.81368534415484106, -10.88017736071110342 ) ) ;
#89760 = CARTESIAN_POINT ( 'NONE',  ( 2.035157376598824452, 63.68868534415484106, 7.964842623401179544 ) ) ;
#89761 = CARTESIAN_POINT ( 'NONE',  ( 18.95785429995054372, 17.24216108172007011, 6.499999999999841016 ) ) ;
#89762 = CARTESIAN_POINT ( 'NONE',  ( 19.84674366389459621, 23.50893115100078390, 7.409399052514197653E-17 ) ) ;
#89763 = CYLINDRICAL_SURFACE ( 'NONE', #40201, 0.2500000000000002220 ) ;
#89764 = CARTESIAN_POINT ( 'NONE',  ( 14.92337183194729988, 4.342264484334117824, -8.527530157486177487 ) ) ;
#89765 =( GEOMETRIC_REPRESENTATION_CONTEXT ( 3 ) GLOBAL_UNCERTAINTY_ASSIGNED_CONTEXT ( ( #32090 ) ) GLOBAL_UNIT_ASSIGNED_CONTEXT ( ( #71913, #55941, #79428 ) ) REPRESENTATION_CONTEXT ( 'NONE', 'WORKASPACE' ) );
#89766 = CARTESIAN_POINT ( 'NONE',  ( -1.266189978427564089, -7.341591041528217097E-16, 3.630449589664167753 ) ) ;
#89767 = CARTESIAN_POINT ( 'NONE',  ( 7.361572987183170547, 32.05059781766745175, 9.846743663894590881 ) ) ;
#89768 = CARTESIAN_POINT ( 'NONE',  ( 10.00000000000000000, 64.75893115100078035, -9.846743663894594434 ) ) ;
#89769 = CARTESIAN_POINT ( 'NONE',  ( 12.91533473730993009, 31.60535201082150891, -10.88017736071109987 ) ) ;
#89770 = VECTOR ( 'NONE', #61934, 1000.000000000000000 ) ;
#89771 = EDGE_LOOP ( 'NONE', ( #31948, #37354, #35840, #34609 ) ) ;
#89772 = CARTESIAN_POINT ( 'NONE',  ( 22.81628187352647785, 56.62363466993042493, 6.195893100308588602E-16 ) ) ;
#89773 = SPHERICAL_SURFACE ( 'NONE', #63618, 0.2500000000000000000 ) ;
#89774 = CARTESIAN_POINT ( 'NONE',  ( 17.20831665107776587, 14.13393115100078568, -7.208316651077762316 ) ) ;
#89775 = CARTESIAN_POINT ( 'NONE',  ( 0.6178305044545818747, 48.49863466993042493, -9.382169495545419124 ) ) ;
#89777 = CARTESIAN_POINT ( 'NONE',  ( 12.63842701281683922, 39.55059781766744464, -9.846743663894590881 ) ) ;
#89776 = CARTESIAN_POINT ( 'NONE',  ( 10.00000000000000000, 6.813685344154838397, -10.88017736071110342 ) ) ;
#89778 = CYLINDRICAL_SURFACE ( 'NONE', #56814, 15.00000000000000000 ) ;
#89779 = CARTESIAN_POINT ( 'NONE',  ( 7.361572987183169658, -0.03273551566588185635, -9.846743663894592657 ) ) ;
#89780 = CARTESIAN_POINT ( 'NONE',  ( -4.164238869374099039, 21.80374883491396787, 8.674139862899312516E-16 ) ) ;
#89781 = CARTESIAN_POINT ( 'NONE',  ( 24.16423886937410614, 49.30374883491396787, 8.672049930838204340E-16 ) ) ;
#89782 = CARTESIAN_POINT ( 'NONE',  ( 12.63842701281683922, 49.55059781766744464, -9.846743663894590881 ) ) ;
#89783 = CARTESIAN_POINT ( 'NONE',  ( 4.669717816207066718, -13.81568353606978761, -2.500000000000000888 ) ) ;
#89784 = CARTESIAN_POINT ( 'NONE',  ( 20.88017736071110875, 40.77201867748818387, -2.915334737309920765 ) ) ;
#89785 = ADVANCED_FACE ( 'NONE', ( #93039 ), #62532, .F. ) ;
#89786 = CARTESIAN_POINT ( 'NONE',  ( 12.63842701281683922, 4.550597817667451750, -9.846743663894590881 ) ) ;
#89787 = DIRECTION ( 'NONE',  ( -0.000000000000000000, -1.000000000000000000, -0.000000000000000000 ) ) ;
#89788 = VERTEX_POINT ( 'NONE', #55547 ) ;
#89789 = CARTESIAN_POINT ( 'NONE',  ( -2.816281873526473856, 64.12363466993042493, 9.499525473075851096E-16 ) ) ;
#89790 = CARTESIAN_POINT ( 'NONE',  ( 12.91533473730993009, 61.60535201082150536, -10.88017736071109987 ) ) ;
#89791 = EDGE_LOOP ( 'NONE', ( #32797, #12208, #25244, #88278, #18306, #81857 ) ) ;
#89792 = CARTESIAN_POINT ( 'NONE',  ( 20.36894250292379382, 3.678748834913967869, 10.36894250292379205 ) ) ;
#89793 = CARTESIAN_POINT ( 'NONE',  ( 5.076628168052703671, 6.842264484334118713, 8.527530157486179263 ) ) ;
#89794 = DIRECTION ( 'NONE',  ( -0.04361938736533987893, 0.000000000000000000, 0.9990482215818576872 ) ) ;
#89795 = VERTEX_POINT ( 'NONE', #8567 ) ;
#89796 = CARTESIAN_POINT ( 'NONE',  ( 17.96484262340118221, 19.93868534415484106, 7.964842623401181321 ) ) ;
#89797 = VECTOR ( 'NONE', #97846, 999.9999999999998863 ) ;
#89798 = EDGE_LOOP ( 'NONE', ( #60431, #96707, #19413, #32125, #36968, #94104 ) ) ;
#89799 = CARTESIAN_POINT ( 'NONE',  ( -0.8801773607110991993, 27.85535201082150181, -2.915334737309923874 ) ) ;
#89800 = CARTESIAN_POINT ( 'NONE',  ( 5.076628168052704559, 55.17559781766745175, -8.527530157486179263 ) ) ;
#89801 = ORIENTED_EDGE ( 'NONE', *, *, #85196, .T. ) ;
#89802 = CARTESIAN_POINT ( 'NONE',  ( 7.361572987183170547, 57.05059781766744464, 9.846743663894590881 ) ) ;
#89803 = ORIENTED_EDGE ( 'NONE', *, *, #60838, .F. ) ;
#89804 = CARTESIAN_POINT ( 'NONE',  ( 7.084665262690076126, 62.02201867748816966, -10.88017736071110164 ) ) ;
#89806 = CARTESIAN_POINT ( 'NONE',  ( 10.00000000000000000, 64.75893115100078035, -9.846743663894594434 ) ) ;
#89805 = B_SPLINE_CURVE_WITH_KNOTS ( 'NONE', 3,
 ( #80904, #20407, #73388, #33412, #94421, #25937 ),
 .UNSPECIFIED., .F., .F.,
 ( 4, 2, 4 ),
 ( 3.409110551496046665E-05, 0.0004400426677367835358, 0.0008459942299586066050 ),
 .UNSPECIFIED. ) ;
#89807 = CARTESIAN_POINT ( 'NONE',  ( -2.816281873526473856, 34.33196800326376064, 3.434112377981055619 ) ) ;
#89809 = CARTESIAN_POINT ( 'NONE',  ( 20.10384461210893292, 6.743024370107935539, 6.337995344473741355 ) ) ;
#89808 = CARTESIAN_POINT ( 'NONE',  ( 10.00000000000000000, 26.81368534415484106, -10.88017736071110342 ) ) ;
#89810 = CARTESIAN_POINT ( 'NONE',  ( 0.1532563361054082862, 6.217264484334118713, 2.638427012816831674 ) ) ;
#89811 = CARTESIAN_POINT ( 'NONE',  ( -0.8801773607111008646, 13.27201867748817321, 2.915334737309923430 ) ) ;
#89812 = AXIS2_PLACEMENT_3D ( 'NONE', #60868, #411, #84382 ) ;
#89813 = ORIENTED_EDGE ( 'NONE', *, *, #97896, .F. ) ;
#89814 = CARTESIAN_POINT ( 'NONE',  ( -1.099225684535947600, 53.70696800326376064, -6.408140936763238038 ) ) ;
#89815 = CARTESIAN_POINT ( 'NONE',  ( 15.44008868035555793, 41.39701867748817676, -9.422509992056140149 ) ) ;
#89816 = CARTESIAN_POINT ( 'NONE',  ( 14.66148682522639568, 14.76984938411481352, 2.874551585518038355 ) ) ;
#89817 = CARTESIAN_POINT ( 'NONE',  ( -2.816281873526471635, 58.91530133659707502, -3.434112377981056508 ) ) ;
#89818 = CARTESIAN_POINT ( 'NONE',  ( 0.5774900079438607392, 48.48035201082150536, 5.440088680355550821 ) ) ;
#89819 = CIRCLE ( 'NONE', #41885, 15.00000000000000000 ) ;
#89820 = TOROIDAL_SURFACE ( 'NONE', #54701, 14.49999999999999822, 0.5000000000000000000 ) ;
#89821 = CARTESIAN_POINT ( 'NONE',  ( 5.076628168052704559, 50.17559781766745886, -8.527530157486179263 ) ) ;
#89823 =( NAMED_UNIT ( * ) PLANE_ANGLE_UNIT ( ) SI_UNIT ( $, .RADIAN. ) );
#89822 = CIRCLE ( 'NONE', #49937, 11.92686044187656513 ) ;
#89824 = CARTESIAN_POINT ( 'NONE',  ( 18.52753015748618282, 18.92559781766745175, -4.923371831947291888 ) ) ;
#89825 = PRESENTATION_LAYER_ASSIGNMENT (  '', '', ( #21188 ) ) ;
#89826 = CARTESIAN_POINT ( 'NONE',  ( 22.81628187352648496, 6.831968003263753531, -3.434112377981050290 ) ) ;
#89828 = CARTESIAN_POINT ( 'NONE',  ( 0.1532563361054100626, 60.80059781766744464, -2.638427012816831230 ) ) ;
#89827 = CARTESIAN_POINT ( 'NONE',  ( -13.78969293960296305, 90.90480785988455636, -7.820272038271530057 ) ) ;
#89829 = CARTESIAN_POINT ( 'NONE',  ( 10.00000000000000178, 34.31368534415484106, 10.88017736071110342 ) ) ;
#89830 = CARTESIAN_POINT ( 'NONE',  ( 1.472469842513823179, 45.59226448433412315, -4.923371831947296329 ) ) ;
#89831 = ADVANCED_FACE ( 'NONE', ( #25551 ), #56043, .F. ) ;
#89832 = CARTESIAN_POINT ( 'NONE',  ( 0.1532563361054083140, 6.008931151000784787, 1.131784320476157264E-15 ) ) ;
#89833 = DIRECTION ( 'NONE',  ( 0.7253743710122867450, 0.000000000000000000, -0.6883545756937550220 ) ) ;
#89835 = EDGE_LOOP ( 'NONE', ( #41700, #24640, #76638, #22748, #53432, #32880 ) ) ;
#89834 = CARTESIAN_POINT ( 'NONE',  ( 0.6178305044545818747, 3.498634669930420049, -9.382169495545419124 ) ) ;
#89836 = PRESENTATION_LAYER_ASSIGNMENT (  '', '', ( #89625 ) ) ;
#89837 = CARTESIAN_POINT ( 'NONE',  ( 6.565887622018943937, 65.16530133659709634, 12.81628187352647430 ) ) ;
#89838 = DIRECTION ( 'NONE',  ( 0.000000000000000000, 0.000000000000000000, -1.000000000000000000 ) ) ;
#89839 = CARTESIAN_POINT ( 'NONE',  ( -1.099225684535947600, 33.70696800326375353, -6.408140936763238038 ) ) ;
#89840 = CARTESIAN_POINT ( 'NONE',  ( 10.00000000000000000, 34.75893115100078745, -9.846743663894594434 ) ) ;
#89841 = DIRECTION ( 'NONE',  ( -0.000000000000000000, -0.000000000000000000, -1.000000000000000000 ) ) ;
#89842 = CARTESIAN_POINT ( 'NONE',  ( 0.5774900079438590739, 12.64701867748817321, -5.440088680355550821 ) ) ;
#89843 = CARTESIAN_POINT ( 'NONE',  ( 10.00000000000000178, 32.25893115100078745, 9.846743663894594434 ) ) ;
#89844 = CARTESIAN_POINT ( 'NONE',  ( 14.49999999999999822, 11.00000000000000000, 6.500000000000000888 ) ) ;
#89845 = CARTESIAN_POINT ( 'NONE',  ( 17.96484262340118221, 4.938685344154837509, 7.964842623401181321 ) ) ;
#89846 = CARTESIAN_POINT ( 'NONE',  ( -13.34727560011345382, 90.86036091889430111, -7.765078796629374835 ) ) ;
#89847 = CARTESIAN_POINT ( 'NONE',  ( -0.8801773607111008646, 13.27201867748817321, 2.915334737309923430 ) ) ;
#89848 = CIRCLE ( 'NONE', #91426, 0.5000000000000004441 ) ;
#89849 = CARTESIAN_POINT ( 'NONE',  ( 10.00000000000000178, 53.05374883491396787, 14.16423886937410082 ) ) ;
#89851 = CARTESIAN_POINT ( 'NONE',  ( -3.115783986955356522, 15.00000000000000000, -14.16128137375399554 ) ) ;
#89850 = CARTESIAN_POINT ( 'NONE',  ( -4.164238869374098151, 46.59541550158063927, -3.795296366450310543 ) ) ;
#89852 = CARTESIAN_POINT ( 'NONE',  ( 7.684764310694797373, 14.63606916355816878, 12.88194075009944584 ) ) ;
#89853 = CARTESIAN_POINT ( 'NONE',  ( 17.20831665107776587, 12.88393115100078390, 7.208316651077764980 ) ) ;
#89854 = CARTESIAN_POINT ( 'NONE',  ( 6.565887622018943937, 3.081968003263753531, -12.81628187352647608 ) ) ;
#89855 = ORIENTED_EDGE ( 'NONE', *, *, #69035, .T. ) ;
#89856 = CARTESIAN_POINT ( 'NONE',  ( -0.1503990784575242878, 64.24884699246891273, -6.262539305110083276 ) ) ;
#89857 = DIRECTION ( 'NONE',  ( 0.000000000000000000, 1.000000000000000000, 0.000000000000000000 ) ) ;
#89858 =( BOUNDED_SURFACE ( )  B_SPLINE_SURFACE ( 1, 2, ( 
 ( #25042, #62514, #93019, #55014, #53371, #14907, #21914, #83881, #91876, #15407, #67397, #90874, #75381, #68393, #22404, #30367, #83389, #15888, #28886, #82892, #22899, #67898, #89892, #97420, #6390, #97923, #59884, #21410, #36905, #29383, #23397, #61366, #45891, #6897, #7407, #60378, #37411, #46373, #90375, #66901, #59390, #53882, #74891, #98914, #52390, #14408, #38387, #44879, #44392, #76378, #45379, #91373, #98421, #7893, #75885, #68888, #84389, #76862, #36407, #51905, #82389, #13913, #418, #30869, #29876, #52879, #37904, #60873, #4871, #73839, #57360, #73344, #3886, #87854, #35348, #5367, #72354, #35846, #65344, #50853, #51343, #12842, #50346, #74324, #96869, #66835, #66333, #97357, #81346, #28345, #79868, #43342, #95363, #12354, #95872, #80857, #26863, #72847, #18885, #20852, #19853, #58835, #42861, #4383, #96371, #89342, #80366, #19372, #81828, #13344, #65842, #11372, #20357, #27354, #5850, #28826, #27844, #49857, #36341, #34848, #58332, #11866, #88849, #43828, #59326, #49366, #41894, #34353, #42373, #64844, #57847, #88357, #83324, #91308, #53311, #68332, #69312, #61302, #30306, #8316, #355, #38820, #60808, #98852, #7833, #29320, #91813, #52816, #14850, #83819, #6834, #29815, #15345, #90312, #7340, #46313, #89829, #30804, #68823, #84325, #82324, #833, #22836, #37841, #98357, #45827, #21346, #23334, #76315, #82822, #60324, #21848, #44326, #31293, #90814, #51837, #13844, #59817, #75819, #22343, #38329, #74827, #53814, #15825, #14342, #45321, #52329, #6331, #36843, #76800, #67331, #97857, #44814, #75321, #37348, #67839, #84803, #78779, #40290, #94258, #54781, #48757, #70798, #9791, #69810, #79265, #24316, #2807, #63753, #16805, #93280, #47779, #17791, #1332, #17304, #46796, #31784, #78277, #48266, #16312, #10285, #9294, #93774, #25785, #55787, #24804, #18277, #40785, #10775, #71284, #41291, #25300, #33262, #23826, #86282, #39315, #55281, #39802, #85790, #62279, #47280, #61793, #56280, #62781, #86776, #2315, #77782, #32769, #71765, #85297, #92785, #3275, #92301, #63265, #54289, #77289, #70303, #8800, #1817, #32273, #3778, #20736, #87739, #65224, #34231, #34733, #19742, #65724, #88233, #89227, #96250, #64728, #88727, #27729, #18775, #27235, #35225, #58210, #12236, #13225, #5252, #73226, #51228, #43225, #81712, #4754, #42744, #50742, #72244, #35730, #95751, #57730, #20238, #49735, #72728, #81231, #95238, #50226, #43722, #33738, #73720, #12729, #28224, #26258, #74207, #66218, #80741, #11255, #96749, #58723, #64240, #26746, #94758, #56755, #87249, #57241, #49258, #79757, #41773, #19251, #80243, #11750, #42258, #4262, #7721 ),
 ( #67223, #44208, #91193, #45702, #29697, #97250, #7218, #52216, #61191, #53689, #83211, #74717, #91697, #59708, #37234, #6229, #6718, #90701, #37718, #60206, #23216, #68222, #36732, #60693, #98742, #89714, #98236, #30192, #22718, #14732, #84208, #76202, #45208, #15715, #15223, #46201, #75707, #53202, #83706, #97746, #38218, #67723, #22229, #68703, #21735, #44708, #235, #29209, #52705, #5739, #36226, #30683, #66726, #28720, #59210, #21228, #51732, #82213, #14229, #13724, #90204, #82711, #75207, #69684, #85178, #77176, #31178, #94143, #47159, #18162, #76685, #16197, #62657, #16689, #17677, #724, #93654, #55156, #10170, #1215, #63636, #85670, #24685, #84686, #25671, #39196, #48151, #78664, #31670, #9177, #93160, #32658, #46678, #32156, #61670, #8683, #17189, #63151, #92188, #25188, #24194, #56165, #86167, #86657, #47670, #78164, #55668, #62160, #40667, #39695, #1699, #40172, #92667, #77663, #2196, #54662, #9674, #33141, #8205, #71165, #2690, #38700, #69199, #23714, #70676, #54175, #70183, #19624, #48640, #88604, #50118, #41659, #57124, #49139, #3162, #66099, #19136, #89106, #79143, #87129, #34611, #87622, #20114, #71654, #65603, #27117, #81109, #72127, #35613, #57616, #95628, #56644, #96628, #11140, #50618, #12610, #3654, #80124, #65107, #4641, #18650, #4146, #33624, #79641, #88115, #35105, #64124, #96131, #95119, #80628, #43111, #42624, #11631, #5125, #27612, #28103, #58098, #58605, #12122, #73598, #10655, #73102, #26150, #42147, #26627, #72611, #34119, #64611, #41170, #94640, #49613, #75587, #82592, #6109, #98111, #68095, #82094, #59093, #7099, #60581, #44591, #13107, #22104, #67101, #76075, #68588, #29573, #89602, #7605, #74595, #52099, #21112, #21614, #6595, #52584, #75089, #38101, #83087, #51611, #37601, #14615, #5623, #14107, #45082, #98623, #60076, #118, #91073, #90578, #30072, #22599, #90087, #81595, #67604, #53077, #30565, #83588, #15105, #37108, #28604, #61070, #13605, #59588, #43602, #45581, #74089, #97134, #20618, #51108, #36099, #44085, #66606, #36614, #97626, #29089, #71422, #23098, #86899, #41429, #87390, #24939, #70932, #49384, #94889, #55421, #63884, #26387, #94396, #33386, #93910, #18409, #25911, #56413, #71890, #93416, #41914, #72376, #64379, #16936, #32414, #3413, #2449, #11392, #18907, #32906, #63405, #47417, #9929, #55921, #9426, #40924, #33874, #2938, #48405, #25438, #34373, #78908, #48892, #10907, #85929, #86420, #17921, #10417, #56887, #79403, #78411, #79885, #3906, #91581, #17439, #53568, #85427, #77920, #39930, #70433, #1950, #62915, #47906, #40433, #51361, #96389, #19388, #26885, #34870, #95893 ) ),
 .UNSPECIFIED., .F., .F., .T. ) 
 B_SPLINE_SURFACE_WITH_KNOTS ( ( 2, 2 ),
 ( 3, 2, 2, 2, 2, 2, 2, 2, 2, 2, 2, 2, 2, 2, 2, 2, 2, 2, 2, 2, 2, 2, 2, 2, 2, 2, 2, 2, 2, 2, 2, 2, 2, 2, 2, 2, 2, 2, 2, 2, 2, 2, 2, 2, 2, 2, 2, 2, 2, 2, 2, 2, 2, 2, 2, 2, 2, 2, 2, 2, 2, 2, 2, 2, 2, 2, 2, 2, 2, 2, 2, 2, 2, 2, 2, 2, 2, 2, 2, 2, 2, 2, 2, 2, 2, 2, 2, 2, 2, 2, 2, 2, 2, 2, 2, 2, 2, 2, 2, 2, 2, 2, 2, 2, 2, 2, 2, 2, 2, 2, 2, 2, 2, 2, 2, 2, 2, 2, 2, 2, 2, 2, 2, 2, 2, 2, 2, 2, 2, 2, 2, 2, 2, 2, 2, 2, 2, 2, 2, 2, 2, 2, 2, 2, 2, 2, 2, 2, 2, 2, 2, 2, 2, 2, 2, 2, 2, 2, 2, 2, 2, 2, 3 ),
 ( 0.000000000000000000, 1.000000000000000000 ),
 ( 0.000000000000000000, 0.005952380952380952051, 0.01190476190476190410, 0.01785714285714285615, 0.02380952380952380820, 0.02976190476190476025, 0.03571428571428571230, 0.04166666666666666435, 0.04761904761904761640, 0.05357142857142856845, 0.05952380952380952051, 0.06547619047619047949, 0.07142857142857142461, 0.07738095238095238360, 0.08333333333333332871, 0.08928571428571428770, 0.09523809523809523281, 0.1011904761904761918, 0.1071428571428571369, 0.1130952380952380959, 0.1190476190476190410, 0.1250000000000000000, 0.1309523809523809590, 0.1369047619047619180, 0.1428571428571428492, 0.1488095238095238082, 0.1547619047619047672, 0.1607142857142857262, 0.1666666666666666574, 0.1726190476190476164, 0.1785714285714285754, 0.1845238095238095344, 0.1904761904761904656, 0.1964285714285714246, 0.2023809523809523836, 0.2083333333333333426, 0.2142857142857142738, 0.2202380952380952328, 0.2261904761904761918, 0.2321428571428571508, 0.2380952380952380820, 0.2440476190476190410, 0.2500000000000000000, 0.2559523809523809312, 0.2619047619047619180, 0.2678571428571428492, 0.2738095238095238360, 0.2797619047619047672, 0.2857142857142856984, 0.2916666666666666852, 0.2976190476190476164, 0.3035714285714285476, 0.3095238095238095344, 0.3154761904761904656, 0.3214285714285714524, 0.3273809523809523836, 0.3333333333333333148, 0.3392857142857143016, 0.3452380952380952328, 0.3511904761904761640, 0.3571428571428571508, 0.3630952380952380820, 0.3690476190476190688, 0.3750000000000000000, 0.3809523809523809312, 0.3869047619047619180, 0.3928571428571428492, 0.3988095238095238360, 0.4047619047619047672, 0.4107142857142856984, 0.4166666666666666852, 0.4226190476190476164, 0.4285714285714285476, 0.4345238095238095344, 0.4404761904761904656, 0.4464285714285714524, 0.4523809523809523836, 0.4583333333333333148, 0.4642857142857143016, 0.4702380952380952328, 0.4761904761904761640, 0.4821428571428571508, 0.4880952380952380820, 0.4940476190476190688, 0.5000000000000000000, 0.5059523809523809312, 0.5119047619047618625, 0.5178571428571429047, 0.5238095238095238360, 0.5297619047619047672, 0.5357142857142856984, 0.5416666666666666297, 0.5476190476190476719, 0.5535714285714286031, 0.5595238095238095344, 0.5654761904761904656, 0.5714285714285713969, 0.5773809523809523281, 0.5833333333333333703, 0.5892857142857143016, 0.5952380952380952328, 0.6011904761904761640, 0.6071428571428570953, 0.6130952380952381375, 0.6190476190476190688, 0.6250000000000000000, 0.6309523809523809312, 0.6369047619047618625, 0.6428571428571429047, 0.6488095238095238360, 0.6547619047619047672, 0.6607142857142856984, 0.6666666666666666297, 0.6726190476190476719, 0.6785714285714286031, 0.6845238095238095344, 0.6904761904761904656, 0.6964285714285713969, 0.7023809523809523281, 0.7083333333333333703, 0.7142857142857143016, 0.7202380952380952328, 0.7261904761904761640, 0.7321428571428570953, 0.7380952380952381375, 0.7440476190476190688, 0.7500000000000000000, 0.7559523809523809312, 0.7619047619047618625, 0.7678571428571429047, 0.7738095238095238360, 0.7797619047619047672, 0.7857142857142856984, 0.7916666666666666297, 0.7976190476190476719, 0.8035714285714286031, 0.8095238095238095344, 0.8154761904761904656, 0.8214285714285713969, 0.8273809523809523281, 0.8333333333333333703, 0.8392857142857143016, 0.8452380952380952328, 0.8511904761904761640, 0.8571428571428570953, 0.8630952380952381375, 0.8690476190476190688, 0.8750000000000000000, 0.8809523809523809312, 0.8869047619047618625, 0.8928571428571429047, 0.8988095238095238360, 0.9047619047619047672, 0.9107142857142856984, 0.9166666666666666297, 0.9226190476190476719, 0.9285714285714286031, 0.9345238095238095344, 0.9404761904761904656, 0.9464285714285713969, 0.9523809523809523281, 0.9583333333333333703, 0.9642857142857143016 ),
 .UNSPECIFIED. ) 
 GEOMETRIC_REPRESENTATION_ITEM ( )  RATIONAL_B_SPLINE_SURFACE ( (
 ( 1.000000000000000000, 0.9659258262890683122, 1.000000000000000000, 0.9659258262890683122, 1.000000000000000000, 0.9659258262890683122, 1.000000000000000000, 0.9659258262890683122, 1.000000000000000000, 0.9659258262890683122, 1.000000000000000000, 0.9659258262890683122, 1.000000000000000000, 0.9659258262890683122, 1.000000000000000000, 0.9659258262890683122, 1.000000000000000000, 0.9659258262890683122, 1.000000000000000000, 0.9659258262890683122, 1.000000000000000000, 0.9659258262890683122, 1.000000000000000000, 0.9659258262890683122, 1.000000000000000000, 0.9659258262890683122, 1.000000000000000000, 0.9659258262890683122, 1.000000000000000000, 0.9659258262890683122, 1.000000000000000000, 0.9659258262890683122, 1.000000000000000000, 0.9659258262890683122, 1.000000000000000000, 0.9659258262890683122, 1.000000000000000000, 0.9659258262890683122, 1.000000000000000000, 0.9659258262890683122, 1.000000000000000000, 0.9659258262890683122, 1.000000000000000000, 0.9659258262890683122, 1.000000000000000000, 0.9659258262890683122, 1.000000000000000000, 0.9659258262890683122, 1.000000000000000000, 0.9659258262890683122, 1.000000000000000000, 0.9659258262890683122, 1.000000000000000000, 0.9659258262890683122, 1.000000000000000000, 0.9659258262890683122, 1.000000000000000000, 0.9659258262890683122, 1.000000000000000000, 0.9659258262890683122, 1.000000000000000000, 0.9659258262890683122, 1.000000000000000000, 0.9659258262890683122, 1.000000000000000000, 0.9659258262890683122, 1.000000000000000000, 0.9659258262890683122, 1.000000000000000000, 0.9659258262890683122, 1.000000000000000000, 0.9659258262890683122, 1.000000000000000000, 0.9659258262890683122, 1.000000000000000000, 0.9659258262890683122, 1.000000000000000000, 0.9659258262890683122, 1.000000000000000000, 0.9659258262890683122, 1.000000000000000000, 0.9659258262890683122, 1.000000000000000000, 0.9659258262890683122, 1.000000000000000000, 0.9659258262890683122, 1.000000000000000000, 0.9659258262890683122, 1.000000000000000000, 0.9659258262890683122, 1.000000000000000000, 0.9659258262890683122, 1.000000000000000000, 0.9659258262890683122, 1.000000000000000000, 0.9659258262890683122, 1.000000000000000000, 0.9659258262890683122, 1.000000000000000000, 0.9659258262890683122, 1.000000000000000000, 0.9659258262890683122, 1.000000000000000000, 0.9659258262890683122, 1.000000000000000000, 0.9659258262890683122, 1.000000000000000000, 0.9659258262890683122, 1.000000000000000000, 0.9659258262890683122, 1.000000000000000000, 0.9659258262890683122, 1.000000000000000000, 0.9659258262890683122, 1.000000000000000000, 0.9659258262890683122, 1.000000000000000000, 0.9659258262890683122, 1.000000000000000000, 0.9659258262890683122, 1.000000000000000000, 0.9659258262890683122, 1.000000000000000000, 0.9659258262890683122, 1.000000000000000000, 0.9659258262890683122, 1.000000000000000000, 0.9659258262890683122, 1.000000000000000000, 0.9659258262890683122, 1.000000000000000000, 0.9659258262890683122, 1.000000000000000000, 0.9659258262890683122, 1.000000000000000000, 0.9659258262890683122, 1.000000000000000000, 0.9659258262890683122, 1.000000000000000000, 0.9659258262890683122, 1.000000000000000000, 0.9659258262890683122, 1.000000000000000000, 0.9659258262890683122, 1.000000000000000000, 0.9659258262890683122, 1.000000000000000000, 0.9659258262890683122, 1.000000000000000000, 0.9659258262890683122, 1.000000000000000000, 0.9659258262890683122, 1.000000000000000000, 0.9659258262890683122, 1.000000000000000000, 0.9659258262890683122, 1.000000000000000000, 0.9659258262890683122, 1.000000000000000000, 0.9659258262890683122, 1.000000000000000000, 0.9659258262890683122, 1.000000000000000000, 0.9659258262890683122, 1.000000000000000000, 0.9659258262890683122, 1.000000000000000000, 0.9659258262890683122, 1.000000000000000000, 0.9659258262890683122, 1.000000000000000000, 0.9659258262890683122, 1.000000000000000000, 0.9659258262890683122, 1.000000000000000000, 0.9659258262890683122, 1.000000000000000000, 0.9659258262890683122, 1.000000000000000000, 0.9659258262890683122, 1.000000000000000000, 0.9659258262890683122, 1.000000000000000000, 0.9659258262890683122, 1.000000000000000000, 0.9659258262890683122, 1.000000000000000000, 0.9659258262890683122, 1.000000000000000000, 0.9659258262890683122, 1.000000000000000000, 0.9659258262890683122, 1.000000000000000000, 0.9659258262890683122, 1.000000000000000000, 0.9659258262890683122, 1.000000000000000000, 0.9659258262890683122, 1.000000000000000000, 0.9659258262890683122, 1.000000000000000000, 0.9659258262890683122, 1.000000000000000000, 0.9659258262890683122, 1.000000000000000000, 0.9659258262890683122, 1.000000000000000000, 0.9659258262890683122, 1.000000000000000000, 0.9659258262890683122, 1.000000000000000000, 0.9659258262890683122, 1.000000000000000000, 0.9659258262890683122, 1.000000000000000000, 0.9659258262890683122, 1.000000000000000000, 0.9659258262890683122, 1.000000000000000000, 0.9659258262890683122, 1.000000000000000000, 0.9659258262890683122, 1.000000000000000000, 0.9659258262890683122, 1.000000000000000000, 0.9659258262890683122, 1.000000000000000000, 0.9659258262890683122, 1.000000000000000000, 0.9659258262890683122, 1.000000000000000000, 0.9659258262890683122, 1.000000000000000000, 0.9659258262890683122, 1.000000000000000000, 0.9659258262890683122, 1.000000000000000000, 0.9659258262890683122, 1.000000000000000000, 0.9659258262890683122, 1.000000000000000000, 0.9659258262890683122, 1.000000000000000000, 0.9659258262890683122, 1.000000000000000000, 0.9659258262890683122, 1.000000000000000000, 0.9659258262890683122, 1.000000000000000000, 0.9659258262890683122, 1.000000000000000000, 0.9659258262890683122, 1.000000000000000000, 0.9659258262890683122, 1.000000000000000000, 0.9659258262890683122, 1.000000000000000000, 0.9659258262890683122, 1.000000000000000000, 0.9659258262890683122, 1.000000000000000000, 0.9659258262890683122, 1.000000000000000000, 0.9659258262890683122, 1.000000000000000000, 0.9659258262890683122, 1.000000000000000000, 0.9659258262890683122, 1.000000000000000000, 0.9659258262890683122, 1.000000000000000000, 0.9659258262890683122, 1.000000000000000000, 0.9659258262890683122, 1.000000000000000000, 0.9659258262890683122, 1.000000000000000000, 0.9659258262890683122, 1.000000000000000000, 0.9659258262890683122, 1.000000000000000000, 0.9659258262890683122, 1.000000000000000000, 0.9659258262890683122, 1.000000000000000000, 0.9659258262890683122, 1.000000000000000000, 0.9659258262890683122, 1.000000000000000000, 0.9659258262890683122, 1.000000000000000000, 0.9659258262890683122, 1.000000000000000000, 0.9659258262890683122, 1.000000000000000000, 0.9659258262890683122, 1.000000000000000000, 0.9659258262890683122, 1.000000000000000000, 0.9659258262890683122, 1.000000000000000000, 0.9659258262890683122, 1.000000000000000000, 0.9659258262890683122, 1.000000000000000000, 0.9659258262890683122, 1.000000000000000000, 0.9659258262890683122, 1.000000000000000000, 0.9659258262890683122, 1.000000000000000000, 0.9659258262890683122, 1.000000000000000000, 0.9659258262890683122, 1.000000000000000000, 0.9659258262890683122, 1.000000000000000000, 0.9659258262890683122, 1.000000000000000000, 0.9659258262890683122, 1.000000000000000000, 0.9659258262890683122, 1.000000000000000000, 0.9659258262890683122, 1.000000000000000000),
 ( 1.000000000000000000, 0.9659258262890683122, 1.000000000000000000, 0.9659258262890683122, 1.000000000000000000, 0.9659258262890683122, 1.000000000000000000, 0.9659258262890683122, 1.000000000000000000, 0.9659258262890683122, 1.000000000000000000, 0.9659258262890683122, 1.000000000000000000, 0.9659258262890683122, 1.000000000000000000, 0.9659258262890683122, 1.000000000000000000, 0.9659258262890683122, 1.000000000000000000, 0.9659258262890683122, 1.000000000000000000, 0.9659258262890683122, 1.000000000000000000, 0.9659258262890683122, 1.000000000000000000, 0.9659258262890683122, 1.000000000000000000, 0.9659258262890683122, 1.000000000000000000, 0.9659258262890683122, 1.000000000000000000, 0.9659258262890683122, 1.000000000000000000, 0.9659258262890683122, 1.000000000000000000, 0.9659258262890683122, 1.000000000000000000, 0.9659258262890683122, 1.000000000000000000, 0.9659258262890683122, 1.000000000000000000, 0.9659258262890683122, 1.000000000000000000, 0.9659258262890683122, 1.000000000000000000, 0.9659258262890683122, 1.000000000000000000, 0.9659258262890683122, 1.000000000000000000, 0.9659258262890683122, 1.000000000000000000, 0.9659258262890683122, 1.000000000000000000, 0.9659258262890683122, 1.000000000000000000, 0.9659258262890683122, 1.000000000000000000, 0.9659258262890683122, 1.000000000000000000, 0.9659258262890683122, 1.000000000000000000, 0.9659258262890683122, 1.000000000000000000, 0.9659258262890683122, 1.000000000000000000, 0.9659258262890683122, 1.000000000000000000, 0.9659258262890683122, 1.000000000000000000, 0.9659258262890683122, 1.000000000000000000, 0.9659258262890683122, 1.000000000000000000, 0.9659258262890683122, 1.000000000000000000, 0.9659258262890683122, 1.000000000000000000, 0.9659258262890683122, 1.000000000000000000, 0.9659258262890683122, 1.000000000000000000, 0.9659258262890683122, 1.000000000000000000, 0.9659258262890683122, 1.000000000000000000, 0.9659258262890683122, 1.000000000000000000, 0.9659258262890683122, 1.000000000000000000, 0.9659258262890683122, 1.000000000000000000, 0.9659258262890683122, 1.000000000000000000, 0.9659258262890683122, 1.000000000000000000, 0.9659258262890683122, 1.000000000000000000, 0.9659258262890683122, 1.000000000000000000, 0.9659258262890683122, 1.000000000000000000, 0.9659258262890683122, 1.000000000000000000, 0.9659258262890683122, 1.000000000000000000, 0.9659258262890683122, 1.000000000000000000, 0.9659258262890683122, 1.000000000000000000, 0.9659258262890683122, 1.000000000000000000, 0.9659258262890683122, 1.000000000000000000, 0.9659258262890683122, 1.000000000000000000, 0.9659258262890683122, 1.000000000000000000, 0.9659258262890683122, 1.000000000000000000, 0.9659258262890683122, 1.000000000000000000, 0.9659258262890683122, 1.000000000000000000, 0.9659258262890683122, 1.000000000000000000, 0.9659258262890683122, 1.000000000000000000, 0.9659258262890683122, 1.000000000000000000, 0.9659258262890683122, 1.000000000000000000, 0.9659258262890683122, 1.000000000000000000, 0.9659258262890683122, 1.000000000000000000, 0.9659258262890683122, 1.000000000000000000, 0.9659258262890683122, 1.000000000000000000, 0.9659258262890683122, 1.000000000000000000, 0.9659258262890683122, 1.000000000000000000, 0.9659258262890683122, 1.000000000000000000, 0.9659258262890683122, 1.000000000000000000, 0.9659258262890683122, 1.000000000000000000, 0.9659258262890683122, 1.000000000000000000, 0.9659258262890683122, 1.000000000000000000, 0.9659258262890683122, 1.000000000000000000, 0.9659258262890683122, 1.000000000000000000, 0.9659258262890683122, 1.000000000000000000, 0.9659258262890683122, 1.000000000000000000, 0.9659258262890683122, 1.000000000000000000, 0.9659258262890683122, 1.000000000000000000, 0.9659258262890683122, 1.000000000000000000, 0.9659258262890683122, 1.000000000000000000, 0.9659258262890683122, 1.000000000000000000, 0.9659258262890683122, 1.000000000000000000, 0.9659258262890683122, 1.000000000000000000, 0.9659258262890683122, 1.000000000000000000, 0.9659258262890683122, 1.000000000000000000, 0.9659258262890683122, 1.000000000000000000, 0.9659258262890683122, 1.000000000000000000, 0.9659258262890683122, 1.000000000000000000, 0.9659258262890683122, 1.000000000000000000, 0.9659258262890683122, 1.000000000000000000, 0.9659258262890683122, 1.000000000000000000, 0.9659258262890683122, 1.000000000000000000, 0.9659258262890683122, 1.000000000000000000, 0.9659258262890683122, 1.000000000000000000, 0.9659258262890683122, 1.000000000000000000, 0.9659258262890683122, 1.000000000000000000, 0.9659258262890683122, 1.000000000000000000, 0.9659258262890683122, 1.000000000000000000, 0.9659258262890683122, 1.000000000000000000, 0.9659258262890683122, 1.000000000000000000, 0.9659258262890683122, 1.000000000000000000, 0.9659258262890683122, 1.000000000000000000, 0.9659258262890683122, 1.000000000000000000, 0.9659258262890683122, 1.000000000000000000, 0.9659258262890683122, 1.000000000000000000, 0.9659258262890683122, 1.000000000000000000, 0.9659258262890683122, 1.000000000000000000, 0.9659258262890683122, 1.000000000000000000, 0.9659258262890683122, 1.000000000000000000, 0.9659258262890683122, 1.000000000000000000, 0.9659258262890683122, 1.000000000000000000, 0.9659258262890683122, 1.000000000000000000, 0.9659258262890683122, 1.000000000000000000, 0.9659258262890683122, 1.000000000000000000, 0.9659258262890683122, 1.000000000000000000, 0.9659258262890683122, 1.000000000000000000, 0.9659258262890683122, 1.000000000000000000, 0.9659258262890683122, 1.000000000000000000, 0.9659258262890683122, 1.000000000000000000, 0.9659258262890683122, 1.000000000000000000, 0.9659258262890683122, 1.000000000000000000, 0.9659258262890683122, 1.000000000000000000, 0.9659258262890683122, 1.000000000000000000, 0.9659258262890683122, 1.000000000000000000, 0.9659258262890683122, 1.000000000000000000, 0.9659258262890683122, 1.000000000000000000, 0.9659258262890683122, 1.000000000000000000, 0.9659258262890683122, 1.000000000000000000, 0.9659258262890683122, 1.000000000000000000, 0.9659258262890683122, 1.000000000000000000, 0.9659258262890683122, 1.000000000000000000, 0.9659258262890683122, 1.000000000000000000, 0.9659258262890683122, 1.000000000000000000, 0.9659258262890683122, 1.000000000000000000, 0.9659258262890683122, 1.000000000000000000, 0.9659258262890683122, 1.000000000000000000, 0.9659258262890683122, 1.000000000000000000, 0.9659258262890683122, 1.000000000000000000, 0.9659258262890683122, 1.000000000000000000, 0.9659258262890683122, 1.000000000000000000, 0.9659258262890683122, 1.000000000000000000, 0.9659258262890683122, 1.000000000000000000, 0.9659258262890683122, 1.000000000000000000, 0.9659258262890683122, 1.000000000000000000, 0.9659258262890683122, 1.000000000000000000, 0.9659258262890683122, 1.000000000000000000, 0.9659258262890683122, 1.000000000000000000, 0.9659258262890683122, 1.000000000000000000, 0.9659258262890683122, 1.000000000000000000, 0.9659258262890683122, 1.000000000000000000, 0.9659258262890683122, 1.000000000000000000, 0.9659258262890683122, 1.000000000000000000, 0.9659258262890683122, 1.000000000000000000, 0.9659258262890683122, 1.000000000000000000, 0.9659258262890683122, 1.000000000000000000, 0.9659258262890683122, 1.000000000000000000, 0.9659258262890683122, 1.000000000000000000, 0.9659258262890683122, 1.000000000000000000) ) ) 
 REPRESENTATION_ITEM ( '' )  SURFACE ( )  );
#89859 = DIRECTION ( 'NONE',  ( 1.000000000000000000, 0.000000000000000000, 0.000000000000000000 ) ) ;
#89860 = CARTESIAN_POINT ( 'NONE',  ( -2.266590686148945544, 1.387082168247301128, -7.082119434687050408 ) ) ;
#89861 = MECHANICAL_DESIGN_GEOMETRIC_PRESENTATION_REPRESENTATION (  '', ( #16438 ), #29192 ) ;
#89862 = CARTESIAN_POINT ( 'NONE',  ( 5.076628168052704559, 25.17559781766745175, -8.527530157486179263 ) ) ;
#89863 = EDGE_CURVE ( 'NONE', #31758, #9043, #92542, .T. ) ;
#89864 = CARTESIAN_POINT ( 'NONE',  ( -8.606322355891206755, 3.940577227621431661E-16, -11.66967075398818743 ) ) ;
#89865 = ORIENTED_EDGE ( 'NONE', *, *, #97611, .F. ) ;
#89866 = CARTESIAN_POINT ( 'NONE',  ( 10.00000000000000000, 35.55374883491396787, -14.16423886937410082 ) ) ;
#89867 = CARTESIAN_POINT ( 'NONE',  ( 18.52753015748617571, 8.092264484334117824, 4.923371831947298993 ) ) ;
#89869 = CARTESIAN_POINT ( 'NONE',  ( -5.624999999999997335, 8.755135511184874986, 9.742785792574938597 ) ) ;
#89868 = CARTESIAN_POINT ( 'NONE',  ( -0.03932841506541356197, 63.12161441960502373, 6.397827110479011203 ) ) ;
#89870 = CARTESIAN_POINT ( 'NONE',  ( -0.8801773607111008646, 33.27201867748817676, 2.915334737309923430 ) ) ;
#89871 = CARTESIAN_POINT ( 'NONE',  ( 3.591859063236761518, 39.95696800326375353, 11.09922568453594849 ) ) ;
#89872 = ADVANCED_FACE ( 'NONE', ( #32028 ), #55032, .T. ) ;
#89873 = SURFACE_SIDE_STYLE ('',( #28865 ) ) ;
#89874 = CARTESIAN_POINT ( 'NONE',  ( 19.38216949554541202, 40.99863466993042493, 9.382169495545424454 ) ) ;
#89875 = CARTESIAN_POINT ( 'NONE',  ( 10.00000000000000000, 62.87363466993042493, -12.81628187352647608 ) ) ;
#89876 = ORIENTED_EDGE ( 'NONE', *, *, #49595, .F. ) ;
#89877 = DIRECTION ( 'NONE',  ( 0.5664062369248205053, 0.000000000000000000, 0.8241261886220241362 ) ) ;
#89878 = CARTESIAN_POINT ( 'NONE',  ( -3.836325488035988052, 15.00000000000000000, -14.50112432709427424 ) ) ;
#89879 = CARTESIAN_POINT ( 'NONE',  ( -4.164238869374099927, 47.01208216824729647, 3.795296366450308767 ) ) ;
#89880 = CARTESIAN_POINT ( 'NONE',  ( 12.91533473730993009, 26.60535201082150536, -10.88017736071109987 ) ) ;
#89881 = DIRECTION ( 'NONE',  ( 0.000000000000000000, -1.000000000000000000, 0.000000000000000000 ) ) ;
#89882 = DIRECTION ( 'NONE',  ( 0.3338068592337776197, 0.000000000000000000, -0.9426414910921760981 ) ) ;
#89883 = CARTESIAN_POINT ( 'NONE',  ( 4.559911319644449179, 53.89701867748817676, 9.422509992056141925 ) ) ;
#89884 = CARTESIAN_POINT ( 'NONE',  ( 19.42250999205614193, 55.14701867748817676, 5.440088680355555262 ) ) ;
#89885 = CARTESIAN_POINT ( 'NONE',  ( 13.43411237798106583, 7.665301336597086568, -12.81628187352647252 ) ) ;
#89886 = DIRECTION ( 'NONE',  ( -0.4461978131098131573, 0.000000000000000000, 0.8949343616020228875 ) ) ;
#89887 = DIRECTION ( 'NONE',  ( -0.000000000000000000, -0.000000000000000000, -1.000000000000000000 ) ) ;
#89888 = CARTESIAN_POINT ( 'NONE',  ( 18.52753015748617571, 23.09226448433411960, 4.923371831947298993 ) ) ;
#89889 = CARTESIAN_POINT ( 'NONE',  ( 0.5774900079438607392, 63.48035201082149825, 5.440088680355550821 ) ) ;
#89890 = CARTESIAN_POINT ( 'NONE',  ( 22.81628187352647785, 16.62363466993042138, 6.195893100308588602E-16 ) ) ;
#89891 = CARTESIAN_POINT ( 'NONE',  ( 0.000000000000000000, 0.5000000000000004441, 0.000000000000000000 ) ) ;
#89892 = CARTESIAN_POINT ( 'NONE',  ( 15.44008868035555793, 6.397018677488170546, -9.422509992056140149 ) ) ;
#89893 = CARTESIAN_POINT ( 'NONE',  ( 10.00000000000000000, 44.75893115100078745, -9.846743663894594434 ) ) ;
#89894 = CARTESIAN_POINT ( 'NONE',  ( 21.09922568453595559, 42.04030133659708213, -6.408140936763230044 ) ) ;
#89895 = TOROIDAL_SURFACE ( 'NONE', #49925, 62.00000000000000000, 0.5000000000000000000 ) ;
#89896 = CARTESIAN_POINT ( 'NONE',  ( 5.076628168052703671, 21.84226448433411960, 8.527530157486179263 ) ) ;
#89897 = STYLED_ITEM ( 'NONE', ( #23844 ), #49642 ) ;
#89898 = CARTESIAN_POINT ( 'NONE',  ( -0.3689425029237898834, 11.17874883491396787, -10.36894250292378850 ) ) ;
#89899 = CARTESIAN_POINT ( 'NONE',  ( -2.913501739333859586, 15.00000000000000000, 14.20427779279530434 ) ) ;
#89900 = CARTESIAN_POINT ( 'NONE',  ( -0.8801773607111009756, 23.06368534415484106, 1.068504757029289695E-15 ) ) ;
#89902 = CARTESIAN_POINT ( 'NONE',  ( 6.204703633549690345, 32.84541550158063927, 14.16423886937410082 ) ) ;
#89901 = CARTESIAN_POINT ( 'NONE',  ( -10.93781366033354097, 0.5000000000000004441, 10.26470809774057713 ) ) ;
#89903 = CARTESIAN_POINT ( 'NONE',  ( 17.20831665107776587, 49.13393115100078745, -7.208316651077762316 ) ) ;
#89904 = CIRCLE ( 'NONE', #11678, 0.2500000000000002220 ) ;
#89905 = CARTESIAN_POINT ( 'NONE',  ( 19.42250999205614548, 25.98035201082150891, -5.440088680355545492 ) ) ;
#89906 = CARTESIAN_POINT ( 'NONE',  ( -0.8801773607110991993, 17.85535201082150536, -2.915334737309923874 ) ) ;
#89907 = VERTEX_POINT ( 'NONE', #11508 ) ;
#89908 =( GEOMETRIC_REPRESENTATION_CONTEXT ( 3 ) GLOBAL_UNCERTAINTY_ASSIGNED_CONTEXT ( ( #92225 ) ) GLOBAL_UNIT_ASSIGNED_CONTEXT ( ( #8539, #17528, #76534 ) ) REPRESENTATION_CONTEXT ( 'NONE', 'WORKASPACE' ) );
#89909 = CARTESIAN_POINT ( 'NONE',  ( 10.00000000000000178, 29.31368534415483751, 10.88017736071110342 ) ) ;
#89910 = CARTESIAN_POINT ( 'NONE',  ( -2.816281873526473856, 49.12363466993042493, 9.499525473075851096E-16 ) ) ;
#89911 = CARTESIAN_POINT ( 'NONE',  ( 19.42250999205614193, 35.14701867748816966, 5.440088680355555262 ) ) ;
#89912 = CARTESIAN_POINT ( 'NONE',  ( 20.88017736071110164, 35.35535201082150536, 2.915334737309930979 ) ) ;
#89913 = VERTEX_POINT ( 'NONE', #43477 ) ;
#89914 = CARTESIAN_POINT ( 'NONE',  ( 5.076628168052704559, 55.17559781766745175, -8.527530157486179263 ) ) ;
#89915 = CARTESIAN_POINT ( 'NONE',  ( 0.5774900079438590739, 37.64701867748817676, -5.440088680355550821 ) ) ;
#89916 = CARTESIAN_POINT ( 'NONE',  ( 4.395886034088992034, -0.8422402087801302839, 4.000000000000000000 ) ) ;
#89917 = DIRECTION ( 'NONE',  ( 1.000000000000000000, 0.000000000000000000, 0.000000000000000000 ) ) ;
#89918 =( NAMED_UNIT ( * ) PLANE_ANGLE_UNIT ( ) SI_UNIT ( $, .RADIAN. ) );
#89919 = CARTESIAN_POINT ( 'NONE',  ( 2.603489959281613420, 60.43575266056826933, -6.500000000000031086 ) ) ;
#89920 = CARTESIAN_POINT ( 'NONE',  ( -0.3689425029237898834, 51.17874883491397497, -10.36894250292378850 ) ) ;
#89921 = CARTESIAN_POINT ( 'NONE',  ( 20.88017736071110875, 55.77201867748816966, -2.915334737309920765 ) ) ;
#89922 = CARTESIAN_POINT ( 'NONE',  ( 17.39651004071841456, 49.08210964143329136, -6.500000000000001776 ) ) ;
#89923 = CARTESIAN_POINT ( 'NONE',  ( 14.97653319723437626, -0.03417435944610275333, 5.619684139539351975 ) ) ;
#89924 = CARTESIAN_POINT ( 'NONE',  ( 19.84674366389459621, 58.50893115100078745, 7.409399052514197653E-17 ) ) ;
#89925 = CARTESIAN_POINT ( 'NONE',  ( 18.52753015748617571, 23.09226448433411960, 4.923371831947298993 ) ) ;
#89926 = ORIENTED_EDGE ( 'NONE', *, *, #1499, .T. ) ;
#89927 = CARTESIAN_POINT ( 'NONE',  ( 12.63842701281683034, 17.46726448433411250, 9.846743663894596210 ) ) ;
#89928 = CARTESIAN_POINT ( 'NONE',  ( 9.382169495545415572, -22.75136533006957862, -9.382169495545422677 ) ) ;
#89929 = CARTESIAN_POINT ( 'NONE',  ( -0.8801773607110991993, 32.85535201082151247, -2.915334737309923874 ) ) ;
#89930 = CARTESIAN_POINT ( 'NONE',  ( 1.472469842513823179, 20.59226448433411960, -4.923371831947296329 ) ) ;
#89931 = CARTESIAN_POINT ( 'NONE',  ( 16.40814093676323893, 10.79030133659708923, 11.09922568453595026 ) ) ;
#89932 = CARTESIAN_POINT ( 'NONE',  ( 4.559911319644449179, 58.89701867748817676, 9.422509992056141925 ) ) ;
#89934 = CARTESIAN_POINT ( 'NONE',  ( -2.816281873526473856, 54.33196800326376064, 3.434112377981055619 ) ) ;
#89933 = CARTESIAN_POINT ( 'NONE',  ( 0.5774900079438607392, 28.48035201082150891, 5.440088680355550821 ) ) ;
#89935 = CARTESIAN_POINT ( 'NONE',  ( 10.00000000000000178, 43.05374883491397497, 14.16423886937410082 ) ) ;
#89936 = AXIS2_PLACEMENT_3D ( 'NONE', #3186, #55693, #86191 ) ;
#89937 = TOROIDAL_SURFACE ( 'NONE', #77158, 14.49999999999999822, 0.5000000000000000000 ) ;
#89938 = CARTESIAN_POINT ( 'NONE',  ( 69.60148758828984228, 0.4999999999999960032, 9.500000000000000000 ) ) ;
#89939 = ORIENTED_EDGE ( 'NONE', *, *, #94315, .T. ) ;
#89940 = CARTESIAN_POINT ( 'NONE',  ( 19.38216949554541202, 10.99863466993042138, 9.382169495545424454 ) ) ;
#89941 = CARTESIAN_POINT ( 'NONE',  ( 10.00000000000000000, 6.813685344154838397, -10.88017736071110342 ) ) ;
#89942 = CARTESIAN_POINT ( 'NONE',  ( 2.035157376598822676, 52.43868534415483396, -7.964842623401177768 ) ) ;
#89943 = CARTESIAN_POINT ( 'NONE',  ( 18.29284471827479308, 25.40189080397286148, -6.500000000000035527 ) ) ;
#89944 = EDGE_LOOP ( 'NONE', ( #40408, #69171, #44746, #60053, #9208, #19683 ) ) ;
#89945 = CARTESIAN_POINT ( 'NONE',  ( 4.559911319644449179, 63.89701867748817676, 9.422509992056141925 ) ) ;
#89946 = CARTESIAN_POINT ( 'NONE',  ( 18.52753015748617571, 38.09226448433412315, 4.923371831947298993 ) ) ;
#89947 = CARTESIAN_POINT ( 'NONE',  ( 18.52753015748618282, 28.92559781766745175, -4.923371831947291888 ) ) ;
#89948 = CARTESIAN_POINT ( 'NONE',  ( 17.20831665107776587, 17.88393115100078745, 7.208316651077764980 ) ) ;
#89950 = CARTESIAN_POINT ( 'NONE',  ( 6.565887622018943937, 40.16530133659708923, 12.81628187352647430 ) ) ;
#89949 = CARTESIAN_POINT ( 'NONE',  ( 14.43063482171891465, 15.00000000000000888, 2.386446184883126875 ) ) ;
#89951 = EDGE_CURVE ( 'NONE', #18862, #77019, #4028, .T. ) ;
#89953 = LINE ( 'NONE', #51968, #64285 ) ;
#89952 = CARTESIAN_POINT ( 'NONE',  ( 2.791683348922240793, 1.633931151000784565, 7.208316651077764092 ) ) ;
#89954 = CARTESIAN_POINT ( 'NONE',  ( 11.18664512657591459, -81.61943089668858420, 4.000000000000000000 ) ) ;
#89956 = ORIENTED_EDGE ( 'NONE', *, *, #90769, .F. ) ;
#89955 = CARTESIAN_POINT ( 'NONE',  ( 7.361572987183170547, 32.05059781766745175, 9.846743663894590881 ) ) ;
#89957 = CARTESIAN_POINT ( 'NONE',  ( 16.40814093676324603, 57.45696800326375353, -11.09922568453594671 ) ) ;
#89958 = DIRECTION ( 'NONE',  ( -0.000000000000000000, -0.000000000000000000, 1.000000000000000000 ) ) ;
#89959 = CARTESIAN_POINT ( 'NONE',  ( 13.43411237798105340, 0.5819680032637533085, 12.81628187352647963 ) ) ;
#89960 = TOROIDAL_SURFACE ( 'NONE', #88392, 14.49999999999999822, 0.5000000000000000000 ) ;
#89961 = CARTESIAN_POINT ( 'NONE',  ( -0.8801773607111008646, 13.27201867748817143, 2.915334737309923430 ) ) ;
#89962 = CARTESIAN_POINT ( 'NONE',  ( 20.36894250292379738, 29.92874883491396432, -10.36894250292379027 ) ) ;
#89963 = VECTOR ( 'NONE', #98730, 1000.000000000000114 ) ;
#89964 = DIRECTION ( 'NONE',  ( 0.000000000000000000, 1.000000000000000000, 0.000000000000000000 ) ) ;
#89965 = CIRCLE ( 'NONE', #91621, 4.000000000000001776 ) ;
#89966 = CARTESIAN_POINT ( 'NONE',  ( 20.36894250292379382, 28.67874883491396787, 10.36894250292379205 ) ) ;
#89967 = CARTESIAN_POINT ( 'NONE',  ( 24.16423886937410614, 44.51208216824730357, -3.795296366450302550 ) ) ;
#89968 = CARTESIAN_POINT ( 'NONE',  ( -2.266590686148945544, 6.387082168247300906, -7.082119434687050408 ) ) ;
#89970 = CARTESIAN_POINT ( 'NONE',  ( -13.77612262535527954, 90.93158326518027934, -7.883772450803742338 ) ) ;
#89969 = CARTESIAN_POINT ( 'NONE',  ( 24.16423886937409904, 9.095415501580633943, 3.795296366450317205 ) ) ;
#89971 = CARTESIAN_POINT ( 'NONE',  ( 7.084665262690076126, 47.02201867748818387, -10.88017736071110164 ) ) ;
#89973 = AXIS2_PLACEMENT_3D ( 'NONE', #4752, #66725, #59209 ) ;
#89972 = CARTESIAN_POINT ( 'NONE',  ( 0.1532563361054082862, 36.21726448433410894, 2.638427012816831674 ) ) ;
#89975 = CARTESIAN_POINT ( 'NONE',  ( 0.1532563361054083140, 26.00893115100078745, 1.131784320476157264E-15 ) ) ;
#89974 = LINE ( 'NONE', #66984, #59632 ) ;
#89976 = CARTESIAN_POINT ( 'NONE',  ( 12.91533473730992121, 14.52201867748817143, 10.88017736071110164 ) ) ;
#89977 = CARTESIAN_POINT ( 'NONE',  ( 6.565887622018943937, 58.08196800326376064, -12.81628187352647608 ) ) ;
#89978 = CARTESIAN_POINT ( 'NONE',  ( 12.63842701281683922, 54.55059781766745175, -9.846743663894590881 ) ) ;
#89979 = CARTESIAN_POINT ( 'NONE',  ( -0.1503990784575280903, 23.10158574516642815, 6.262539305110076171 ) ) ;
#89980 = CARTESIAN_POINT ( 'NONE',  ( 12.63842701281683922, 29.55059781766745175, -9.846743663894590881 ) ) ;
#89981 = CARTESIAN_POINT ( 'NONE',  ( 16.40814093676323893, 45.79030133659708923, 11.09922568453595026 ) ) ;
#89982 = CARTESIAN_POINT ( 'NONE',  ( 14.16423886937410082, -15.48791783175269643, -3.795296366450314096 ) ) ;
#89983 = CARTESIAN_POINT ( 'NONE',  ( -0.8801773607111008646, 38.27201867748816255, 2.915334737309923430 ) ) ;
#89984 = CARTESIAN_POINT ( 'NONE',  ( 0.1532563361054100626, 40.80059781766745886, -2.638427012816831230 ) ) ;
#89985 = CARTESIAN_POINT ( 'NONE',  ( -0.3689425029237881626, 27.42874883491397142, 10.36894250292379027 ) ) ;
#89986 = EDGE_CURVE ( 'NONE', #29326, #39731, #57499, .T. ) ;
#89987 = ORIENTED_EDGE ( 'NONE', *, *, #81638, .F. ) ;
#89988 = CARTESIAN_POINT ( 'NONE',  ( 13.79529636645031943, 5.345415501580634832, -14.16423886937409904 ) ) ;
#89989 = CARTESIAN_POINT ( 'NONE',  ( 2.035157376598824452, 63.68868534415484106, 7.964842623401179544 ) ) ;
#89990 = CARTESIAN_POINT ( 'NONE',  ( 2.035157376598822676, 67.43868534415484817, -7.964842623401177768 ) ) ;
#89991 = CARTESIAN_POINT ( 'NONE',  ( 2.917880565312948704, 52.63708216824730357, 12.26659068614894643 ) ) ;
#89992 = CARTESIAN_POINT ( 'NONE',  ( 16.40814093676323893, 0.7903013365970867898, 11.09922568453595026 ) ) ;
#89993 = CARTESIAN_POINT ( 'NONE',  ( 9.898881779040729967, -0.03417435944610275333, -10.25059215482576214 ) ) ;
#89994 = CARTESIAN_POINT ( 'NONE',  ( -0.8801773607111008646, 58.27201867748816966, 2.915334737309923430 ) ) ;
#89995 = CARTESIAN_POINT ( 'NONE',  ( -1.926860441876564023, 27.87045670184114243, 3.195792623639529761 ) ) ;
#89996 = CARTESIAN_POINT ( 'NONE',  ( -1.099225684535947600, 34.54030133659708923, 6.408140936763237150 ) ) ;
#89997 = CARTESIAN_POINT ( 'NONE',  ( 5.440088680355549045, 31.39701867748817676, -9.422509992056141925 ) ) ;
#89998 = CARTESIAN_POINT ( 'NONE',  ( 17.96484262340118221, 19.93868534415484106, 7.964842623401181321 ) ) ;
#89999 = CARTESIAN_POINT ( 'NONE',  ( 7.084665262690076126, 9.105352010821503583, 10.88017736071109987 ) ) ;
#90000 = CARTESIAN_POINT ( 'NONE',  ( 2.791683348922240793, 36.63393115100078035, 7.208316651077764092 ) ) ;
#90001 = CARTESIAN_POINT ( 'NONE',  ( 6.565887622018943937, 45.16530133659708923, 12.81628187352647430 ) ) ;
#90002 = ORIENTED_EDGE ( 'NONE', *, *, #48131, .T. ) ;
#90003 = CARTESIAN_POINT ( 'NONE',  ( -0.8801773607110991993, 22.85535201082150181, -2.915334737309923874 ) ) ;
#90004 = CARTESIAN_POINT ( 'NONE',  ( 3.591859063236761518, 4.956968003263753531, 11.09922568453594849 ) ) ;
#90005 = DIRECTION ( 'NONE',  ( 0.000000000000000000, 1.000000000000000000, 0.000000000000000000 ) ) ;
#90006 = CARTESIAN_POINT ( 'NONE',  ( 18.52753015748617571, 8.092264484334117824, 4.923371831947298993 ) ) ;
#90007 = CARTESIAN_POINT ( 'NONE',  ( 14.92337183194729988, 49.34226448433411605, -8.527530157486177487 ) ) ;
#90008 = CARTESIAN_POINT ( 'NONE',  ( 19.42250999205614193, 30.14701867748817321, 5.440088680355555262 ) ) ;
#90009 = CARTESIAN_POINT ( 'NONE',  ( 6.565887622018943937, 13.08196800326374998, -12.81628187352647608 ) ) ;
#90011 = FACE_OUTER_BOUND ( 'NONE', #31728, .T. ) ;
#90010 = CARTESIAN_POINT ( 'NONE',  ( 4.559911319644449179, 53.89701867748817676, 9.422509992056141925 ) ) ;
#90012 = DIRECTION ( 'NONE',  ( -0.000000000000000000, -0.000000000000000000, 1.000000000000000000 ) ) ;
#90013 = CARTESIAN_POINT ( 'NONE',  ( 21.09922568453594849, 46.20696800326376064, 6.408140936763242479 ) ) ;
#90014 = ORIENTED_EDGE ( 'NONE', *, *, #11098, .F. ) ;
#90015 = CARTESIAN_POINT ( 'NONE',  ( 2.035157376598822676, 62.43868534415483396, -7.964842623401177768 ) ) ;
#90016 = CARTESIAN_POINT ( 'NONE',  ( 22.81628187352647785, 36.41530133659707502, 3.434112377981063169 ) ) ;
#90017 = DIRECTION ( 'NONE',  ( 0.000000000000000000, 0.000000000000000000, 1.000000000000000000 ) ) ;
#90018 = CARTESIAN_POINT ( 'NONE',  ( 17.96484262340118221, 44.93868534415483396, 7.964842623401181321 ) ) ;
#90019 = DIRECTION ( 'NONE',  ( 0.000000000000000000, 1.000000000000000000, 0.000000000000000000 ) ) ;
#90020 = CARTESIAN_POINT ( 'NONE',  ( 19.84674366389459621, 48.50893115100078745, 7.409399052514197653E-17 ) ) ;
#90021 = CARTESIAN_POINT ( 'NONE',  ( 5.076628168052703671, 21.84226448433411960, 8.527530157486179263 ) ) ;
#90022 = EDGE_CURVE ( 'NONE', #39466, #71601, #88991, .T. ) ;
#90023 = CARTESIAN_POINT ( 'NONE',  ( 1.472469842513823179, 11.42559781766745175, 4.923371831947296329 ) ) ;
#90024 =( NAMED_UNIT ( * ) SI_UNIT ( $, .STERADIAN. ) SOLID_ANGLE_UNIT ( ) );
#90025 = CARTESIAN_POINT ( 'NONE',  ( -4.164238869374099039, 46.80374883491397497, 8.674139862899312516E-16 ) ) ;
#90026 = LINE ( 'NONE', #13543, #63377 ) ;
#90027 = ADVANCED_FACE ( 'NONE', ( #27002 ), #53433, .T. ) ;
#90028 = CARTESIAN_POINT ( 'NONE',  ( 5.171435456984222689, 0.000000000000000000, 1.730338099014012476 ) ) ;
#90029 = CARTESIAN_POINT ( 'NONE',  ( -7.072388532740516709, -84.40601219567591329, -3.750000000000806022 ) ) ;
#90030 = ORIENTED_EDGE ( 'NONE', *, *, #17762, .F. ) ;
#90031 = CARTESIAN_POINT ( 'NONE',  ( 22.26659068614895176, 59.72041550158063927, -7.082119434687042414 ) ) ;
#90032 = CARTESIAN_POINT ( 'NONE',  ( -0.3689425029237881626, 67.42874883491396076, 10.36894250292379027 ) ) ;
#90033 = CARTESIAN_POINT ( 'NONE',  ( 1.472469842513823179, 31.42559781766745530, 4.923371831947296329 ) ) ;
#90034 = CARTESIAN_POINT ( 'NONE',  ( 13.43411237798105340, 25.58196800326374998, 12.81628187352647963 ) ) ;
#90035 = LINE ( 'NONE', #6058, #97049 ) ;
#90038 = CARTESIAN_POINT ( 'NONE',  ( 13.79529636645030344, 13.26208216824729824, 14.16423886937410614 ) ) ;
#90037 = DIRECTION ( 'NONE',  ( 1.000000000000000000, 0.000000000000000000, 0.000000000000000000 ) ) ;
#90036 = VECTOR ( 'NONE', #46259, 1000.000000000000000 ) ;
#90039 = CARTESIAN_POINT ( 'NONE',  ( 19.42250999205614548, 10.98035201082150358, -5.440088680355545492 ) ) ;
#90040 = CARTESIAN_POINT ( 'NONE',  ( 2.917880565312948704, 57.63708216824731068, 12.26659068614894643 ) ) ;
#90041 = CARTESIAN_POINT ( 'NONE',  ( 7.361572987183169658, 34.96726448433411605, -9.846743663894592657 ) ) ;
#90042 = DIRECTION ( 'NONE',  ( 0.000000000000000000, 1.000000000000000000, 0.000000000000000000 ) ) ;
#90043 = CARTESIAN_POINT ( 'NONE',  ( 1.472469842513823179, 6.425597817667451750, 4.923371831947296329 ) ) ;
#90044 = VECTOR ( 'NONE', #15616, 1000.000000000000000 ) ;
#90045 = CARTESIAN_POINT ( 'NONE',  ( 0.000000000000000000, 0.000000000000000000, 0.000000000000000000 ) ) ;
#90046 = CARTESIAN_POINT ( 'NONE',  ( 9.846743663894590881, 13.71726448433412493, -2.638427012816833894 ) ) ;
#90047 = ORIENTED_EDGE ( 'NONE', *, *, #53064, .F. ) ;
#90048 = ORIENTED_EDGE ( 'NONE', *, *, #82290, .F. ) ;
#90049 = ORIENTED_EDGE ( 'NONE', *, *, #8280, .F. ) ;
#90050 = CARTESIAN_POINT ( 'NONE',  ( 0.1532563361054083140, 41.00893115100078745, 1.131784320476157264E-15 ) ) ;
#90051 = CARTESIAN_POINT ( 'NONE',  ( 22.26659068614894466, 18.88708216824730002, 7.082119434687054849 ) ) ;
#90053 = CARTESIAN_POINT ( 'NONE',  ( 12.91533473730993009, 26.60535201082150536, -10.88017736071109987 ) ) ;
#90052 = CARTESIAN_POINT ( 'NONE',  ( 19.42250999205614548, 25.98035201082150891, -5.440088680355545492 ) ) ;
#90055 = CARTESIAN_POINT ( 'NONE',  ( -2.816281873526473856, 14.33196800326375531, 3.434112377981055619 ) ) ;
#90054 = CARTESIAN_POINT ( 'NONE',  ( 5.076628168052704559, 65.17559781766745175, -8.527530157486179263 ) ) ;
#90056 = CARTESIAN_POINT ( 'NONE',  ( -0.3689425029237898834, 1.178748834913967869, -10.36894250292378850 ) ) ;
#90057 = CARTESIAN_POINT ( 'NONE',  ( -0.8801773607110991993, 62.85535201082150536, -2.915334737309923874 ) ) ;
#90058 = CARTESIAN_POINT ( 'NONE',  ( 6.565887622018943937, 38.08196800326376064, -12.81628187352647608 ) ) ;
#90059 = EDGE_LOOP ( 'NONE', ( #61594, #64216, #51597, #40756 ) ) ;
#90060 = CARTESIAN_POINT ( 'NONE',  ( 10.00000000000000000, 34.75893115100078745, -9.846743663894594434 ) ) ;
#90061 = CARTESIAN_POINT ( 'NONE',  ( 10.00000000000000000, 11.81368534415483751, -10.88017736071110342 ) ) ;
#90062 = ORIENTED_EDGE ( 'NONE', *, *, #17199, .F. ) ;
#90063 = CARTESIAN_POINT ( 'NONE',  ( 0.5774900079438607392, 8.480352010821505360, 5.440088680355550821 ) ) ;
#90064 = ORIENTED_EDGE ( 'NONE', *, *, #67149, .F. ) ;
#90065 = CARTESIAN_POINT ( 'NONE',  ( 7.084665262690076126, 49.10535201082149825, 10.88017736071109987 ) ) ;
#90066 = CARTESIAN_POINT ( 'NONE',  ( -0.8801773607110991993, 57.85535201082149825, -2.915334737309923874 ) ) ;
#90067 = CARTESIAN_POINT ( 'NONE',  ( 0.2751277870542871429, 42.28217586085238366, -6.499999999999984901 ) ) ;
#90068 = SURFACE_SIDE_STYLE ('',( #75568 ) ) ;
#90069 = CARTESIAN_POINT ( 'NONE',  ( 2.035157376598822676, 52.43868534415483396, -7.964842623401177768 ) ) ;
#90070 = DIRECTION ( 'NONE',  ( 0.4924235601034648302, 0.000000000000000000, 0.8703556959399010307 ) ) ;
#90071 = ADVANCED_FACE ( 'NONE', ( #59979 ), #26290, .T. ) ;
#90072 = CARTESIAN_POINT ( 'NONE',  ( 12.63842701281683034, 32.46726448433412315, 9.846743663894596210 ) ) ;
#90073 = ORIENTED_EDGE ( 'NONE', *, *, #27524, .T. ) ;
#90074 = CARTESIAN_POINT ( 'NONE',  ( 2.791683348922240793, 56.63393115100078035, 7.208316651077764092 ) ) ;
#90075 = EDGE_CURVE ( 'NONE', #40424, #42957, #42291, .T. ) ;
#90076 = DIRECTION ( 'NONE',  ( -0.000000000000000000, -1.000000000000000000, -0.000000000000000000 ) ) ;
#90077 = B_SPLINE_CURVE_WITH_KNOTS ( 'NONE', 3,
 ( #97142, #28612, #85563, #1592, #92557, #55044 ),
 .UNSPECIFIED., .F., .F.,
 ( 4, 2, 4 ),
 ( 3.409110551491190117E-05, 0.0004400426677367364815, 0.0008459942299585610686 ),
 .UNSPECIFIED. ) ;
#90078 = CARTESIAN_POINT ( 'NONE',  ( 6.204703633549690345, 5.762082168247301794, -14.16423886937410259 ) ) ;
#90079 = EDGE_LOOP ( 'NONE', ( #51669, #95063, #14307, #78753 ) ) ;
#90080 = CARTESIAN_POINT ( 'NONE',  ( 19.72487221294571214, 44.78217586085236945, 6.499999999999993783 ) ) ;
#90081 = DIRECTION ( 'NONE',  ( 0.000000000000000000, 0.000000000000000000, -1.000000000000000000 ) ) ;
#90082 =( NAMED_UNIT ( * ) PLANE_ANGLE_UNIT ( ) SI_UNIT ( $, .RADIAN. ) );
#90083 = CARTESIAN_POINT ( 'NONE',  ( 10.00000000000000000, 11.81368534415483751, -10.88017736071110342 ) ) ;
#90084 = CARTESIAN_POINT ( 'NONE',  ( 18.06765999051789251, 63.99127512925452521, 6.499999999999953815 ) ) ;
#90085 = ORIENTED_EDGE ( 'NONE', *, *, #76586, .F. ) ;
#90086 = FILL_AREA_STYLE_COLOUR ( '', #78379 ) ;
#90087 = CARTESIAN_POINT ( 'NONE',  ( 17.20831665107776587, 47.88393115100078745, 7.208316651077764980 ) ) ;
#90088 = CARTESIAN_POINT ( 'NONE',  ( -2.518025504887084765, 0.000000000000000000, -4.837081990145629007 ) ) ;
#90089 = CARTESIAN_POINT ( 'NONE',  ( 13.43411237798105340, 15.58196800326374998, 12.81628187352647963 ) ) ;
#90090 = CARTESIAN_POINT ( 'NONE',  ( 14.92337183194729988, 9.342264484334119601, -8.527530157486177487 ) ) ;
#90091 = CARTESIAN_POINT ( 'NONE',  ( 0.2751277870542913062, 29.36607318730131411, -6.499999999999992006 ) ) ;
#90092 = CARTESIAN_POINT ( 'NONE',  ( 19.38216949554541202, 5.998634669930420493, 9.382169495545424454 ) ) ;
#90093 = CARTESIAN_POINT ( 'NONE',  ( 0.1532563361054083140, 26.00893115100078745, 1.131784320476157264E-15 ) ) ;
#90094 = EDGE_CURVE ( 'NONE', #8246, #2122, #46944, .T. ) ;
#90095 = CIRCLE ( 'NONE', #86892, 1.999999999999996669 ) ;
#90096 = EDGE_LOOP ( 'NONE', ( #45090, #92025, #52543, #62193 ) ) ;
#90097 = CARTESIAN_POINT ( 'NONE',  ( 4.559911319644449179, 8.897018677488173211, 9.422509992056141925 ) ) ;
#90098 = CARTESIAN_POINT ( 'NONE',  ( 24.16423886937410614, 24.30374883491396787, 8.672049930838204340E-16 ) ) ;
#90099 = CARTESIAN_POINT ( 'NONE',  ( 18.52753015748617571, 33.09226448433411605, 4.923371831947298993 ) ) ;
#90100 = CARTESIAN_POINT ( 'NONE',  ( 20.88017736071110164, 50.35535201082151247, 2.915334737309930979 ) ) ;
#90101 = CARTESIAN_POINT ( 'NONE',  ( 16.40814093676324603, 42.45696800326375353, -11.09922568453594671 ) ) ;
#90102 = CARTESIAN_POINT ( 'NONE',  ( 19.42250999205614548, 20.98035201082150891, -5.440088680355545492 ) ) ;
#90103 = EDGE_CURVE ( 'NONE', #34211, #91796, #2955, .T. ) ;
#90104 =( GEOMETRIC_REPRESENTATION_CONTEXT ( 3 ) GLOBAL_UNCERTAINTY_ASSIGNED_CONTEXT ( ( #75456 ) ) GLOBAL_UNIT_ASSIGNED_CONTEXT ( ( #47065, #55057, #18066 ) ) REPRESENTATION_CONTEXT ( 'NONE', 'WORKASPACE' ) );
#90105 = B_SPLINE_CURVE_WITH_KNOTS ( 'NONE', 3,
 ( #65364, #27373, #88377, #49873, #57865, #19874 ),
 .UNSPECIFIED., .F., .F.,
 ( 4, 2, 4 ),
 ( 3.409110551494643978E-05, 0.0004400426677367928058, 0.0008459942299586392395 ),
 .UNSPECIFIED. ) ;
#90106 = DIRECTION ( 'NONE',  ( -0.000000000000000000, 1.000000000000000000, 0.000000000000000000 ) ) ;
#90107 = PLANE ( 'NONE',  #61566 ) ;
#90108 = CARTESIAN_POINT ( 'NONE',  ( 1.472469842513823179, 60.59226448433412315, -4.923371831947296329 ) ) ;
#90109 = CARTESIAN_POINT ( 'NONE',  ( 5.076628168052703671, 26.84226448433411960, 8.527530157486179263 ) ) ;
#90110 = CARTESIAN_POINT ( 'NONE',  ( -5.440088680355547268, -11.10298132251182146, 9.422509992056143702 ) ) ;
#90111 = CARTESIAN_POINT ( 'NONE',  ( 6.565887622018943937, 40.16530133659708923, 12.81628187352647430 ) ) ;
#90112 = DIRECTION ( 'NONE',  ( 0.000000000000000000, -1.000000000000000000, 0.000000000000000000 ) ) ;
#90114 = CARTESIAN_POINT ( 'NONE',  ( 13.14228782657339956, 0.5000000000000004441, -7.230509711182238064 ) ) ;
#90113 = CARTESIAN_POINT ( 'NONE',  ( 12.91533473730993009, 46.60535201082150536, -10.88017736071109987 ) ) ;
#90115 = CARTESIAN_POINT ( 'NONE',  ( 13.82192141328812518, 15.00000000000000000, -4.382292601468683380 ) ) ;
#90116 = CARTESIAN_POINT ( 'NONE',  ( 20.88017736071110875, 60.77201867748817676, -2.915334737309920765 ) ) ;
#90117 = CARTESIAN_POINT ( 'NONE',  ( 17.96484262340118221, 46.18868534415484106, -7.964842623401177768 ) ) ;
#90118 = CARTESIAN_POINT ( 'NONE',  ( 10.00000000000000178, 49.31368534415484106, 10.88017736071110342 ) ) ;
#90119 = DIRECTION ( 'NONE',  ( 0.000000000000000000, 1.000000000000000000, 0.000000000000000000 ) ) ;
#90120 = CARTESIAN_POINT ( 'NONE',  ( 10.00000000000000000, 51.81368534415484106, -10.88017736071110342 ) ) ;
#90121 = CARTESIAN_POINT ( 'NONE',  ( 17.20831665107776587, 37.88393115100078745, 7.208316651077764980 ) ) ;
#90122 = CARTESIAN_POINT ( 'NONE',  ( 12.91533473730992121, 9.522018677488171434, 10.88017736071110164 ) ) ;
#90123 = CARTESIAN_POINT ( 'NONE',  ( 6.565887622018943937, 13.08196800326374998, -12.81628187352647608 ) ) ;
#90124 = ORIENTED_EDGE ( 'NONE', *, *, #16876, .F. ) ;
#90125 = CARTESIAN_POINT ( 'NONE',  ( 15.44008868035555260, 24.73035201082150891, 9.422509992056143702 ) ) ;
#90126 = CARTESIAN_POINT ( 'NONE',  ( 0.5774900079438607392, 23.48035201082150536, 5.440088680355550821 ) ) ;
#90127 = CARTESIAN_POINT ( 'NONE',  ( -0.8801773607111008646, 68.27201867748817676, 2.915334737309923430 ) ) ;
#90128 = CARTESIAN_POINT ( 'NONE',  ( 6.204703633549690345, 25.76208216824730712, -14.16423886937410259 ) ) ;
#90129 = CARTESIAN_POINT ( 'NONE',  ( 17.20831665107776587, 7.883931151000784787, 7.208316651077764980 ) ) ;
#90130 = CARTESIAN_POINT ( 'NONE',  ( 10.00000000000000000, 41.81368534415484106, -10.88017736071110342 ) ) ;
#90131 = CARTESIAN_POINT ( 'NONE',  ( 8.839000071701287098, 14.95037109469702230, -11.81225584161899178 ) ) ;
#90132 = TOROIDAL_SURFACE ( 'NONE', #47030, 14.49999999999999822, 0.5000000000000000000 ) ;
#90133 = ADVANCED_FACE ( 'NONE', ( #18430 ), #85400, .T. ) ;
#90134 = ORIENTED_EDGE ( 'NONE', *, *, #59954, .T. ) ;
#90135 = CARTESIAN_POINT ( 'NONE',  ( -9.898881779040801021, -0.03417435944610275333, 10.25059215482569641 ) ) ;
#90136 = CARTESIAN_POINT ( 'NONE',  ( 0.1532563361054083140, 41.00893115100078745, 1.131784320476157264E-15 ) ) ;
#90137 = ORIENTED_EDGE ( 'NONE', *, *, #3476, .T. ) ;
#90138 = ORIENTED_EDGE ( 'NONE', *, *, #28800, .T. ) ;
#90139 = DIRECTION ( 'NONE',  ( -0.7716245833877148907, 0.000000000000000000, -0.6360782202777701677 ) ) ;
#90140 = CARTESIAN_POINT ( 'NONE',  ( 24.16423886937410614, 19.30374883491397142, 8.672049930838204340E-16 ) ) ;
#90141 = CARTESIAN_POINT ( 'NONE',  ( 22.26659068614895176, 19.72041550158063572, -7.082119434687042414 ) ) ;
#90142 = CARTESIAN_POINT ( 'NONE',  ( -0.8801773607110991993, 57.85535201082149825, -2.915334737309923874 ) ) ;
#90143 = CARTESIAN_POINT ( 'NONE',  ( 4.559911319644449179, 2.230352010821504916, -9.422509992056141925 ) ) ;
#90144 = CARTESIAN_POINT ( 'NONE',  ( -2.816281873526473856, -0.6680319967362464695, 3.434112377981055619 ) ) ;
#90145 = CARTESIAN_POINT ( 'NONE',  ( 10.00000000000000000, 54.75893115100078745, -9.846743663894594434 ) ) ;
#90146 = LINE ( 'NONE', #80689, #27517 ) ;
#90148 = CARTESIAN_POINT ( 'NONE',  ( 10.00000000000000178, 10.37363466993041961, 12.81628187352647608 ) ) ;
#90147 = CARTESIAN_POINT ( 'NONE',  ( -0.8801773607110991993, 42.85535201082150536, -2.915334737309923874 ) ) ;
#90149 = CARTESIAN_POINT ( 'NONE',  ( -0.3689425029237898834, 16.17874883491396076, -10.36894250292378850 ) ) ;
#90150 = CARTESIAN_POINT ( 'NONE',  ( -0.8801773607111008646, 13.27201867748817321, 2.915334737309923430 ) ) ;
#90151 = CARTESIAN_POINT ( 'NONE',  ( 15.44008868035555793, 16.39701867748817321, -9.422509992056140149 ) ) ;
#90152 = DIRECTION ( 'NONE',  ( -1.000000000000000000, 0.000000000000000000, 0.000000000000000000 ) ) ;
#90153 = CARTESIAN_POINT ( 'NONE',  ( 7.084665262690076126, 39.10535201082150536, 10.88017736071109987 ) ) ;
#90154 = CARTESIAN_POINT ( 'NONE',  ( -7.208316651077764980, -24.61606884899921255, -7.208316651077759651 ) ) ;
#90155 = ORIENTED_EDGE ( 'NONE', *, *, #81605, .T. ) ;
#90156 = DIRECTION ( 'NONE',  ( -0.000000000000000000, 0.000000000000000000, 1.000000000000000000 ) ) ;
#90157 = VERTEX_POINT ( 'NONE', #85448 ) ;
#90158 = CARTESIAN_POINT ( 'NONE',  ( 1.472469842513823179, 31.42559781766745530, 4.923371831947296329 ) ) ;
#90159 = VERTEX_POINT ( 'NONE', #54931 ) ;
#90160 = CARTESIAN_POINT ( 'NONE',  ( -0.9082943533638192513, 4.617951328659527895E-16, 14.47152380945584582 ) ) ;
#90162 = CARTESIAN_POINT ( 'NONE',  ( 15.44008868035555793, 11.39701867748817143, -9.422509992056140149 ) ) ;
#90161 = CARTESIAN_POINT ( 'NONE',  ( 13.79529636645030344, 48.26208216824728936, 14.16423886937410614 ) ) ;
#90164 = CARTESIAN_POINT ( 'NONE',  ( 2.791683348922240793, 46.63393115100077324, 7.208316651077764092 ) ) ;
#90163 = CARTESIAN_POINT ( 'NONE',  ( 0.1532563361054082862, 21.21726448433412315, 2.638427012816831674 ) ) ;
#90165 = CARTESIAN_POINT ( 'NONE',  ( -0.8801773607110991993, 67.85535201082151957, -2.915334737309923874 ) ) ;
#90166 = CARTESIAN_POINT ( 'NONE',  ( 10.00000000000000000, 4.758931151000784787, -9.846743663894594434 ) ) ;
#90167 = VECTOR ( 'NONE', #57985, 1000.000000000000000 ) ;
#90168 = CARTESIAN_POINT ( 'NONE',  ( 9.382169495545415572, 27.24863466993041428, -9.382169495545422677 ) ) ;
#90169 = ORIENTED_EDGE ( 'NONE', *, *, #64407, .F. ) ;
#90170 = EDGE_CURVE ( 'NONE', #31275, #73541, #71441, .T. ) ;
#90171 = CARTESIAN_POINT ( 'NONE',  ( 2.917880565312950480, 35.97041550158063217, -12.26659068614894821 ) ) ;
#90172 = AXIS2_PLACEMENT_3D ( 'NONE', #70344, #68869, #8356 ) ;
#90173 = CARTESIAN_POINT ( 'NONE',  ( 0.6178305044545818747, 28.49863466993041783, -9.382169495545419124 ) ) ;
#90174 = ORIENTED_EDGE ( 'NONE', *, *, #5571, .F. ) ;
#90175 = CARTESIAN_POINT ( 'NONE',  ( 3.591859063236763294, 48.29030133659708923, -11.09922568453595026 ) ) ;
#90176 = CARTESIAN_POINT ( 'NONE',  ( 17.96484262340118221, 16.18868534415483396, -7.964842623401177768 ) ) ;
#90177 = CARTESIAN_POINT ( 'NONE',  ( 7.361572987183169658, 39.96726448433411605, -9.846743663894592657 ) ) ;
#90178 = CARTESIAN_POINT ( 'NONE',  ( 2.035157376598822676, 27.43868534415483396, -7.964842623401177768 ) ) ;
#90179 = VECTOR ( 'NONE', #96757, 1000.000000000000000 ) ;
#90180 = DIRECTION ( 'NONE',  ( -1.000000000000000000, -1.049065152435176504E-16, 0.000000000000000000 ) ) ;
#90181 = CARTESIAN_POINT ( 'NONE',  ( -0.2838433074297238012, 13.12729635533385597, -9.500000000000000000 ) ) ;
#90182 = CARTESIAN_POINT ( 'NONE',  ( 18.52753015748618282, 38.92559781766745175, -4.923371831947291888 ) ) ;
#90183 = CARTESIAN_POINT ( 'NONE',  ( 7.361572987183169658, 44.96726448433412315, -9.846743663894592657 ) ) ;
#90184 = EDGE_CURVE ( 'NONE', #34829, #89237, #10923, .T. ) ;
#90186 = ORIENTED_EDGE ( 'NONE', *, *, #8057, .T. ) ;
#90185 = DIRECTION ( 'NONE',  ( 0.9799247046208295897, 0.000000000000000000, -0.1993679344171971901 ) ) ;
#90187 = AXIS2_PLACEMENT_3D ( 'NONE', #47927, #78928, #82869 ) ;
#90188 = CARTESIAN_POINT ( 'NONE',  ( -0.3093388210927633941, 0.5000000000000004441, -14.99680997725065978 ) ) ;
#90189 = LINE ( 'NONE', #43706, #70640 ) ;
#90190 = DIRECTION ( 'NONE',  ( 0.000000000000000000, 0.000000000000000000, -1.000000000000000000 ) ) ;
#90191 = EDGE_CURVE ( 'NONE', #98827, #94698, #48913, .T. ) ;
#90192 = CARTESIAN_POINT ( 'NONE',  ( 2.791683348922237240, 20.38393115100078745, -7.208316651077763204 ) ) ;
#90193 = EDGE_CURVE ( 'NONE', #41646, #22776, #90665, .T. ) ;
#90194 = CARTESIAN_POINT ( 'NONE',  ( 19.38216949554541202, 30.99863466993042138, 9.382169495545424454 ) ) ;
#90195 = LINE ( 'NONE', #44699, #2071 ) ;
#90196 = ORIENTED_EDGE ( 'NONE', *, *, #41225, .T. ) ;
#90197 = CARTESIAN_POINT ( 'NONE',  ( 5.076628168052703671, 51.84226448433412315, 8.527530157486179263 ) ) ;
#90198 = CARTESIAN_POINT ( 'NONE',  ( 19.72487221294571569, 27.80223176428830811, -6.499999999999990230 ) ) ;
#90199 = CARTESIAN_POINT ( 'NONE',  ( 14.92337183194729633, 37.67559781766745175, 8.527530157486181039 ) ) ;
#90200 = CARTESIAN_POINT ( 'NONE',  ( 22.26659068614894466, 38.88708216824731068, 7.082119434687054849 ) ) ;
#90201 = CARTESIAN_POINT ( 'NONE',  ( 18.52753015748618282, 43.92559781766745175, -4.923371831947291888 ) ) ;
#90202 = CARTESIAN_POINT ( 'NONE',  ( 22.81628187352647785, 46.62363466993041783, 6.195893100308588602E-16 ) ) ;
#90203 = DIRECTION ( 'NONE',  ( -0.000000000000000000, -0.000000000000000000, -1.000000000000000000 ) ) ;
#90204 = CARTESIAN_POINT ( 'NONE',  ( 10.00000000000000178, 12.25893115100078568, 9.846743663894594434 ) ) ;
#90205 = CARTESIAN_POINT ( 'NONE',  ( 0.000000000000000000, 0.5000000000000004441, 0.000000000000000000 ) ) ;
#90206 =( GEOMETRIC_REPRESENTATION_CONTEXT ( 3 ) GLOBAL_UNCERTAINTY_ASSIGNED_CONTEXT ( ( #26312 ) ) GLOBAL_UNIT_ASSIGNED_CONTEXT ( ( #27681, #3724, #4213 ) ) REPRESENTATION_CONTEXT ( 'NONE', 'WORKASPACE' ) );
#90207 = CARTESIAN_POINT ( 'NONE',  ( 19.84674366389459266, 53.71726448433411605, -2.638427012816827677 ) ) ;
#90208 = CARTESIAN_POINT ( 'NONE',  ( 12.91533473730993009, 46.60535201082150536, -10.88017736071109987 ) ) ;
#90209 = ITEM_DEFINED_TRANSFORMATION ( 'NONE', 'NONE', #40794,  #27931 ) ;
#90210 = CARTESIAN_POINT ( 'NONE',  ( 20.10384461210892582, 31.74302437010793199, 6.337995344473749348 ) ) ;
#90211 = CARTESIAN_POINT ( 'NONE',  ( 4.559911319644449179, 42.23035201082151247, -9.422509992056141925 ) ) ;
#90212 = VERTEX_POINT ( 'NONE', #40944 ) ;
#90213 = CARTESIAN_POINT ( 'NONE',  ( -3.866399090317088838, 0.04922511925147263906, -14.23717170745777949 ) ) ;
#90214 = CARTESIAN_POINT ( 'NONE',  ( 15.44008868035555260, 9.730352010821505360, 9.422509992056143702 ) ) ;
#90216 = CARTESIAN_POINT ( 'NONE',  ( 17.96484262340118221, 46.18868534415484106, -7.964842623401177768 ) ) ;
#90215 = CARTESIAN_POINT ( 'NONE',  ( 13.43411237798105340, 0.5819680032637533085, 12.81628187352647963 ) ) ;
#90217 = CARTESIAN_POINT ( 'NONE',  ( 2.603489959281591659, 15.43575266056827999, -6.500000000000006217 ) ) ;
#90218 = ADVANCED_FACE ( 'NONE', ( #62934 ), #94415, .F. ) ;
#90219 = CARTESIAN_POINT ( 'NONE',  ( 4.559911319644449179, 53.89701867748817676, 9.422509992056141925 ) ) ;
#90220 = CARTESIAN_POINT ( 'NONE',  ( -5.204170427930421283E-15, 6.412123368507812948, -11.92686044187656513 ) ) ;
#90222 = DIRECTION ( 'NONE',  ( -1.000000000000000000, 0.000000000000000000, 0.000000000000000000 ) ) ;
#90221 = CARTESIAN_POINT ( 'NONE',  ( 2.035157376598824452, 43.68868534415484106, 7.964842623401179544 ) ) ;
#90223 = CARTESIAN_POINT ( 'NONE',  ( 14.92337183194729633, 12.67559781766745353, 8.527530157486181039 ) ) ;
#90224 = CARTESIAN_POINT ( 'NONE',  ( 18.52753015748617571, 23.09226448433411960, 4.923371831947298993 ) ) ;
#90225 = PRESENTATION_STYLE_ASSIGNMENT (( #38720 ) ) ;
#90227 = CONICAL_SURFACE ( 'NONE', #57058, 13.74999999999999467, 0.7853981633974458365 ) ;
#90226 = CARTESIAN_POINT ( 'NONE',  ( 14.16423886937410437, 24.09541550158063572, 3.795296366450304770 ) ) ;
#90228 = CARTESIAN_POINT ( 'NONE',  ( 10.00000000000000000, 59.75893115100078745, -9.846743663894594434 ) ) ;
#90229 = CARTESIAN_POINT ( 'NONE',  ( 20.88017736071110519, 5.563685344154838397, 2.639326808657452039E-16 ) ) ;
#90230 = LINE ( 'NONE', #84235, #38921 ) ;
#90231 = CARTESIAN_POINT ( 'NONE',  ( 24.16423886937409904, 29.09541550158063572, 3.795296366450317205 ) ) ;
#90232 = CARTESIAN_POINT ( 'NONE',  ( 17.08211943468705130, 53.47041550158063217, 12.26659068614894998 ) ) ;
#90233 = CARTESIAN_POINT ( 'NONE',  ( 0.5774900079438607392, 3.480352010821504027, 5.440088680355550821 ) ) ;
#90234 = ORIENTED_EDGE ( 'NONE', *, *, #75409, .F. ) ;
#90235 = CARTESIAN_POINT ( 'NONE',  ( 10.00000000000000178, 22.25893115100078745, 9.846743663894594434 ) ) ;
#90236 = CARTESIAN_POINT ( 'NONE',  ( 0.5774900079438590739, 17.64701867748817321, -5.440088680355550821 ) ) ;
#90237 = CARTESIAN_POINT ( 'NONE',  ( 2.791683348922237240, 50.38393115100078035, -7.208316651077763204 ) ) ;
#90239 = DIRECTION ( 'NONE',  ( 0.000000000000000000, 0.000000000000000000, 1.000000000000000000 ) ) ;
#90238 = PLANE ( 'NONE',  #53154 ) ;
#90240 = DIRECTION ( 'NONE',  ( 0.000000000000000000, 0.000000000000000000, 1.000000000000000000 ) ) ;
#90241 = AXIS2_PLACEMENT_3D ( 'NONE', #64730, #87741, #19253 ) ;
#90242 = CARTESIAN_POINT ( 'NONE',  ( -0.9940297508538862292, -0.03417435944610275333, 14.21528771620248932 ) ) ;
#90243 = CARTESIAN_POINT ( 'NONE',  ( 0.6178305044545818747, 18.49863466993041428, -9.382169495545419124 ) ) ;
#90244 = CARTESIAN_POINT ( 'NONE',  ( 0.1532563361054100626, 40.80059781766745886, -2.638427012816831230 ) ) ;
#90245 = ORIENTED_EDGE ( 'NONE', *, *, #56512, .T. ) ;
#90246 = CARTESIAN_POINT ( 'NONE',  ( 18.52753015748617571, 8.092264484334117824, 4.923371831947298993 ) ) ;
#90247 = CARTESIAN_POINT ( 'NONE',  ( 11.29392812347916752, -89.88967135474473480, -4.000000000001793232 ) ) ;
#90248 = CARTESIAN_POINT ( 'NONE',  ( -0.8801773607111009756, 13.06368534415483929, 1.068504757029289695E-15 ) ) ;
#90249 = CARTESIAN_POINT ( 'NONE',  ( 10.00000000000000178, 38.05374883491396787, 14.16423886937410082 ) ) ;
#90250 = CARTESIAN_POINT ( 'NONE',  ( 15.44008868035555260, 44.73035201082151247, 9.422509992056143702 ) ) ;
#90251 = CARTESIAN_POINT ( 'NONE',  ( 7.084665262690076126, 64.10535201082150536, 10.88017736071109987 ) ) ;
#90252 = CARTESIAN_POINT ( 'NONE',  ( 0.1532563361054100626, 25.80059781766744820, -2.638427012816831230 ) ) ;
#90253 = CARTESIAN_POINT ( 'NONE',  ( 2.791683348922237240, 5.383931151000785675, -7.208316651077763204 ) ) ;
#90254 = CARTESIAN_POINT ( 'NONE',  ( 4.850097797904266983, 0.04962897333335813954, -13.93319274793802798 ) ) ;
#90255 = CARTESIAN_POINT ( 'NONE',  ( 18.52753015748617571, 43.09226448433412315, 4.923371831947298993 ) ) ;
#90256 = CARTESIAN_POINT ( 'NONE',  ( 0.5774900079438590739, 37.64701867748817676, -5.440088680355550821 ) ) ;
#90257 = ORIENTED_EDGE ( 'NONE', *, *, #42717, .T. ) ;
#90258 = CARTESIAN_POINT ( 'NONE',  ( -1.099225684535947600, 64.54030133659709634, 6.408140936763237150 ) ) ;
#90259 = AXIS2_PLACEMENT_3D ( 'NONE', #3199, #54698, #33181 ) ;
#90260 = LINE ( 'NONE', #69262, #63552 ) ;
#90261 = CARTESIAN_POINT ( 'NONE',  ( 1.472469842513823179, 5.592264484334118713, -4.923371831947296329 ) ) ;
#90262 = CARTESIAN_POINT ( 'NONE',  ( 19.38216949554541202, 45.99863466993041072, 9.382169495545424454 ) ) ;
#90264 = CARTESIAN_POINT ( 'NONE',  ( 7.361572987183170547, 42.05059781766745886, 9.846743663894590881 ) ) ;
#90263 = CARTESIAN_POINT ( 'NONE',  ( 4.559911319644449179, 12.23035201082150714, -9.422509992056141925 ) ) ;
#90265 =( NAMED_UNIT ( * ) PLANE_ANGLE_UNIT ( ) SI_UNIT ( $, .RADIAN. ) );
#90266 = CARTESIAN_POINT ( 'NONE',  ( 20.36894250292379738, 29.92874883491396432, -10.36894250292379027 ) ) ;
#90267 = CARTESIAN_POINT ( 'NONE',  ( 20.36894250292379738, 49.92874883491396787, -10.36894250292379027 ) ) ;
#90268 = CARTESIAN_POINT ( 'NONE',  ( 1.472469842513823179, 60.59226448433412315, -4.923371831947296329 ) ) ;
#90269 = DIRECTION ( 'NONE',  ( 0.000000000000000000, 0.000000000000000000, 1.000000000000000000 ) ) ;
#90270 = CARTESIAN_POINT ( 'NONE',  ( 20.88017736071110164, 35.35535201082150536, 2.915334737309930979 ) ) ;
#90271 = CARTESIAN_POINT ( 'NONE',  ( 10.00000000000000178, 7.258931151000785675, 9.846743663894594434 ) ) ;
#90272 = ORIENTED_EDGE ( 'NONE', *, *, #93009, .T. ) ;
#90273 = CARTESIAN_POINT ( 'NONE',  ( 16.40814093676324603, 62.45696800326376064, -11.09922568453594671 ) ) ;
#90274 = CARTESIAN_POINT ( 'NONE',  ( 7.084665262690076126, 64.10535201082150536, 10.88017736071109987 ) ) ;
#90275 = ORIENTED_EDGE ( 'NONE', *, *, #51717, .F. ) ;
#90277 = ADVANCED_FACE ( 'NONE', ( #93436 ), #50198, .T. ) ;
#90276 = MECHANICAL_DESIGN_GEOMETRIC_PRESENTATION_REPRESENTATION (  '', ( #21640 ), #71102 ) ;
#90278 = CARTESIAN_POINT ( 'NONE',  ( 22.26659068614894466, 3.887082168247300906, 7.082119434687054849 ) ) ;
#90279 = CARTESIAN_POINT ( 'NONE',  ( 14.92337183194729633, 12.67559781766745353, 8.527530157486181039 ) ) ;
#90280 = LINE ( 'NONE', #65803, #71198 ) ;
#90281 = VERTEX_POINT ( 'NONE', #63427 ) ;
#90282 = CARTESIAN_POINT ( 'NONE',  ( 2.035157376598824452, 33.68868534415484106, 7.964842623401179544 ) ) ;
#90283 = EDGE_LOOP ( 'NONE', ( #95499, #16541, #47624, #53787, #10628, #88984 ) ) ;
#90284 = CARTESIAN_POINT ( 'NONE',  ( 0.5774900079438590739, 32.64701867748816966, -5.440088680355550821 ) ) ;
#90285 = CARTESIAN_POINT ( 'NONE',  ( 19.80777595082616216, 55.68878173731741299, -6.499999999999961808 ) ) ;
#90286 = VERTEX_POINT ( 'NONE', #56432 ) ;
#90287 = ORIENTED_EDGE ( 'NONE', *, *, #84704, .F. ) ;
#90288 = CARTESIAN_POINT ( 'NONE',  ( 15.44008868035555260, 64.73035201082151957, 9.422509992056143702 ) ) ;
#90289 = CARTESIAN_POINT ( 'NONE',  ( 12.63842701281683922, 64.55059781766745175, -9.846743663894590881 ) ) ;
#90290 = EDGE_CURVE ( 'NONE', #66694, #25004, #69463, .T. ) ;
#90292 = PLANE ( 'NONE',  #6332 ) ;
#90291 = CARTESIAN_POINT ( 'NONE',  ( -0.8801773607111008646, 18.27201867748817321, 2.915334737309923430 ) ) ;
#90293 = CARTESIAN_POINT ( 'NONE',  ( 15.44008868035555793, 66.39701867748817676, -9.422509992056140149 ) ) ;
#90294 = CARTESIAN_POINT ( 'NONE',  ( 0.5774900079438607392, 13.48035201082150358, 5.440088680355550821 ) ) ;
#90295 = AXIS2_PLACEMENT_3D ( 'NONE', #63945, #17505, #85495 ) ;
#90296 = EDGE_CURVE ( 'NONE', #3803, #34327, #24466, .T. ) ;
#90297 = AXIS2_PLACEMENT_3D ( 'NONE', #8929, #70929, #23468 ) ;
#90298 = EDGE_LOOP ( 'NONE', ( #50049, #23171, #20209, #76905 ) ) ;
#90299 = CARTESIAN_POINT ( 'NONE',  ( 21.09922568453594849, 56.20696800326375353, 6.408140936763242479 ) ) ;
#90300 = CARTESIAN_POINT ( 'NONE',  ( 10.00000000000000000, 41.81368534415484106, -10.88017736071110342 ) ) ;
#90301 = CARTESIAN_POINT ( 'NONE',  ( -8.000000000000000000, 83.99999999999994316, 4.000000000000000000 ) ) ;
#90302 = CARTESIAN_POINT ( 'NONE',  ( 6.565887622018943937, 53.08196800326374643, -12.81628187352647608 ) ) ;
#90303 = CARTESIAN_POINT ( 'NONE',  ( 12.91533473730992121, 44.52201867748816966, 10.88017736071110164 ) ) ;
#90304 = EDGE_CURVE ( 'NONE', #53168, #89098, #9446, .T. ) ;
#90305 = CARTESIAN_POINT ( 'NONE',  ( 13.43411237798106583, 2.665301336597086568, -12.81628187352647252 ) ) ;
#90306 = CARTESIAN_POINT ( 'NONE',  ( -14.02068044289382875, 0.5000000000000004441, 5.331089937175565119 ) ) ;
#90307 = CARTESIAN_POINT ( 'NONE',  ( 5.076628168052703671, 16.84226448433411960, 8.527530157486179263 ) ) ;
#90308 = CARTESIAN_POINT ( 'NONE',  ( 4.380000000000002558, 1.019547802438462547, -3.750000000000000000 ) ) ;
#90309 = CARTESIAN_POINT ( 'NONE',  ( 16.40814093676323893, 0.7903013365970867898, 11.09922568453595026 ) ) ;
#90311 = CARTESIAN_POINT ( 'NONE',  ( 1.472469842513823179, 65.59226448433412315, -4.923371831947296329 ) ) ;
#90310 = CARTESIAN_POINT ( 'NONE',  ( 0.000000000000000000, 14.49999999999999822, 0.000000000000000000 ) ) ;
#90312 = CARTESIAN_POINT ( 'NONE',  ( 2.035157376598824452, 33.68868534415484106, 7.964842623401179544 ) ) ;
#90313 = CARTESIAN_POINT ( 'NONE',  ( 5.076628168052704559, 45.17559781766745175, -8.527530157486179263 ) ) ;
#90314 = CARTESIAN_POINT ( 'NONE',  ( 12.63842701281683922, 19.55059781766745175, -9.846743663894590881 ) ) ;
#90315 = CARTESIAN_POINT ( 'NONE',  ( 10.00000000000000178, 2.258931151000784787, 9.846743663894594434 ) ) ;
#90317 = ORIENTED_EDGE ( 'NONE', *, *, #5682, .T. ) ;
#90316 = CARTESIAN_POINT ( 'NONE',  ( 22.81628187352647785, 1.415301336597087012, 3.434112377981063169 ) ) ;
#90318 =( NAMED_UNIT ( * ) PLANE_ANGLE_UNIT ( ) SI_UNIT ( $, .RADIAN. ) );
#90319 = CARTESIAN_POINT ( 'NONE',  ( 18.52753015748617571, 58.09226448433411605, 4.923371831947298993 ) ) ;
#90320 = CIRCLE ( 'NONE', #931, 15.00000000000000000 ) ;
#90321 = CARTESIAN_POINT ( 'NONE',  ( 1.472469842513823179, 31.42559781766745530, 4.923371831947296329 ) ) ;
#90322 = CARTESIAN_POINT ( 'NONE',  ( 6.579634127946653699, -87.99828267815713900, -2.500000000000001332 ) ) ;
#90323 = CARTESIAN_POINT ( 'NONE',  ( -4.164238869374099927, 67.01208216824728936, 3.795296366450308767 ) ) ;
#90324 = CARTESIAN_POINT ( 'NONE',  ( 17.20831665107776587, 39.13393115100079456, -7.208316651077762316 ) ) ;
#90325 = CARTESIAN_POINT ( 'NONE',  ( 20.15039907845753930, 70.00000000000000000, 6.262539305110068177 ) ) ;
#90326 = CARTESIAN_POINT ( 'NONE',  ( 13.79529636645031943, 65.34541550158063217, -14.16423886937409904 ) ) ;
#90327 = CARTESIAN_POINT ( 'NONE',  ( -5.418184704451246780, 0.000000000000000000, 0.6173241701922714819 ) ) ;
#90328 = EDGE_CURVE ( 'NONE', #70993, #72571, #37023, .T. ) ;
#90329 = CARTESIAN_POINT ( 'NONE',  ( 15.44008868035555793, 16.39701867748817321, -9.422509992056140149 ) ) ;
#90330 = CARTESIAN_POINT ( 'NONE',  ( 10.00000000000000000, 55.55374883491396787, -14.16423886937410082 ) ) ;
#90332 = DIRECTION ( 'NONE',  ( 0.000000000000000000, 0.000000000000000000, -1.000000000000000000 ) ) ;
#90331 = CARTESIAN_POINT ( 'NONE',  ( -4.164238869374098151, 51.59541550158063217, -3.795296366450310543 ) ) ;
#90333 = SURFACE_STYLE_FILL_AREA ( #23352 ) ;
#90334 = CARTESIAN_POINT ( 'NONE',  ( 5.076628168052704559, 25.17559781766745175, -8.527530157486179263 ) ) ;
#90335 = CARTESIAN_POINT ( 'NONE',  ( 22.81628187352647785, 6.623634669930420493, 6.195893100308588602E-16 ) ) ;
#90336 = ORIENTED_EDGE ( 'NONE', *, *, #81160, .T. ) ;
#90337 = VECTOR ( 'NONE', #15238, 1000.000000000000000 ) ;
#90338 = CARTESIAN_POINT ( 'NONE',  ( 11.01793658010034704, -96.10624868222545558, 3.750000000000000444 ) ) ;
#90339 = CARTESIAN_POINT ( 'NONE',  ( 1.472469842513823179, 60.59226448433412315, -4.923371831947296329 ) ) ;
#90340 = FACE_OUTER_BOUND ( 'NONE', #11285, .T. ) ;
#90341 = EDGE_CURVE ( 'NONE', #58602, #17129, #23107, .T. ) ;
#90342 = CARTESIAN_POINT ( 'NONE',  ( 6.715867195167449566, 4.285122813354096929E-16, -12.85095824508326956 ) ) ;
#90343 = CARTESIAN_POINT ( 'NONE',  ( 17.08211943468705840, 15.13708216824730179, -12.26659068614894466 ) ) ;
#90344 = CARTESIAN_POINT ( 'NONE',  ( 19.84674366389459266, 28.71726448433411960, -2.638427012816827677 ) ) ;
#90345 = CARTESIAN_POINT ( 'NONE',  ( 2.917880565312948704, 37.63708216824731068, 12.26659068614894643 ) ) ;
#90346 = CARTESIAN_POINT ( 'NONE',  ( 19.84674366389459621, 8.508931151000785675, 7.409399052514197653E-17 ) ) ;
#90348 = CARTESIAN_POINT ( 'NONE',  ( -2.393480905992962704, 0.3639310596586416979, -14.80781041047758073 ) ) ;
#90347 = CARTESIAN_POINT ( 'NONE',  ( -7.079903288618116797, -69.52484394646381816, -2.750000000000000000 ) ) ;
#90349 = CARTESIAN_POINT ( 'NONE',  ( 2.035157376598822676, 32.43868534415483396, -7.964842623401177768 ) ) ;
#90350 = CARTESIAN_POINT ( 'NONE',  ( 6.565887622018943937, 38.08196800326376064, -12.81628187352647608 ) ) ;
#90351 = CARTESIAN_POINT ( 'NONE',  ( 12.91533473730993009, 6.605352010821504471, -10.88017736071109987 ) ) ;
#90352 = CARTESIAN_POINT ( 'NONE',  ( -1.099225684535947600, 38.70696800326375353, -6.408140936763238038 ) ) ;
#90353 = CARTESIAN_POINT ( 'NONE',  ( 3.591859063236763294, 58.29030133659708923, -11.09922568453595026 ) ) ;
#90354 = VERTEX_POINT ( 'NONE', #11907 ) ;
#90355 = FILL_AREA_STYLE ('',( #45870 ) ) ;
#90356 = CARTESIAN_POINT ( 'NONE',  ( 8.629999999999991900, 70.25000000000000000, -6.500000000000000888 ) ) ;
#90357 = CARTESIAN_POINT ( 'NONE',  ( 22.26659068614895176, 44.72041550158063927, -7.082119434687042414 ) ) ;
#90358 = CARTESIAN_POINT ( 'NONE',  ( 22.26659068614895176, 4.720415501580633943, -7.082119434687042414 ) ) ;
#90359 = CARTESIAN_POINT ( 'NONE',  ( 20.88017736071110519, 10.56368534415483751, 2.639326808657452039E-16 ) ) ;
#90360 = CARTESIAN_POINT ( 'NONE',  ( 19.42250999205614193, 20.14701867748817321, 5.440088680355555262 ) ) ;
#90361 = CARTESIAN_POINT ( 'NONE',  ( 10.04796213703179220, 15.00000000000000888, -10.62905469192465091 ) ) ;
#90362 = LINE ( 'NONE', #67887, #54359 ) ;
#90364 = B_SPLINE_CURVE_WITH_KNOTS ( 'NONE', 3,
 ( #38315, #75806, #61779, #77275 ),
 .UNSPECIFIED., .F., .F.,
 ( 4, 4 ),
 ( 9.697399036122160616E-19, 0.002392975128318514545 ),
 .UNSPECIFIED. ) ;
#90363 = CARTESIAN_POINT ( 'NONE',  ( 10.00000000000000000, 46.81368534415484106, -10.88017736071110342 ) ) ;
#90365 = CARTESIAN_POINT ( 'NONE',  ( 4.559911319644449179, 62.23035201082150536, -9.422509992056141925 ) ) ;
#90366 = CARTESIAN_POINT ( 'NONE',  ( 0.6178305044545818747, 23.49863466993041783, -9.382169495545419124 ) ) ;
#90367 = LINE ( 'NONE', #73896, #97029 ) ;
#90368 = CARTESIAN_POINT ( 'NONE',  ( 3.469446951953614189E-15, 3.912123368507817833, 11.92686044187656513 ) ) ;
#90369 = CARTESIAN_POINT ( 'NONE',  ( 7.361572987183170547, 17.05059781766745530, 9.846743663894590881 ) ) ;
#90370 = CARTESIAN_POINT ( 'NONE',  ( 19.42250999205614193, 60.14701867748817676, 5.440088680355555262 ) ) ;
#90371 = AXIS2_PLACEMENT_3D ( 'NONE', #27433, #56949, #87935 ) ;
#90372 = UNCERTAINTY_MEASURE_WITH_UNIT (LENGTH_MEASURE( 1.000000000000000082E-05 ), #73522, 'distance_accuracy_value', 'NONE');
#90373 = VECTOR ( 'NONE', #91153, 1000.000000000000000 ) ;
#90374 = CARTESIAN_POINT ( 'NONE',  ( 13.43411237798106583, 12.66530133659708746, -12.81628187352647252 ) ) ;
#90375 = CARTESIAN_POINT ( 'NONE',  ( 15.44008868035555260, 9.730352010821505360, 9.422509992056143702 ) ) ;
#90376 = CARTESIAN_POINT ( 'NONE',  ( 0.1532563361054100626, 40.80059781766745886, -2.638427012816831230 ) ) ;
#90377 = CARTESIAN_POINT ( 'NONE',  ( -8.209432707285007069, 14.49999999999999112, 12.55409154915484393 ) ) ;
#90378 = CARTESIAN_POINT ( 'NONE',  ( 7.361572987183170547, 17.05059781766745530, 9.846743663894590881 ) ) ;
#90379 =( LENGTH_UNIT ( ) NAMED_UNIT ( * ) SI_UNIT ( .MILLI., .METRE. ) );
#90380 = CARTESIAN_POINT ( 'NONE',  ( 20.88017736071110519, 30.56368534415484106, 2.639326808657452039E-16 ) ) ;
#90381 = CARTESIAN_POINT ( 'NONE',  ( -0.8801773607111009756, 33.06368534415484106, 1.068504757029289695E-15 ) ) ;
#90382 = CARTESIAN_POINT ( 'NONE',  ( 20.36894250292379738, 34.92874883491396076, -10.36894250292379027 ) ) ;
#90383 = CARTESIAN_POINT ( 'NONE',  ( 7.361572987183169658, 44.96726448433412315, -9.846743663894592657 ) ) ;
#90384 = CARTESIAN_POINT ( 'NONE',  ( -0.8801773607110991993, 27.85535201082150181, -2.915334737309923874 ) ) ;
#90385 = EDGE_CURVE ( 'NONE', #63123, #7097, #74173, .T. ) ;
#90386 = CARTESIAN_POINT ( 'NONE',  ( 2.035157376598824452, 18.68868534415484106, 7.964842623401179544 ) ) ;
#90387 = ORIENTED_EDGE ( 'NONE', *, *, #53184, .F. ) ;
#90388 = CARTESIAN_POINT ( 'NONE',  ( 20.88017736071110164, 30.35535201082151247, 2.915334737309930979 ) ) ;
#90389 = EDGE_CURVE ( 'NONE', #58376, #76182, #94959, .T. ) ;
#90390 = CARTESIAN_POINT ( 'NONE',  ( 10.00000000000000000, 47.87363466993042493, -12.81628187352647608 ) ) ;
#90391 = CARTESIAN_POINT ( 'NONE',  ( 19.42250999205614193, 30.14701867748817321, 5.440088680355555262 ) ) ;
#90392 = CARTESIAN_POINT ( 'NONE',  ( -12.25993886608596029, 14.63606888159244690, -8.642563219313824874 ) ) ;
#90393 = ORIENTED_EDGE ( 'NONE', *, *, #59994, .T. ) ;
#90394 = CARTESIAN_POINT ( 'NONE',  ( 19.84674366389459266, 58.30059781766745886, 2.638427012816836559 ) ) ;
#90395 = CARTESIAN_POINT ( 'NONE',  ( 0.5774900079438607392, 33.48035201082150536, 5.440088680355550821 ) ) ;
#90396 = CARTESIAN_POINT ( 'NONE',  ( 0.4400000000000020006, 1.019547802438468986, -2.750000000000000000 ) ) ;
#90397 = DIRECTION ( 'NONE',  ( -0.000000000000000000, -0.000000000000000000, -1.000000000000000000 ) ) ;
#90398 = CARTESIAN_POINT ( 'NONE',  ( 2.917880565312948704, 47.63708216824730357, 12.26659068614894643 ) ) ;
#90399 = CARTESIAN_POINT ( 'NONE',  ( 10.00000000000000000, 56.81368534415484106, -10.88017736071110342 ) ) ;
#90400 = FILL_AREA_STYLE_COLOUR ( '', #3552 ) ;
#90401 = DIRECTION ( 'NONE',  ( -0.000000000000000000, 1.000000000000000000, 0.000000000000000000 ) ) ;
#90402 = CARTESIAN_POINT ( 'NONE',  ( 7.361572987183170547, 67.05059781766746596, 9.846743663894590881 ) ) ;
#90403 = DIRECTION ( 'NONE',  ( 0.06975647374410356982, 0.9975640502598257520, -0.000000000000000000 ) ) ;
#90404 = CARTESIAN_POINT ( 'NONE',  ( 17.20831665107776587, 32.88393115100078745, 7.208316651077764980 ) ) ;
#90405 = CARTESIAN_POINT ( 'NONE',  ( 0.1532563361054082862, 41.21726448433411605, 2.638427012816831674 ) ) ;
#90406 = CARTESIAN_POINT ( 'NONE',  ( 3.434112377981054287, -22.33469866340291077, -12.81628187352647608 ) ) ;
#90407 = CARTESIAN_POINT ( 'NONE',  ( 10.00000000000000000, 31.81368534415483751, -10.88017736071110342 ) ) ;
#90408 = CARTESIAN_POINT ( 'NONE',  ( 7.361572987183170547, 27.05059781766745175, 9.846743663894590881 ) ) ;
#90409 = CARTESIAN_POINT ( 'NONE',  ( 22.81628187352648496, 21.83196800326374643, -3.434112377981050290 ) ) ;
#90411 = CARTESIAN_POINT ( 'NONE',  ( 10.00000000000000000, 61.81368534415484106, -10.88017736071110342 ) ) ;
#90410 = CYLINDRICAL_SURFACE ( 'NONE', #77053, 3.000000000000000888 ) ;
#90413 = CARTESIAN_POINT ( 'NONE',  ( 2.035157376598822676, 7.438685344154837509, -7.964842623401177768 ) ) ;
#90412 = CARTESIAN_POINT ( 'NONE',  ( 0.5774900079438607392, 33.48035201082150536, 5.440088680355550821 ) ) ;
#90414 = CARTESIAN_POINT ( 'NONE',  ( -4.164238869374098151, 46.59541550158063927, -3.795296366450310543 ) ) ;
#90415 = CIRCLE ( 'NONE', #72850, 0.5000000000000004441 ) ;
#90416 = EDGE_CURVE ( 'NONE', #60398, #72885, #26405, .T. ) ;
#90417 = CARTESIAN_POINT ( 'NONE',  ( 0.000000000000000000, 14.49999999999999822, 0.000000000000000000 ) ) ;
#90418 = ORIENTED_EDGE ( 'NONE', *, *, #83556, .F. ) ;
#90419 = CARTESIAN_POINT ( 'NONE',  ( -2.816281873526473856, 14.12363466993041961, 9.499525473075851096E-16 ) ) ;
#90420 = CARTESIAN_POINT ( 'NONE',  ( 12.91533473730992121, 9.522018677488171434, 10.88017736071110164 ) ) ;
#90421 = EDGE_CURVE ( 'NONE', #13765, #18862, #40563, .T. ) ;
#90422 = CARTESIAN_POINT ( 'NONE',  ( -0.8801773607110991993, 52.85535201082151247, -2.915334737309923874 ) ) ;
#90423 = PRESENTATION_STYLE_ASSIGNMENT (( #30420 ) ) ;
#90424 = ORIENTED_EDGE ( 'NONE', *, *, #56594, .T. ) ;
#90425 = CARTESIAN_POINT ( 'NONE',  ( 4.559911319644449179, 53.89701867748817676, 9.422509992056141925 ) ) ;
#90426 = CARTESIAN_POINT ( 'NONE',  ( 7.361572987183170547, 32.05059781766745175, 9.846743663894590881 ) ) ;
#90427 = CARTESIAN_POINT ( 'NONE',  ( 5.076628168052704559, 25.17559781766745175, -8.527530157486179263 ) ) ;
#90428 = CIRCLE ( 'NONE', #32913, 2.900000000000002576 ) ;
#90429 = CARTESIAN_POINT ( 'NONE',  ( 18.52753015748618282, 13.92559781766745175, -4.923371831947291888 ) ) ;
#90431 = CARTESIAN_POINT ( 'NONE',  ( 16.40814093676324603, 37.45696800326376064, -11.09922568453594671 ) ) ;
#90430 = CARTESIAN_POINT ( 'NONE',  ( -5.809210876173504623, -36.07757871006354122, 2.500000000001614264 ) ) ;
#90433 = CARTESIAN_POINT ( 'NONE',  ( 0.000000000000000000, 15.00000000000000000, 0.000000000000000000 ) ) ;
#90432 = CARTESIAN_POINT ( 'NONE',  ( 5.076628168052703671, 1.842264484334118047, 8.527530157486179263 ) ) ;
#90434 = CARTESIAN_POINT ( 'NONE',  ( 7.185089000015953964, -80.58569572050204499, -4.000000000000000000 ) ) ;
#90436 = ORIENTED_EDGE ( 'NONE', *, *, #76203, .T. ) ;
#90435 = CARTESIAN_POINT ( 'NONE',  ( 10.00000000000000178, 32.25893115100078745, 9.846743663894594434 ) ) ;
#90437 = CARTESIAN_POINT ( 'NONE',  ( 0.6178305044545818747, 58.49863466993042493, -9.382169495545419124 ) ) ;
#90438 = FACE_OUTER_BOUND ( 'NONE', #62665, .T. ) ;
#90439 = CARTESIAN_POINT ( 'NONE',  ( 16.40814093676324603, 7.456968003263754419, -11.09922568453594671 ) ) ;
#90440 = EDGE_CURVE ( 'NONE', #25641, #50375, #11856, .T. ) ;
#90441 = EDGE_CURVE ( 'NONE', #61835, #57201, #89434, .T. ) ;
#90442 = CARTESIAN_POINT ( 'NONE',  ( 19.42250999205614193, 55.14701867748817676, 5.440088680355555262 ) ) ;
#90443 = VECTOR ( 'NONE', #81093, 1000.000000000000000 ) ;
#90444 = CARTESIAN_POINT ( 'NONE',  ( -2.266590686148945544, 31.38708216824730002, -7.082119434687050408 ) ) ;
#90445 = UNCERTAINTY_MEASURE_WITH_UNIT (LENGTH_MEASURE( 1.000000000000000082E-05 ), #16978, 'distance_accuracy_value', 'NONE');
#90446 = CARTESIAN_POINT ( 'NONE',  ( -8.051738205446136831, 84.95449735710184314, 3.788866803286794038 ) ) ;
#90447 = CARTESIAN_POINT ( 'NONE',  ( 22.26659068614894466, 28.88708216824730357, 7.082119434687054849 ) ) ;
#90448 = EDGE_CURVE ( 'NONE', #19669, #62224, #42409, .T. ) ;
#90449 = CARTESIAN_POINT ( 'NONE',  ( -4.164238869374099927, 42.01208216824728936, 3.795296366450308767 ) ) ;
#90450 = CARTESIAN_POINT ( 'NONE',  ( 17.08211943468705130, 13.47041550158063572, 12.26659068614894998 ) ) ;
#90452 = CARTESIAN_POINT ( 'NONE',  ( 15.44008868035555793, 66.39701867748817676, -9.422509992056140149 ) ) ;
#90451 = CARTESIAN_POINT ( 'NONE',  ( -4.164238869374099927, 7.012082168247302683, 3.795296366450308767 ) ) ;
#90453 = CARTESIAN_POINT ( 'NONE',  ( -0.8801773607110991993, 42.85535201082150536, -2.915334737309923874 ) ) ;
#90454 = CARTESIAN_POINT ( 'NONE',  ( 0.000000000000000000, 14.49999999999999822, 0.000000000000000000 ) ) ;
#90455 = CARTESIAN_POINT ( 'NONE',  ( 17.20831665107776587, 32.88393115100078745, 7.208316651077764980 ) ) ;
#90457 = CARTESIAN_POINT ( 'NONE',  ( 2.791683348922237240, 30.38393115100078390, -7.208316651077763204 ) ) ;
#90456 = DIRECTION ( 'NONE',  ( 0.000000000000000000, 1.000000000000000000, -0.000000000000000000 ) ) ;
#90458 = VECTOR ( 'NONE', #76252, 1000.000000000000000 ) ;
#90459 = CARTESIAN_POINT ( 'NONE',  ( -0.8801773607111008646, 28.27201867748817321, 2.915334737309923430 ) ) ;
#90460 = CARTESIAN_POINT ( 'NONE',  ( 21.09922568453594849, 56.20696800326375353, 6.408140936763242479 ) ) ;
#90461 = CARTESIAN_POINT ( 'NONE',  ( 1.472469842513823179, 60.59226448433412315, -4.923371831947296329 ) ) ;
#90462 = FACE_OUTER_BOUND ( 'NONE', #28774, .T. ) ;
#90463 = CARTESIAN_POINT ( 'NONE',  ( 19.84674366389459266, 28.30059781766745886, 2.638427012816836559 ) ) ;
#90465 = CARTESIAN_POINT ( 'NONE',  ( 3.591859063236763294, 38.29030133659708923, -11.09922568453595026 ) ) ;
#90464 = VECTOR ( 'NONE', #90711, 1000.000000000000000 ) ;
#90466 = CARTESIAN_POINT ( 'NONE',  ( -12.26659068614895354, -13.61291783175269643, -7.082119434687038861 ) ) ;
#90467 = CARTESIAN_POINT ( 'NONE',  ( 20.88017736071110164, 40.35535201082150536, 2.915334737309930979 ) ) ;
#90468 = CARTESIAN_POINT ( 'NONE',  ( 2.791683348922240793, 56.63393115100078035, 7.208316651077764092 ) ) ;
#90469 = CARTESIAN_POINT ( 'NONE',  ( 2.917880565312950480, 20.97041550158063217, -12.26659068614894821 ) ) ;
#90470 = ORIENTED_EDGE ( 'NONE', *, *, #5771, .T. ) ;
#90471 = DIRECTION ( 'NONE',  ( 0.8433914458128921599, 0.000000000000000000, -0.5372996083468138950 ) ) ;
#90472 = B_SPLINE_CURVE_WITH_KNOTS ( 'NONE', 3,
 ( #17883, #62880, #39894, #32869, #63369, #48856 ),
 .UNSPECIFIED., .F., .F.,
 ( 4, 2, 4 ),
 ( 3.409110551496086645E-05, 0.0004400426677367858127, 0.0008459942299586108334 ),
 .UNSPECIFIED. ) ;
#90473 = CARTESIAN_POINT ( 'NONE',  ( 4.559911319644449179, 58.89701867748817676, 9.422509992056141925 ) ) ;
#90474 = CARTESIAN_POINT ( 'NONE',  ( 10.70613742633613796, 15.00000000000000000, 9.778988772292906972 ) ) ;
#90475 = CARTESIAN_POINT ( 'NONE',  ( 13.79529636645030344, 53.26208216824730357, 14.16423886937410614 ) ) ;
#90476 = CARTESIAN_POINT ( 'NONE',  ( 19.38216949554541557, 2.248634669930420049, -9.382169495545420901 ) ) ;
#90477 = CARTESIAN_POINT ( 'NONE',  ( 0.5774900079438590739, 57.64701867748817676, -5.440088680355550821 ) ) ;
#90478 = CARTESIAN_POINT ( 'NONE',  ( 1.114591949024916984, 15.00000000000000000, 14.45709807627962817 ) ) ;
#90479 = B_SPLINE_CURVE_WITH_KNOTS ( 'NONE', 3,
 ( #73155, #96682, #97183, #50167, #88164, #88660 ),
 .UNSPECIFIED., .F., .F.,
 ( 4, 2, 4 ),
 ( 3.409110551496134756E-05, 0.0004400426677367868427, 0.0008459942299586123513 ),
 .UNSPECIFIED. ) ;
#90480 = CARTESIAN_POINT ( 'NONE',  ( -5.204170427930421283E-15, 21.81368534415484106, -10.88017736071110342 ) ) ;
#90481 = CARTESIAN_POINT ( 'NONE',  ( 4.559911319644449179, 7.230352010821504471, -9.422509992056141925 ) ) ;
#90482 = CARTESIAN_POINT ( 'NONE',  ( 15.44008868035555260, 9.730352010821505360, 9.422509992056143702 ) ) ;
#90483 = CARTESIAN_POINT ( 'NONE',  ( 17.20831665107776587, 59.13393115100078745, -7.208316651077762316 ) ) ;
#90484 = VECTOR ( 'NONE', #88403, 1000.000000000000114 ) ;
#90485 = CARTESIAN_POINT ( 'NONE',  ( 3.591859063236763294, 53.29030133659708923, -11.09922568453595026 ) ) ;
#90486 = DIRECTION ( 'NONE',  ( 0.8320502943378436100, -0.5547001962252291474, 0.000000000000000000 ) ) ;
#90487 = ORIENTED_EDGE ( 'NONE', *, *, #83129, .F. ) ;
#90488 = CARTESIAN_POINT ( 'NONE',  ( 7.084665262690076126, 14.10535201082150358, 10.88017736071109987 ) ) ;
#90489 = CARTESIAN_POINT ( 'NONE',  ( 22.81628187352647785, 16.41530133659708923, 3.434112377981063169 ) ) ;
#90490 = FACE_OUTER_BOUND ( 'NONE', #40609, .T. ) ;
#90491 = CARTESIAN_POINT ( 'NONE',  ( 0.1532563361054100626, 5.800597817667452638, -2.638427012816831230 ) ) ;
#90492 = VECTOR ( 'NONE', #10150, 1000.000000000000000 ) ;
#90493 = CARTESIAN_POINT ( 'NONE',  ( 18.52753015748618282, 48.92559781766745886, -4.923371831947291888 ) ) ;
#90494 = CARTESIAN_POINT ( 'NONE',  ( 17.96484262340118221, 34.93868534415482685, 7.964842623401181321 ) ) ;
#90495 = AXIS2_PLACEMENT_3D ( 'NONE', #69184, #69669, #46662 ) ;
#90496 = CARTESIAN_POINT ( 'NONE',  ( 22.81628187352647785, 26.62363466993042138, 6.195893100308588602E-16 ) ) ;
#90498 = CARTESIAN_POINT ( 'NONE',  ( 17.99999999999999645, 91.28723161455539525, 8.000000000000000000 ) ) ;
#90497 = CARTESIAN_POINT ( 'NONE',  ( 2.035157376598824452, 43.68868534415484106, 7.964842623401179544 ) ) ;
#90499 = FACE_OUTER_BOUND ( 'NONE', #83796, .T. ) ;
#90500 = CARTESIAN_POINT ( 'NONE',  ( 22.81628187352647785, 51.41530133659708923, 3.434112377981063169 ) ) ;
#90501 = EDGE_LOOP ( 'NONE', ( #37654, #39663, #71258, #90048 ) ) ;
#90502 = PLANE ( 'NONE',  #71790 ) ;
#90503 = CARTESIAN_POINT ( 'NONE',  ( -0.8801773607111008646, 53.27201867748816966, 2.915334737309923430 ) ) ;
#90505 = CARTESIAN_POINT ( 'NONE',  ( 13.79529636645031943, 5.345415501580634832, -14.16423886937409904 ) ) ;
#90504 = CARTESIAN_POINT ( 'NONE',  ( -2.816281873526473856, 39.33196800326374643, 3.434112377981055619 ) ) ;
#90506 = CARTESIAN_POINT ( 'NONE',  ( 12.91533473730992121, 44.52201867748816966, 10.88017736071110164 ) ) ;
#90507 = DIRECTION ( 'NONE',  ( 0.000000000000000000, 0.000000000000000000, 1.000000000000000000 ) ) ;
#90508 = FILL_AREA_STYLE_COLOUR ( '', #1920 ) ;
#90509 = CARTESIAN_POINT ( 'NONE',  ( 12.63842701281683034, 22.46726448433411605, 9.846743663894596210 ) ) ;
#90510 = CARTESIAN_POINT ( 'NONE',  ( 10.00000000000000000, 4.758931151000784787, -9.846743663894594434 ) ) ;
#90511 = CARTESIAN_POINT ( 'NONE',  ( 13.61464873478167981, 0.3640475087720990155, -6.296136897217838424 ) ) ;
#90512 = CARTESIAN_POINT ( 'NONE',  ( 13.79529636645031943, 40.34541550158063217, -14.16423886937409904 ) ) ;
#90513 = CARTESIAN_POINT ( 'NONE',  ( 20.15039907845753220, 24.72266099184919241, 6.262539305110077947 ) ) ;
#90514 = EDGE_CURVE ( 'NONE', #74236, #78251, #64598, .T. ) ;
#90515 = SURFACE_STYLE_FILL_AREA ( #60020 ) ;
#90516 = CARTESIAN_POINT ( 'NONE',  ( -5.811454672306065383, -36.11427488547452214, -3.750000000000000000 ) ) ;
#90517 = ORIENTED_EDGE ( 'NONE', *, *, #41583, .F. ) ;
#90518 = CARTESIAN_POINT ( 'NONE',  ( -4.164238869374098151, 66.59541550158060375, -3.795296366450310543 ) ) ;
#90519 = CARTESIAN_POINT ( 'NONE',  ( 10.00000000000000178, 68.05374883491397497, 14.16423886937410082 ) ) ;
#90520 = CARTESIAN_POINT ( 'NONE',  ( 10.00000000000000000, 24.75893115100078745, -9.846743663894594434 ) ) ;
#90521 = CARTESIAN_POINT ( 'NONE',  ( 6.565887622018943937, 38.08196800326376064, -12.81628187352647608 ) ) ;
#90522 = FILL_AREA_STYLE ('',( #59045 ) ) ;
#90524 = CARTESIAN_POINT ( 'NONE',  ( 20.36894250292379738, 9.928748834913966093, -10.36894250292379027 ) ) ;
#90523 = CARTESIAN_POINT ( 'NONE',  ( -10.91371419741714277, 89.69638457836573764, -6.151049038649611056 ) ) ;
#90525 = CARTESIAN_POINT ( 'NONE',  ( -0.8801773607111009756, 8.063685344154837509, 1.068504757029289695E-15 ) ) ;
#90526 = CARTESIAN_POINT ( 'NONE',  ( 13.79529636645031943, 55.34541550158062506, -14.16423886937409904 ) ) ;
#90527 = AXIS2_PLACEMENT_3D ( 'NONE', #33618, #86651, #32652 ) ;
#90528 = CARTESIAN_POINT ( 'NONE',  ( 19.84674366389459266, 33.30059781766744464, 2.638427012816836559 ) ) ;
#90529 =( BOUNDED_CURVE ( )  B_SPLINE_CURVE ( 2, ( #23813, #61291, #76787, #75310, #7326, #98838, #6821, #22819, #83807 ),
 .UNSPECIFIED., .F., .T. ) 
 B_SPLINE_CURVE_WITH_KNOTS ( ( 3, 2, 2, 2, 3 ),
 ( 0.6544266512259456769, 0.6547619047619047672, 0.6607142857142858094, 0.6666666666666667407, 0.6670019202026259419 ),
 .UNSPECIFIED. ) 
 CURVE ( )  GEOMETRIC_REPRESENTATION_ITEM ( )  RATIONAL_B_SPLINE_CURVE ( ( 0.9963778908391764944, 0.9980808541467923733, 1.000000000000000000, 0.9659258262890682012, 1.000000000000000000, 0.9659258262890682012, 1.000000000000000000, 0.9980808541467917072, 0.9963778908391753841 ) ) 
 REPRESENTATION_ITEM ( '' )  );
#90530 = CARTESIAN_POINT ( 'NONE',  ( 19.05866839779139710, 40.95508385108959004, -6.499999999999974243 ) ) ;
#90531 = CARTESIAN_POINT ( 'NONE',  ( 5.076628168052703671, 16.84226448433411960, 8.527530157486179263 ) ) ;
#90532 = DIRECTION ( 'NONE',  ( 0.000000000000000000, 0.000000000000000000, 1.000000000000000000 ) ) ;
#90533 = CARTESIAN_POINT ( 'NONE',  ( 4.923371831947295441, 19.34226448433412671, -8.527530157486179263 ) ) ;
#90534 = ORIENTED_EDGE ( 'NONE', *, *, #44400, .T. ) ;
#90535 = ORIENTED_EDGE ( 'NONE', *, *, #29070, .T. ) ;
#90536 = LINE ( 'NONE', #83546, #95682 ) ;
#90537 = EDGE_LOOP ( 'NONE', ( #65188, #3528, #86165, #22436 ) ) ;
#90539 = CARTESIAN_POINT ( 'NONE',  ( 7.361572987183170547, 47.05059781766745175, 9.846743663894590881 ) ) ;
#90538 = TOROIDAL_SURFACE ( 'NONE', #33082, 14.49999999999999822, 0.5000000000000000000 ) ;
#90540 = CARTESIAN_POINT ( 'NONE',  ( 20.36894250292379738, 19.92874883491396787, -10.36894250292379027 ) ) ;
#90542 = CARTESIAN_POINT ( 'NONE',  ( 7.084665262690076126, 34.10535201082151247, 10.88017736071109987 ) ) ;
#90541 = CARTESIAN_POINT ( 'NONE',  ( 2.035157376598824452, 38.68868534415483396, 7.964842623401179544 ) ) ;
#90544 = CARTESIAN_POINT ( 'NONE',  ( 10.00000000000000178, 35.37363466993042493, 12.81628187352647608 ) ) ;
#90543 = CARTESIAN_POINT ( 'NONE',  ( 19.84674366389459266, 63.71726448433412315, -2.638427012816827677 ) ) ;
#90545 = CARTESIAN_POINT ( 'NONE',  ( 24.16423886937409904, 4.095415501580634832, 3.795296366450317205 ) ) ;
#90546 = CIRCLE ( 'NONE', #25048, 0.5000000000000000000 ) ;
#90547 = COLOUR_RGB ( '', 0.40784314, 0.44705882, 0.49803922) ;
#90548 = ADVANCED_FACE ( 'NONE', ( #57398 ), #70093, .T. ) ;
#90549 = CARTESIAN_POINT ( 'NONE',  ( 22.81628187352648496, 31.83196800326375353, -3.434112377981050290 ) ) ;
#90550 = EDGE_LOOP ( 'NONE', ( #84268, #36809, #2549, #26932 ) ) ;
#90551 = CARTESIAN_POINT ( 'NONE',  ( 5.076628168052704559, 50.17559781766745886, -8.527530157486179263 ) ) ;
#90552 = EDGE_CURVE ( 'NONE', #43285, #24087, #18225, .T. ) ;
#90553 = CARTESIAN_POINT ( 'NONE',  ( 7.084665262690076126, 7.022018677488170546, -10.88017736071110164 ) ) ;
#90554 = ORIENTED_EDGE ( 'NONE', *, *, #49841, .F. ) ;
#90555 = CARTESIAN_POINT ( 'NONE',  ( 19.42250999205614193, 15.14701867748817143, 5.440088680355555262 ) ) ;
#90556 = ORIENTED_EDGE ( 'NONE', *, *, #33522, .F. ) ;
#90557 = CARTESIAN_POINT ( 'NONE',  ( -0.8801773607111008646, 48.27201867748816966, 2.915334737309923430 ) ) ;
#90558 = CARTESIAN_POINT ( 'NONE',  ( 2.035157376598824452, 58.68868534415482685, 7.964842623401179544 ) ) ;
#90559 = CARTESIAN_POINT ( 'NONE',  ( 19.42250999205614193, 65.14701867748817676, 5.440088680355555262 ) ) ;
#90560 = TOROIDAL_SURFACE ( 'NONE', #61792, 14.49999999999999822, 0.5000000000000000000 ) ;
#90561 = CARTESIAN_POINT ( 'NONE',  ( 7.361572987183169658, -0.03273551566588185635, -9.846743663894592657 ) ) ;
#90562 = CARTESIAN_POINT ( 'NONE',  ( 17.96484262340118221, 49.93868534415484106, 7.964842623401181321 ) ) ;
#90563 = CARTESIAN_POINT ( 'NONE',  ( -1.926860441876563801, 52.66212336850780673, 1.004413902775740978E-15 ) ) ;
#90564 = ORIENTED_EDGE ( 'NONE', *, *, #74292, .T. ) ;
#90565 = CARTESIAN_POINT ( 'NONE',  ( 2.791683348922237240, 25.38393115100078390, -7.208316651077763204 ) ) ;
#90566 = ORIENTED_EDGE ( 'NONE', *, *, #9899, .T. ) ;
#90567 = CARTESIAN_POINT ( 'NONE',  ( 0.000000000000000000, 0.000000000000000000, 0.000000000000000000 ) ) ;
#90568 = FILL_AREA_STYLE ('',( #98102 ) ) ;
#90569 =( GEOMETRIC_REPRESENTATION_CONTEXT ( 3 ) GLOBAL_UNCERTAINTY_ASSIGNED_CONTEXT ( ( #37145 ) ) GLOBAL_UNIT_ASSIGNED_CONTEXT ( ( #97413, #35403, #89396 ) ) REPRESENTATION_CONTEXT ( 'NONE', 'WORKASPACE' ) );
#90570 = CARTESIAN_POINT ( 'NONE',  ( -4.164238869374098151, 1.595415501580634388, -3.795296366450310543 ) ) ;
#90571 = EDGE_CURVE ( 'NONE', #91132, #57334, #44075, .T. ) ;
#90572 = LINE ( 'NONE', #98617, #25105 ) ;
#90573 = CARTESIAN_POINT ( 'NONE',  ( -46.76851119026090231, 103.5739182654012325, -5.803562628621293129 ) ) ;
#90574 = CARTESIAN_POINT ( 'NONE',  ( 6.204703633549690345, 67.84541550158060375, 14.16423886937410082 ) ) ;
#90575 = CARTESIAN_POINT ( 'NONE',  ( 13.21236992757670059, 0.000000000000000000, 5.338143956176803151 ) ) ;
#90576 = ORIENTED_EDGE ( 'NONE', *, *, #2304, .T. ) ;
#90577 = CARTESIAN_POINT ( 'NONE',  ( 11.59580422753459494, 0.2301505044262100452, -9.421229451859201021 ) ) ;
#90578 = CARTESIAN_POINT ( 'NONE',  ( 10.00000000000000178, 47.25893115100078745, 9.846743663894594434 ) ) ;
#90579 = DIRECTION ( 'NONE',  ( -0.6626200482157305061, 0.000000000000000000, -0.7489557207890082946 ) ) ;
#90580 = CARTESIAN_POINT ( 'NONE',  ( -1.099225684535947600, 23.70696800326375708, -6.408140936763238038 ) ) ;
#90582 = EDGE_CURVE ( 'NONE', #90354, #95793, #9562, .T. ) ;
#90581 = CARTESIAN_POINT ( 'NONE',  ( 18.52753015748618282, 18.92559781766745175, -4.923371831947291888 ) ) ;
#90583 = CARTESIAN_POINT ( 'NONE',  ( 1.816707512666850599, 30.10290668512023160, -6.499999999999995559 ) ) ;
#90584 = CARTESIAN_POINT ( 'NONE',  ( 0.1532563361054083140, 21.00893115100078745, 1.131784320476157264E-15 ) ) ;
#90585 = CARTESIAN_POINT ( 'NONE',  ( 22.81628187352647785, 6.623634669930420493, 6.195893100308588602E-16 ) ) ;
#90586 = ORIENTED_EDGE ( 'NONE', *, *, #86995, .T. ) ;
#90587 = ORIENTED_EDGE ( 'NONE', *, *, #42600, .F. ) ;
#90588 = CARTESIAN_POINT ( 'NONE',  ( 15.44008868035555260, 29.73035201082150891, 9.422509992056143702 ) ) ;
#90589 = CARTESIAN_POINT ( 'NONE',  ( 17.08211943468705840, 15.13708216824730179, -12.26659068614894466 ) ) ;
#90590 = CARTESIAN_POINT ( 'NONE',  ( 18.52753015748617571, 28.09226448433411960, 4.923371831947298993 ) ) ;
#90591 = CARTESIAN_POINT ( 'NONE',  ( -0.8801773607111009756, 58.06368534415484106, 1.068504757029289695E-15 ) ) ;
#90593 = CARTESIAN_POINT ( 'NONE',  ( -3.500000000000000444, -0.04521315095527938394, -3.750000000000000000 ) ) ;
#90592 = CARTESIAN_POINT ( 'NONE',  ( 6.565887622018943937, 43.08196800326374643, -12.81628187352647608 ) ) ;
#90594 = CARTESIAN_POINT ( 'NONE',  ( 10.00000000000000178, 14.31368534415483751, 10.88017736071110342 ) ) ;
#90595 = CARTESIAN_POINT ( 'NONE',  ( 8.979619469809167143, 27.03494536863381015, -2.900000000000000799 ) ) ;
#90596 = DIRECTION ( 'NONE',  ( -0.000000000000000000, -1.000000000000000000, -0.000000000000000000 ) ) ;
#90597 = CIRCLE ( 'NONE', #88968, 15.00000000000000000 ) ;
#90598 = CARTESIAN_POINT ( 'NONE',  ( 22.81628187352647785, 11.41530133659708390, 3.434112377981063169 ) ) ;
#90599 = CARTESIAN_POINT ( 'NONE',  ( 17.20831665107776587, 32.88393115100078745, 7.208316651077764980 ) ) ;
#90600 = CARTESIAN_POINT ( 'NONE',  ( -2.915334737309917656, -15.89464798917849109, 10.88017736071110164 ) ) ;
#90601 = CARTESIAN_POINT ( 'NONE',  ( 22.81628187352647785, 31.41530133659709279, 3.434112377981063169 ) ) ;
#90602 = CARTESIAN_POINT ( 'NONE',  ( -4.000000000000000000, 36.75000000000000000, 4.000000000000000000 ) ) ;
#90604 = CARTESIAN_POINT ( 'NONE',  ( 11.35178980618967337, 14.49999999999999822, 9.804941009311999522 ) ) ;
#90603 = CARTESIAN_POINT ( 'NONE',  ( 4.559911319644449179, 42.23035201082151247, -9.422509992056141925 ) ) ;
#90605 = CIRCLE ( 'NONE', #47505, 15.00000000000000000 ) ;
#90606 = AXIS2_PLACEMENT_3D ( 'NONE', #76677, #78156, #93645 ) ;
#90607 = DIRECTION ( 'NONE',  ( 0.000000000000000000, 0.000000000000000000, 1.000000000000000000 ) ) ;
#90608 = DIRECTION ( 'NONE',  ( -1.000000000000000000, 0.000000000000000000, 0.000000000000000000 ) ) ;
#90609 = AXIS2_PLACEMENT_3D ( 'NONE', #53504, #46496, #16508 ) ;
#90610 = CARTESIAN_POINT ( 'NONE',  ( -0.8801773607110991993, 37.85535201082151247, -2.915334737309923874 ) ) ;
#90611 = CARTESIAN_POINT ( 'NONE',  ( 7.084665262690076126, 47.02201867748818387, -10.88017736071110164 ) ) ;
#90612 = CARTESIAN_POINT ( 'NONE',  ( 7.361572987183170547, 67.05059781766746596, 9.846743663894590881 ) ) ;
#90613 = CARTESIAN_POINT ( 'NONE',  ( 12.91533473730993009, 61.60535201082150536, -10.88017736071109987 ) ) ;
#90614 = CARTESIAN_POINT ( 'NONE',  ( 12.63842701281683034, 37.46726448433411605, 9.846743663894596210 ) ) ;
#90615 = CARTESIAN_POINT ( 'NONE',  ( 19.42250999205614548, 10.98035201082150358, -5.440088680355545492 ) ) ;
#90616 = CARTESIAN_POINT ( 'NONE',  ( 21.09922568453594849, 16.20696800326375353, 6.408140936763242479 ) ) ;
#90617 = ORIENTED_EDGE ( 'NONE', *, *, #94605, .T. ) ;
#90618 = CARTESIAN_POINT ( 'NONE',  ( 19.42250999205614193, 30.14701867748817321, 5.440088680355555262 ) ) ;
#90619 = CARTESIAN_POINT ( 'NONE',  ( 4.130000000000002558, 1.019547802438464545, -2.500000000000000000 ) ) ;
#90620 = CARTESIAN_POINT ( 'NONE',  ( 20.88017736071110164, 25.35535201082150891, 2.915334737309930979 ) ) ;
#90621 = CARTESIAN_POINT ( 'NONE',  ( 4.559911319644449179, 63.89701867748817676, 9.422509992056141925 ) ) ;
#90622 = CARTESIAN_POINT ( 'NONE',  ( 2.917880565312948704, 32.63708216824730357, 12.26659068614894643 ) ) ;
#90623 = CARTESIAN_POINT ( 'NONE',  ( 1.472469842513823179, 30.59226448433411960, -4.923371831947296329 ) ) ;
#90624 = CARTESIAN_POINT ( 'NONE',  ( 0.5774900079438607392, 43.48035201082151247, 5.440088680355550821 ) ) ;
#90625 = CARTESIAN_POINT ( 'NONE',  ( 8.721827932837868502, 14.99999999999802291, -11.74045266257544462 ) ) ;
#90626 = CARTESIAN_POINT ( 'NONE',  ( 20.36894250292379382, 3.678748834913967869, 10.36894250292379205 ) ) ;
#90627 = EDGE_CURVE ( 'NONE', #21427, #8937, #40657, .T. ) ;
#90628 = VERTEX_POINT ( 'NONE', #32715 ) ;
#90629 = DIRECTION ( 'NONE',  ( -1.000000000000000000, 5.818595309480552676E-17, 0.000000000000000000 ) ) ;
#90630 = CARTESIAN_POINT ( 'NONE',  ( 1.472469842513823179, 61.42559781766745175, 4.923371831947296329 ) ) ;
#90631 = VERTEX_POINT ( 'NONE', #63213 ) ;
#90632 = VERTEX_POINT ( 'NONE', #24745 ) ;
#90633 = CARTESIAN_POINT ( 'NONE',  ( 1.274849032794292736, 62.55509018479936145, -6.499999999999977796 ) ) ;
#90634 = CARTESIAN_POINT ( 'NONE',  ( 13.79529636645031943, 15.34541550158063750, -14.16423886937409904 ) ) ;
#90635 = CARTESIAN_POINT ( 'NONE',  ( 2.917880565312948704, 27.63708216824730357, 12.26659068614894643 ) ) ;
#90636 = CARTESIAN_POINT ( 'NONE',  ( 7.084665262690076126, 54.10535201082151247, 10.88017736071109987 ) ) ;
#90637 = CARTESIAN_POINT ( 'NONE',  ( 17.08211943468705130, 63.47041550158063927, 12.26659068614894998 ) ) ;
#90638 = CARTESIAN_POINT ( 'NONE',  ( 14.92337183194729988, 64.34226448433412315, -8.527530157486177487 ) ) ;
#90639 = CARTESIAN_POINT ( 'NONE',  ( 1.472469842513823179, 51.42559781766745886, 4.923371831947296329 ) ) ;
#90640 = CARTESIAN_POINT ( 'NONE',  ( -8.468251459920482560, -9.345277391848098247, 3.750000000000000000 ) ) ;
#90642 = CARTESIAN_POINT ( 'NONE',  ( -2.816281873526473856, 24.33196800326375353, 3.434112377981055619 ) ) ;
#90641 = CARTESIAN_POINT ( 'NONE',  ( 19.42250999205614193, 50.14701867748817676, 5.440088680355555262 ) ) ;
#90643 = CARTESIAN_POINT ( 'NONE',  ( 13.79529636645030344, 13.26208216824729824, 14.16423886937410614 ) ) ;
#90644 = CARTESIAN_POINT ( 'NONE',  ( 17.96484262340118221, 16.18868534415483396, -7.964842623401177768 ) ) ;
#90645 = CARTESIAN_POINT ( 'NONE',  ( 17.96484262340118221, 19.93868534415484106, 7.964842623401181321 ) ) ;
#90646 = B_SPLINE_CURVE_WITH_KNOTS ( 'NONE', 3,
 ( #92723, #76736, #47716, #24248, #2246, #69254, #54715, #23269, #92238, #1266 ),
 .UNSPECIFIED., .F., .F.,
 ( 4, 3, 3, 4 ),
 ( 7.757919228897728493E-18, 0.0006253016069560782611, 0.001250604074564933433, 0.002501455912506544803 ),
 .UNSPECIFIED. ) ;
#90647 = CARTESIAN_POINT ( 'NONE',  ( 20.88017736071110875, 60.77201867748817676, -2.915334737309920765 ) ) ;
#90648 = CARTESIAN_POINT ( 'NONE',  ( 22.81628187352647785, 46.41530133659708213, 3.434112377981063169 ) ) ;
#90649 = CARTESIAN_POINT ( 'NONE',  ( -7.208316651077756099, -23.36606884899921255, 7.208316651077766757 ) ) ;
#90650 = ORIENTED_EDGE ( 'NONE', *, *, #84161, .T. ) ;
#90651 = LINE ( 'NONE', #21687, #49132 ) ;
#90652 = ORIENTED_EDGE ( 'NONE', *, *, #27106, .T. ) ;
#90653 = DIRECTION ( 'NONE',  ( -5.818595309480553908E-17, -1.000000000000000000, -0.000000000000000000 ) ) ;
#90654 = DIRECTION ( 'NONE',  ( 1.000000000000000000, 0.000000000000000000, 0.000000000000000000 ) ) ;
#90655 = ORIENTED_EDGE ( 'NONE', *, *, #64354, .F. ) ;
#90656 = CARTESIAN_POINT ( 'NONE',  ( 0.000000000000000000, 14.49999999999999822, 0.000000000000000000 ) ) ;
#90658 = CARTESIAN_POINT ( 'NONE',  ( 10.00000000000000178, 4.313685344154837509, 10.88017736071110342 ) ) ;
#90657 = CARTESIAN_POINT ( 'NONE',  ( -4.164238869374099039, 41.80374883491397497, 8.674139862899312516E-16 ) ) ;
#90660 = CARTESIAN_POINT ( 'NONE',  ( 2.791683348922240793, 41.63393115100078745, 7.208316651077764092 ) ) ;
#90659 = CARTESIAN_POINT ( 'NONE',  ( 19.84674366389459621, 23.50893115100078390, 7.409399052514197653E-17 ) ) ;
#90661 = CARTESIAN_POINT ( 'NONE',  ( 12.91533473730993009, 66.60535201082150536, -10.88017736071109987 ) ) ;
#90662 = CIRCLE ( 'NONE', #69908, 14.49999999999999822 ) ;
#90663 = CARTESIAN_POINT ( 'NONE',  ( 5.076628168052704559, 0.1755978176674514724, -8.527530157486179263 ) ) ;
#90664 = EDGE_CURVE ( 'NONE', #64876, #50256, #47727, .T. ) ;
#90665 = B_SPLINE_CURVE_WITH_KNOTS ( 'NONE', 3,
 ( #9948, #78926, #69958, #40451, #39947, #16960 ),
 .UNSPECIFIED., .F., .F.,
 ( 4, 2, 4 ),
 ( 0.0002800591277523107204, 0.0006862649357714370240, 0.001092470743790563328 ),
 .UNSPECIFIED. ) ;
#90666 = CARTESIAN_POINT ( 'NONE',  ( -3.434112377981067610, 23.08196800326375708, -12.81628187352647252 ) ) ;
#90667 = ORIENTED_EDGE ( 'NONE', *, *, #28910, .T. ) ;
#90668 = CARTESIAN_POINT ( 'NONE',  ( 24.16423886937410614, 39.30374883491396787, 8.672049930838204340E-16 ) ) ;
#90669 = ADVANCED_FACE ( 'NONE', ( #33208 ), #53415, .F. ) ;
#90670 = CARTESIAN_POINT ( 'NONE',  ( 19.38216949554541202, 20.99863466993042138, 9.382169495545424454 ) ) ;
#90671 = ORIENTED_EDGE ( 'NONE', *, *, #21031, .T. ) ;
#90672 = CARTESIAN_POINT ( 'NONE',  ( 0.6178305044545838731, 54.74863466993042493, 9.382169495545420901 ) ) ;
#90673 = AXIS2_PLACEMENT_3D ( 'NONE', #29647, #28676, #83161 ) ;
#90674 = CARTESIAN_POINT ( 'NONE',  ( -0.8801773607111008646, 23.27201867748817676, 2.915334737309923430 ) ) ;
#90675 = CARTESIAN_POINT ( 'NONE',  ( 1.472469842513823179, 30.59226448433411960, -4.923371831947296329 ) ) ;
#90676 = CARTESIAN_POINT ( 'NONE',  ( 0.5774900079438590739, 22.64701867748817321, -5.440088680355550821 ) ) ;
#90677 = DIRECTION ( 'NONE',  ( 1.049065152435176504E-16, -1.000000000000000000, 0.000000000000000000 ) ) ;
#90678 = DIRECTION ( 'NONE',  ( 0.6626200482157357241, 0.000000000000000000, 0.7489557207890036317 ) ) ;
#90679 = CARTESIAN_POINT ( 'NONE',  ( 1.472469842513823179, 56.42559781766745886, 4.923371831947296329 ) ) ;
#90680 = CARTESIAN_POINT ( 'NONE',  ( 0.1532563361054082862, 46.21726448433411605, 2.638427012816831674 ) ) ;
#90681 = VECTOR ( 'NONE', #17330, 1000.000000000000000 ) ;
#90682 = AXIS2_PLACEMENT_3D ( 'NONE', #7165, #29156, #90152 ) ;
#90684 = EDGE_LOOP ( 'NONE', ( #19210, #51799, #29044, #26026 ) ) ;
#90683 = CARTESIAN_POINT ( 'NONE',  ( 7.313705784284598721, 0.3640475087720987935, -13.09617149020744087 ) ) ;
#90685 = CARTESIAN_POINT ( 'NONE',  ( -9.876730923139378504, 15.00000000000000000, 11.28938378619056415 ) ) ;
#90686 = DIRECTION ( 'NONE',  ( 1.000000000000000000, 0.000000000000000000, 0.000000000000000000 ) ) ;
#90687 = DIRECTION ( 'NONE',  ( -0.3665012267242880872, 0.000000000000000000, -0.9304175679820281264 ) ) ;
#90688 = CARTESIAN_POINT ( 'NONE',  ( 10.00000000000000178, 37.25893115100078745, 9.846743663894594434 ) ) ;
#90689 = DIRECTION ( 'NONE',  ( -0.3173046564050965856, 0.000000000000000000, 0.9483236552061978797 ) ) ;
#90690 = CARTESIAN_POINT ( 'NONE',  ( 19.38216949554541202, 35.99863466993041072, 9.382169495545424454 ) ) ;
#90691 = DIRECTION ( 'NONE',  ( 0.000000000000000000, 1.000000000000000000, 0.000000000000000000 ) ) ;
#90692 = VERTEX_POINT ( 'NONE', #10234 ) ;
#90693 = CARTESIAN_POINT ( 'NONE',  ( 5.076628168052703671, 61.84226448433412315, 8.527530157486179263 ) ) ;
#90694 = CARTESIAN_POINT ( 'NONE',  ( 0.000000000000000000, 0.5000000000000004441, 0.000000000000000000 ) ) ;
#90695 = CARTESIAN_POINT ( 'NONE',  ( 19.84674366389459266, 38.71726448433412315, -2.638427012816827677 ) ) ;
#90696 = CARTESIAN_POINT ( 'NONE',  ( 20.36894250292379738, 34.92874883491396076, -10.36894250292379027 ) ) ;
#90697 = CARTESIAN_POINT ( 'NONE',  ( 10.00000000000000000, 39.75893115100078745, -9.846743663894594434 ) ) ;
#90698 = CARTESIAN_POINT ( 'NONE',  ( 22.81628187352647785, 51.62363466993042493, 6.195893100308588602E-16 ) ) ;
#90700 =( LENGTH_UNIT ( ) NAMED_UNIT ( * ) SI_UNIT ( .MILLI., .METRE. ) );
#90699 = FACE_OUTER_BOUND ( 'NONE', #32611, .T. ) ;
#90701 = CARTESIAN_POINT ( 'NONE',  ( 19.84674366389459266, 3.300597817667451750, 2.638427012816836559 ) ) ;
#90702 = CARTESIAN_POINT ( 'NONE',  ( -2.266590686148945544, 1.387082168247301128, -7.082119434687050408 ) ) ;
#90703 = CARTESIAN_POINT ( 'NONE',  ( 17.20831665107776587, 44.13393115100078745, -7.208316651077762316 ) ) ;
#90705 = ADVANCED_FACE ( 'NONE', ( #87196 ), #18719, .F. ) ;
#90704 = CARTESIAN_POINT ( 'NONE',  ( 19.42250999205614193, 40.14701867748817676, 5.440088680355555262 ) ) ;
#90706 = CARTESIAN_POINT ( 'NONE',  ( 17.20831665107776587, 42.88393115100077324, 7.208316651077764980 ) ) ;
#90707 = DIRECTION ( 'NONE',  ( -0.000000000000000000, -0.000000000000000000, -1.000000000000000000 ) ) ;
#90708 = ORIENTED_EDGE ( 'NONE', *, *, #44600, .T. ) ;
#90709 = CARTESIAN_POINT ( 'NONE',  ( 0.5774900079438590739, 52.64701867748817676, -5.440088680355550821 ) ) ;
#90710 = ORIENTED_EDGE ( 'NONE', *, *, #56567, .F. ) ;
#90711 = DIRECTION ( 'NONE',  ( -0.000000000000000000, 1.000000000000000000, 0.000000000000000000 ) ) ;
#90712 = CARTESIAN_POINT ( 'NONE',  ( -0.8801773607111008646, 18.27201867748817321, 2.915334737309923430 ) ) ;
#90714 = CARTESIAN_POINT ( 'NONE',  ( -0.8801773607111008646, 48.27201867748816966, 2.915334737309923430 ) ) ;
#90713 = CARTESIAN_POINT ( 'NONE',  ( 22.81628187352647785, 1.623634669930420271, 6.195893100308588602E-16 ) ) ;
#90715 = CARTESIAN_POINT ( 'NONE',  ( -1.926860441876562247, 47.45379003517447813, -3.195792623639530650 ) ) ;
#90716 = CARTESIAN_POINT ( 'NONE',  ( 0.000000000000000000, 15.00000000000000000, 0.000000000000000000 ) ) ;
#90717 = CARTESIAN_POINT ( 'NONE',  ( 27.50000000000000355, 35.99999999999997158, -10.00000000000000000 ) ) ;
#90719 = CARTESIAN_POINT ( 'NONE',  ( 5.419894505350628222, 14.49999999999999112, -13.98659156302463735 ) ) ;
#90718 = CARTESIAN_POINT ( 'NONE',  ( -0.8801773607110991993, 42.85535201082150536, -2.915334737309923874 ) ) ;
#90720 = CARTESIAN_POINT ( 'NONE',  ( 0.1532563361054083140, 16.00893115100078390, 1.131784320476157264E-15 ) ) ;
#90721 = CARTESIAN_POINT ( 'NONE',  ( 19.84674366389459266, 23.71726448433412315, -2.638427012816827677 ) ) ;
#90722 =( BOUNDED_CURVE ( )  B_SPLINE_CURVE ( 2, ( #79003, #94494, #62026, #85039, #16552, #58961, #57480, #4500, #11004, #3513, #50469, #65962, #20477 ),
 .UNSPECIFIED., .F., .T. ) 
 B_SPLINE_CURVE_WITH_KNOTS ( ( 3, 2, 2, 2, 2, 2, 3 ),
 ( 0.6333333333333334147, 0.6388888888888889506, 0.6444444444444445974, 0.6500000000000001332, 0.6555555555555556690, 0.6611111111111112049, 0.6666666666666667407 ),
 .UNSPECIFIED. ) 
 CURVE ( )  GEOMETRIC_REPRESENTATION_ITEM ( )  RATIONAL_B_SPLINE_CURVE ( ( 0.9999999999999993339, 0.9659258262890689783, 1.000000000000000000, 0.9659258262890683122, 1.000000000000000000, 0.9659258262890683122, 1.000000000000000000, 0.9659258262890683122, 1.000000000000000000, 0.9659258262890683122, 1.000000000000000000, 0.9659258262890676461, 1.000000000000000666 ) ) 
 REPRESENTATION_ITEM ( '' )  );
#90723 = CARTESIAN_POINT ( 'NONE',  ( -12.26659068614895354, 21.38708216824730712, -7.082119434687038861 ) ) ;
#90724 = CARTESIAN_POINT ( 'NONE',  ( 10.00000000000000178, 62.25893115100078745, 9.846743663894594434 ) ) ;
#90726 = CARTESIAN_POINT ( 'NONE',  ( 0.1922240491738544388, 18.18878173731740944, 6.500000000000007105 ) ) ;
#90725 = CARTESIAN_POINT ( 'NONE',  ( 7.084665262690076126, 2.022018677488171434, -10.88017736071110164 ) ) ;
#90727 = DIRECTION ( 'NONE',  ( -1.000000000000000000, 0.000000000000000000, 0.000000000000000000 ) ) ;
#90728 = CARTESIAN_POINT ( 'NONE',  ( -4.164238869374099927, 17.01208216824730357, 3.795296366450308767 ) ) ;
#90729 = CARTESIAN_POINT ( 'NONE',  ( 2.917880565312950480, 45.97041550158063927, -12.26659068614894821 ) ) ;
#90730 = CIRCLE ( 'NONE', #52410, 2.999999999999999112 ) ;
#90731 = CARTESIAN_POINT ( 'NONE',  ( 7.084665262690076126, 4.105352010821503583, 10.88017736071109987 ) ) ;
#90732 = ORIENTED_EDGE ( 'NONE', *, *, #46756, .T. ) ;
#90733 = CARTESIAN_POINT ( 'NONE',  ( 17.20831665107776587, 24.13393115100078035, -7.208316651077762316 ) ) ;
#90734 = CARTESIAN_POINT ( 'NONE',  ( -0.8801773607111008646, 23.27201867748817676, 2.915334737309923430 ) ) ;
#90735 = CARTESIAN_POINT ( 'NONE',  ( 2.791683348922237240, 55.38393115100078745, -7.208316651077763204 ) ) ;
#90736 = CARTESIAN_POINT ( 'NONE',  ( 22.26659068614894466, 8.887082168247300018, 7.082119434687054849 ) ) ;
#90737 = CARTESIAN_POINT ( 'NONE',  ( -10.58981376305275468, 15.00000000000000000, -9.535111140613857117 ) ) ;
#90738 = FACE_OUTER_BOUND ( 'NONE', #82957, .T. ) ;
#90739 = CARTESIAN_POINT ( 'NONE',  ( 21.09922568453595559, 37.04030133659708923, -6.408140936763230044 ) ) ;
#90740 = CARTESIAN_POINT ( 'NONE',  ( 2.791683348922237240, 40.38393115100078035, -7.208316651077763204 ) ) ;
#90741 = ORIENTED_EDGE ( 'NONE', *, *, #10215, .F. ) ;
#90742 = CARTESIAN_POINT ( 'NONE',  ( 2.791683348922237240, 5.383931151000785675, -7.208316651077763204 ) ) ;
#90743 = CARTESIAN_POINT ( 'NONE',  ( 8.959589291399149502, -9.312544548374205533, -4.000000000000000000 ) ) ;
#90744 = CARTESIAN_POINT ( 'NONE',  ( -12.11331110855129367, 0.04922511925147014800, -8.421032842869621504 ) ) ;
#90745 = CARTESIAN_POINT ( 'NONE',  ( 12.91533473730992121, 14.52201867748817143, 10.88017736071110164 ) ) ;
#90746 = CARTESIAN_POINT ( 'NONE',  ( 24.16423886937409904, 49.09541550158063217, 3.795296366450317205 ) ) ;
#90747 = AXIS2_PLACEMENT_3D ( 'NONE', #84411, #90403, #98449 ) ;
#90748 = DIRECTION ( 'NONE',  ( 0.000000000000000000, 0.000000000000000000, -1.000000000000000000 ) ) ;
#90749 = CARTESIAN_POINT ( 'NONE',  ( -11.96291822454887033, 4.341775326899288507E-16, 8.193813980848993594 ) ) ;
#90750 = CARTESIAN_POINT ( 'NONE',  ( 17.20831665107776587, 27.88393115100078390, 7.208316651077764980 ) ) ;
#90751 = CARTESIAN_POINT ( 'NONE',  ( -0.8801773607110991993, 12.85535201082150358, -2.915334737309923874 ) ) ;
#90752 = CARTESIAN_POINT ( 'NONE',  ( 5.076628168052703671, 41.84226448433411605, 8.527530157486179263 ) ) ;
#90753 = CARTESIAN_POINT ( 'NONE',  ( 4.838527690343616960, 0.3639308167276188999, -14.19819177887730710 ) ) ;
#90754 = CARTESIAN_POINT ( 'NONE',  ( 1.472469842513823179, 51.42559781766745886, 4.923371831947296329 ) ) ;
#90755 = B_SPLINE_CURVE_WITH_KNOTS ( 'NONE', 3,
 ( #45701, #98741, #30191, #38699, #38217, #60692 ),
 .UNSPECIFIED., .F., .F.,
 ( 4, 2, 4 ),
 ( 3.409110551494646689E-05, 0.0004400426677367933479, 0.0008459942299586402153 ),
 .UNSPECIFIED. ) ;
#90756 = CARTESIAN_POINT ( 'NONE',  ( 19.42250999205614548, 40.98035201082150536, -5.440088680355545492 ) ) ;
#90757 = AXIS2_PLACEMENT_3D ( 'NONE', #79811, #72787, #4324 ) ;
#90758 = EDGE_CURVE ( 'NONE', #24281, #84653, #6138, .T. ) ;
#90759 = CIRCLE ( 'NONE', #14115, 0.1000000000000001166 ) ;
#90760 = B_SPLINE_CURVE_WITH_KNOTS ( 'NONE', 3,
 ( #28940, #49979, #13460, #80486, #45428, #38438 ),
 .UNSPECIFIED., .F., .F.,
 ( 4, 2, 4 ),
 ( 3.409110551496121881E-05, 0.0004400426677367874390, 0.0008459942299586136524 ),
 .UNSPECIFIED. ) ;
#90761 = EDGE_LOOP ( 'NONE', ( #66615, #81722, #27059, #11860 ) ) ;
#90762 = CARTESIAN_POINT ( 'NONE',  ( -2.816281873526473856, 64.12363466993042493, 9.499525473075851096E-16 ) ) ;
#90763 = FACE_OUTER_BOUND ( 'NONE', #73051, .T. ) ;
#90764 = CARTESIAN_POINT ( 'NONE',  ( 10.00000000000000000, 4.758931151000784787, -9.846743663894594434 ) ) ;
#90765 = CARTESIAN_POINT ( 'NONE',  ( 22.81628187352647785, 61.41530133659709634, 3.434112377981063169 ) ) ;
#90767 = CARTESIAN_POINT ( 'NONE',  ( 1.472469842513823179, 31.42559781766745530, 4.923371831947296329 ) ) ;
#90766 = CARTESIAN_POINT ( 'NONE',  ( 17.96484262340118221, 4.938685344154837509, 7.964842623401181321 ) ) ;
#90768 = CARTESIAN_POINT ( 'NONE',  ( -12.69000000000001371, 93.50000000000000000, -9.500000000000000000 ) ) ;
#90769 = EDGE_CURVE ( 'NONE', #85778, #85655, #52162, .T. ) ;
#90770 = DIRECTION ( 'NONE',  ( 0.000000000000000000, 0.000000000000000000, 1.000000000000000000 ) ) ;
#90771 = CARTESIAN_POINT ( 'NONE',  ( 2.917880565312950480, 50.97041550158064638, -12.26659068614894821 ) ) ;
#90772 = CARTESIAN_POINT ( 'NONE',  ( 0.1532563361054100626, 50.80059781766745175, -2.638427012816831230 ) ) ;
#90773 = CARTESIAN_POINT ( 'NONE',  ( 17.85999999999999588, 33.98752635800203592, 10.00000000000000000 ) ) ;
#90774 = CARTESIAN_POINT ( 'NONE',  ( 15.44008868035555260, 34.73035201082151247, 9.422509992056143702 ) ) ;
#90775 = CARTESIAN_POINT ( 'NONE',  ( 5.076628168052704559, 5.175597817667451750, -8.527530157486179263 ) ) ;
#90776 = ORIENTED_EDGE ( 'NONE', *, *, #16528, .T. ) ;
#90777 = CARTESIAN_POINT ( 'NONE',  ( 0.6178305044545838731, 59.74863466993041783, 9.382169495545420901 ) ) ;
#90778 = VERTEX_POINT ( 'NONE', #34680 ) ;
#90779 = EDGE_CURVE ( 'NONE', #93614, #95526, #86562, .T. ) ;
#90780 = CARTESIAN_POINT ( 'NONE',  ( 7.361572987183170547, 2.050597817667451750, 9.846743663894590881 ) ) ;
#90781 = ORIENTED_EDGE ( 'NONE', *, *, #82204, .F. ) ;
#90782 = CARTESIAN_POINT ( 'NONE',  ( 2.917880565312950480, 0.9704155015806342766, -12.26659068614894821 ) ) ;
#90783 = CARTESIAN_POINT ( 'NONE',  ( 0.1532563361054100626, 5.800597817667452638, -2.638427012816831230 ) ) ;
#90784 = CARTESIAN_POINT ( 'NONE',  ( 0.5774900079438590739, 32.64701867748816966, -5.440088680355550821 ) ) ;
#90785 = CARTESIAN_POINT ( 'NONE',  ( 7.264509831664601514, 0.2301509507469222116, 13.05561747642794934 ) ) ;
#90786 = ORIENTED_EDGE ( 'NONE', *, *, #92560, .T. ) ;
#90787 = CARTESIAN_POINT ( 'NONE',  ( -0.8801773607111009756, 28.06368534415484106, 1.068504757029289695E-15 ) ) ;
#90788 = ORIENTED_EDGE ( 'NONE', *, *, #52270, .T. ) ;
#90789 = CARTESIAN_POINT ( 'NONE',  ( 10.00000000000000000, 31.81368534415483751, -10.88017736071110342 ) ) ;
#90790 = CYLINDRICAL_SURFACE ( 'NONE', #13735, 8.000000000000000000 ) ;
#90791 = ORIENTED_EDGE ( 'NONE', *, *, #93727, .F. ) ;
#90792 = EDGE_CURVE ( 'NONE', #37315, #35951, #53066, .T. ) ;
#90793 = VERTEX_POINT ( 'NONE', #59655 ) ;
#90794 = CARTESIAN_POINT ( 'NONE',  ( 3.591859063236763294, 13.29030133659708746, -11.09922568453595026 ) ) ;
#90795 = CARTESIAN_POINT ( 'NONE',  ( 10.00000000000000178, 2.258931151000784787, 9.846743663894594434 ) ) ;
#90796 = DIRECTION ( 'NONE',  ( 0.000000000000000000, 0.000000000000000000, 1.000000000000000000 ) ) ;
#90798 = CARTESIAN_POINT ( 'NONE',  ( 19.80448550324507551, 6.827036817733427299, 6.500000000002767564 ) ) ;
#90797 = CARTESIAN_POINT ( 'NONE',  ( 19.42250999205614193, 20.14701867748817321, 5.440088680355555262 ) ) ;
#90799 = CARTESIAN_POINT ( 'NONE',  ( -0.8801773607111008646, 68.27201867748817676, 2.915334737309923430 ) ) ;
#90800 = CARTESIAN_POINT ( 'NONE',  ( 15.44008868035555793, 31.39701867748817676, -9.422509992056140149 ) ) ;
#90801 = ORIENTED_EDGE ( 'NONE', *, *, #10850, .T. ) ;
#90802 = CARTESIAN_POINT ( 'NONE',  ( 13.43411237798105340, 50.58196800326375353, 12.81628187352647963 ) ) ;
#90803 = CARTESIAN_POINT ( 'NONE',  ( 2.035157376598824452, 48.68868534415483396, 7.964842623401179544 ) ) ;
#90804 = CARTESIAN_POINT ( 'NONE',  ( -1.099225684535947600, 49.54030133659708923, 6.408140936763237150 ) ) ;
#90805 = CARTESIAN_POINT ( 'NONE',  ( 19.42250999205614193, 45.14701867748817676, 5.440088680355555262 ) ) ;
#90806 = CARTESIAN_POINT ( 'NONE',  ( 22.81628187352648496, 1.831968003263753753, -3.434112377981050290 ) ) ;
#90807 = SURFACE_SIDE_STYLE ('',( #91300 ) ) ;
#90808 = CARTESIAN_POINT ( 'NONE',  ( 0.1532563361054100626, 15.80059781766745353, -2.638427012816831230 ) ) ;
#90809 = CARTESIAN_POINT ( 'NONE',  ( 3.591859063236761518, 59.95696800326375353, 11.09922568453594849 ) ) ;
#90810 = CARTESIAN_POINT ( 'NONE',  ( 4.471356726113142166, -3.620120708367990492, -3.750000000000000888 ) ) ;
#90811 = CARTESIAN_POINT ( 'NONE',  ( 7.361572987183170547, 12.05059781766744997, 9.846743663894590881 ) ) ;
#90812 = CARTESIAN_POINT ( 'NONE',  ( 21.09922568453594849, 1.206968003263753531, 6.408140936763242479 ) ) ;
#90813 = CARTESIAN_POINT ( 'NONE',  ( 14.92337183194729988, 64.34226448433412315, -8.527530157486177487 ) ) ;
#90814 = CARTESIAN_POINT ( 'NONE',  ( -0.8801773607111009756, 38.06368534415484106, 1.068504757029289695E-15 ) ) ;
#90815 = CARTESIAN_POINT ( 'NONE',  ( 0.1532563361054082862, 51.21726448433412315, 2.638427012816831674 ) ) ;
#90817 = CARTESIAN_POINT ( 'NONE',  ( 19.84674366389459266, 23.71726448433412315, -2.638427012816827677 ) ) ;
#90816 = PRESENTATION_LAYER_ASSIGNMENT (  '', '', ( #22188 ) ) ;
#90818 = CARTESIAN_POINT ( 'NONE',  ( 1.472469842513823179, 11.42559781766745175, 4.923371831947296329 ) ) ;
#90819 = EDGE_CURVE ( 'NONE', #72372, #57586, #90146, .T. ) ;
#90821 = ORIENTED_EDGE ( 'NONE', *, *, #23539, .F. ) ;
#90820 = CARTESIAN_POINT ( 'NONE',  ( 13.43411237798105340, 5.581968003263753531, 12.81628187352647963 ) ) ;
#90822 = COLOUR_RGB ( '', 0.08235294, 0.09019608, 0.10196078) ;
#90823 = CARTESIAN_POINT ( 'NONE',  ( 19.42250999205614548, 5.980352010821504471, -5.440088680355545492 ) ) ;
#90824 =( NAMED_UNIT ( * ) SI_UNIT ( $, .STERADIAN. ) SOLID_ANGLE_UNIT ( ) );
#90825 = CARTESIAN_POINT ( 'NONE',  ( 17.20831665107776587, 64.13393115100079456, -7.208316651077762316 ) ) ;
#90826 = CARTESIAN_POINT ( 'NONE',  ( 14.71525861348293596, 14.49999999999999112, 2.908807992686717192 ) ) ;
#90827 = CARTESIAN_POINT ( 'NONE',  ( 20.88017736071110164, 5.355352010821503583, 2.915334737309930979 ) ) ;
#90828 = CARTESIAN_POINT ( 'NONE',  ( 10.00000000000000178, 42.25893115100078745, 9.846743663894594434 ) ) ;
#90829 = ORIENTED_EDGE ( 'NONE', *, *, #70589, .F. ) ;
#90830 = DIRECTION ( 'NONE',  ( 0.000000000000000000, 0.000000000000000000, 1.000000000000000000 ) ) ;
#90831 = CARTESIAN_POINT ( 'NONE',  ( -2.266590686148945544, 66.38708216824730357, -7.082119434687050408 ) ) ;
#90832 = DIRECTION ( 'NONE',  ( 1.000000000000000000, 0.000000000000000000, -0.000000000000000000 ) ) ;
#90833 = CARTESIAN_POINT ( 'NONE',  ( 19.42250999205614548, 30.98035201082150536, -5.440088680355545492 ) ) ;
#90834 = CARTESIAN_POINT ( 'NONE',  ( 10.00000000000000000, 45.55374883491397497, -14.16423886937410082 ) ) ;
#90836 = DIRECTION ( 'NONE',  ( 0.4461978131097943945, 0.000000000000000000, 0.8949343616020322134 ) ) ;
#90835 = CARTESIAN_POINT ( 'NONE',  ( 0.5774900079438607392, 3.480352010821504916, 5.440088680355550821 ) ) ;
#90837 = CARTESIAN_POINT ( 'NONE',  ( 2.791683348922240793, 26.63393115100078745, 7.208316651077764092 ) ) ;
#90838 = CARTESIAN_POINT ( 'NONE',  ( 10.00000000000000178, 10.37363466993041961, 12.81628187352647608 ) ) ;
#90839 = ORIENTED_EDGE ( 'NONE', *, *, #59271, .F. ) ;
#90840 = TOROIDAL_SURFACE ( 'NONE', #19052, 0.5000000000000000000, 0.2500000000000000000 ) ;
#90841 = DIRECTION ( 'NONE',  ( 0.7253743710122775301, 0.000000000000000000, 0.6883545756937645699 ) ) ;
#90842 = CARTESIAN_POINT ( 'NONE',  ( -4.164238869374099039, 6.803748834913967869, 8.674139862899312516E-16 ) ) ;
#90843 = CARTESIAN_POINT ( 'NONE',  ( 0.1532563361054100626, 25.80059781766744820, -2.638427012816831230 ) ) ;
#90844 = B_SPLINE_CURVE_WITH_KNOTS ( 'NONE', 3,
 ( #26767, #21248, #82230, #64749, #95261, #57261, #87756, #19270, #49754, #6736, #15735, #83722, #22737, #30700 ),
 .UNSPECIFIED., .F., .F.,
 ( 4, 2, 2, 2, 2, 2, 4 ),
 ( 0.000000000000000000, 0.004797171936611957510, 0.007195757904917936265, 0.009594343873223915020, 0.01199292984152989378, 0.01439151580983587253, 0.01918868774644783004 ),
 .UNSPECIFIED. ) ;
#90845 = CARTESIAN_POINT ( 'NONE',  ( 1.377727649040772586E-15, 15.00000000000000000, 11.25000000000000178 ) ) ;
#90846 = CARTESIAN_POINT ( 'NONE',  ( 10.00000000000000000, 45.55374883491397497, -14.16423886937410082 ) ) ;
#90847 = CARTESIAN_POINT ( 'NONE',  ( 12.63842701281683922, 14.55059781766744997, -9.846743663894590881 ) ) ;
#90849 = FACE_OUTER_BOUND ( 'NONE', #44789, .T. ) ;
#90848 = DIRECTION ( 'NONE',  ( -1.000000000000000000, -0.000000000000000000, 0.000000000000000000 ) ) ;
#90850 = CARTESIAN_POINT ( 'NONE',  ( 10.00000000000000000, 26.81368534415484106, -10.88017736071110342 ) ) ;
#90851 = CARTESIAN_POINT ( 'NONE',  ( 21.09922568453595559, 57.04030133659708923, -6.408140936763230044 ) ) ;
#90852 = CARTESIAN_POINT ( 'NONE',  ( 15.44008868035555260, 4.730352010821504471, 9.422509992056143702 ) ) ;
#90853 = CARTESIAN_POINT ( 'NONE',  ( 16.40814093676323893, 40.79030133659708923, 11.09922568453595026 ) ) ;
#90854 = CARTESIAN_POINT ( 'NONE',  ( 14.92337183194729633, 7.675597817667451750, 8.527530157486181039 ) ) ;
#90855 = ORIENTED_EDGE ( 'NONE', *, *, #85476, .T. ) ;
#90856 = DIRECTION ( 'NONE',  ( 1.000000000000000000, 0.000000000000000000, 0.000000000000000000 ) ) ;
#90857 = CARTESIAN_POINT ( 'NONE',  ( 19.72487221294570148, 35.71833443783938833, -6.500000000000010658 ) ) ;
#90858 = CARTESIAN_POINT ( 'NONE',  ( 17.08211943468705840, 40.13708216824731068, -12.26659068614894466 ) ) ;
#90859 = CARTESIAN_POINT ( 'NONE',  ( 20.36894250292379382, 13.67874883491396965, 10.36894250292379205 ) ) ;
#90860 = CARTESIAN_POINT ( 'NONE',  ( 20.88017736071110164, 10.35535201082150714, 2.915334737309930979 ) ) ;
#90861 = CARTESIAN_POINT ( 'NONE',  ( 7.084665262690076126, 27.02201867748817676, -10.88017736071110164 ) ) ;
#90862 = CARTESIAN_POINT ( 'NONE',  ( -13.61464873478171533, 0.5000000000000004441, 6.296136897217742501 ) ) ;
#90863 = STYLED_ITEM ( 'NONE', ( #79070 ), #3977 ) ;
#90864 = DIRECTION ( 'NONE',  ( 0.000000000000000000, 0.000000000000000000, -1.000000000000000000 ) ) ;
#90865 = CARTESIAN_POINT ( 'NONE',  ( 4.559911319644449179, 52.23035201082151247, -9.422509992056141925 ) ) ;
#90866 = CARTESIAN_POINT ( 'NONE',  ( 17.96484262340118221, 61.18868534415482685, -7.964842623401177768 ) ) ;
#90867 = CARTESIAN_POINT ( 'NONE',  ( 10.00000000000000178, 20.37363466993042138, 12.81628187352647608 ) ) ;
#90868 = CARTESIAN_POINT ( 'NONE',  ( -5.806616290881503772, -3.110304982317789662E-15, 13.42355087257358548 ) ) ;
#90869 = CARTESIAN_POINT ( 'NONE',  ( 19.80448550324510038, 26.82703681773341131, 6.500000000002802203 ) ) ;
#90870 = CARTESIAN_POINT ( 'NONE',  ( 0.1532563361054082862, 41.21726448433411605, 2.638427012816831674 ) ) ;
#90871 = EDGE_CURVE ( 'NONE', #26502, #37917, #73872, .T. ) ;
#90872 = ADVANCED_FACE ( 'NONE', ( #20682 ), #94317, .T. ) ;
#90873 = CARTESIAN_POINT ( 'NONE',  ( 21.09922568453594849, 16.20696800326375353, 6.408140936763242479 ) ) ;
#90875 = ADVANCED_FACE ( 'NONE', ( #47107 ), #40614, .T. ) ;
#90874 = CARTESIAN_POINT ( 'NONE',  ( 7.084665262690076126, 4.105352010821503583, 10.88017736071109987 ) ) ;
#90876 = EDGE_CURVE ( 'NONE', #2021, #22085, #73763, .T. ) ;
#90877 = CARTESIAN_POINT ( 'NONE',  ( 14.92337183194729988, 39.34226448433412315, -8.527530157486177487 ) ) ;
#90878 = LINE ( 'NONE', #7410, #80210 ) ;
#90879 = CARTESIAN_POINT ( 'NONE',  ( 14.92337183194729988, 14.34226448433411782, -8.527530157486177487 ) ) ;
#90880 = CARTESIAN_POINT ( 'NONE',  ( 20.36894250292379382, 3.678748834913967869, 10.36894250292379205 ) ) ;
#90881 = CARTESIAN_POINT ( 'NONE',  ( 19.42250999205614193, 30.14701867748817321, 5.440088680355555262 ) ) ;
#90882 = CARTESIAN_POINT ( 'NONE',  ( 4.559911319644449179, 27.23035201082150536, -9.422509992056141925 ) ) ;
#90884 = CARTESIAN_POINT ( 'NONE',  ( 24.16423886937410614, 29.30374883491396787, 8.672049930838204340E-16 ) ) ;
#90883 = LINE ( 'NONE', #43899, #31280 ) ;
#90885 = CARTESIAN_POINT ( 'NONE',  ( 18.52753015748617571, 38.09226448433412315, 4.923371831947298993 ) ) ;
#90886 = CARTESIAN_POINT ( 'NONE',  ( 15.44008868035555793, 31.39701867748817676, -9.422509992056140149 ) ) ;
#90887 = CARTESIAN_POINT ( 'NONE',  ( 17.96484262340118221, 21.18868534415483396, -7.964842623401177768 ) ) ;
#90888 = ORIENTED_EDGE ( 'NONE', *, *, #93713, .F. ) ;
#90889 = CARTESIAN_POINT ( 'NONE',  ( 4.559911319644449179, 23.89701867748817321, 9.422509992056141925 ) ) ;
#90891 = CARTESIAN_POINT ( 'NONE',  ( -1.099225684535947600, 44.54030133659708923, 6.408140936763237150 ) ) ;
#90890 = AXIS2_PLACEMENT_3D ( 'NONE', #7569, #21070, #67563 ) ;
#90892 = CARTESIAN_POINT ( 'NONE',  ( 2.035157376598822676, 47.43868534415484817, -7.964842623401177768 ) ) ;
#90894 = CARTESIAN_POINT ( 'NONE',  ( 15.44008868035555793, 56.39701867748817676, -9.422509992056140149 ) ) ;
#90893 =( NAMED_UNIT ( * ) PLANE_ANGLE_UNIT ( ) SI_UNIT ( $, .RADIAN. ) );
#90895 = ORIENTED_EDGE ( 'NONE', *, *, #66820, .F. ) ;
#90896 = CARTESIAN_POINT ( 'NONE',  ( 14.92337183194729633, 57.67559781766745886, 8.527530157486181039 ) ) ;
#90897 = CARTESIAN_POINT ( 'NONE',  ( 15.44008868035555260, 39.73035201082150536, 9.422509992056143702 ) ) ;
#90898 = CARTESIAN_POINT ( 'NONE',  ( 6.934035614004487869, -73.16521313705239038, 3.750000000000000000 ) ) ;
#90899 = SURFACE_STYLE_USAGE ( .BOTH. , #60403 ) ;
#90900 = DIRECTION ( 'NONE',  ( 0.000000000000000000, -0.000000000000000000, -1.000000000000000000 ) ) ;
#90901 = CARTESIAN_POINT ( 'NONE',  ( -2.266590686148945544, 47.22041550158063927, 7.082119434687048631 ) ) ;
#90902 = CARTESIAN_POINT ( 'NONE',  ( 4.559911319644449179, 52.23035201082151247, -9.422509992056141925 ) ) ;
#90903 = B_SPLINE_CURVE_WITH_KNOTS ( 'NONE', 3,
 ( #38865, #76362, #84371, #53355, #15386, #60361 ),
 .UNSPECIFIED., .F., .F.,
 ( 4, 2, 4 ),
 ( 3.409110551494650755E-05, 0.0004400426677367948658, 0.0008459942299586432511 ),
 .UNSPECIFIED. ) ;
#90904 = SURFACE_SIDE_STYLE ('',( #60899 ) ) ;
#90905 = CARTESIAN_POINT ( 'NONE',  ( 7.361572987183169658, 59.96726448433410894, -9.846743663894592657 ) ) ;
#90906 = CARTESIAN_POINT ( 'NONE',  ( 18.52753015748617571, 28.09226448433411960, 4.923371831947298993 ) ) ;
#90907 = EDGE_LOOP ( 'NONE', ( #42706, #54372, #91654, #45135 ) ) ;
#90908 = EDGE_CURVE ( 'NONE', #45908, #3546, #78607, .T. ) ;
#90909 = CARTESIAN_POINT ( 'NONE',  ( 12.63842701281683034, 32.46726448433412315, 9.846743663894596210 ) ) ;
#90910 = CARTESIAN_POINT ( 'NONE',  ( -5.204170427930421283E-15, -17.12636533006957862, -12.81628187352647608 ) ) ;
#90911 = CARTESIAN_POINT ( 'NONE',  ( 2.035157376598824452, 23.68868534415484461, 7.964842623401179544 ) ) ;
#90912 = CARTESIAN_POINT ( 'NONE',  ( 2.791683348922240793, 41.63393115100078745, 7.208316651077764092 ) ) ;
#90913 = DIRECTION ( 'NONE',  ( -0.9588197348681908316, 0.000000000000000000, -0.2840153447039300283 ) ) ;
#90914 = CARTESIAN_POINT ( 'NONE',  ( 2.035157376598824452, 28.68868534415484106, 7.964842623401179544 ) ) ;
#90915 = CARTESIAN_POINT ( 'NONE',  ( 17.08211943468705130, 43.47041550158063927, 12.26659068614894998 ) ) ;
#90916 = PRESENTATION_LAYER_ASSIGNMENT (  '', '', ( #20701 ) ) ;
#90917 = CARTESIAN_POINT ( 'NONE',  ( 1.472469842513823179, 51.42559781766745886, 4.923371831947296329 ) ) ;
#90918 = VERTEX_POINT ( 'NONE', #2640 ) ;
#90919 = CARTESIAN_POINT ( 'NONE',  ( 0.6178305044545818747, 18.49863466993041428, -9.382169495545419124 ) ) ;
#90920 = CARTESIAN_POINT ( 'NONE',  ( -0.8801773607111009756, 13.06368534415483929, 1.068504757029289695E-15 ) ) ;
#90921 = CARTESIAN_POINT ( 'NONE',  ( 2.035157376598822676, 47.43868534415484817, -7.964842623401177768 ) ) ;
#90922 = DIRECTION ( 'NONE',  ( 0.000000000000000000, 0.000000000000000000, -1.000000000000000000 ) ) ;
#90923 = ORIENTED_EDGE ( 'NONE', *, *, #89075, .T. ) ;
#90924 = CIRCLE ( 'NONE', #17444, 14.49999999999999822 ) ;
#90925 = CARTESIAN_POINT ( 'NONE',  ( -0.8801773607111009756, 58.06368534415484106, 1.068504757029289695E-15 ) ) ;
#90926 = CARTESIAN_POINT ( 'NONE',  ( 0.1532563361054083140, 41.00893115100078745, 1.131784320476157264E-15 ) ) ;
#90927 = CARTESIAN_POINT ( 'NONE',  ( 0.1532563361054082862, 21.21726448433412315, 2.638427012816831674 ) ) ;
#90928 = CARTESIAN_POINT ( 'NONE',  ( 1.472469842513823179, 11.42559781766745175, 4.923371831947296329 ) ) ;
#90929 = CARTESIAN_POINT ( 'NONE',  ( 12.98685442714197791, 15.00000000000000000, -6.449155920600934344 ) ) ;
#90931 = CARTESIAN_POINT ( 'NONE',  ( 22.81628187352647785, 41.41530133659708923, 3.434112377981063169 ) ) ;
#90930 = CARTESIAN_POINT ( 'NONE',  ( -6.867320125584340573, -58.36821204062218982, 2.500000000000000000 ) ) ;
#90933 = CARTESIAN_POINT ( 'NONE',  ( 0.9413316022086128942, 33.45508385108959004, 6.499999999999978684 ) ) ;
#90932 = CARTESIAN_POINT ( 'NONE',  ( 10.00000000000000000, 19.75893115100078390, -9.846743663894594434 ) ) ;
#90934 = LINE ( 'NONE', #92418, #2660 ) ;
#90936 = EDGE_LOOP ( 'NONE', ( #97044, #28316, #40542, #78639 ) ) ;
#90935 = CARTESIAN_POINT ( 'NONE',  ( 0.1532563361054100626, 35.80059781766745175, -2.638427012816831230 ) ) ;
#90937 = CARTESIAN_POINT ( 'NONE',  ( 21.92686044187656691, 17.18830936912750929, 4.562052436263911564E-16 ) ) ;
#90938 = CARTESIAN_POINT ( 'NONE',  ( 21.09922568453595559, 12.04030133659708746, -6.408140936763230044 ) ) ;
#90939 = CARTESIAN_POINT ( 'NONE',  ( 17.96484262340118221, 49.93868534415484106, 7.964842623401181321 ) ) ;
#90940 = CARTESIAN_POINT ( 'NONE',  ( -0.3689425029237898834, 31.17874883491396787, -10.36894250292378850 ) ) ;
#90941 = DIRECTION ( 'NONE',  ( 0.7808688094430307203, -0.6246950475544238435, 0.000000000000000000 ) ) ;
#90942 = CARTESIAN_POINT ( 'NONE',  ( 6.204703633549690345, 32.84541550158063927, 14.16423886937410082 ) ) ;
#90943 = CARTESIAN_POINT ( 'NONE',  ( -4.164238869374099927, 52.01208216824729647, 3.795296366450308767 ) ) ;
#90944 = EDGE_CURVE ( 'NONE', #67494, #44503, #38669, .T. ) ;
#90945 = CARTESIAN_POINT ( 'NONE',  ( 17.08211943468705840, 5.137082168247300906, -12.26659068614894466 ) ) ;
#90947 = DIRECTION ( 'NONE',  ( 0.000000000000000000, 1.000000000000000000, 0.000000000000000000 ) ) ;
#90946 = CARTESIAN_POINT ( 'NONE',  ( 6.204703633549690345, 27.84541550158063217, 14.16423886937410082 ) ) ;
#90948 = CARTESIAN_POINT ( 'NONE',  ( 20.88017736071110164, 50.35535201082151247, 2.915334737309930979 ) ) ;
#90949 = CARTESIAN_POINT ( 'NONE',  ( -3.014428414850123250, 11.15970029564931565, 11.25000000000000178 ) ) ;
#90950 = CARTESIAN_POINT ( 'NONE',  ( 1.472469842513823179, 35.59226448433412315, -4.923371831947296329 ) ) ;
#90951 = CARTESIAN_POINT ( 'NONE',  ( 18.52753015748617571, 48.09226448433412315, 4.923371831947298993 ) ) ;
#90952 = CARTESIAN_POINT ( 'NONE',  ( -0.8801773607110991993, 22.85535201082150181, -2.915334737309923874 ) ) ;
#90953 = CARTESIAN_POINT ( 'NONE',  ( 22.81628187352647785, 61.41530133659709634, 3.434112377981063169 ) ) ;
#90954 = CYLINDRICAL_SURFACE ( 'NONE', #53796, 3.999999999999999112 ) ;
#90955 = EDGE_CURVE ( 'NONE', #53414, #88480, #28685, .T. ) ;
#90956 = CARTESIAN_POINT ( 'NONE',  ( 20.00000000000000711, 80.90097674908675174, -4.954892789988381452 ) ) ;
#90957 = CARTESIAN_POINT ( 'NONE',  ( 17.20831665107776587, 27.88393115100078390, 7.208316651077764980 ) ) ;
#90958 = CARTESIAN_POINT ( 'NONE',  ( 22.81628187352648496, 61.83196800326376774, -3.434112377981050290 ) ) ;
#90959 = CARTESIAN_POINT ( 'NONE',  ( 10.36894250292379027, -16.32125116508603213, 10.36894250292378672 ) ) ;
#90960 = CARTESIAN_POINT ( 'NONE',  ( -0.8801773607111009756, 43.06368534415484106, 1.068504757029289695E-15 ) ) ;
#90961 = CARTESIAN_POINT ( 'NONE',  ( 19.84674366389459266, 48.71726448433413026, -2.638427012816827677 ) ) ;
#90962 = CARTESIAN_POINT ( 'NONE',  ( 24.16423886937410614, 44.30374883491397497, 8.672049930838204340E-16 ) ) ;
#90963 = ORIENTED_EDGE ( 'NONE', *, *, #75189, .T. ) ;
#90964 = CARTESIAN_POINT ( 'NONE',  ( -4.164238869374099039, 1.803748834913967647, 8.674139862899312516E-16 ) ) ;
#90965 = CARTESIAN_POINT ( 'NONE',  ( 2.035157376598822676, 62.43868534415483396, -7.964842623401177768 ) ) ;
#90966 = CARTESIAN_POINT ( 'NONE',  ( 17.96484262340118221, 66.18868534415483396, -7.964842623401177768 ) ) ;
#90967 = CARTESIAN_POINT ( 'NONE',  ( 6.204703633549690345, 65.76208216824731778, -14.16423886937410259 ) ) ;
#90968 = CARTESIAN_POINT ( 'NONE',  ( 3.591859063236761518, 9.956968003263753531, 11.09922568453594849 ) ) ;
#90969 = CARTESIAN_POINT ( 'NONE',  ( 24.35999999999999233, 37.99999999999997868, 7.000000000000000000 ) ) ;
#90970 = CARTESIAN_POINT ( 'NONE',  ( -0.8801773607111008646, 53.27201867748816966, 2.915334737309923430 ) ) ;
#90971 = CARTESIAN_POINT ( 'NONE',  ( 0.1077916266722474120, 27.24062864464240619, -6.478736007405939468 ) ) ;
#90972 = VECTOR ( 'NONE', #14897, 1000.000000000000000 ) ;
#90973 = DIRECTION ( 'NONE',  ( 1.224646799147353207E-16, 1.000000000000000000, 0.000000000000000000 ) ) ;
#90974 = CARTESIAN_POINT ( 'NONE',  ( -2.266590686148945544, 51.38708216824730357, -7.082119434687050408 ) ) ;
#90975 = CARTESIAN_POINT ( 'NONE',  ( -2.915334737309934532, 22.02201867748818742, -10.88017736071109987 ) ) ;
#90976 = CARTESIAN_POINT ( 'NONE',  ( 20.88017736071110875, 10.77201867748817143, -2.915334737309920765 ) ) ;
#90977 = CARTESIAN_POINT ( 'NONE',  ( 20.88017736071110164, 20.35535201082150891, 2.915334737309930979 ) ) ;
#90978 = CARTESIAN_POINT ( 'NONE',  ( 17.20831665107776587, 57.88393115100078745, 7.208316651077764980 ) ) ;
#90979 = CARTESIAN_POINT ( 'NONE',  ( 0.6178305044545818747, 53.49863466993041072, -9.382169495545419124 ) ) ;
#90980 =( NAMED_UNIT ( * ) SI_UNIT ( $, .STERADIAN. ) SOLID_ANGLE_UNIT ( ) );
#90982 = ORIENTED_EDGE ( 'NONE', *, *, #55391, .T. ) ;
#90981 = TOROIDAL_SURFACE ( 'NONE', #47872, 10.65000000000000036, 0.2500000000000000000 ) ;
#90983 = VECTOR ( 'NONE', #26959, 1000.000000000000000 ) ;
#90984 = CARTESIAN_POINT ( 'NONE',  ( 10.00000000000000000, 11.81368534415483751, -10.88017736071110342 ) ) ;
#90985 = CARTESIAN_POINT ( 'NONE',  ( 3.591859063236761518, 24.95696800326375353, 11.09922568453594849 ) ) ;
#90986 = CARTESIAN_POINT ( 'NONE',  ( 19.72487221294571569, 39.78217586085237656, 6.499999999999986677 ) ) ;
#90987 = ADVANCED_FACE ( 'NONE', ( #63587 ), #77607, .F. ) ;
#90988 = CARTESIAN_POINT ( 'NONE',  ( 1.472469842513823179, 50.59226448433411605, -4.923371831947296329 ) ) ;
#90989 = CARTESIAN_POINT ( 'NONE',  ( 19.42250999205614548, 30.98035201082150536, -5.440088680355545492 ) ) ;
#90990 = EDGE_CURVE ( 'NONE', #51712, #31750, #9986, .T. ) ;
#90991 = CARTESIAN_POINT ( 'NONE',  ( 13.43411237798105340, 20.58196800326374643, 12.81628187352647963 ) ) ;
#90993 = DIRECTION ( 'NONE',  ( -0.000000000000000000, -0.000000000000000000, 1.000000000000000000 ) ) ;
#90992 = CARTESIAN_POINT ( 'NONE',  ( 12.91533473730993009, 46.60535201082150536, -10.88017736071109987 ) ) ;
#90994 = DIRECTION ( 'NONE',  ( 0.000000000000000000, 1.000000000000000000, 0.000000000000000000 ) ) ;
#90995 = CARTESIAN_POINT ( 'NONE',  ( 13.43411237798105340, 50.58196800326375353, 12.81628187352647963 ) ) ;
#90996 = ORIENTED_EDGE ( 'NONE', *, *, #38299, .T. ) ;
#90997 = CARTESIAN_POINT ( 'NONE',  ( 20.88017736071110875, 50.77201867748817676, -2.915334737309920765 ) ) ;
#90999 = CARTESIAN_POINT ( 'NONE',  ( -0.3689425029237898834, 1.178748834913967869, -10.36894250292378850 ) ) ;
#90998 = CARTESIAN_POINT ( 'NONE',  ( 16.40814093676324603, 32.45696800326375353, -11.09922568453594671 ) ) ;
#91000 = CARTESIAN_POINT ( 'NONE',  ( 17.20831665107776587, 4.133931151000785675, -7.208316651077762316 ) ) ;
#91001 = CARTESIAN_POINT ( 'NONE',  ( 0.5774900079438607392, 53.48035201082151247, 5.440088680355550821 ) ) ;
#91002 = DIRECTION ( 'NONE',  ( 0.000000000000000000, 0.000000000000000000, 1.000000000000000000 ) ) ;
#91003 = CARTESIAN_POINT ( 'NONE',  ( 5.076628168052703671, 61.84226448433412315, 8.527530157486179263 ) ) ;
#91004 = CARTESIAN_POINT ( 'NONE',  ( 7.361572987183169658, 14.96726448433411960, -9.846743663894592657 ) ) ;
#91005 = CARTESIAN_POINT ( 'NONE',  ( 12.63842701281683034, 2.467264484334118269, 9.846743663894596210 ) ) ;
#91006 = CARTESIAN_POINT ( 'NONE',  ( 4.873787042390699931, -0.03417435944610275333, 13.39061984619922718 ) ) ;
#91007 = CARTESIAN_POINT ( 'NONE',  ( 24.16423886937410614, 39.30374883491396787, 8.672049930838204340E-16 ) ) ;
#91008 = CARTESIAN_POINT ( 'NONE',  ( 6.382347221874473675, 14.49999999999999112, -13.57444820018232079 ) ) ;
#91009 = CARTESIAN_POINT ( 'NONE',  ( -0.8801773607110991993, 2.855352010821504471, -2.915334737309923874 ) ) ;
#91010 = CARTESIAN_POINT ( 'NONE',  ( -5.320324007939504440, -24.96642978971303961, -3.999999999999998224 ) ) ;
#91011 = ORIENTED_EDGE ( 'NONE', *, *, #59162, .F. ) ;
#91012 = CARTESIAN_POINT ( 'NONE',  ( 17.96484262340118221, 6.188685344154837509, -7.964842623401177768 ) ) ;
#91013 = CARTESIAN_POINT ( 'NONE',  ( 20.36894250292379738, 64.92874883491397497, -10.36894250292379027 ) ) ;
#91014 = CARTESIAN_POINT ( 'NONE',  ( 18.52753015748617571, 48.09226448433412315, 4.923371831947298993 ) ) ;
#91015 = CARTESIAN_POINT ( 'NONE',  ( 10.00000000000000178, 40.37363466993042493, 12.81628187352647608 ) ) ;
#91016 =( NAMED_UNIT ( * ) SI_UNIT ( $, .STERADIAN. ) SOLID_ANGLE_UNIT ( ) );
#91018 = CARTESIAN_POINT ( 'NONE',  ( -4.164238869374098151, 6.595415501580634832, -3.795296366450310543 ) ) ;
#91017 = CARTESIAN_POINT ( 'NONE',  ( -12.99123301834679900, 90.70871800849667466, -7.440805305833852579 ) ) ;
#91019 = CARTESIAN_POINT ( 'NONE',  ( 19.42250999205614193, 15.14701867748817143, 5.440088680355555262 ) ) ;
#91020 = ADVANCED_FACE ( 'NONE', ( #25617 ), #56110, .T. ) ;
#91021 = CARTESIAN_POINT ( 'NONE',  ( -0.3689425029237881626, 57.42874883491397497, 10.36894250292379027 ) ) ;
#91022 = EDGE_CURVE ( 'NONE', #39990, #92022, #26575, .T. ) ;
#91023 = CARTESIAN_POINT ( 'NONE',  ( 5.076628168052703671, 36.84226448433412315, 8.527530157486179263 ) ) ;
#91024 = CARTESIAN_POINT ( 'NONE',  ( -14.37564666802077262, -2.717705211265421849E-15, 2.692451322017578530 ) ) ;
#91026 = B_SPLINE_CURVE_WITH_KNOTS ( 'NONE', 3,
 ( #5236, #35713, #96735, #28209, #58708, #68686 ),
 .UNSPECIFIED., .F., .F.,
 ( 4, 2, 4 ),
 ( 0.000000000000000000, 0.0002605067024380912843, 0.0005210134048761825686 ),
 .UNSPECIFIED. ) ;
#91025 = CARTESIAN_POINT ( 'NONE',  ( 17.20831665107776587, 24.13393115100078035, -7.208316651077762316 ) ) ;
#91027 = EDGE_CURVE ( 'NONE', #39498, #58781, #6033, .T. ) ;
#91028 = SURFACE_STYLE_FILL_AREA ( #16531 ) ;
#91029 = CARTESIAN_POINT ( 'NONE',  ( -7.208316651077764980, 15.38393115100078390, -7.208316651077759651 ) ) ;
#91030 = VERTEX_POINT ( 'NONE', #64070 ) ;
#91031 = ORIENTED_EDGE ( 'NONE', *, *, #1822, .T. ) ;
#91032 = DIRECTION ( 'NONE',  ( 0.000000000000000000, 0.000000000000000000, 1.000000000000000000 ) ) ;
#91033 = ORIENTED_EDGE ( 'NONE', *, *, #10726, .T. ) ;
#91034 = CARTESIAN_POINT ( 'NONE',  ( 12.63842701281683034, 52.46726448433413026, 9.846743663894596210 ) ) ;
#91035 = CARTESIAN_POINT ( 'NONE',  ( 10.00000000000000000, 15.55374883491396787, -14.16423886937410082 ) ) ;
#91037 = CARTESIAN_POINT ( 'NONE',  ( 12.91533473730992121, 34.52201867748817676, 10.88017736071110164 ) ) ;
#91036 = CARTESIAN_POINT ( 'NONE',  ( 2.035157376598824452, 33.68868534415484106, 7.964842623401179544 ) ) ;
#91039 = CARTESIAN_POINT ( 'NONE',  ( 21.09922568453595559, 37.04030133659708923, -6.408140936763230044 ) ) ;
#91038 = CARTESIAN_POINT ( 'NONE',  ( 12.63842701281683922, 64.55059781766745175, -9.846743663894590881 ) ) ;
#91040 = CARTESIAN_POINT ( 'NONE',  ( 22.26659068614895176, 9.720415501580633943, -7.082119434687042414 ) ) ;
#91041 = CARTESIAN_POINT ( 'NONE',  ( 7.084665262690076126, 67.02201867748817676, -10.88017736071110164 ) ) ;
#91042 = CARTESIAN_POINT ( 'NONE',  ( 19.38216949554541557, 32.24863466993041783, -9.382169495545420901 ) ) ;
#91043 = VERTEX_POINT ( 'NONE', #94585 ) ;
#91044 = CARTESIAN_POINT ( 'NONE',  ( 10.00000000000000000, 39.75893115100078745, -9.846743663894594434 ) ) ;
#91045 = CARTESIAN_POINT ( 'NONE',  ( 7.084665262690076126, 2.022018677488171434, -10.88017736071110164 ) ) ;
#91046 = VERTEX_POINT ( 'NONE', #56596 ) ;
#91047 = CARTESIAN_POINT ( 'NONE',  ( 4.559911319644449179, 12.23035201082150714, -9.422509992056141925 ) ) ;
#91048 = ORIENTED_EDGE ( 'NONE', *, *, #49412, .F. ) ;
#91049 = CARTESIAN_POINT ( 'NONE',  ( 7.084665262690076126, 57.02201867748817676, -10.88017736071110164 ) ) ;
#91050 = AXIS2_PLACEMENT_3D ( 'NONE', #38617, #649, #31098 ) ;
#91051 = CARTESIAN_POINT ( 'NONE',  ( 12.91533473730993009, 56.60535201082151247, -10.88017736071109987 ) ) ;
#91052 = CARTESIAN_POINT ( 'NONE',  ( -0.8801773607111008646, 58.27201867748816966, 2.915334737309923430 ) ) ;
#91053 =( NAMED_UNIT ( * ) SI_UNIT ( $, .STERADIAN. ) SOLID_ANGLE_UNIT ( ) );
#91054 = CARTESIAN_POINT ( 'NONE',  ( -0.8801773607111009756, 48.06368534415484817, 1.068504757029289695E-15 ) ) ;
#91055 = VECTOR ( 'NONE', #44321, 1000.000000000000000 ) ;
#91056 = CARTESIAN_POINT ( 'NONE',  ( -46.94000000000001194, 100.4376529975699981, 9.000000000001183054 ) ) ;
#91057 = CARTESIAN_POINT ( 'NONE',  ( -46.50435961404672014, 102.7681846068616238, 6.785878169524574233 ) ) ;
#91059 = EDGE_LOOP ( 'NONE', ( #2275, #42359, #91774 ) ) ;
#91058 = CARTESIAN_POINT ( 'NONE',  ( 0.000000000000000000, -97.00000000000000000, 4.000000000000000000 ) ) ;
#91060 = CARTESIAN_POINT ( 'NONE',  ( 18.52753015748617571, 48.09226448433412315, 4.923371831947298993 ) ) ;
#91061 = ORIENTED_EDGE ( 'NONE', *, *, #67539, .T. ) ;
#91062 = CARTESIAN_POINT ( 'NONE',  ( -6.000000000000014211, 79.82179676972448590, 6.250000000000000000 ) ) ;
#91063 = SURFACE_STYLE_USAGE ( .BOTH. , #91571 ) ;
#91064 = CARTESIAN_POINT ( 'NONE',  ( 24.16423886937409904, 4.095415501580634832, 3.795296366450317205 ) ) ;
#91065 = DIRECTION ( 'NONE',  ( -0.000000000000000000, -1.000000000000000000, -0.000000000000000000 ) ) ;
#91067 = CARTESIAN_POINT ( 'NONE',  ( 20.88017736071110875, 60.77201867748817676, -2.915334737309920765 ) ) ;
#91066 =( LENGTH_UNIT ( ) NAMED_UNIT ( * ) SI_UNIT ( .MILLI., .METRE. ) );
#91068 = CARTESIAN_POINT ( 'NONE',  ( 12.91533473730992121, 4.522018677488170546, 10.88017736071110164 ) ) ;
#91069 = DIRECTION ( 'NONE',  ( 0.000000000000000000, 0.000000000000000000, -1.000000000000000000 ) ) ;
#91071 = ORIENTED_EDGE ( 'NONE', *, *, #84820, .T. ) ;
#91070 = CARTESIAN_POINT ( 'NONE',  ( -2.816281873526471635, 43.91530133659708923, -3.434112377981056508 ) ) ;
#91072 = CARTESIAN_POINT ( 'NONE',  ( 11.62719953690064933, 0.5000000000000004441, -9.476720473301794456 ) ) ;
#91073 = CARTESIAN_POINT ( 'NONE',  ( 7.361572987183170547, 47.05059781766745175, 9.846743663894590881 ) ) ;
#91074 = SURFACE_STYLE_USAGE ( .BOTH. , #92067 ) ;
#91075 = CARTESIAN_POINT ( 'NONE',  ( 3.591859063236763294, 23.29030133659708568, -11.09922568453595026 ) ) ;
#91076 = CARTESIAN_POINT ( 'NONE',  ( 7.361572987183170547, 22.05059781766745530, 9.846743663894590881 ) ) ;
#91077 = EDGE_CURVE ( 'NONE', #7091, #49656, #30652, .T. ) ;
#91078 = CARTESIAN_POINT ( 'NONE',  ( -13.80105244024794331, 90.89655890636515778, -7.750000000004162892 ) ) ;
#91079 = CARTESIAN_POINT ( 'NONE',  ( 18.52753015748618282, 18.92559781766745175, -4.923371831947291888 ) ) ;
#91080 = CARTESIAN_POINT ( 'NONE',  ( 2.791683348922237240, 65.38393115100078035, -7.208316651077763204 ) ) ;
#91081 = B_SPLINE_CURVE_WITH_KNOTS ( 'NONE', 3,
 ( #3405, #17432, #40427, #56407, #47900, #33867 ),
 .UNSPECIFIED., .F., .F.,
 ( 4, 2, 4 ),
 ( 0.0002800075630785971810, 0.0006862128664729002202, 0.001092418169867203151 ),
 .UNSPECIFIED. ) ;
#91082 = VECTOR ( 'NONE', #64610, 1000.000000000000000 ) ;
#91083 = ORIENTED_EDGE ( 'NONE', *, *, #45781, .T. ) ;
#91084 = VERTEX_POINT ( 'NONE', #95071 ) ;
#91085 = CARTESIAN_POINT ( 'NONE',  ( 19.42250999205614193, 20.14701867748817321, 5.440088680355555262 ) ) ;
#91086 = CARTESIAN_POINT ( 'NONE',  ( 10.00000000000000178, 23.05374883491397142, 14.16423886937410082 ) ) ;
#91087 = CARTESIAN_POINT ( 'NONE',  ( 5.076628168052703671, 26.84226448433411960, 8.527530157486179263 ) ) ;
#91088 = CARTESIAN_POINT ( 'NONE',  ( 10.00000000000000000, 4.758931151000784787, -9.846743663894594434 ) ) ;
#91090 = CARTESIAN_POINT ( 'NONE',  ( 6.879999999999995453, 43.00000000000000000, 6.250000000000000000 ) ) ;
#91089 = CARTESIAN_POINT ( 'NONE',  ( 13.43411237798105340, 40.58196800326375353, 12.81628187352647963 ) ) ;
#91091 = CARTESIAN_POINT ( 'NONE',  ( 2.035157376598822676, 17.43868534415483751, -7.964842623401177768 ) ) ;
#91092 = FACE_OUTER_BOUND ( 'NONE', #23684, .T. ) ;
#91093 = CARTESIAN_POINT ( 'NONE',  ( -2.816281873526473856, 9.123634669930421381, 9.499525473075851096E-16 ) ) ;
#91094 = CARTESIAN_POINT ( 'NONE',  ( 22.81628187352647785, 6.623634669930420493, 6.195893100308588602E-16 ) ) ;
#91095 = CARTESIAN_POINT ( 'NONE',  ( 14.92337183194729633, 32.67559781766745175, 8.527530157486181039 ) ) ;
#91096 = CARTESIAN_POINT ( 'NONE',  ( 5.440088680355549045, -13.60298132251182324, -9.422509992056141925 ) ) ;
#91097 = CARTESIAN_POINT ( 'NONE',  ( -1.099225684535947600, 39.54030133659708923, 6.408140936763237150 ) ) ;
#91098 = CARTESIAN_POINT ( 'NONE',  ( 13.78891971893211021, 0.3639314269420867998, -5.904717858191556701 ) ) ;
#91100 = CARTESIAN_POINT ( 'NONE',  ( 13.14228782657346528, 14.49999999999999112, -7.230509711182246058 ) ) ;
#91099 = CARTESIAN_POINT ( 'NONE',  ( 4.559911319644449179, 38.89701867748817676, 9.422509992056141925 ) ) ;
#91101 = CARTESIAN_POINT ( 'NONE',  ( 14.16722289976685012, 0.5000000000000004441, -4.928467845925517565 ) ) ;
#91102 = CARTESIAN_POINT ( 'NONE',  ( 20.15039907845753220, 20.60158574516643171, -6.262539305110077947 ) ) ;
#91103 = CARTESIAN_POINT ( 'NONE',  ( 12.91533473730992121, 39.52201867748817676, 10.88017736071110164 ) ) ;
#91104 = AXIS2_PLACEMENT_3D ( 'NONE', #67633, #31580, #83618 ) ;
#91105 = CARTESIAN_POINT ( 'NONE',  ( 20.88017736071110519, 40.56368534415484106, 2.639326808657452039E-16 ) ) ;
#91106 = CARTESIAN_POINT ( 'NONE',  ( 19.84674366389459266, 58.71726448433411605, -2.638427012816827677 ) ) ;
#91107 = ADVANCED_FACE ( 'NONE', ( #57078 ), #70124, .T. ) ;
#91108 = CARTESIAN_POINT ( 'NONE',  ( -0.8801773607111009756, 68.06368534415484817, 1.068504757029289695E-15 ) ) ;
#91109 = UNCERTAINTY_MEASURE_WITH_UNIT (LENGTH_MEASURE( 1.000000000000000082E-05 ), #88551, 'distance_accuracy_value', 'NONE');
#91110 = EDGE_CURVE ( 'NONE', #54251, #26502, #93102, .T. ) ;
#91111 = CARTESIAN_POINT ( 'NONE',  ( 7.361572987183170547, 57.05059781766744464, 9.846743663894590881 ) ) ;
#91113 = DIRECTION ( 'NONE',  ( -0.000000000000000000, -1.000000000000000000, -0.000000000000000000 ) ) ;
#91112 = CARTESIAN_POINT ( 'NONE',  ( 4.559911319644449179, 7.230352010821504471, -9.422509992056141925 ) ) ;
#91114 = AXIS2_PLACEMENT_3D ( 'NONE', #62442, #8962, #39959 ) ;
#91115 = CARTESIAN_POINT ( 'NONE',  ( 16.40814093676323893, 10.79030133659708923, 11.09922568453595026 ) ) ;
#91116 = VERTEX_POINT ( 'NONE', #78110 ) ;
#91117 = CARTESIAN_POINT ( 'NONE',  ( 0.5774900079438607392, 43.48035201082151247, 5.440088680355550821 ) ) ;
#91118 = CARTESIAN_POINT ( 'NONE',  ( 1.274849032794199255, 23.57228050351030646, 6.499999999999850786 ) ) ;
#91119 = CARTESIAN_POINT ( 'NONE',  ( 0.5774900079438607392, 3.480352010821504027, 5.440088680355550821 ) ) ;
#91120 = CIRCLE ( 'NONE', #12891, 3.000000000000000000 ) ;
#91121 = CARTESIAN_POINT ( 'NONE',  ( 0.5774900079438607392, 28.48035201082150891, 5.440088680355550821 ) ) ;
#91122 = CARTESIAN_POINT ( 'NONE',  ( 19.84674366389459621, 13.50893115100078568, 7.409399052514197653E-17 ) ) ;
#91123 = CARTESIAN_POINT ( 'NONE',  ( 20.36894250292379738, 34.92874883491396076, -10.36894250292379027 ) ) ;
#91124 = CARTESIAN_POINT ( 'NONE',  ( 0.1532563361054083140, 26.00893115100078745, 1.131784320476157264E-15 ) ) ;
#91125 = CARTESIAN_POINT ( 'NONE',  ( 19.42250999205614548, 50.98035201082151247, -5.440088680355545492 ) ) ;
#91126 = PLANE ( 'NONE',  #53797 ) ;
#91127 = CARTESIAN_POINT ( 'NONE',  ( 13.79529636645030344, 8.262082168247300018, 14.16423886937410614 ) ) ;
#91128 = CIRCLE ( 'NONE', #86358, 14.49999999999999822 ) ;
#91129 = FACE_OUTER_BOUND ( 'NONE', #82300, .T. ) ;
#91130 = CARTESIAN_POINT ( 'NONE',  ( 18.52753015748617571, 63.09226448433412315, 4.923371831947298993 ) ) ;
#91131 = ORIENTED_EDGE ( 'NONE', *, *, #96255, .T. ) ;
#91132 = VERTEX_POINT ( 'NONE', #9616 ) ;
#91133 = CARTESIAN_POINT ( 'NONE',  ( 24.16423886937410614, 24.51208216824730002, -3.795296366450302550 ) ) ;
#91134 = CARTESIAN_POINT ( 'NONE',  ( -4.164238869374099927, 27.01208216824730357, 3.795296366450308767 ) ) ;
#91135 = CARTESIAN_POINT ( 'NONE',  ( 20.88017736071110875, 55.77201867748816966, -2.915334737309920765 ) ) ;
#91136 = CARTESIAN_POINT ( 'NONE',  ( 2.035157376598822676, 2.438685344154838397, -7.964842623401177768 ) ) ;
#91137 = CARTESIAN_POINT ( 'NONE',  ( 0.1532563361054100626, 50.80059781766745175, -2.638427012816831230 ) ) ;
#91138 = CARTESIAN_POINT ( 'NONE',  ( -10.91022435251843348, -52.91485255063418691, 4.000000000000000000 ) ) ;
#91140 = CARTESIAN_POINT ( 'NONE',  ( 0.6178305044545838731, 14.74863466993041783, 9.382169495545420901 ) ) ;
#91139 = CARTESIAN_POINT ( 'NONE',  ( -0.8801773607110991993, 52.85535201082151247, -2.915334737309923874 ) ) ;
#91141 = CARTESIAN_POINT ( 'NONE',  ( 17.08211943468705840, 20.13708216824730357, -12.26659068614894466 ) ) ;
#91142 = CARTESIAN_POINT ( 'NONE',  ( 7.084665262690076126, 17.02201867748817676, -10.88017736071110164 ) ) ;
#91143 = CARTESIAN_POINT ( 'NONE',  ( 15.44008868035555793, 31.39701867748817676, -9.422509992056140149 ) ) ;
#91144 = CARTESIAN_POINT ( 'NONE',  ( 7.084665262690076126, 62.02201867748816966, -10.88017736071110164 ) ) ;
#91145 = CARTESIAN_POINT ( 'NONE',  ( 6.565887622018943937, 50.16530133659708213, 12.81628187352647430 ) ) ;
#91146 = CARTESIAN_POINT ( 'NONE',  ( 4.923371831947301658, -22.32440218233254470, 8.527530157486175710 ) ) ;
#91147 = VERTEX_POINT ( 'NONE', #55099 ) ;
#91148 = CARTESIAN_POINT ( 'NONE',  ( 19.89220837332776171, 34.74062864464240619, 6.478736007405959008 ) ) ;
#91149 = EDGE_LOOP ( 'NONE', ( #48989, #77616, #68935, #89876 ) ) ;
#91150 = DIRECTION ( 'NONE',  ( 0.000000000000000000, 0.000000000000000000, -1.000000000000000000 ) ) ;
#91151 = ORIENTED_EDGE ( 'NONE', *, *, #66949, .T. ) ;
#91152 = CIRCLE ( 'NONE', #71953, 0.5000000000000004441 ) ;
#91153 = DIRECTION ( 'NONE',  ( -0.000000000000000000, -1.000000000000000000, -0.000000000000000000 ) ) ;
#91155 = CARTESIAN_POINT ( 'NONE',  ( 24.16423886937409904, 64.09541550158064638, 3.795296366450317205 ) ) ;
#91154 = CARTESIAN_POINT ( 'NONE',  ( 10.00000000000000178, 53.05374883491396787, 14.16423886937410082 ) ) ;
#91157 = CARTESIAN_POINT ( 'NONE',  ( 2.791683348922237240, 65.38393115100078035, -7.208316651077763204 ) ) ;
#91156 = CARTESIAN_POINT ( 'NONE',  ( 0.1532563361054100626, 25.80059781766744820, -2.638427012816831230 ) ) ;
#91158 = CARTESIAN_POINT ( 'NONE',  ( 19.42250999205614193, 65.14701867748817676, 5.440088680355555262 ) ) ;
#91159 = EDGE_CURVE ( 'NONE', #64436, #19224, #32603, .T. ) ;
#91160 = LINE ( 'NONE', #688, #78353 ) ;
#91161 = CARTESIAN_POINT ( 'NONE',  ( -12.81628187352647963, 18.91530133659709634, -3.434112377981046293 ) ) ;
#91162 = ORIENTED_EDGE ( 'NONE', *, *, #77384, .T. ) ;
#91163 = CARTESIAN_POINT ( 'NONE',  ( 22.26659068614894466, 33.88708216824730357, 7.082119434687054849 ) ) ;
#91164 = CARTESIAN_POINT ( 'NONE',  ( -4.164238869374099927, 47.01208216824729647, 3.795296366450308767 ) ) ;
#91165 = EDGE_LOOP ( 'NONE', ( #5698, #94141, #57368, #8096 ) ) ;
#91166 = CARTESIAN_POINT ( 'NONE',  ( 16.40814093676324603, 62.45696800326376064, -11.09922568453594671 ) ) ;
#91167 = CARTESIAN_POINT ( 'NONE',  ( 0.1532563361054082862, 56.21726448433411605, 2.638427012816831674 ) ) ;
#91168 = CARTESIAN_POINT ( 'NONE',  ( 7.084665262690076126, 27.02201867748817676, -10.88017736071110164 ) ) ;
#91169 = CARTESIAN_POINT ( 'NONE',  ( 13.16740645155967115, 0.04922511925147067535, 6.653232860246649061 ) ) ;
#91170 = CARTESIAN_POINT ( 'NONE',  ( -0.1298530154764001854, 80.39370036920264795, -9.500000000000000000 ) ) ;
#91171 = CARTESIAN_POINT ( 'NONE',  ( 19.84674366389459266, 58.30059781766745886, 2.638427012816836559 ) ) ;
#91172 = CARTESIAN_POINT ( 'NONE',  ( 19.84674366389459266, 53.30059781766744464, 2.638427012816836559 ) ) ;
#91173 = TOROIDAL_SURFACE ( 'NONE', #48056, 0.5000000000000000000, 0.2500000000000000000 ) ;
#91176 = ORIENTED_EDGE ( 'NONE', *, *, #36022, .F. ) ;
#91175 =( GEOMETRIC_REPRESENTATION_CONTEXT ( 3 ) GLOBAL_UNCERTAINTY_ASSIGNED_CONTEXT ( ( #94195 ) ) GLOBAL_UNIT_ASSIGNED_CONTEXT ( ( #43632, #31089, #62073 ) ) REPRESENTATION_CONTEXT ( 'NONE', 'WORKASPACE' ) );
#91174 = CARTESIAN_POINT ( 'NONE',  ( 7.003840667633727257, 6.657678965418798693E-16, -12.84073839985654608 ) ) ;
#91177 = DIRECTION ( 'NONE',  ( 0.000000000000000000, 0.000000000000000000, -1.000000000000000000 ) ) ;
#91178 = CARTESIAN_POINT ( 'NONE',  ( 17.20831665107776587, 7.883931151000784787, 7.208316651077764980 ) ) ;
#91179 = SURFACE_STYLE_USAGE ( .BOTH. , #97734 ) ;
#91180 = VERTEX_POINT ( 'NONE', #66051 ) ;
#91181 =( LENGTH_UNIT ( ) NAMED_UNIT ( * ) SI_UNIT ( .MILLI., .METRE. ) );
#91182 = CARTESIAN_POINT ( 'NONE',  ( 18.52753015748618282, 28.92559781766745175, -4.923371831947291888 ) ) ;
#91183 = CARTESIAN_POINT ( 'NONE',  ( 1.915564264621432589, 3.914659629196372862E-16, -14.37291249357990530 ) ) ;
#91184 = CARTESIAN_POINT ( 'NONE',  ( 6.565887622018943937, 40.16530133659708923, 12.81628187352647430 ) ) ;
#91185 = CARTESIAN_POINT ( 'NONE',  ( -13.69000000000001194, 92.00000000000000000, -9.500000000000000000 ) ) ;
#91186 = FACE_OUTER_BOUND ( 'NONE', #25150, .T. ) ;
#91187 = CARTESIAN_POINT ( 'NONE',  ( 19.84674366389459266, 63.71726448433412315, -2.638427012816827677 ) ) ;
#91188 = DIRECTION ( 'NONE',  ( 1.000000000000000000, 0.000000000000000000, 0.000000000000000000 ) ) ;
#91189 = CARTESIAN_POINT ( 'NONE',  ( 14.92337183194729988, 34.34226448433411605, -8.527530157486177487 ) ) ;
#91190 = CARTESIAN_POINT ( 'NONE',  ( 6.204703633549690345, 30.76208216824730357, -14.16423886937410259 ) ) ;
#91191 = CARTESIAN_POINT ( 'NONE',  ( 2.791683348922237240, 40.38393115100078035, -7.208316651077763204 ) ) ;
#91192 = LINE ( 'NONE', #53201, #24084 ) ;
#91193 = CARTESIAN_POINT ( 'NONE',  ( 5.076628168052704559, 0.1755978176674514724, -8.527530157486179263 ) ) ;
#91194 = CARTESIAN_POINT ( 'NONE',  ( 19.84674366389459266, 43.71726448433410894, -2.638427012816827677 ) ) ;
#91195 = CARTESIAN_POINT ( 'NONE',  ( 19.42250999205614193, 55.14701867748817676, 5.440088680355555262 ) ) ;
#91196 = EDGE_CURVE ( 'NONE', #46169, #35060, #5073, .T. ) ;
#91197 = CARTESIAN_POINT ( 'NONE',  ( 7.361572987183169658, 39.96726448433411605, -9.846743663894592657 ) ) ;
#91198 = CARTESIAN_POINT ( 'NONE',  ( 11.61621867929611973, -0.03417435944610275333, -10.99731149103385874 ) ) ;
#91199 = CARTESIAN_POINT ( 'NONE',  ( 19.42250999205614548, 45.98035201082150536, -5.440088680355545492 ) ) ;
#91200 = ORIENTED_EDGE ( 'NONE', *, *, #10994, .F. ) ;
#91201 = CARTESIAN_POINT ( 'NONE',  ( 0.000000000000000000, 0.5000000000000004441, 0.000000000000000000 ) ) ;
#91202 = CARTESIAN_POINT ( 'NONE',  ( 19.42250999205614193, 25.14701867748817321, 5.440088680355555262 ) ) ;
#91204 = CARTESIAN_POINT ( 'NONE',  ( 7.084665262690076126, 39.10535201082150536, 10.88017736071109987 ) ) ;
#91203 = CARTESIAN_POINT ( 'NONE',  ( 3.591859063236763294, -1.709698663402913210, -11.09922568453595026 ) ) ;
#91205 = DIRECTION ( 'NONE',  ( -0.000000000000000000, -0.000000000000000000, -1.000000000000000000 ) ) ;
#91206 = DIRECTION ( 'NONE',  ( -0.000000000000000000, -1.000000000000000000, 0.000000000000000000 ) ) ;
#91207 =( LENGTH_UNIT ( ) NAMED_UNIT ( * ) SI_UNIT ( .MILLI., .METRE. ) );
#91209 = DIRECTION ( 'NONE',  ( -0.000000000000000000, -0.000000000000000000, -1.000000000000000000 ) ) ;
#91208 = CARTESIAN_POINT ( 'NONE',  ( -0.8801773607111009756, 38.06368534415484106, 1.068504757029289695E-15 ) ) ;
#91210 = CARTESIAN_POINT ( 'NONE',  ( 10.00000000000000178, 17.25893115100078745, 9.846743663894594434 ) ) ;
#91211 = CARTESIAN_POINT ( 'NONE',  ( 10.00000000000000000, 34.75893115100078745, -9.846743663894594434 ) ) ;
#91212 = CARTESIAN_POINT ( 'NONE',  ( 19.80427997160309417, 57.75733960839543357, -6.499999999999988454 ) ) ;
#91213 = CARTESIAN_POINT ( 'NONE',  ( 12.26659068614894466, 24.72041550158063217, -7.082119434687053960 ) ) ;
#91214 = CARTESIAN_POINT ( 'NONE',  ( 22.81628187352647785, 1.623634669930420271, 6.195893100308588602E-16 ) ) ;
#91215 = CARTESIAN_POINT ( 'NONE',  ( -2.266590686148945544, 61.38708216824730357, -7.082119434687050408 ) ) ;
#91217 = CIRCLE ( 'NONE', #260, 14.49999999999999822 ) ;
#91216 = CARTESIAN_POINT ( 'NONE',  ( 20.10239578412225470, 27.63377557478296254, -6.340343622311919169 ) ) ;
#91218 = CARTESIAN_POINT ( 'NONE',  ( -4.164238869374099039, 26.80374883491397142, 8.674139862899312516E-16 ) ) ;
#91219 = CARTESIAN_POINT ( 'NONE',  ( 2.917880565312948704, 47.63708216824730357, 12.26659068614894643 ) ) ;
#91220 = CARTESIAN_POINT ( 'NONE',  ( 12.63842701281683034, 22.46726448433411605, 9.846743663894596210 ) ) ;
#91221 = CARTESIAN_POINT ( 'NONE',  ( 3.640395162852214650, 89.00000000000000000, 12.00000000000000000 ) ) ;
#91222 = MECHANICAL_DESIGN_GEOMETRIC_PRESENTATION_REPRESENTATION (  '', ( #78456 ), #54529 ) ;
#91223 = ORIENTED_EDGE ( 'NONE', *, *, #20344, .T. ) ;
#91224 = CARTESIAN_POINT ( 'NONE',  ( 12.63842701281683922, 29.55059781766745175, -9.846743663894590881 ) ) ;
#91225 = EDGE_CURVE ( 'NONE', #48243, #97330, #49562, .T. ) ;
#91226 = CARTESIAN_POINT ( 'NONE',  ( 0.5774900079438590739, 22.64701867748817321, -5.440088680355550821 ) ) ;
#91227 = CARTESIAN_POINT ( 'NONE',  ( 2.791683348922240793, 51.63393115100078745, 7.208316651077764092 ) ) ;
#91229 = DIRECTION ( 'NONE',  ( 0.000000000000000000, -1.000000000000000000, 0.000000000000000000 ) ) ;
#91228 = CARTESIAN_POINT ( 'NONE',  ( 22.26659068614895176, 9.720415501580633943, -7.082119434687042414 ) ) ;
#91230 = DIRECTION ( 'NONE',  ( 0.8433914458128920488, 0.000000000000000000, -0.5372996083468137840 ) ) ;
#91231 = UNCERTAINTY_MEASURE_WITH_UNIT (LENGTH_MEASURE( 1.000000000000000082E-05 ), #1585, 'distance_accuracy_value', 'NONE');
#91232 = CARTESIAN_POINT ( 'NONE',  ( 0.1532563361054100626, 10.80059781766745175, -2.638427012816831230 ) ) ;
#91233 = CARTESIAN_POINT ( 'NONE',  ( 10.00000000000000178, 35.37363466993042493, 12.81628187352647608 ) ) ;
#91234 = CARTESIAN_POINT ( 'NONE',  ( 19.84674366389459266, 43.71726448433410894, -2.638427012816827677 ) ) ;
#91236 = ORIENTED_EDGE ( 'NONE', *, *, #59388, .F. ) ;
#91235 = ADVANCED_FACE ( 'NONE', ( #96078 ), #19574, .F. ) ;
#91237 = CARTESIAN_POINT ( 'NONE',  ( 0.1532563361054082862, 26.21726448433411605, 2.638427012816831674 ) ) ;
#91238 = CARTESIAN_POINT ( 'NONE',  ( 10.85665724876936089, -52.68265776531869449, -4.000000000000000000 ) ) ;
#91239 = FACE_OUTER_BOUND ( 'NONE', #18744, .T. ) ;
#91240 = CARTESIAN_POINT ( 'NONE',  ( 2.917880565312950480, 55.97041550158063217, -12.26659068614894821 ) ) ;
#91241 = CARTESIAN_POINT ( 'NONE',  ( 20.88017736071110164, 40.35535201082150536, 2.915334737309930979 ) ) ;
#91242 = CARTESIAN_POINT ( 'NONE',  ( -4.164238869374099039, 1.803748834913967647, 8.674139862899312516E-16 ) ) ;
#91243 = CARTESIAN_POINT ( 'NONE',  ( 1.472469842513823179, 31.42559781766745530, 4.923371831947296329 ) ) ;
#91244 = CARTESIAN_POINT ( 'NONE',  ( -0.8801773607111009756, 13.06368534415483929, 1.068504757029289695E-15 ) ) ;
#91245 = CARTESIAN_POINT ( 'NONE',  ( 1.472469842513823179, 36.42559781766745175, 4.923371831947296329 ) ) ;
#91246 = CARTESIAN_POINT ( 'NONE',  ( -1.187721892393765133, 1.950157826164673567E-16, -1.468135075551455948 ) ) ;
#91247 = CARTESIAN_POINT ( 'NONE',  ( 12.63842701281683034, 57.46726448433411605, 9.846743663894596210 ) ) ;
#91248 = CARTESIAN_POINT ( 'NONE',  ( -0.8801773607111008646, 53.27201867748816966, 2.915334737309923430 ) ) ;
#91249 = AXIS2_PLACEMENT_3D ( 'NONE', #49055, #79558, #34031 ) ;
#91250 = VERTEX_POINT ( 'NONE', #20568 ) ;
#91251 = EDGE_LOOP ( 'NONE', ( #2226, #7676, #32354, #54161 ) ) ;
#91252 = CARTESIAN_POINT ( 'NONE',  ( 22.81628187352648496, 56.83196800326374643, -3.434112377981050290 ) ) ;
#91253 = DIRECTION ( 'NONE',  ( 0.000000000000000000, 1.000000000000000000, 0.000000000000000000 ) ) ;
#91254 = CARTESIAN_POINT ( 'NONE',  ( 17.20831665107776587, 12.88393115100078390, 7.208316651077764980 ) ) ;
#91255 = CARTESIAN_POINT ( 'NONE',  ( 19.38216949554541557, 57.24863466993042493, -9.382169495545420901 ) ) ;
#91257 = CARTESIAN_POINT ( 'NONE',  ( 19.84674366389459266, 53.30059781766744464, 2.638427012816836559 ) ) ;
#91256 = CARTESIAN_POINT ( 'NONE',  ( 12.91533473730992121, 4.522018677488170546, 10.88017736071110164 ) ) ;
#91258 = SURFACE_SIDE_STYLE ('',( #21798 ) ) ;
#91259 = CARTESIAN_POINT ( 'NONE',  ( 0.1532563361054083140, 1.008931151000784787, 1.131784320476157264E-15 ) ) ;
#91260 = CARTESIAN_POINT ( 'NONE',  ( 17.08211943468705130, 28.47041550158063572, 12.26659068614894998 ) ) ;
#91261 = CARTESIAN_POINT ( 'NONE',  ( 22.26659068614894466, 43.88708216824729647, 7.082119434687054849 ) ) ;
#91262 = CARTESIAN_POINT ( 'NONE',  ( 0.1532563361054082862, 56.21726448433411605, 2.638427012816831674 ) ) ;
#91263 = MECHANICAL_DESIGN_GEOMETRIC_PRESENTATION_REPRESENTATION (  '', ( #11389 ), #33715 ) ;
#91264 = CARTESIAN_POINT ( 'NONE',  ( 17.35999999999999588, 33.99999999999997868, 9.632054252037205444 ) ) ;
#91265 = CARTESIAN_POINT ( 'NONE',  ( 17.96484262340118221, 51.18868534415483396, -7.964842623401177768 ) ) ;
#91266 = CARTESIAN_POINT ( 'NONE',  ( 19.84674366389459621, 8.508931151000785675, 7.409399052514197653E-17 ) ) ;
#91267 = FILL_AREA_STYLE ('',( #61261 ) ) ;
#91268 = ADVANCED_FACE ( 'NONE', ( #80074 ), #35444, .T. ) ;
#91269 = VERTEX_POINT ( 'NONE', #74539 ) ;
#91270 = CARTESIAN_POINT ( 'NONE',  ( 0.6178305044545818747, 53.49863466993041072, -9.382169495545419124 ) ) ;
#91271 = CIRCLE ( 'NONE', #3636, 1.249999999999987121 ) ;
#91272 = ORIENTED_EDGE ( 'NONE', *, *, #81866, .T. ) ;
#91273 = CARTESIAN_POINT ( 'NONE',  ( 17.20831665107776587, 9.133931151000787452, -7.208316651077762316 ) ) ;
#91274 = ORIENTED_EDGE ( 'NONE', *, *, #92796, .F. ) ;
#91275 = CARTESIAN_POINT ( 'NONE',  ( 10.00000000000000178, 13.05374883491396787, 14.16423886937410082 ) ) ;
#91276 = CARTESIAN_POINT ( 'NONE',  ( 7.361572987183169658, 19.96726448433411960, -9.846743663894592657 ) ) ;
#91277 = CARTESIAN_POINT ( 'NONE',  ( -0.8801773607111008646, 28.27201867748817321, 2.915334737309923430 ) ) ;
#91278 = ADVANCED_FACE ( 'NONE', ( #11580 ), #73057, .F. ) ;
#91279 = CARTESIAN_POINT ( 'NONE',  ( 0.000000000000000000, 14.49999999999999822, 0.000000000000000000 ) ) ;
#91280 = VERTEX_POINT ( 'NONE', #81060 ) ;
#91281 = CARTESIAN_POINT ( 'NONE',  ( 12.91533473730992121, 24.52201867748816966, 10.88017736071110164 ) ) ;
#91282 = ORIENTED_EDGE ( 'NONE', *, *, #17077, .T. ) ;
#91283 = CARTESIAN_POINT ( 'NONE',  ( 10.00000000000000178, 34.31368534415484106, 10.88017736071110342 ) ) ;
#91284 = CARTESIAN_POINT ( 'NONE',  ( 0.000000000000000000, 84.07179676972448590, 12.00000000000000000 ) ) ;
#91285 = ORIENTED_EDGE ( 'NONE', *, *, #24332, .T. ) ;
#91286 = CARTESIAN_POINT ( 'NONE',  ( -2.816281873526471635, 18.91530133659708213, -3.434112377981056508 ) ) ;
#91287 = CARTESIAN_POINT ( 'NONE',  ( 10.00000000000000000, 9.758931151000785675, -9.846743663894594434 ) ) ;
#91288 = FACE_OUTER_BOUND ( 'NONE', #44779, .T. ) ;
#91289 = CARTESIAN_POINT ( 'NONE',  ( -9.000000000000001776, 80.99999999999994316, 0.000000000000000000 ) ) ;
#91290 = CARTESIAN_POINT ( 'NONE',  ( 19.84674366389459266, 13.30059781766745353, 2.638427012816836559 ) ) ;
#91291 = CARTESIAN_POINT ( 'NONE',  ( 12.91533473730993009, 26.60535201082150536, -10.88017736071109987 ) ) ;
#91292 = CIRCLE ( 'NONE', #40273, 10.65000000000026326 ) ;
#91293 = ORIENTED_EDGE ( 'NONE', *, *, #54887, .F. ) ;
#91294 = CARTESIAN_POINT ( 'NONE',  ( 16.40814093676323893, 60.79030133659709634, 11.09922568453595026 ) ) ;
#91295 = CARTESIAN_POINT ( 'NONE',  ( -0.8801773607111009756, 43.06368534415484106, 1.068504757029289695E-15 ) ) ;
#91296 = CARTESIAN_POINT ( 'NONE',  ( -46.85982187872481575, 103.4720723654396721, -5.834173416404226487 ) ) ;
#91297 = CARTESIAN_POINT ( 'NONE',  ( 16.40814093676323893, 50.79030133659708923, 11.09922568453595026 ) ) ;
#91298 = CARTESIAN_POINT ( 'NONE',  ( -0.8801773607111008646, 58.27201867748816966, 2.915334737309923430 ) ) ;
#91299 = CARTESIAN_POINT ( 'NONE',  ( 5.076628168052703671, 66.84226448433412315, 8.527530157486179263 ) ) ;
#91300 = SURFACE_STYLE_FILL_AREA ( #22827 ) ;
#91301 = CARTESIAN_POINT ( 'NONE',  ( 19.84674366389459266, 33.71726448433410894, -2.638427012816827677 ) ) ;
#91302 = CARTESIAN_POINT ( 'NONE',  ( 6.565887622018943937, 48.08196800326375353, -12.81628187352647608 ) ) ;
#91303 = CARTESIAN_POINT ( 'NONE',  ( 0.000000000000000000, 78.76819843555267653, 9.368993295344042238 ) ) ;
#91304 = CARTESIAN_POINT ( 'NONE',  ( 10.00000000000000178, 12.25893115100078568, 9.846743663894594434 ) ) ;
#91305 = CARTESIAN_POINT ( 'NONE',  ( 10.00000000000000000, 17.87363466993041783, -12.81628187352647608 ) ) ;
#91307 = CARTESIAN_POINT ( 'NONE',  ( -46.94000000000001194, 100.4376529975699981, 9.000000000001183054 ) ) ;
#91306 = DIRECTION ( 'NONE',  ( 0.000000000000000000, 1.000000000000000000, 0.000000000000000000 ) ) ;
#91308 = CARTESIAN_POINT ( 'NONE',  ( 12.91533473730992121, 29.52201867748817321, 10.88017736071110164 ) ) ;
#91309 = CARTESIAN_POINT ( 'NONE',  ( 12.63842701281683034, 62.46726448433410894, 9.846743663894596210 ) ) ;
#91310 = CARTESIAN_POINT ( 'NONE',  ( 12.63842701281683922, 24.55059781766745175, -9.846743663894590881 ) ) ;
#91311 = CARTESIAN_POINT ( 'NONE',  ( 5.076628168052704559, 5.175597817667451750, -8.527530157486179263 ) ) ;
#91312 = EDGE_CURVE ( 'NONE', #23152, #81206, #88062, .T. ) ;
#91314 = VERTEX_POINT ( 'NONE', #5576 ) ;
#91313 = CARTESIAN_POINT ( 'NONE',  ( 13.43411237798106583, 12.66530133659708746, -12.81628187352647252 ) ) ;
#91315 = CIRCLE ( 'NONE', #48203, 15.00000000000000000 ) ;
#91316 = CARTESIAN_POINT ( 'NONE',  ( 4.559911319644449179, 7.230352010821504471, -9.422509992056141925 ) ) ;
#91317 = PLANE ( 'NONE',  #3986 ) ;
#91318 = CARTESIAN_POINT ( 'NONE',  ( 6.905507196098383815, -69.44000359822096868, -2.500000000000000000 ) ) ;
#91320 = EDGE_CURVE ( 'NONE', #9418, #92281, #36051, .T. ) ;
#91319 = CARTESIAN_POINT ( 'NONE',  ( -0.8801773607111008646, 3.272018677488171434, 2.915334737309923430 ) ) ;
#91321 = CARTESIAN_POINT ( 'NONE',  ( 5.076628168052704559, 40.17559781766745175, -8.527530157486179263 ) ) ;
#91322 = VERTEX_POINT ( 'NONE', #95578 ) ;
#91323 = DIRECTION ( 'NONE',  ( 0.000000000000000000, 0.000000000000000000, 1.000000000000000000 ) ) ;
#91324 = CARTESIAN_POINT ( 'NONE',  ( -0.8801773607110991993, 7.855352010821506248, -2.915334737309923874 ) ) ;
#91326 = B_SPLINE_CURVE_WITH_KNOTS ( 'NONE', 3,
 ( #98748, #90210, #37240, #52224, #51737, #15723 ),
 .UNSPECIFIED., .F., .F.,
 ( 4, 2, 4 ),
 ( 0.000000000000000000, 0.0002626113303184732001, 0.0005252226606369464002 ),
 .UNSPECIFIED. ) ;
#91325 = CARTESIAN_POINT ( 'NONE',  ( -14.16722289976678617, 15.00000000000000000, -4.928467845925704083 ) ) ;
#91327 = CARTESIAN_POINT ( 'NONE',  ( 0.5774900079438607392, 33.48035201082150536, 5.440088680355550821 ) ) ;
#91328 = CARTESIAN_POINT ( 'NONE',  ( 24.16423886937409904, 49.09541550158063217, 3.795296366450317205 ) ) ;
#91330 = FACE_OUTER_BOUND ( 'NONE', #9749, .T. ) ;
#91329 = CARTESIAN_POINT ( 'NONE',  ( 15.44008868035555260, 4.730352010821505360, 9.422509992056143702 ) ) ;
#91331 = CARTESIAN_POINT ( 'NONE',  ( 7.361572987183170547, 7.050597817667451750, 9.846743663894590881 ) ) ;
#91332 = VECTOR ( 'NONE', #70058, 1000.000000000000000 ) ;
#91333 = CARTESIAN_POINT ( 'NONE',  ( 12.63842701281683922, 19.55059781766745175, -9.846743663894590881 ) ) ;
#91334 = EDGE_CURVE ( 'NONE', #15989, #60007, #13133, .T. ) ;
#91335 = CARTESIAN_POINT ( 'NONE',  ( 16.40814093676324603, 17.45696800326375353, -11.09922568453594671 ) ) ;
#91336 = SURFACE_STYLE_USAGE ( .BOTH. , #60346 ) ;
#91337 = CARTESIAN_POINT ( 'NONE',  ( 6.000000000000000000, 60.50000000000000000, -6.500000000000000888 ) ) ;
#91338 = CARTESIAN_POINT ( 'NONE',  ( -10.32525428029501313, -40.46312579908686757, -4.000000000000000000 ) ) ;
#91339 = CARTESIAN_POINT ( 'NONE',  ( 13.79529636645031943, 15.34541550158063750, -14.16423886937409904 ) ) ;
#91340 = CARTESIAN_POINT ( 'NONE',  ( 12.63842701281683922, 19.55059781766745175, -9.846743663894590881 ) ) ;
#91341 = DIRECTION ( 'NONE',  ( 0.000000000000000000, 1.000000000000000000, 0.000000000000000000 ) ) ;
#91342 = VERTEX_POINT ( 'NONE', #4590 ) ;
#91343 = EDGE_CURVE ( 'NONE', #95512, #33681, #373, .T. ) ;
#91344 = CARTESIAN_POINT ( 'NONE',  ( 24.16423886937410614, 59.30374883491397497, 8.672049930838204340E-16 ) ) ;
#91345 = CARTESIAN_POINT ( 'NONE',  ( 14.92337183194729633, 7.675597817667451750, 8.527530157486181039 ) ) ;
#91347 = LINE ( 'NONE', #23366, #43862 ) ;
#91346 = DIRECTION ( 'NONE',  ( -0.000000000000000000, -1.000000000000000000, 0.000000000000000000 ) ) ;
#91348 = CARTESIAN_POINT ( 'NONE',  ( 0.5774900079438607392, 38.48035201082150536, 5.440088680355550821 ) ) ;
#91349 = CARTESIAN_POINT ( 'NONE',  ( -1.099225684535947600, 53.70696800326376064, -6.408140936763238038 ) ) ;
#91350 = CARTESIAN_POINT ( 'NONE',  ( 7.084665262690076126, 2.022018677488170990, -10.88017736071110164 ) ) ;
#91351 = CARTESIAN_POINT ( 'NONE',  ( 21.09922568453595559, 32.04030133659708923, -6.408140936763230044 ) ) ;
#91352 = CARTESIAN_POINT ( 'NONE',  ( -1.099225684535947600, 4.540301336597087456, 6.408140936763237150 ) ) ;
#91353 = CARTESIAN_POINT ( 'NONE',  ( 17.20831665107776587, 7.883931151000784787, 7.208316651077764980 ) ) ;
#91355 = ORIENTED_EDGE ( 'NONE', *, *, #16039, .F. ) ;
#91354 = EDGE_CURVE ( 'NONE', #28441, #16892, #92974, .T. ) ;
#91356 = CARTESIAN_POINT ( 'NONE',  ( 1.274849032794305170, 12.55509018479935968, -6.499999999999995559 ) ) ;
#91357 = CARTESIAN_POINT ( 'NONE',  ( -11.35178980618966804, 14.49999999999999112, -9.804941009312102551 ) ) ;
#91358 = CARTESIAN_POINT ( 'NONE',  ( -0.3689425029237898834, 41.17874883491397497, -10.36894250292378850 ) ) ;
#91359 = CARTESIAN_POINT ( 'NONE',  ( -2.266590686148945544, 17.22041550158063572, 7.082119434687048631 ) ) ;
#91360 =( NAMED_UNIT ( * ) PLANE_ANGLE_UNIT ( ) SI_UNIT ( $, .RADIAN. ) );
#91361 = CARTESIAN_POINT ( 'NONE',  ( 10.00000000000000000, 31.81368534415483751, -10.88017736071110342 ) ) ;
#91362 = DIRECTION ( 'NONE',  ( -1.000000000000000000, 0.000000000000000000, 0.000000000000000000 ) ) ;
#91363 = FACE_OUTER_BOUND ( 'NONE', #49284, .T. ) ;
#91364 = CARTESIAN_POINT ( 'NONE',  ( 20.88017736071110875, 60.77201867748817676, -2.915334737309920765 ) ) ;
#91365 = CARTESIAN_POINT ( 'NONE',  ( 10.00000000000000178, 69.31368534415484817, 10.88017736071110342 ) ) ;
#91366 = CARTESIAN_POINT ( 'NONE',  ( 10.00000000000000178, 30.37363466993042138, 12.81628187352647608 ) ) ;
#91367 = DIRECTION ( 'NONE',  ( 0.000000000000000000, 0.000000000000000000, 1.000000000000000000 ) ) ;
#91368 = LINE ( 'NONE', #22894, #13157 ) ;
#91369 = CARTESIAN_POINT ( 'NONE',  ( 12.63842701281683034, 32.46726448433412315, 9.846743663894596210 ) ) ;
#91370 = AXIS2_PLACEMENT_3D ( 'NONE', #89559, #22066, #90532 ) ;
#91371 = CARTESIAN_POINT ( 'NONE',  ( 13.43411237798106583, 22.66530133659708923, -12.81628187352647252 ) ) ;
#91372 = CARTESIAN_POINT ( 'NONE',  ( 19.84674366389459266, 13.71726448433411782, -2.638427012816827677 ) ) ;
#91373 = CARTESIAN_POINT ( 'NONE',  ( 2.035157376598822676, 12.43868534415483751, -7.964842623401177768 ) ) ;
#91374 = CARTESIAN_POINT ( 'NONE',  ( 19.84674366389459266, 33.71726448433410894, -2.638427012816827677 ) ) ;
#91375 = CARTESIAN_POINT ( 'NONE',  ( -7.771322705638593398, 15.00000000000000000, 12.24159072200411380 ) ) ;
#91376 = CARTESIAN_POINT ( 'NONE',  ( 18.52753015748617571, 13.09226448433411960, 4.923371831947298993 ) ) ;
#91377 = CARTESIAN_POINT ( 'NONE',  ( -4.164238869374098151, 6.595415501580634832, -3.795296366450310543 ) ) ;
#91378 = DIRECTION ( 'NONE',  ( 0.000000000000000000, 0.000000000000000000, 1.000000000000000000 ) ) ;
#91379 = CARTESIAN_POINT ( 'NONE',  ( 19.42250999205614193, 35.14701867748816966, 5.440088680355555262 ) ) ;
#91381 = CARTESIAN_POINT ( 'NONE',  ( 2.917880565312950480, 40.97041550158063217, -12.26659068614894821 ) ) ;
#91380 = CARTESIAN_POINT ( 'NONE',  ( 7.084665262690076126, 12.02201867748817143, -10.88017736071110164 ) ) ;
#91382 = CARTESIAN_POINT ( 'NONE',  ( 15.44008868035555260, 29.73035201082150891, 9.422509992056143702 ) ) ;
#91383 = CARTESIAN_POINT ( 'NONE',  ( 15.44008868035555793, 11.39701867748817143, -9.422509992056140149 ) ) ;
#91384 = ORIENTED_EDGE ( 'NONE', *, *, #88912, .T. ) ;
#91385 = CARTESIAN_POINT ( 'NONE',  ( 17.96484262340118221, 44.93868534415483396, 7.964842623401181321 ) ) ;
#91386 = CARTESIAN_POINT ( 'NONE',  ( 19.38216949554541557, 42.24863466993041783, -9.382169495545420901 ) ) ;
#91387 = EDGE_CURVE ( 'NONE', #76539, #38225, #42851, .T. ) ;
#91388 = CARTESIAN_POINT ( 'NONE',  ( 17.96484262340118221, 49.93868534415484106, 7.964842623401181321 ) ) ;
#91390 = CARTESIAN_POINT ( 'NONE',  ( 2.035157376598822676, 52.43868534415483396, -7.964842623401177768 ) ) ;
#91389 = SURFACE_STYLE_USAGE ( .BOTH. , #44896 ) ;
#91391 = VECTOR ( 'NONE', #28210, 1000.000000000000000 ) ;
#91392 = ORIENTED_EDGE ( 'NONE', *, *, #84249, .F. ) ;
#91393 = CARTESIAN_POINT ( 'NONE',  ( 19.42250999205614548, 55.98035201082150536, -5.440088680355545492 ) ) ;
#91394 = FILL_AREA_STYLE_COLOUR ( '', #83338 ) ;
#91395 = CARTESIAN_POINT ( 'NONE',  ( -14.26328062697239751, 14.95037112300443383, -3.770429249334984245 ) ) ;
#91396 = CARTESIAN_POINT ( 'NONE',  ( 24.16423886937410614, 44.51208216824730357, -3.795296366450302550 ) ) ;
#91397 = CARTESIAN_POINT ( 'NONE',  ( -0.8801773607111009756, 68.06368534415484817, 1.068504757029289695E-15 ) ) ;
#91398 = CARTESIAN_POINT ( 'NONE',  ( -5.795997163829992083, 0.000000000000000000, -13.01802277140713926 ) ) ;
#91399 = AXIS2_PLACEMENT_3D ( 'NONE', #6827, #13839, #6325 ) ;
#91400 = CARTESIAN_POINT ( 'NONE',  ( -6.857531195348598452, -50.94829529698460391, -3.999999999999998224 ) ) ;
#91401 = CARTESIAN_POINT ( 'NONE',  ( 0.1532563361054083140, 61.00893115100078745, 1.131784320476157264E-15 ) ) ;
#91402 = CIRCLE ( 'NONE', #51436, 14.49999999999999822 ) ;
#91403 = SURFACE_STYLE_FILL_AREA ( #46882 ) ;
#91404 = CARTESIAN_POINT ( 'NONE',  ( 2.791683348922240793, 31.63393115100078745, 7.208316651077764092 ) ) ;
#91405 = VERTEX_POINT ( 'NONE', #68042 ) ;
#91406 = AXIS2_PLACEMENT_3D ( 'NONE', #9120, #26101, #86113 ) ;
#91407 = CARTESIAN_POINT ( 'NONE',  ( 19.84674366389459266, 28.30059781766745886, 2.638427012816836559 ) ) ;
#91408 = CARTESIAN_POINT ( 'NONE',  ( 12.81628187352647252, -3.168031996736245137, -3.434112377981059172 ) ) ;
#91409 = AXIS2_PLACEMENT_3D ( 'NONE', #58369, #51880, #5407 ) ;
#91410 = CARTESIAN_POINT ( 'NONE',  ( 20.88017736071110519, 30.56368534415484106, 2.639326808657452039E-16 ) ) ;
#91411 = CARTESIAN_POINT ( 'NONE',  ( 12.63842701281683034, 37.46726448433411605, 9.846743663894596210 ) ) ;
#91412 = CARTESIAN_POINT ( 'NONE',  ( 19.38216949554541557, 17.24863466993041783, -9.382169495545420901 ) ) ;
#91414 = CARTESIAN_POINT ( 'NONE',  ( 0.5774900079438590739, 57.64701867748817676, -5.440088680355550821 ) ) ;
#91413 = DIRECTION ( 'NONE',  ( 0.000000000000000000, 0.000000000000000000, 1.000000000000000000 ) ) ;
#91416 = CARTESIAN_POINT ( 'NONE',  ( 19.42250999205614193, 5.147018677488171434, 5.440088680355555262 ) ) ;
#91415 = CARTESIAN_POINT ( 'NONE',  ( 20.88017736071110519, 45.56368534415484106, 2.639326808657452039E-16 ) ) ;
#91417 = CARTESIAN_POINT ( 'NONE',  ( 20.36894250292379738, 64.92874883491397497, -10.36894250292379027 ) ) ;
#91418 = VECTOR ( 'NONE', #76943, 1000.000000000000000 ) ;
#91419 = CARTESIAN_POINT ( 'NONE',  ( 0.6178305044545838731, 19.74863466993042138, 9.382169495545420901 ) ) ;
#91420 = DIRECTION ( 'NONE',  ( 1.000000000000000000, -0.000000000000000000, -0.000000000000000000 ) ) ;
#91421 = EDGE_LOOP ( 'NONE', ( #1988, #29799, #77553, #2688 ) ) ;
#91422 = CARTESIAN_POINT ( 'NONE',  ( 3.591859063236761518, 9.956968003263753531, 11.09922568453594849 ) ) ;
#91423 = CARTESIAN_POINT ( 'NONE',  ( 15.44008868035555260, 14.73035201082150536, 9.422509992056143702 ) ) ;
#91424 = CARTESIAN_POINT ( 'NONE',  ( 15.44008868035555260, 59.73035201082151247, 9.422509992056143702 ) ) ;
#91425 = ORIENTED_EDGE ( 'NONE', *, *, #24868, .T. ) ;
#91426 = AXIS2_PLACEMENT_3D ( 'NONE', #29936, #46428, #29439 ) ;
#91427 = B_SPLINE_CURVE_WITH_KNOTS ( 'NONE', 3,
 ( #69186, #29681, #76671, #14216 ),
 .UNSPECIFIED., .F., .F.,
 ( 4, 4 ),
 ( 7.757919228897728493E-18, 0.002392975128318548372 ),
 .UNSPECIFIED. ) ;
#91428 = CARTESIAN_POINT ( 'NONE',  ( 2.035157376598824452, 63.68868534415484106, 7.964842623401179544 ) ) ;
#91429 = CARTESIAN_POINT ( 'NONE',  ( 7.361572987183170547, 42.05059781766745886, 9.846743663894590881 ) ) ;
#91431 = EDGE_CURVE ( 'NONE', #38057, #37189, #94023, .T. ) ;
#91430 = CARTESIAN_POINT ( 'NONE',  ( 12.63842701281683922, 24.55059781766745175, -9.846743663894590881 ) ) ;
#91432 = CARTESIAN_POINT ( 'NONE',  ( 19.84674366389459621, 18.50893115100078745, 7.409399052514197653E-17 ) ) ;
#91433 = CARTESIAN_POINT ( 'NONE',  ( 21.92686044187657046, 57.39664270246084499, -3.195792623639524432 ) ) ;
#91435 = CARTESIAN_POINT ( 'NONE',  ( 21.09922568453595559, 42.04030133659708213, -6.408140936763230044 ) ) ;
#91434 = CARTESIAN_POINT ( 'NONE',  ( 0.2751277870542982451, 17.28217586085238011, -6.500000000000002665 ) ) ;
#91437 = DIRECTION ( 'NONE',  ( 0.000000000000000000, 1.000000000000000000, 0.000000000000000000 ) ) ;
#91436 = CARTESIAN_POINT ( 'NONE',  ( 12.63842701281683922, 9.550597817667449974, -9.846743663894590881 ) ) ;
#91438 = CARTESIAN_POINT ( 'NONE',  ( 21.92686044187657401, 45.37045670184114243, -3.195792623639525765 ) ) ;
#91440 = ORIENTED_EDGE ( 'NONE', *, *, #4085, .F. ) ;
#91439 = CARTESIAN_POINT ( 'NONE',  ( 10.00000000000000000, 29.75893115100078745, -9.846743663894594434 ) ) ;
#91441 = VECTOR ( 'NONE', #77386, 1000.000000000000000 ) ;
#91442 = DIRECTION ( 'NONE',  ( 0.6246950475544238435, 0.7808688094430307203, 0.000000000000000000 ) ) ;
#91443 = CARTESIAN_POINT ( 'NONE',  ( 6.565887622018943937, 10.16530133659708746, 12.81628187352647430 ) ) ;
#91444 = EDGE_CURVE ( 'NONE', #24643, #26555, #36832, .T. ) ;
#91445 = CARTESIAN_POINT ( 'NONE',  ( 10.00000000000000178, 49.31368534415484106, 10.88017736071110342 ) ) ;
#91447 = EDGE_CURVE ( 'NONE', #14105, #34568, #78630, .T. ) ;
#91446 = CARTESIAN_POINT ( 'NONE',  ( 20.36894250292379382, 33.67874883491396076, 10.36894250292379205 ) ) ;
#91448 =( BOUNDED_SURFACE ( )  B_SPLINE_SURFACE ( 3, 2, ( 
 ( #85425, #31420, #47415 ),
 ( #84931, #32412, #16443 ),
 ( #39928, #93414, #78409 ),
 ( #24937, #55419, #484 ),
 ( #30932, #32904, #91938 ),
 ( #63403, #84449, #93908 ),
 ( #15948, #46440, #34371 ),
 ( #26385, #4888, #41427 ),
 ( #42387, #71420, #12371 ),
 ( #64377, #79883, #71888 ),
 ( #88867, #41912, #12859 ),
 ( #73360, #94886, #79401 ),
 ( #10905, #35367, #64861 ),
 ( #72373, #11390, #96387 ) ),
 .UNSPECIFIED., .F., .F., .F. ) 
 B_SPLINE_SURFACE_WITH_KNOTS ( ( 4, 2, 2, 2, 2, 2, 4 ),
 ( 3, 3 ),
 ( 0.000000000000000000, 0.004797171936611957510, 0.007195757904917936265, 0.009594343873223915020, 0.01199292984152989378, 0.01439151580983587253, 0.01918868774644783004 ),
 ( 0.000000000000000000, 1.000000000000000000 ),
 .UNSPECIFIED. ) 
 GEOMETRIC_REPRESENTATION_ITEM ( )  RATIONAL_B_SPLINE_SURFACE ( (
 ( 1.000000000000000000, 0.7071067811865475727, 1.000000000000000000),
 ( 1.000000000000000000, 0.7404680669564855933, 1.000000000000000000),
 ( 1.000000000000000000, 0.7699744256216403127, 1.000000000000000000),
 ( 1.000000000000000000, 0.8013264333395565542, 1.000000000000000000),
 ( 1.000000000000000000, 0.8096066803152818236, 1.000000000000000000),
 ( 1.000000000000000000, 0.8208168491803492506, 1.000000000000000000),
 ( 1.000000000000000000, 0.8237352673350482046, 1.000000000000000000),
 ( 1.000000000000000000, 0.8237872525054150685, 1.000000000000000000),
 ( 1.000000000000000000, 0.8209201555337369838, 1.000000000000000000),
 ( 1.000000000000000000, 0.8097813946838617882, 1.000000000000000000),
 ( 1.000000000000000000, 0.8015207097676279036, 1.000000000000000000),
 ( 1.000000000000000000, 0.7701797223629573974, 1.000000000000000000),
 ( 1.000000000000000000, 0.7406378784107887636, 1.000000000000000000),
 ( 1.000000000000000000, 0.7071067811865475727, 1.000000000000000000) ) ) 
 REPRESENTATION_ITEM ( '' )  SURFACE ( )  );
#91449 = CARTESIAN_POINT ( 'NONE',  ( -12.99123301833645172, 90.70871800849351985, 7.440805305829000460 ) ) ;
#91450 = CARTESIAN_POINT ( 'NONE',  ( 10.00000000000000000, 30.55374883491397142, -14.16423886937410082 ) ) ;
#91451 = CARTESIAN_POINT ( 'NONE',  ( 24.16423886937410614, 64.51208216824728936, -3.795296366450302550 ) ) ;
#91452 = CARTESIAN_POINT ( 'NONE',  ( 22.26659068614895176, 14.72041550158063572, -7.082119434687042414 ) ) ;
#91453 = CARTESIAN_POINT ( 'NONE',  ( 20.36894250292379738, 24.92874883491396787, -10.36894250292379027 ) ) ;
#91454 = CARTESIAN_POINT ( 'NONE',  ( 12.91533473730993009, 41.60535201082149825, -10.88017736071109987 ) ) ;
#91455 = CARTESIAN_POINT ( 'NONE',  ( 4.400664535130860422, -1.180071741297640253, -3.750000000000000888 ) ) ;
#91457 = CARTESIAN_POINT ( 'NONE',  ( 5.076628168052703671, 36.84226448433412315, 8.527530157486179263 ) ) ;
#91456 = CARTESIAN_POINT ( 'NONE',  ( -0.8801773607111008646, 68.27201867748817676, 2.915334737309923430 ) ) ;
#91458 = CARTESIAN_POINT ( 'NONE',  ( 20.88017736071110519, 20.56368534415484106, 2.639326808657452039E-16 ) ) ;
#91459 = LINE ( 'NONE', #45968, #91418 ) ;
#91460 = CARTESIAN_POINT ( 'NONE',  ( 1.472469842513823179, 61.42559781766745175, 4.923371831947296329 ) ) ;
#91461 = CARTESIAN_POINT ( 'NONE',  ( 19.99999999999863576, 84.95449374057137959, -5.196918121119169065 ) ) ;
#91462 = CARTESIAN_POINT ( 'NONE',  ( 10.00000000000000178, 32.25893115100078745, 9.846743663894594434 ) ) ;
#91463 = CARTESIAN_POINT ( 'NONE',  ( 13.43411237798105340, 55.58196800326374643, 12.81628187352647963 ) ) ;
#91464 = CARTESIAN_POINT ( 'NONE',  ( -12.26659068614895354, -8.612917831752692877, -7.082119434687038861 ) ) ;
#91465 = AXIS2_PLACEMENT_3D ( 'NONE', #59383, #28880, #81889 ) ;
#91466 = CARTESIAN_POINT ( 'NONE',  ( 5.076628168052703671, 41.84226448433411605, 8.527530157486179263 ) ) ;
#91467 = CARTESIAN_POINT ( 'NONE',  ( 2.791683348922237240, 50.38393115100078035, -7.208316651077763204 ) ) ;
#91468 = CARTESIAN_POINT ( 'NONE',  ( 24.16423886937410614, 39.51208216824731068, -3.795296366450302550 ) ) ;
#91469 = VERTEX_POINT ( 'NONE', #69028 ) ;
#91470 = CARTESIAN_POINT ( 'NONE',  ( 17.08211943468705840, 15.13708216824730179, -12.26659068614894466 ) ) ;
#91471 = CARTESIAN_POINT ( 'NONE',  ( 20.88017736071110519, 60.56368534415484106, 2.639326808657452039E-16 ) ) ;
#91472 = LINE ( 'NONE', #39948, #17897 ) ;
#91474 = VECTOR ( 'NONE', #61659, 999.9999999999998863 ) ;
#91473 = CARTESIAN_POINT ( 'NONE',  ( -0.3689425029237898834, 61.17874883491396076, -10.36894250292378850 ) ) ;
#91475 = CARTESIAN_POINT ( 'NONE',  ( 22.81628187352647785, 16.62363466993042138, 6.195893100308588602E-16 ) ) ;
#91476 = AXIS2_PLACEMENT_3D ( 'NONE', #79411, #33878, #79889 ) ;
#91477 = DIRECTION ( 'NONE',  ( 0.9890158633619187123, 0.000000000000000000, -0.1478094111295981949 ) ) ;
#91478 = CARTESIAN_POINT ( 'NONE',  ( 2.035157376598824452, 58.68868534415482685, 7.964842623401179544 ) ) ;
#91479 = ADVANCED_FACE ( 'NONE', ( #68 ), #69013, .T. ) ;
#91480 = CARTESIAN_POINT ( 'NONE',  ( -3.750000000000000000, 78.07179676972445748, -4.000000000000000000 ) ) ;
#91481 = FACE_OUTER_BOUND ( 'NONE', #13235, .T. ) ;
#91482 = CARTESIAN_POINT ( 'NONE',  ( 19.38216949554541557, 32.24863466993041783, -9.382169495545420901 ) ) ;
#91483 = CARTESIAN_POINT ( 'NONE',  ( 10.00000000000000178, 58.05374883491397497, 14.16423886937410082 ) ) ;
#91484 = CARTESIAN_POINT ( 'NONE',  ( -5.440088680355547268, 23.89701867748818387, 9.422509992056143702 ) ) ;
#91485 = CARTESIAN_POINT ( 'NONE',  ( 12.91533473730993009, 16.60535201082150891, -10.88017736071109987 ) ) ;
#91487 = CIRCLE ( 'NONE', #49941, 0.2500000000000002220 ) ;
#91486 = CARTESIAN_POINT ( 'NONE',  ( 7.084665262690076126, 19.10535201082150181, 10.88017736071109987 ) ) ;
#91488 = CARTESIAN_POINT ( 'NONE',  ( 2.791683348922240793, 56.63393115100078035, 7.208316651077764092 ) ) ;
#91489 = CARTESIAN_POINT ( 'NONE',  ( 12.63842701281683034, 52.46726448433413026, 9.846743663894596210 ) ) ;
#91490 = CARTESIAN_POINT ( 'NONE',  ( -1.099225684535947600, 49.54030133659708923, 6.408140936763237150 ) ) ;
#91491 = CARTESIAN_POINT ( 'NONE',  ( 0.1532563361054100626, 0.8005978176674514168, -2.638427012816831230 ) ) ;
#91492 = ORIENTED_EDGE ( 'NONE', *, *, #58102, .T. ) ;
#91493 = CARTESIAN_POINT ( 'NONE',  ( 15.44008868035555793, 21.39701867748817321, -9.422509992056140149 ) ) ;
#91494 = CARTESIAN_POINT ( 'NONE',  ( -1.099225684535947600, 23.70696800326375708, -6.408140936763238038 ) ) ;
#91495 = CARTESIAN_POINT ( 'NONE',  ( -5.448048636097841957, 0.000000000000000000, -0.2378669404635215812 ) ) ;
#91496 = CARTESIAN_POINT ( 'NONE',  ( 19.84674366389459266, 43.30059781766744464, 2.638427012816836559 ) ) ;
#91497 = CARTESIAN_POINT ( 'NONE',  ( 15.44008868035555260, 34.73035201082151247, 9.422509992056143702 ) ) ;
#91498 = CARTESIAN_POINT ( 'NONE',  ( 16.40814093676323893, 15.79030133659708746, 11.09922568453595026 ) ) ;
#91500 = LINE ( 'NONE', #31472, #3267 ) ;
#91499 = CARTESIAN_POINT ( 'NONE',  ( -0.8801773607111008646, 53.27201867748816966, 2.915334737309923430 ) ) ;
#91501 = DIRECTION ( 'NONE',  ( 0.000000000000000000, 1.000000000000000000, 0.000000000000000000 ) ) ;
#91502 = CARTESIAN_POINT ( 'NONE',  ( 3.591859063236763294, 48.29030133659708923, -11.09922568453595026 ) ) ;
#91503 = VERTEX_POINT ( 'NONE', #23044 ) ;
#91504 = CARTESIAN_POINT ( 'NONE',  ( 1.472469842513823179, 65.59226448433412315, -4.923371831947296329 ) ) ;
#91505 = DIRECTION ( 'NONE',  ( 0.000000000000000000, 0.000000000000000000, 1.000000000000000000 ) ) ;
#91506 = CARTESIAN_POINT ( 'NONE',  ( 10.00000000000000000, 51.81368534415484106, -10.88017736071110342 ) ) ;
#91508 = CARTESIAN_POINT ( 'NONE',  ( -0.3689425029237898834, 16.17874883491396076, -10.36894250292378850 ) ) ;
#91507 = CARTESIAN_POINT ( 'NONE',  ( 10.00000000000000000, 32.87363466993042493, -12.81628187352647608 ) ) ;
#91509 = CARTESIAN_POINT ( 'NONE',  ( 0.5774900079438590739, 52.64701867748817676, -5.440088680355550821 ) ) ;
#91510 = CARTESIAN_POINT ( 'NONE',  ( -2.266590686148945544, 42.22041550158063217, 7.082119434687048631 ) ) ;
#91511 = VECTOR ( 'NONE', #10859, 1000.000000000000000 ) ;
#91512 = DIRECTION ( 'NONE',  ( -0.000000000000000000, 0.000000000000000000, 1.000000000000000000 ) ) ;
#91513 = CARTESIAN_POINT ( 'NONE',  ( 19.84674366389459621, 18.50893115100078745, 7.409399052514197653E-17 ) ) ;
#91514 = CARTESIAN_POINT ( 'NONE',  ( 19.84674366389459266, 8.300597817667451750, 2.638427012816836559 ) ) ;
#91515 = CARTESIAN_POINT ( 'NONE',  ( 2.562013731377108972, 0.5000000000000000000, -6.499999999999999112 ) ) ;
#91516 = CARTESIAN_POINT ( 'NONE',  ( 20.36894250292379738, 39.92874883491396787, -10.36894250292379027 ) ) ;
#91517 = CARTESIAN_POINT ( 'NONE',  ( 21.92686044187657401, 25.37045670184114243, -3.195792623639525765 ) ) ;
#91518 = AXIS2_PLACEMENT_3D ( 'NONE', #26913, #26414, #48433 ) ;
#91519 = CARTESIAN_POINT ( 'NONE',  ( 2.035157376598822676, 2.438685344154837953, -7.964842623401177768 ) ) ;
#91520 = CARTESIAN_POINT ( 'NONE',  ( -7.037696229836970296, -86.26312365674226612, -4.000000000000000000 ) ) ;
#91521 = ORIENTED_EDGE ( 'NONE', *, *, #16837, .F. ) ;
#91522 = ORIENTED_EDGE ( 'NONE', *, *, #42417, .T. ) ;
#91523 = AXIS2_PLACEMENT_3D ( 'NONE', #86267, #32757, #87237 ) ;
#91524 = CARTESIAN_POINT ( 'NONE',  ( 10.00000000000000178, 14.31368534415483929, 10.88017736071110342 ) ) ;
#91525 = CARTESIAN_POINT ( 'NONE',  ( 6.204703633549690345, 60.76208216824730357, -14.16423886937410259 ) ) ;
#91526 = CARTESIAN_POINT ( 'NONE',  ( 5.076628168052704559, 50.17559781766745886, -8.527530157486179263 ) ) ;
#91527 = CARTESIAN_POINT ( 'NONE',  ( 0.6178305044545838731, 39.74863466993041072, 9.382169495545420901 ) ) ;
#91528 = CARTESIAN_POINT ( 'NONE',  ( 19.72487221294570858, 64.78217586085237656, 6.499999999999992895 ) ) ;
#91530 = CARTESIAN_POINT ( 'NONE',  ( -4.164238869374099927, 2.012082168247300906, 3.795296366450308767 ) ) ;
#91529 = DIRECTION ( 'NONE',  ( 0.000000000000000000, 0.000000000000000000, 1.000000000000000000 ) ) ;
#91531 = CARTESIAN_POINT ( 'NONE',  ( 20.88017736071110519, 30.56368534415484106, 2.639326808657452039E-16 ) ) ;
#91532 = CARTESIAN_POINT ( 'NONE',  ( -2.266590686148945544, 66.38708216824730357, -7.082119434687050408 ) ) ;
#91533 = CARTESIAN_POINT ( 'NONE',  ( 14.92337183194729988, 44.34226448433412315, -8.527530157486177487 ) ) ;
#91534 = CARTESIAN_POINT ( 'NONE',  ( 14.49999999999999822, 61.50000000000000711, 6.500000000000000888 ) ) ;
#91535 = CARTESIAN_POINT ( 'NONE',  ( 7.361572987183169658, 19.96726448433411960, -9.846743663894592657 ) ) ;
#91536 =( NAMED_UNIT ( * ) PLANE_ANGLE_UNIT ( ) SI_UNIT ( $, .RADIAN. ) );
#91537 = CARTESIAN_POINT ( 'NONE',  ( 3.469446951953614189E-15, 17.25893115100080166, 9.846743663894594434 ) ) ;
#91538 = ORIENTED_EDGE ( 'NONE', *, *, #12413, .T. ) ;
#91539 = DIRECTION ( 'NONE',  ( 0.9975640502598243087, -0.06975647374412452528, 0.000000000000000000 ) ) ;
#91540 = EDGE_LOOP ( 'NONE', ( #42586, #89184, #74165, #95328 ) ) ;
#91541 = CARTESIAN_POINT ( 'NONE',  ( 7.361572987183170547, 57.05059781766744464, 9.846743663894590881 ) ) ;
#91543 = CARTESIAN_POINT ( 'NONE',  ( -0.8801773607110991993, 37.85535201082151247, -2.915334737309923874 ) ) ;
#91542 = CARTESIAN_POINT ( 'NONE',  ( -0.8801773607111009756, 33.06368534415484106, 1.068504757029289695E-15 ) ) ;
#91545 = CARTESIAN_POINT ( 'NONE',  ( -1.099225684535947600, 29.54030133659708923, 6.408140936763237150 ) ) ;
#91544 = CARTESIAN_POINT ( 'NONE',  ( 12.63842701281683034, 62.46726448433410894, 9.846743663894596210 ) ) ;
#91546 = CARTESIAN_POINT ( 'NONE',  ( 13.79529636645030344, 13.26208216824729824, 14.16423886937410614 ) ) ;
#91547 = EDGE_CURVE ( 'NONE', #48799, #16296, #64197, .T. ) ;
#91548 = CARTESIAN_POINT ( 'NONE',  ( -2.816281873526473856, 39.12363466993041783, 9.499525473075851096E-16 ) ) ;
#91549 = VERTEX_POINT ( 'NONE', #44540 ) ;
#91550 = TOROIDAL_SURFACE ( 'NONE', #3765, 14.49999999999999822, 0.5000000000000000000 ) ;
#91551 = CARTESIAN_POINT ( 'NONE',  ( 1.472469842513823179, 40.59226448433411605, -4.923371831947296329 ) ) ;
#91552 = CARTESIAN_POINT ( 'NONE',  ( 0.5774900079438607392, 13.48035201082150358, 5.440088680355550821 ) ) ;
#91553 = ORIENTED_EDGE ( 'NONE', *, *, #9620, .T. ) ;
#91554 = CARTESIAN_POINT ( 'NONE',  ( 12.91533473730992121, 14.52201867748817143, 10.88017736071110164 ) ) ;
#91555 = VERTEX_POINT ( 'NONE', #1034 ) ;
#91556 = CARTESIAN_POINT ( 'NONE',  ( 4.559911319644449179, 67.23035201082150536, -9.422509992056141925 ) ) ;
#91557 = CARTESIAN_POINT ( 'NONE',  ( 20.88017736071110519, 55.56368534415484817, 2.639326808657452039E-16 ) ) ;
#91558 = CARTESIAN_POINT ( 'NONE',  ( 2.035157376598822676, 67.43868534415484817, -7.964842623401177768 ) ) ;
#91559 = CIRCLE ( 'NONE', #69220, 1.249999999999987121 ) ;
#91560 = CARTESIAN_POINT ( 'NONE',  ( 0.1532563361054082862, 1.217264484334117824, 2.638427012816831674 ) ) ;
#91561 = EDGE_CURVE ( 'NONE', #55464, #80099, #57842, .T. ) ;
#91562 = CARTESIAN_POINT ( 'NONE',  ( 17.96484262340118221, 51.18868534415483396, -7.964842623401177768 ) ) ;
#91563 = CARTESIAN_POINT ( 'NONE',  ( -8.000000000000000000, 80.99999999999994316, 0.000000000000000000 ) ) ;
#91564 = CARTESIAN_POINT ( 'NONE',  ( -46.82586484710777341, 100.5857744218339036, 9.343464521776596143 ) ) ;
#91566 = ORIENTED_EDGE ( 'NONE', *, *, #8526, .F. ) ;
#91565 = SURFACE_STYLE_FILL_AREA ( #29559 ) ;
#91567 = EDGE_CURVE ( 'NONE', #53936, #46415, #54699, .T. ) ;
#91568 = CARTESIAN_POINT ( 'NONE',  ( 14.92337183194729633, 37.67559781766745175, 8.527530157486181039 ) ) ;
#91569 = EDGE_LOOP ( 'NONE', ( #56861, #40042, #64098, #94733 ) ) ;
#91570 = CARTESIAN_POINT ( 'NONE',  ( 0.000000000000000000, 15.00000000000000000, 0.000000000000000000 ) ) ;
#91572 = EDGE_CURVE ( 'NONE', #66663, #67824, #72580, .T. ) ;
#91571 = SURFACE_SIDE_STYLE ('',( #30060 ) ) ;
#91573 = CARTESIAN_POINT ( 'NONE',  ( 2.917880565312950480, 15.97041550158063217, -12.26659068614894821 ) ) ;
#91574 = CARTESIAN_POINT ( 'NONE',  ( 0.1143410931637277583, 35.21691075486304356, 6.480892540919860778 ) ) ;
#91575 = CARTESIAN_POINT ( 'NONE',  ( 2.831191079880678085, 79.91181047996344944, 5.000000000000000000 ) ) ;
#91576 = CARTESIAN_POINT ( 'NONE',  ( 0.5774900079438607392, 3.480352010821504916, 5.440088680355550821 ) ) ;
#91577 = CARTESIAN_POINT ( 'NONE',  ( 20.15039907845753220, 29.72266099184918531, 6.262539305110077947 ) ) ;
#91579 = ORIENTED_EDGE ( 'NONE', *, *, #91840, .T. ) ;
#91578 = CARTESIAN_POINT ( 'NONE',  ( 22.81628187352647785, 36.62363466993041783, 6.195893100308588602E-16 ) ) ;
#91580 = CARTESIAN_POINT ( 'NONE',  ( 0.000000000000000000, 0.000000000000000000, 0.000000000000000000 ) ) ;
#91581 = CARTESIAN_POINT ( 'NONE',  ( 18.52753015748618282, 63.92559781766745886, -4.923371831947291888 ) ) ;
#91582 = CARTESIAN_POINT ( 'NONE',  ( 0.1532563361054082862, 1.217264484334117824, 2.638427012816831674 ) ) ;
#91583 = CARTESIAN_POINT ( 'NONE',  ( 22.81628187352647785, 21.62363466993041783, 6.195893100308588602E-16 ) ) ;
#91584 = CARTESIAN_POINT ( 'NONE',  ( 19.84674366389459621, 18.50893115100078745, 7.409399052514197653E-17 ) ) ;
#91585 = CARTESIAN_POINT ( 'NONE',  ( -12.34086200392816757, 15.00000000000000000, -7.125000000000143885 ) ) ;
#91586 = CARTESIAN_POINT ( 'NONE',  ( 19.84674366389459621, 18.50893115100078745, 7.409399052514197653E-17 ) ) ;
#91587 = CARTESIAN_POINT ( 'NONE',  ( 21.09922568453594849, 21.20696800326375353, 6.408140936763242479 ) ) ;
#91588 = PRESENTATION_STYLE_ASSIGNMENT (( #22112 ) ) ;
#91589 = CARTESIAN_POINT ( 'NONE',  ( 18.52753015748618282, 8.925597817667451750, -4.923371831947291888 ) ) ;
#91590 = ORIENTED_EDGE ( 'NONE', *, *, #47982, .T. ) ;
#91591 = ORIENTED_EDGE ( 'NONE', *, *, #61362, .F. ) ;
#91592 = CARTESIAN_POINT ( 'NONE',  ( 15.44008868035555793, 26.39701867748817321, -9.422509992056140149 ) ) ;
#91593 = CARTESIAN_POINT ( 'NONE',  ( 2.917880565312948704, 22.63708216824730002, 12.26659068614894643 ) ) ;
#91594 = CARTESIAN_POINT ( 'NONE',  ( 7.361572987183170547, 47.05059781766745175, 9.846743663894590881 ) ) ;
#91595 = CARTESIAN_POINT ( 'NONE',  ( -0.8801773607111008646, 68.27201867748817676, 2.915334737309923430 ) ) ;
#91597 = DIRECTION ( 'NONE',  ( 1.000000000000000000, 0.000000000000000000, 0.000000000000000000 ) ) ;
#91596 = CARTESIAN_POINT ( 'NONE',  ( 22.81628187352647785, 36.41530133659707502, 3.434112377981063169 ) ) ;
#91598 = CARTESIAN_POINT ( 'NONE',  ( 17.96484262340118221, 9.938685344154837509, 7.964842623401181321 ) ) ;
#91599 = EDGE_CURVE ( 'NONE', #86051, #42399, #66869, .T. ) ;
#91600 = DIRECTION ( 'NONE',  ( -0.9961946980917453232, 0.08715574274766037244, 0.000000000000000000 ) ) ;
#91601 = CARTESIAN_POINT ( 'NONE',  ( 6.565887622018943937, 13.08196800326374998, -12.81628187352647608 ) ) ;
#91602 = CARTESIAN_POINT ( 'NONE',  ( 17.20831665107776587, 27.88393115100078390, 7.208316651077764980 ) ) ;
#91603 = CARTESIAN_POINT ( 'NONE',  ( -9.422509992056136596, -6.519647989178492864, 5.440088680355559703 ) ) ;
#91604 = CARTESIAN_POINT ( 'NONE',  ( 21.09922568453594849, 36.20696800326375353, 6.408140936763242479 ) ) ;
#91605 = CARTESIAN_POINT ( 'NONE',  ( 18.39792806157249672, 24.52224192338641373, 6.499999999999999112 ) ) ;
#91607 = DIRECTION ( 'NONE',  ( 1.000000000000000000, 0.000000000000000000, 0.000000000000000000 ) ) ;
#91606 = CARTESIAN_POINT ( 'NONE',  ( -0.8801773607111008646, 53.27201867748816966, 2.915334737309923430 ) ) ;
#91608 = CARTESIAN_POINT ( 'NONE',  ( -14.17193700899791153, -0.03417435944610275333, 1.489530601563921808 ) ) ;
#91609 = CARTESIAN_POINT ( 'NONE',  ( 10.00000000000000000, 66.81368534415484817, -10.88017736071110342 ) ) ;
#91610 = CARTESIAN_POINT ( 'NONE',  ( 20.88017736071110519, 35.56368534415484106, 2.639326808657452039E-16 ) ) ;
#91611 = CARTESIAN_POINT ( 'NONE',  ( 0.5774900079438607392, 43.48035201082151247, 5.440088680355550821 ) ) ;
#91612 = CARTESIAN_POINT ( 'NONE',  ( 12.63842701281683922, 59.55059781766744464, -9.846743663894590881 ) ) ;
#91613 = CARTESIAN_POINT ( 'NONE',  ( 20.88017736071110875, 60.77201867748817676, -2.915334737309920765 ) ) ;
#91614 = AXIS2_PLACEMENT_3D ( 'NONE', #86715, #18219, #48699 ) ;
#91615 = CARTESIAN_POINT ( 'NONE',  ( 18.52753015748618282, 53.92559781766745175, -4.923371831947291888 ) ) ;
#91617 = CARTESIAN_POINT ( 'NONE',  ( 13.82671409943293739, -0.03417435944610275333, 3.447387012295318076 ) ) ;
#91616 = CARTESIAN_POINT ( 'NONE',  ( 2.035157376598822676, 2.438685344154837953, -7.964842623401177768 ) ) ;
#91618 = CARTESIAN_POINT ( 'NONE',  ( -1.099225684535947600, 13.70696800326375353, -6.408140936763238038 ) ) ;
#91619 = ORIENTED_EDGE ( 'NONE', *, *, #13948, .T. ) ;
#91620 = CARTESIAN_POINT ( 'NONE',  ( 15.44008868035555793, 41.39701867748817676, -9.422509992056140149 ) ) ;
#91621 = AXIS2_PLACEMENT_3D ( 'NONE', #65910, #20428, #64429 ) ;
#91623 = FILL_AREA_STYLE_COLOUR ( '', #62093 ) ;
#91622 = CARTESIAN_POINT ( 'NONE',  ( 12.63842701281683922, 59.55059781766744464, -9.846743663894590881 ) ) ;
#91624 = CARTESIAN_POINT ( 'NONE',  ( -0.8801773607111009756, 18.06368534415484106, 1.068504757029289695E-15 ) ) ;
#91625 = CARTESIAN_POINT ( 'NONE',  ( 12.91533473730992121, 29.52201867748817321, 10.88017736071110164 ) ) ;
#91626 = CARTESIAN_POINT ( 'NONE',  ( 6.204703633549690345, 37.84541550158063927, 14.16423886937410082 ) ) ;
#91627 = CARTESIAN_POINT ( 'NONE',  ( 14.92337183194729633, 22.67559781766745175, 8.527530157486181039 ) ) ;
#91628 = CARTESIAN_POINT ( 'NONE',  ( 2.035157376598822676, 52.43868534415483396, -7.964842623401177768 ) ) ;
#91629 = DIRECTION ( 'NONE',  ( 0.000000000000000000, 0.000000000000000000, -1.000000000000000000 ) ) ;
#91630 =( NAMED_UNIT ( * ) SI_UNIT ( $, .STERADIAN. ) SOLID_ANGLE_UNIT ( ) );
#91631 = CARTESIAN_POINT ( 'NONE',  ( -2.614810775378867191, 35.00346125376525919, 7.000000000000000000 ) ) ;
#91632 = CARTESIAN_POINT ( 'NONE',  ( 2.791683348922240793, 61.63393115100079456, 7.208316651077764092 ) ) ;
#91633 = ORIENTED_EDGE ( 'NONE', *, *, #46181, .F. ) ;
#91634 = VERTEX_POINT ( 'NONE', #92497 ) ;
#91635 = CARTESIAN_POINT ( 'NONE',  ( 22.26659068614895176, 34.72041550158063927, -7.082119434687042414 ) ) ;
#91636 = CARTESIAN_POINT ( 'NONE',  ( 24.16423886937410614, 29.51208216824729647, -3.795296366450302550 ) ) ;
#91637 = CARTESIAN_POINT ( 'NONE',  ( 10.00000000000000178, 2.258931151000784787, 9.846743663894594434 ) ) ;
#91638 = CARTESIAN_POINT ( 'NONE',  ( 0.6178305044545818747, 8.498634669930421381, -9.382169495545419124 ) ) ;
#91639 = CARTESIAN_POINT ( 'NONE',  ( 5.076628168052703671, 51.84226448433412315, 8.527530157486179263 ) ) ;
#91640 = CARTESIAN_POINT ( 'NONE',  ( -11.48887051637748691, -88.22984412037381219, 3.750000000000000000 ) ) ;
#91642 = CARTESIAN_POINT ( 'NONE',  ( 13.43411237798106583, 17.66530133659708923, -12.81628187352647252 ) ) ;
#91641 = CARTESIAN_POINT ( 'NONE',  ( 17.96484262340118221, 46.18868534415484106, -7.964842623401177768 ) ) ;
#91643 = CARTESIAN_POINT ( 'NONE',  ( 6.204703633549690345, 27.84541550158063217, 14.16423886937410082 ) ) ;
#91644 = CARTESIAN_POINT ( 'NONE',  ( 2.035157376598824452, 13.68868534415483751, 7.964842623401179544 ) ) ;
#91645 = CARTESIAN_POINT ( 'NONE',  ( 2.035157376598824452, 33.68868534415484106, 7.964842623401179544 ) ) ;
#91646 = CARTESIAN_POINT ( 'NONE',  ( 21.92686044187657046, 5.162123368507804066, 4.562052436263912550E-16 ) ) ;
#91647 = CARTESIAN_POINT ( 'NONE',  ( -0.8801773607111008646, 63.27201867748817676, 2.915334737309923430 ) ) ;
#91648 = CARTESIAN_POINT ( 'NONE',  ( 22.81628187352647785, 51.41530133659708923, 3.434112377981063169 ) ) ;
#91649 = CARTESIAN_POINT ( 'NONE',  ( -4.923371831947302546, -24.82440218233254470, -8.527530157486173934 ) ) ;
#91650 = VERTEX_POINT ( 'NONE', #71000 ) ;
#91651 = FACE_OUTER_BOUND ( 'NONE', #75098, .T. ) ;
#91652 = ORIENTED_EDGE ( 'NONE', *, *, #75995, .T. ) ;
#91653 = CARTESIAN_POINT ( 'NONE',  ( -0.3289641300567998083, 13.07879003517447103, 5.963430220938281678 ) ) ;
#91654 = ORIENTED_EDGE ( 'NONE', *, *, #95067, .F. ) ;
#91655 = DIRECTION ( 'NONE',  ( 0.000000000000000000, -0.000000000000000000, -1.000000000000000000 ) ) ;
#91657 = CARTESIAN_POINT ( 'NONE',  ( -0.8801773607110991993, 2.855352010821504471, -2.915334737309923874 ) ) ;
#91656 = CARTESIAN_POINT ( 'NONE',  ( 24.16423886937409904, 54.09541550158063217, 3.795296366450317205 ) ) ;
#91659 = CARTESIAN_POINT ( 'NONE',  ( 5.076628168052704559, 60.17559781766745175, -8.527530157486179263 ) ) ;
#91658 = CARTESIAN_POINT ( 'NONE',  ( 18.52753015748618282, 23.92559781766745530, -4.923371831947291888 ) ) ;
#91660 = DIRECTION ( 'NONE',  ( -1.000000000000000000, 0.000000000000000000, 0.000000000000000000 ) ) ;
#91661 = ADVANCED_FACE ( 'NONE', ( #24525 ), #95831, .F. ) ;
#91662 = CARTESIAN_POINT ( 'NONE',  ( 0.000000000000000000, 0.000000000000000000, 0.000000000000000000 ) ) ;
#91663 = CARTESIAN_POINT ( 'NONE',  ( 1.472469842513823179, 10.59226448433411782, -4.923371831947296329 ) ) ;
#91664 = CARTESIAN_POINT ( 'NONE',  ( 21.09922568453595559, 7.040301336597086568, -6.408140936763230044 ) ) ;
#91665 = CARTESIAN_POINT ( 'NONE',  ( 9.382169495545419124, 25.99863466993042849, 9.382169495545417348 ) ) ;
#91666 = ORIENTED_EDGE ( 'NONE', *, *, #13689, .F. ) ;
#91667 = CARTESIAN_POINT ( 'NONE',  ( 24.16423886937410614, 29.51208216824729647, -3.795296366450302550 ) ) ;
#91668 = CARTESIAN_POINT ( 'NONE',  ( -0.3689425029237881626, 47.42874883491396787, 10.36894250292379027 ) ) ;
#91669 = ORIENTED_EDGE ( 'NONE', *, *, #95160, .T. ) ;
#91670 = CARTESIAN_POINT ( 'NONE',  ( 22.81628187352648496, 61.83196800326376774, -3.434112377981050290 ) ) ;
#91671 = CARTESIAN_POINT ( 'NONE',  ( 4.559911319644449179, 28.89701867748817321, 9.422509992056141925 ) ) ;
#91672 = CARTESIAN_POINT ( 'NONE',  ( 2.791683348922240793, 51.63393115100078745, 7.208316651077764092 ) ) ;
#91673 = CARTESIAN_POINT ( 'NONE',  ( 15.44008868035555260, 29.73035201082150891, 9.422509992056143702 ) ) ;
#91674 = PLANE ( 'NONE',  #72286 ) ;
#91675 = CARTESIAN_POINT ( 'NONE',  ( -8.099999999999999645, 75.73428692542562146, 3.000000000000000000 ) ) ;
#91676 = CARTESIAN_POINT ( 'NONE',  ( 19.84674366389459621, 53.50893115100078745, 7.409399052514197653E-17 ) ) ;
#91677 = CARTESIAN_POINT ( 'NONE',  ( 12.63842701281683034, 47.46726448433412315, 9.846743663894596210 ) ) ;
#91678 = CARTESIAN_POINT ( 'NONE',  ( -3.843478602184641435, 14.76930270348882068, 14.43834224996319904 ) ) ;
#91679 = EDGE_CURVE ( 'NONE', #22307, #61223, #4833, .T. ) ;
#91680 = CARTESIAN_POINT ( 'NONE',  ( 34.56412365047463453, 26.99999999999999645, -9.500000000000000000 ) ) ;
#91681 = VECTOR ( 'NONE', #1943, 1000.000000000000000 ) ;
#91682 = CARTESIAN_POINT ( 'NONE',  ( -14.40939250470707478, 15.00000000000000000, -1.618458416369986219 ) ) ;
#91683 = ORIENTED_EDGE ( 'NONE', *, *, #13215, .F. ) ;
#91684 = CARTESIAN_POINT ( 'NONE',  ( 2.791683348922240793, 31.63393115100078745, 7.208316651077764092 ) ) ;
#91686 = ADVANCED_FACE ( 'NONE', ( #25013 ), #46647, .T. ) ;
#91685 = DIRECTION ( 'NONE',  ( -0.000000000000000000, -1.000000000000000000, -0.000000000000000000 ) ) ;
#91687 = CARTESIAN_POINT ( 'NONE',  ( 13.43411237798105340, 35.58196800326375353, 12.81628187352647963 ) ) ;
#91688 = DIRECTION ( 'NONE',  ( 0.000000000000000000, 0.000000000000000000, -1.000000000000000000 ) ) ;
#91689 = CARTESIAN_POINT ( 'NONE',  ( 11.35178980618970890, 0.3639309078821234555, 9.804941009312011957 ) ) ;
#91690 = VERTEX_POINT ( 'NONE', #2523 ) ;
#91691 = DIRECTION ( 'NONE',  ( 0.000000000000000000, 0.000000000000000000, -1.000000000000000000 ) ) ;
#91692 = DIRECTION ( 'NONE',  ( -1.000000000000000000, 0.000000000000000000, 0.000000000000000000 ) ) ;
#91693 = CARTESIAN_POINT ( 'NONE',  ( 18.52753015748617571, 53.09226448433412315, 4.923371831947298993 ) ) ;
#91694 = CARTESIAN_POINT ( 'NONE',  ( 10.00000000000000178, 38.05374883491396787, 14.16423886937410082 ) ) ;
#91695 = CARTESIAN_POINT ( 'NONE',  ( 1.472469842513823179, 60.59226448433412315, -4.923371831947296329 ) ) ;
#91696 = DIRECTION ( 'NONE',  ( -1.000000000000000000, 0.000000000000000000, 0.000000000000000000 ) ) ;
#91697 = CARTESIAN_POINT ( 'NONE',  ( 10.00000000000000178, 2.258931151000784787, 9.846743663894594434 ) ) ;
#91698 = PRODUCT_RELATED_PRODUCT_CATEGORY ( 'part', '', ( #98603 ) ) ;
#91699 = CARTESIAN_POINT ( 'NONE',  ( 0.6178305044545818747, 58.49863466993042493, -9.382169495545419124 ) ) ;
#91700 = FACE_OUTER_BOUND ( 'NONE', #80835, .T. ) ;
#91701 = CARTESIAN_POINT ( 'NONE',  ( 2.791683348922240793, 51.63393115100078745, 7.208316651077764092 ) ) ;
#91702 = CARTESIAN_POINT ( 'NONE',  ( 20.88017736071110875, 50.77201867748817676, -2.915334737309920765 ) ) ;
#91703 = CARTESIAN_POINT ( 'NONE',  ( 14.92337183194729633, 47.67559781766745175, 8.527530157486181039 ) ) ;
#91704 =( BOUNDED_SURFACE ( )  B_SPLINE_SURFACE ( 1, 2, ( 
 ( #93252, #40264, #56255, #77754, #48731, #2780, #10748, #79235, #16286, #86747, #24285, #10260, #1309, #33716, #16777, #18252, #46766, #63729, #24776, #32745, #78250, #55252, #33236, #63241, #41266, #9268, #77261, #71740, #94229, #47752, #93745, #3249, #54752, #26236, #85767, #8773, #84777, #17278, #47252, #25761, #39289, #62255, #70275, #70771, #39777, #2286, #85271, #55761, #1793, #40754, #25280, #9767, #71257, #86253, #92760, #17767, #64214, #94731, #48242, #69780, #31759, #32247, #62750, #97222, #35701, #87222, #42715, #81203, #58185, #57705, #19715, #42233, #35193, #5222, #26717, #73198, #27205, #72700, #34704, #96221, #4235, #58693, #36198, #80215, #65199, #95212, #12704, #88205, #57213, #27701, #66186, #50202, #80714, #66695, #13197, #20206, #87710, #43198, #50711, #49229, #19226, #49706, #11721, #56731, #18745, #73687, #5709, #12209, #4729, #65697, #96721, #43690, #74177, #79730, #11229, #88697, #72219, #28197, #89197, #20707, #95720, #51200, #81683, #41749, #3749, #34210, #64700, #23185, #89687, #98708, #21702, #97715, #69170, #44680, #8174, #53169, #74686, #30651, #98206, #91667, #75673, #29179, #60662, #22690, #83675, #38667, #83176, #67191, #38187, #14701, #59679, #7690, #53661, #6198, #13693, #6687, #15189, #68673, #45672, #30158, #91163, #200, #44177, #82680, #82182, #37203, #36702, #51701, #76170, #61158, #90171, #14199, #84178, #46171, #15685, #76654, #60173, #28690, #52186, #75175, #59182, #21202, #67694, #29664, #45172, #68188, #90668, #22195, #52674, #7186, #37690, #71136, #25642, #69654, #16163, #32124, #92158, #31147, #55124, #39662, #32626, #85640, #1180, #93627, #79116, #17159, #93128, #31637, #62622, #10629, #61638, #62129, #92638, #24162, #77143, #33115, #2169, #8652, #47639, #48612, #48120, #41141, #77628, #9145, #2664, #9644, #25162, #23682, #78135, #70153, #63124, #40142, #54632, #55637, #693, #70645, #24654, #85149, #86137, #54146, #84654, #16657, #47131, #1671, #39165, #63609, #17651, #78636, #10143, #46645, #40638, #94115, #56135, #86628, #18140, #80598, #65574, #64095, #41633, #3625, #72099, #13077, #71627, #88579, #20591, #95600, #72584, #65075, #27584, #58576, #28078, #51078, #3136, #4117, #87106, #58075, #34581, #27086, #80096, #5094, #95092, #11600, #18621, #42598, #81569, #66073, #33597, #73077, #64583, #34093, #94610, #87593, #26125, #96101, #49112, #73570, #42119, #35584, #19597, #26600, #4613, #20088, #50591, #56617, #57588, #11114, #81082, #88085, #57097, #12585, #96601, #79613, #19103, #49584, #43084, #89078, #50093, #35074, #12096, #22573, #59067, #97598, #97106, #21585, #89572 ),
 ( #83061, #91045, #6568, #37079, #23071, #92, #7074, #13577, #98596, #37576, #28577, #67578, #45051, #5597, #30539, #51580, #36076, #43571, #7581, #74065, #21083, #15082, #66579, #53044, #82569, #90553, #98088, #14083, #60554, #22082, #76051, #36583, #82068, #45553, #83561, #29546, #52557, #61039, #44061, #84053, #52076, #74568, #6082, #44563, #67071, #38069, #29060, #59568, #90061, #60052, #75061, #14582, #75560, #68069, #30046, #68561, #91552, #53539, #9523, #77512, #92038, #62509, #33004, #40024, #47021, #9029, #70034, #85526, #32512, #56019, #93513, #46054, #1558, #70527, #17039, #16546, #39546, #1059, #93014, #63011, #84546, #32005, #85034, #31525, #92522, #55009, #62021, #17536, #94005, #39047, #24047, #54035, #2050, #24551, #16044, #47518, #25039, #78020, #55524, #25528, #71025, #86021, #46533, #48003, #78511, #586, #10026, #40526, #76541, #2548, #23567, #8058, #15573, #63505, #38556, #77035, #69051, #31030, #61530, #8548, #69542, #54518, #42005, #88465, #42973, #71986, #56979, #11485, #4003, #73453, #86518, #27467, #4981, #27956, #94979, #72471, #57961, #79501, #50465, #4496, #12469, #80969, #18016, #19967, #26008, #80481, #3031, #35461, #18501, #11981, #87970, #87484, #49474, #3510, #64959, #34961, #56502, #34467, #18999, #33969, #64472, #26977, #26483, #65957, #96484, #10999, #79982, #86994, #42482, #95486, #48991, #57476, #65459, #19483, #49975, #48498, #79000, #72965, #41519, #95986, #10505, #71521, #41020, #33480, #63976, #94490, #66449, #50959, #58449, #22451, #88964, #35953, #29428, #67451, #75436, #96984, #20971, #51456, #13965, #60428, #14957, #43940, #28935, #82441, #74942, #45424, #20472, #98470, #75929, #98963, #66953, #44440, #29923, #81945, #52924, #6950, #83437, #7454, #81455, #90921, #28461, #52442, #73954, #37951, #89455, #68444, #12956, #37457, #97471, #6445, #51957, #59440, #67945, #36954, #43452, #13455, #5480, #58955, #74439, #21459, #97972, #5964, #36458, #89942, #59933, #90422, #21961, #82940, #14457, #44929, #83925, #7940, #15927, #17775, #84430, #48251, #68933, #2793, #23443, #25770, #78762, #23928, #56264, #92405, #38435, #10270, #49238, #86757, #61898, #54399, #86262, #33245, #48741, #72229, #10760, #60919, #40764, #94740, #91424, #463, #63739, #71266, #79246, #30911, #91918, #53921, #94240, #33725, #87235, #46419, #938, #18262, #41275, #18757, #30419, #71750, #79742, #22952, #38928, #3257, #64224, #76908, #26245, #56739, #11239, #41758, #53418, #15455, #61409, #45934, #76425, #8421, #69415, #31399, #64712, #81696, #42730, #50724, #96233, #73207, #20720, #81214, #36209, #95732, #95221 ) ),
 .UNSPECIFIED., .F., .F., .F. ) 
 B_SPLINE_SURFACE_WITH_KNOTS ( ( 2, 2 ),
 ( 3, 2, 2, 2, 2, 2, 2, 2, 2, 2, 2, 2, 2, 2, 2, 2, 2, 2, 2, 2, 2, 2, 2, 2, 2, 2, 2, 2, 2, 2, 2, 2, 2, 2, 2, 2, 2, 2, 2, 2, 2, 2, 2, 2, 2, 2, 2, 2, 2, 2, 2, 2, 2, 2, 2, 2, 2, 2, 2, 2, 2, 2, 2, 2, 2, 2, 2, 2, 2, 2, 2, 2, 2, 2, 2, 2, 2, 2, 2, 2, 2, 2, 2, 2, 2, 2, 2, 2, 2, 2, 2, 2, 2, 2, 2, 2, 2, 2, 2, 2, 2, 2, 2, 2, 2, 2, 2, 2, 2, 2, 2, 2, 2, 2, 2, 2, 2, 2, 2, 2, 2, 2, 2, 2, 2, 2, 2, 2, 2, 2, 2, 2, 2, 2, 2, 2, 2, 2, 2, 2, 2, 2, 2, 2, 2, 2, 2, 2, 2, 2, 2, 2, 2, 2, 2, 2, 2, 2, 2, 2, 2, 2, 3 ),
 ( 0.000000000000000000, 1.000000000000000000 ),
 ( 0.000000000000000000, 0.005952380952380952051, 0.01190476190476190410, 0.01785714285714285615, 0.02380952380952380820, 0.02976190476190476025, 0.03571428571428571230, 0.04166666666666666435, 0.04761904761904761640, 0.05357142857142856845, 0.05952380952380952051, 0.06547619047619047949, 0.07142857142857142461, 0.07738095238095238360, 0.08333333333333332871, 0.08928571428571428770, 0.09523809523809523281, 0.1011904761904761918, 0.1071428571428571369, 0.1130952380952380959, 0.1190476190476190410, 0.1250000000000000000, 0.1309523809523809590, 0.1369047619047619180, 0.1428571428571428492, 0.1488095238095238082, 0.1547619047619047672, 0.1607142857142857262, 0.1666666666666666574, 0.1726190476190476164, 0.1785714285714285754, 0.1845238095238095344, 0.1904761904761904656, 0.1964285714285714246, 0.2023809523809523836, 0.2083333333333333426, 0.2142857142857142738, 0.2202380952380952328, 0.2261904761904761918, 0.2321428571428571508, 0.2380952380952380820, 0.2440476190476190410, 0.2500000000000000000, 0.2559523809523809312, 0.2619047619047619180, 0.2678571428571428492, 0.2738095238095238360, 0.2797619047619047672, 0.2857142857142856984, 0.2916666666666666852, 0.2976190476190476164, 0.3035714285714285476, 0.3095238095238095344, 0.3154761904761904656, 0.3214285714285714524, 0.3273809523809523836, 0.3333333333333333148, 0.3392857142857143016, 0.3452380952380952328, 0.3511904761904761640, 0.3571428571428571508, 0.3630952380952380820, 0.3690476190476190688, 0.3750000000000000000, 0.3809523809523809312, 0.3869047619047619180, 0.3928571428571428492, 0.3988095238095238360, 0.4047619047619047672, 0.4107142857142856984, 0.4166666666666666852, 0.4226190476190476164, 0.4285714285714285476, 0.4345238095238095344, 0.4404761904761904656, 0.4464285714285714524, 0.4523809523809523836, 0.4583333333333333148, 0.4642857142857143016, 0.4702380952380952328, 0.4761904761904761640, 0.4821428571428571508, 0.4880952380952380820, 0.4940476190476190688, 0.5000000000000000000, 0.5059523809523809312, 0.5119047619047618625, 0.5178571428571429047, 0.5238095238095238360, 0.5297619047619047672, 0.5357142857142856984, 0.5416666666666666297, 0.5476190476190476719, 0.5535714285714286031, 0.5595238095238095344, 0.5654761904761904656, 0.5714285714285713969, 0.5773809523809523281, 0.5833333333333333703, 0.5892857142857143016, 0.5952380952380952328, 0.6011904761904761640, 0.6071428571428570953, 0.6130952380952381375, 0.6190476190476190688, 0.6250000000000000000, 0.6309523809523809312, 0.6369047619047618625, 0.6428571428571429047, 0.6488095238095238360, 0.6547619047619047672, 0.6607142857142856984, 0.6666666666666666297, 0.6726190476190476719, 0.6785714285714286031, 0.6845238095238095344, 0.6904761904761904656, 0.6964285714285713969, 0.7023809523809523281, 0.7083333333333333703, 0.7142857142857143016, 0.7202380952380952328, 0.7261904761904761640, 0.7321428571428570953, 0.7380952380952381375, 0.7440476190476190688, 0.7500000000000000000, 0.7559523809523809312, 0.7619047619047618625, 0.7678571428571429047, 0.7738095238095238360, 0.7797619047619047672, 0.7857142857142856984, 0.7916666666666666297, 0.7976190476190476719, 0.8035714285714286031, 0.8095238095238095344, 0.8154761904761904656, 0.8214285714285713969, 0.8273809523809523281, 0.8333333333333333703, 0.8392857142857143016, 0.8452380952380952328, 0.8511904761904761640, 0.8571428571428570953, 0.8630952380952381375, 0.8690476190476190688, 0.8750000000000000000, 0.8809523809523809312, 0.8869047619047618625, 0.8928571428571429047, 0.8988095238095238360, 0.9047619047619047672, 0.9107142857142856984, 0.9166666666666666297, 0.9226190476190476719, 0.9285714285714286031, 0.9345238095238095344, 0.9404761904761904656, 0.9464285714285713969, 0.9523809523809523281, 0.9583333333333333703, 0.9642857142857143016 ),
 .UNSPECIFIED. ) 
 GEOMETRIC_REPRESENTATION_ITEM ( )  RATIONAL_B_SPLINE_SURFACE ( (
 ( 1.000000000000000000, 0.9659258262890683122, 1.000000000000000000, 0.9659258262890683122, 1.000000000000000000, 0.9659258262890683122, 1.000000000000000000, 0.9659258262890683122, 1.000000000000000000, 0.9659258262890683122, 1.000000000000000000, 0.9659258262890683122, 1.000000000000000000, 0.9659258262890683122, 1.000000000000000000, 0.9659258262890683122, 1.000000000000000000, 0.9659258262890683122, 1.000000000000000000, 0.9659258262890683122, 1.000000000000000000, 0.9659258262890683122, 1.000000000000000000, 0.9659258262890683122, 1.000000000000000000, 0.9659258262890683122, 1.000000000000000000, 0.9659258262890683122, 1.000000000000000000, 0.9659258262890683122, 1.000000000000000000, 0.9659258262890683122, 1.000000000000000000, 0.9659258262890683122, 1.000000000000000000, 0.9659258262890683122, 1.000000000000000000, 0.9659258262890683122, 1.000000000000000000, 0.9659258262890683122, 1.000000000000000000, 0.9659258262890683122, 1.000000000000000000, 0.9659258262890683122, 1.000000000000000000, 0.9659258262890683122, 1.000000000000000000, 0.9659258262890683122, 1.000000000000000000, 0.9659258262890683122, 1.000000000000000000, 0.9659258262890683122, 1.000000000000000000, 0.9659258262890683122, 1.000000000000000000, 0.9659258262890683122, 1.000000000000000000, 0.9659258262890683122, 1.000000000000000000, 0.9659258262890683122, 1.000000000000000000, 0.9659258262890683122, 1.000000000000000000, 0.9659258262890683122, 1.000000000000000000, 0.9659258262890683122, 1.000000000000000000, 0.9659258262890683122, 1.000000000000000000, 0.9659258262890683122, 1.000000000000000000, 0.9659258262890683122, 1.000000000000000000, 0.9659258262890683122, 1.000000000000000000, 0.9659258262890683122, 1.000000000000000000, 0.9659258262890683122, 1.000000000000000000, 0.9659258262890683122, 1.000000000000000000, 0.9659258262890683122, 1.000000000000000000, 0.9659258262890683122, 1.000000000000000000, 0.9659258262890683122, 1.000000000000000000, 0.9659258262890683122, 1.000000000000000000, 0.9659258262890683122, 1.000000000000000000, 0.9659258262890683122, 1.000000000000000000, 0.9659258262890683122, 1.000000000000000000, 0.9659258262890683122, 1.000000000000000000, 0.9659258262890683122, 1.000000000000000000, 0.9659258262890683122, 1.000000000000000000, 0.9659258262890683122, 1.000000000000000000, 0.9659258262890683122, 1.000000000000000000, 0.9659258262890683122, 1.000000000000000000, 0.9659258262890683122, 1.000000000000000000, 0.9659258262890683122, 1.000000000000000000, 0.9659258262890683122, 1.000000000000000000, 0.9659258262890683122, 1.000000000000000000, 0.9659258262890683122, 1.000000000000000000, 0.9659258262890683122, 1.000000000000000000, 0.9659258262890683122, 1.000000000000000000, 0.9659258262890683122, 1.000000000000000000, 0.9659258262890683122, 1.000000000000000000, 0.9659258262890683122, 1.000000000000000000, 0.9659258262890683122, 1.000000000000000000, 0.9659258262890683122, 1.000000000000000000, 0.9659258262890683122, 1.000000000000000000, 0.9659258262890683122, 1.000000000000000000, 0.9659258262890683122, 1.000000000000000000, 0.9659258262890683122, 1.000000000000000000, 0.9659258262890683122, 1.000000000000000000, 0.9659258262890683122, 1.000000000000000000, 0.9659258262890683122, 1.000000000000000000, 0.9659258262890683122, 1.000000000000000000, 0.9659258262890683122, 1.000000000000000000, 0.9659258262890683122, 1.000000000000000000, 0.9659258262890683122, 1.000000000000000000, 0.9659258262890683122, 1.000000000000000000, 0.9659258262890683122, 1.000000000000000000, 0.9659258262890683122, 1.000000000000000000, 0.9659258262890683122, 1.000000000000000000, 0.9659258262890683122, 1.000000000000000000, 0.9659258262890683122, 1.000000000000000000, 0.9659258262890683122, 1.000000000000000000, 0.9659258262890683122, 1.000000000000000000, 0.9659258262890683122, 1.000000000000000000, 0.9659258262890683122, 1.000000000000000000, 0.9659258262890683122, 1.000000000000000000, 0.9659258262890683122, 1.000000000000000000, 0.9659258262890683122, 1.000000000000000000, 0.9659258262890683122, 1.000000000000000000, 0.9659258262890683122, 1.000000000000000000, 0.9659258262890683122, 1.000000000000000000, 0.9659258262890683122, 1.000000000000000000, 0.9659258262890683122, 1.000000000000000000, 0.9659258262890683122, 1.000000000000000000, 0.9659258262890683122, 1.000000000000000000, 0.9659258262890683122, 1.000000000000000000, 0.9659258262890683122, 1.000000000000000000, 0.9659258262890683122, 1.000000000000000000, 0.9659258262890683122, 1.000000000000000000, 0.9659258262890683122, 1.000000000000000000, 0.9659258262890683122, 1.000000000000000000, 0.9659258262890683122, 1.000000000000000000, 0.9659258262890683122, 1.000000000000000000, 0.9659258262890683122, 1.000000000000000000, 0.9659258262890683122, 1.000000000000000000, 0.9659258262890683122, 1.000000000000000000, 0.9659258262890683122, 1.000000000000000000, 0.9659258262890683122, 1.000000000000000000, 0.9659258262890683122, 1.000000000000000000, 0.9659258262890683122, 1.000000000000000000, 0.9659258262890683122, 1.000000000000000000, 0.9659258262890683122, 1.000000000000000000, 0.9659258262890683122, 1.000000000000000000, 0.9659258262890683122, 1.000000000000000000, 0.9659258262890683122, 1.000000000000000000, 0.9659258262890683122, 1.000000000000000000, 0.9659258262890683122, 1.000000000000000000, 0.9659258262890683122, 1.000000000000000000, 0.9659258262890683122, 1.000000000000000000, 0.9659258262890683122, 1.000000000000000000, 0.9659258262890683122, 1.000000000000000000, 0.9659258262890683122, 1.000000000000000000, 0.9659258262890683122, 1.000000000000000000, 0.9659258262890683122, 1.000000000000000000, 0.9659258262890683122, 1.000000000000000000, 0.9659258262890683122, 1.000000000000000000, 0.9659258262890683122, 1.000000000000000000, 0.9659258262890683122, 1.000000000000000000, 0.9659258262890683122, 1.000000000000000000, 0.9659258262890683122, 1.000000000000000000, 0.9659258262890683122, 1.000000000000000000, 0.9659258262890683122, 1.000000000000000000, 0.9659258262890683122, 1.000000000000000000, 0.9659258262890683122, 1.000000000000000000, 0.9659258262890683122, 1.000000000000000000, 0.9659258262890683122, 1.000000000000000000, 0.9659258262890683122, 1.000000000000000000, 0.9659258262890683122, 1.000000000000000000, 0.9659258262890683122, 1.000000000000000000, 0.9659258262890683122, 1.000000000000000000, 0.9659258262890683122, 1.000000000000000000, 0.9659258262890683122, 1.000000000000000000, 0.9659258262890683122, 1.000000000000000000, 0.9659258262890683122, 1.000000000000000000, 0.9659258262890683122, 1.000000000000000000, 0.9659258262890683122, 1.000000000000000000, 0.9659258262890683122, 1.000000000000000000, 0.9659258262890683122, 1.000000000000000000, 0.9659258262890683122, 1.000000000000000000, 0.9659258262890683122, 1.000000000000000000, 0.9659258262890683122, 1.000000000000000000, 0.9659258262890683122, 1.000000000000000000, 0.9659258262890683122, 1.000000000000000000, 0.9659258262890683122, 1.000000000000000000, 0.9659258262890683122, 1.000000000000000000, 0.9659258262890683122, 1.000000000000000000, 0.9659258262890683122, 1.000000000000000000, 0.9659258262890683122, 1.000000000000000000, 0.9659258262890683122, 1.000000000000000000, 0.9659258262890683122, 1.000000000000000000, 0.9659258262890683122, 1.000000000000000000),
 ( 1.000000000000000000, 0.9659258262890683122, 1.000000000000000000, 0.9659258262890683122, 1.000000000000000000, 0.9659258262890683122, 1.000000000000000000, 0.9659258262890683122, 1.000000000000000000, 0.9659258262890683122, 1.000000000000000000, 0.9659258262890683122, 1.000000000000000000, 0.9659258262890683122, 1.000000000000000000, 0.9659258262890683122, 1.000000000000000000, 0.9659258262890683122, 1.000000000000000000, 0.9659258262890683122, 1.000000000000000000, 0.9659258262890683122, 1.000000000000000000, 0.9659258262890683122, 1.000000000000000000, 0.9659258262890683122, 1.000000000000000000, 0.9659258262890683122, 1.000000000000000000, 0.9659258262890683122, 1.000000000000000000, 0.9659258262890683122, 1.000000000000000000, 0.9659258262890683122, 1.000000000000000000, 0.9659258262890683122, 1.000000000000000000, 0.9659258262890683122, 1.000000000000000000, 0.9659258262890683122, 1.000000000000000000, 0.9659258262890683122, 1.000000000000000000, 0.9659258262890683122, 1.000000000000000000, 0.9659258262890683122, 1.000000000000000000, 0.9659258262890683122, 1.000000000000000000, 0.9659258262890683122, 1.000000000000000000, 0.9659258262890683122, 1.000000000000000000, 0.9659258262890683122, 1.000000000000000000, 0.9659258262890683122, 1.000000000000000000, 0.9659258262890683122, 1.000000000000000000, 0.9659258262890683122, 1.000000000000000000, 0.9659258262890683122, 1.000000000000000000, 0.9659258262890683122, 1.000000000000000000, 0.9659258262890683122, 1.000000000000000000, 0.9659258262890683122, 1.000000000000000000, 0.9659258262890683122, 1.000000000000000000, 0.9659258262890683122, 1.000000000000000000, 0.9659258262890683122, 1.000000000000000000, 0.9659258262890683122, 1.000000000000000000, 0.9659258262890683122, 1.000000000000000000, 0.9659258262890683122, 1.000000000000000000, 0.9659258262890683122, 1.000000000000000000, 0.9659258262890683122, 1.000000000000000000, 0.9659258262890683122, 1.000000000000000000, 0.9659258262890683122, 1.000000000000000000, 0.9659258262890683122, 1.000000000000000000, 0.9659258262890683122, 1.000000000000000000, 0.9659258262890683122, 1.000000000000000000, 0.9659258262890683122, 1.000000000000000000, 0.9659258262890683122, 1.000000000000000000, 0.9659258262890683122, 1.000000000000000000, 0.9659258262890683122, 1.000000000000000000, 0.9659258262890683122, 1.000000000000000000, 0.9659258262890683122, 1.000000000000000000, 0.9659258262890683122, 1.000000000000000000, 0.9659258262890683122, 1.000000000000000000, 0.9659258262890683122, 1.000000000000000000, 0.9659258262890683122, 1.000000000000000000, 0.9659258262890683122, 1.000000000000000000, 0.9659258262890683122, 1.000000000000000000, 0.9659258262890683122, 1.000000000000000000, 0.9659258262890683122, 1.000000000000000000, 0.9659258262890683122, 1.000000000000000000, 0.9659258262890683122, 1.000000000000000000, 0.9659258262890683122, 1.000000000000000000, 0.9659258262890683122, 1.000000000000000000, 0.9659258262890683122, 1.000000000000000000, 0.9659258262890683122, 1.000000000000000000, 0.9659258262890683122, 1.000000000000000000, 0.9659258262890683122, 1.000000000000000000, 0.9659258262890683122, 1.000000000000000000, 0.9659258262890683122, 1.000000000000000000, 0.9659258262890683122, 1.000000000000000000, 0.9659258262890683122, 1.000000000000000000, 0.9659258262890683122, 1.000000000000000000, 0.9659258262890683122, 1.000000000000000000, 0.9659258262890683122, 1.000000000000000000, 0.9659258262890683122, 1.000000000000000000, 0.9659258262890683122, 1.000000000000000000, 0.9659258262890683122, 1.000000000000000000, 0.9659258262890683122, 1.000000000000000000, 0.9659258262890683122, 1.000000000000000000, 0.9659258262890683122, 1.000000000000000000, 0.9659258262890683122, 1.000000000000000000, 0.9659258262890683122, 1.000000000000000000, 0.9659258262890683122, 1.000000000000000000, 0.9659258262890683122, 1.000000000000000000, 0.9659258262890683122, 1.000000000000000000, 0.9659258262890683122, 1.000000000000000000, 0.9659258262890683122, 1.000000000000000000, 0.9659258262890683122, 1.000000000000000000, 0.9659258262890683122, 1.000000000000000000, 0.9659258262890683122, 1.000000000000000000, 0.9659258262890683122, 1.000000000000000000, 0.9659258262890683122, 1.000000000000000000, 0.9659258262890683122, 1.000000000000000000, 0.9659258262890683122, 1.000000000000000000, 0.9659258262890683122, 1.000000000000000000, 0.9659258262890683122, 1.000000000000000000, 0.9659258262890683122, 1.000000000000000000, 0.9659258262890683122, 1.000000000000000000, 0.9659258262890683122, 1.000000000000000000, 0.9659258262890683122, 1.000000000000000000, 0.9659258262890683122, 1.000000000000000000, 0.9659258262890683122, 1.000000000000000000, 0.9659258262890683122, 1.000000000000000000, 0.9659258262890683122, 1.000000000000000000, 0.9659258262890683122, 1.000000000000000000, 0.9659258262890683122, 1.000000000000000000, 0.9659258262890683122, 1.000000000000000000, 0.9659258262890683122, 1.000000000000000000, 0.9659258262890683122, 1.000000000000000000, 0.9659258262890683122, 1.000000000000000000, 0.9659258262890683122, 1.000000000000000000, 0.9659258262890683122, 1.000000000000000000, 0.9659258262890683122, 1.000000000000000000, 0.9659258262890683122, 1.000000000000000000, 0.9659258262890683122, 1.000000000000000000, 0.9659258262890683122, 1.000000000000000000, 0.9659258262890683122, 1.000000000000000000, 0.9659258262890683122, 1.000000000000000000, 0.9659258262890683122, 1.000000000000000000, 0.9659258262890683122, 1.000000000000000000, 0.9659258262890683122, 1.000000000000000000, 0.9659258262890683122, 1.000000000000000000, 0.9659258262890683122, 1.000000000000000000, 0.9659258262890683122, 1.000000000000000000, 0.9659258262890683122, 1.000000000000000000, 0.9659258262890683122, 1.000000000000000000, 0.9659258262890683122, 1.000000000000000000, 0.9659258262890683122, 1.000000000000000000, 0.9659258262890683122, 1.000000000000000000, 0.9659258262890683122, 1.000000000000000000, 0.9659258262890683122, 1.000000000000000000, 0.9659258262890683122, 1.000000000000000000, 0.9659258262890683122, 1.000000000000000000, 0.9659258262890683122, 1.000000000000000000, 0.9659258262890683122, 1.000000000000000000, 0.9659258262890683122, 1.000000000000000000, 0.9659258262890683122, 1.000000000000000000, 0.9659258262890683122, 1.000000000000000000, 0.9659258262890683122, 1.000000000000000000, 0.9659258262890683122, 1.000000000000000000, 0.9659258262890683122, 1.000000000000000000, 0.9659258262890683122, 1.000000000000000000, 0.9659258262890683122, 1.000000000000000000, 0.9659258262890683122, 1.000000000000000000, 0.9659258262890683122, 1.000000000000000000, 0.9659258262890683122, 1.000000000000000000, 0.9659258262890683122, 1.000000000000000000, 0.9659258262890683122, 1.000000000000000000, 0.9659258262890683122, 1.000000000000000000, 0.9659258262890683122, 1.000000000000000000, 0.9659258262890683122, 1.000000000000000000, 0.9659258262890683122, 1.000000000000000000, 0.9659258262890683122, 1.000000000000000000, 0.9659258262890683122, 1.000000000000000000, 0.9659258262890683122, 1.000000000000000000, 0.9659258262890683122, 1.000000000000000000, 0.9659258262890683122, 1.000000000000000000, 0.9659258262890683122, 1.000000000000000000, 0.9659258262890683122, 1.000000000000000000, 0.9659258262890683122, 1.000000000000000000) ) ) 
 REPRESENTATION_ITEM ( '' )  SURFACE ( )  );
#91705 = CYLINDRICAL_SURFACE ( 'NONE', #14015, 1.000000000000000888 ) ;
#91706 = CARTESIAN_POINT ( 'NONE',  ( 20.88017736071110164, 55.35535201082149825, 2.915334737309930979 ) ) ;
#91707 = ORIENTED_EDGE ( 'NONE', *, *, #24384, .T. ) ;
#91708 = CARTESIAN_POINT ( 'NONE',  ( 0.000000000000000000, 14.49999999999999822, 0.000000000000000000 ) ) ;
#91709 = CARTESIAN_POINT ( 'NONE',  ( -0.8801773607111008646, 28.27201867748817321, 2.915334737309923430 ) ) ;
#91711 = CARTESIAN_POINT ( 'NONE',  ( 20.88017736071110519, 55.56368534415484817, 2.639326808657452039E-16 ) ) ;
#91710 = CARTESIAN_POINT ( 'NONE',  ( 2.791683348922240793, 66.63393115100079456, 7.208316651077764092 ) ) ;
#91712 = LINE ( 'NONE', #23231, #18496 ) ;
#91713 = DIRECTION ( 'NONE',  ( 0.5664062369248313855, 0.000000000000000000, -0.8241261886220166977 ) ) ;
#91715 = CARTESIAN_POINT ( 'NONE',  ( -46.71039645252511718, 100.6859025094012026, 9.426366605710914115 ) ) ;
#91714 = CARTESIAN_POINT ( 'NONE',  ( 15.44008868035555260, 34.73035201082151247, 9.422509992056143702 ) ) ;
#91716 = CARTESIAN_POINT ( 'NONE',  ( 12.63842701281683034, 17.46726448433411250, 9.846743663894596210 ) ) ;
#91717 = CARTESIAN_POINT ( 'NONE',  ( 2.791683348922237240, 40.38393115100078035, -7.208316651077763204 ) ) ;
#91718 = CARTESIAN_POINT ( 'NONE',  ( 4.629999999999991900, 76.07179676972444327, 4.250000000000000000 ) ) ;
#91719 = CARTESIAN_POINT ( 'NONE',  ( 14.16423886937410259, 14.30374883491396965, -2.602085213965210642E-15 ) ) ;
#91720 = CARTESIAN_POINT ( 'NONE',  ( 5.076628168052704559, 65.17559781766745175, -8.527530157486179263 ) ) ;
#91721 = CARTESIAN_POINT ( 'NONE',  ( 24.16423886937409904, 64.09541550158064638, 3.795296366450317205 ) ) ;
#91722 = FACE_BOUND ( 'NONE', #52662, .T. ) ;
#91723 = CIRCLE ( 'NONE', #955, 0.09999999999999982514 ) ;
#91724 = CARTESIAN_POINT ( 'NONE',  ( -2.266590686148945544, 27.22041550158063572, 7.082119434687048631 ) ) ;
#91725 = CARTESIAN_POINT ( 'NONE',  ( -2.266590686148945544, 57.22041550158063217, 7.082119434687048631 ) ) ;
#91726 = CARTESIAN_POINT ( 'NONE',  ( 10.00000000000000178, 17.25893115100078745, 9.846743663894594434 ) ) ;
#91727 = CARTESIAN_POINT ( 'NONE',  ( 4.559911319644449179, 3.897018677488170990, 9.422509992056141925 ) ) ;
#91728 = ORIENTED_EDGE ( 'NONE', *, *, #6958, .T. ) ;
#91729 = CARTESIAN_POINT ( 'NONE',  ( 2.791683348922237240, 30.38393115100078390, -7.208316651077763204 ) ) ;
#91730 = CARTESIAN_POINT ( 'NONE',  ( 7.084665262690076126, 29.10535201082150181, 10.88017736071109987 ) ) ;
#91731 = CARTESIAN_POINT ( 'NONE',  ( 10.00000000000000178, 67.25893115100079456, 9.846743663894594434 ) ) ;
#91733 = CARTESIAN_POINT ( 'NONE',  ( 0.000000000000000000, 0.000000000000000000, 0.000000000000000000 ) ) ;
#91732 = CARTESIAN_POINT ( 'NONE',  ( 17.08211943468705130, 3.470415501580634388, 12.26659068614894998 ) ) ;
#91735 = DIRECTION ( 'NONE',  ( -0.000000000000000000, -1.000000000000000000, -0.000000000000000000 ) ) ;
#91734 = B_SPLINE_CURVE_WITH_KNOTS ( 'NONE', 3,
 ( #49638, #20139, #96653, #80651, #12145, #28628, #74113, #81132, #87645, #5647 ),
 .UNSPECIFIED., .F., .F.,
 ( 4, 3, 3, 4 ),
 ( 0.000000000000000000, 0.0006253016069560992946, 0.001250604074564904376, 0.002501455912506566921 ),
 .UNSPECIFIED. ) ;
#91736 = CARTESIAN_POINT ( 'NONE',  ( 0.1532563361054082862, 6.217264484334118713, 2.638427012816831674 ) ) ;
#91737 = CARTESIAN_POINT ( 'NONE',  ( 0.6178305044545818747, 38.49863466993042493, -9.382169495545419124 ) ) ;
#91738 = CARTESIAN_POINT ( 'NONE',  ( 0.1532563361054100626, 35.80059781766745175, -2.638427012816831230 ) ) ;
#91739 = EDGE_LOOP ( 'NONE', ( #45193, #24881, #8639, #91920, #79175, #55125 ) ) ;
#91740 = CARTESIAN_POINT ( 'NONE',  ( 18.52753015748617571, 18.09226448433411960, 4.923371831947298993 ) ) ;
#91741 = B_SPLINE_CURVE_WITH_KNOTS ( 'NONE', 3,
 ( #77897, #26370, #56869, #18391, #69920, #39911, #25895, #47889, #64360, #3387, #24920, #9912, #62391, #62896, #40414, #92899, #93889, #56394, #25417, #55901, #17901, #70414, #2918, #40901, #24430, #48384, #78886, #71402, #94376, #54894, #48870, #86881, #1934, #79382 ),
 .UNSPECIFIED., .F., .F.,
 ( 4, 2, 2, 2, 2, 2, 2, 2, 2, 2, 2, 2, 2, 2, 2, 2, 4 ),
 ( -5.999999999205076248E-08, 0.0003894208653645889824, 0.0007789017307291700191, 0.001557863461458290893, 0.003115786922916491657, 0.006231633845832851987, 0.01246332769166561168, 0.01869502153749837137, 0.02492671538333113279, 0.03739010307499662095, 0.04985349076666211604, 0.06231687845832762501, 0.07478026614999312705, 0.08724365384165863602, 0.09347534768749138356, 0.09659119461040775734, 0.09970704153332413111 ),
 .UNSPECIFIED. ) ;
#91742 = CARTESIAN_POINT ( 'NONE',  ( 11.33987066887527284, -87.82218667483482477, -3.750000000000000000 ) ) ;
#91743 = CARTESIAN_POINT ( 'NONE',  ( 6.204703633549690345, 50.76208216824730357, -14.16423886937410259 ) ) ;
#91744 = CARTESIAN_POINT ( 'NONE',  ( 7.084665262690076126, 49.10535201082149825, 10.88017736071109987 ) ) ;
#91745 = DIRECTION ( 'NONE',  ( -0.000000000000000000, 1.000000000000000000, -0.000000000000000000 ) ) ;
#91746 = CARTESIAN_POINT ( 'NONE',  ( 1.472469842513823179, 35.59226448433412315, -4.923371831947296329 ) ) ;
#91747 = CARTESIAN_POINT ( 'NONE',  ( 20.88017736071110164, 10.35535201082150714, 2.915334737309930979 ) ) ;
#91748 = CARTESIAN_POINT ( 'NONE',  ( 0.1532563361054082862, 41.21726448433411605, 2.638427012816831674 ) ) ;
#91749 = CARTESIAN_POINT ( 'NONE',  ( 5.815502996284858561, 0.2306972965111901419, 13.76292046016126491 ) ) ;
#91750 = CARTESIAN_POINT ( 'NONE',  ( 5.076628168052704559, 45.17559781766745175, -8.527530157486179263 ) ) ;
#91751 = CARTESIAN_POINT ( 'NONE',  ( 0.5774900079438590739, 52.64701867748817676, -5.440088680355550821 ) ) ;
#91752 = EDGE_LOOP ( 'NONE', ( #7227, #31528, #9444, #39583 ) ) ;
#91753 = ORIENTED_EDGE ( 'NONE', *, *, #75787, .T. ) ;
#91754 = CARTESIAN_POINT ( 'NONE',  ( -14.91886229468042835, 0.2301503527634116975, 0.8060919667643461350 ) ) ;
#91755 = DIRECTION ( 'NONE',  ( 0.000000000000000000, 1.000000000000000000, 0.000000000000000000 ) ) ;
#91756 = CARTESIAN_POINT ( 'NONE',  ( 12.63842701281683922, 9.550597817667449974, -9.846743663894590881 ) ) ;
#91757 = CARTESIAN_POINT ( 'NONE',  ( -2.816281873526473856, 54.12363466993041783, 9.499525473075851096E-16 ) ) ;
#91759 = CARTESIAN_POINT ( 'NONE',  ( 0.1532563361054083140, 46.00893115100079456, 1.131784320476157264E-15 ) ) ;
#91758 = CARTESIAN_POINT ( 'NONE',  ( 17.96484262340118221, 11.18868534415484106, -7.964842623401177768 ) ) ;
#91760 = CARTESIAN_POINT ( 'NONE',  ( 0.000000000000000000, 0.5000000000000004441, 0.000000000000000000 ) ) ;
#91761 = CARTESIAN_POINT ( 'NONE',  ( -4.164238869374098151, 31.59541550158063927, -3.795296366450310543 ) ) ;
#91762 = AXIS2_PLACEMENT_3D ( 'NONE', #94707, #94205, #71229 ) ;
#91763 = CARTESIAN_POINT ( 'NONE',  ( 20.36894250292379738, 54.92874883491396076, -10.36894250292379027 ) ) ;
#91764 = CARTESIAN_POINT ( 'NONE',  ( 0.1532563361054082862, 61.21726448433412315, 2.638427012816831674 ) ) ;
#91765 =( LENGTH_UNIT ( ) NAMED_UNIT ( * ) SI_UNIT ( .MILLI., .METRE. ) );
#91766 = CARTESIAN_POINT ( 'NONE',  ( 17.96484262340118221, 46.18868534415484106, -7.964842623401177768 ) ) ;
#91767 = VECTOR ( 'NONE', #53587, 1000.000000000000000 ) ;
#91768 = CARTESIAN_POINT ( 'NONE',  ( 14.92337183194729633, 2.675597817667451750, 8.527530157486181039 ) ) ;
#91769 = DIRECTION ( 'NONE',  ( 1.000000000000000000, 0.000000000000000000, 0.000000000000000000 ) ) ;
#91770 = ORIENTED_EDGE ( 'NONE', *, *, #7727, .F. ) ;
#91771 = CARTESIAN_POINT ( 'NONE',  ( 3.591859063236763294, 63.29030133659708923, -11.09922568453595026 ) ) ;
#91772 = EDGE_LOOP ( 'NONE', ( #88946, #88665, #61248, #33446, #91669, #42448, #59699, #98934, #9776, #63374, #36925, #9549, #84310, #66274, #77542, #32369, #98091, #36504, #37193, #67338, #30880, #33524, #13891, #2194, #70074, #47537, #84290, #21612, #91282, #41911, #45811, #13504, #31171, #84583, #97615, #43525, #33954, #34044, #28701, #89530, #23086, #92506, #78955, #74181, #56848, #72185, #98799, #4121, #21309, #79136, #46277, #9902, #44404, #27435, #27485, #83922, #39016, #19704, #92863, #53494, #54746, #26716, #49994, #84145, #24051, #56047, #10868, #28089, #64179, #87221, #80401, #53784, #46273, #86917, #76055, #59739, #33982, #37586, #13880, #65766, #86786, #92637, #93117, #36301, #13309, #82474, #94896, #35955, #78648, #60172, #37564, #13063, #46136, #36238, #4361, #71741, #80277, #56021, #15756, #93233, #89181, #54234, #53133, #73321, #39837, #35987, #83240, #52185, #93243, #61944, #57089 ) ) ;
#91773 = CARTESIAN_POINT ( 'NONE',  ( 5.076628168052703671, 6.842264484334118713, 8.527530157486179263 ) ) ;
#91774 = ORIENTED_EDGE ( 'NONE', *, *, #24306, .F. ) ;
#91775 = CARTESIAN_POINT ( 'NONE',  ( -4.164238869374098151, 16.59541550158063927, -3.795296366450310543 ) ) ;
#91776 = CARTESIAN_POINT ( 'NONE',  ( 10.00000000000000000, 24.75893115100078745, -9.846743663894594434 ) ) ;
#91777 = CARTESIAN_POINT ( 'NONE',  ( 7.084665262690076126, 37.02201867748817676, -10.88017736071110164 ) ) ;
#91778 = ADVANCED_FACE ( 'NONE', ( #32976 ), #93984, .T. ) ;
#91779 = CARTESIAN_POINT ( 'NONE',  ( 17.75000000000000000, 73.00000000000001421, 6.500000000000000888 ) ) ;
#91780 = ORIENTED_EDGE ( 'NONE', *, *, #21393, .F. ) ;
#91781 = CARTESIAN_POINT ( 'NONE',  ( 19.42250999205614548, 30.98035201082150536, -5.440088680355545492 ) ) ;
#91782 = AXIS2_PLACEMENT_3D ( 'NONE', #81869, #58878, #72890 ) ;
#91783 = ORIENTED_EDGE ( 'NONE', *, *, #92151, .F. ) ;
#91784 = CARTESIAN_POINT ( 'NONE',  ( 20.88017736071110519, 30.56368534415484106, 2.639326808657452039E-16 ) ) ;
#91785 = CARTESIAN_POINT ( 'NONE',  ( 2.791683348922240793, 66.63393115100079456, 7.208316651077764092 ) ) ;
#91786 = ORIENTED_EDGE ( 'NONE', *, *, #55130, .F. ) ;
#91787 = PRESENTATION_STYLE_ASSIGNMENT (( #61278 ) ) ;
#91788 = ORIENTED_EDGE ( 'NONE', *, *, #82949, .F. ) ;
#91789 = CARTESIAN_POINT ( 'NONE',  ( 22.81628187352647785, 11.41530133659708390, 3.434112377981063169 ) ) ;
#91790 = CARTESIAN_POINT ( 'NONE',  ( 17.20831665107776587, 4.133931151000785675, -7.208316651077762316 ) ) ;
#91791 = CARTESIAN_POINT ( 'NONE',  ( 3.927832320392247389, -0.03417435944610275333, -13.69797916712104602 ) ) ;
#91792 = CARTESIAN_POINT ( 'NONE',  ( 0.2751277870543045734, 27.28217586085238011, -6.500000000000012434 ) ) ;
#91793 = CARTESIAN_POINT ( 'NONE',  ( 12.63842701281683034, 22.46726448433411605, 9.846743663894596210 ) ) ;
#91794 = CARTESIAN_POINT ( 'NONE',  ( 19.42250999205614548, 30.98035201082150536, -5.440088680355545492 ) ) ;
#91795 = EDGE_LOOP ( 'NONE', ( #89367, #66591, #22181 ) ) ;
#91796 = VERTEX_POINT ( 'NONE', #92991 ) ;
#91797 = EDGE_CURVE ( 'NONE', #15375, #3422, #45151, .T. ) ;
#91798 = CARTESIAN_POINT ( 'NONE',  ( 21.09922568453594849, 61.20696800326376064, 6.408140936763242479 ) ) ;
#91799 = CARTESIAN_POINT ( 'NONE',  ( 15.44008868035555793, 61.39701867748817676, -9.422509992056140149 ) ) ;
#91800 = DIRECTION ( 'NONE',  ( 1.257568779154408793E-17, 1.000000000000000000, -0.000000000000000000 ) ) ;
#91801 = CARTESIAN_POINT ( 'NONE',  ( 10.00000000000000000, 57.87363466993042493, -12.81628187352647608 ) ) ;
#91802 = CARTESIAN_POINT ( 'NONE',  ( -0.8801773607111009756, 63.06368534415484106, 1.068504757029289695E-15 ) ) ;
#91803 = CARTESIAN_POINT ( 'NONE',  ( 2.791683348922240793, 66.63393115100079456, 7.208316651077764092 ) ) ;
#91804 = FACE_OUTER_BOUND ( 'NONE', #54400, .T. ) ;
#91805 = CARTESIAN_POINT ( 'NONE',  ( 0.1532563361054083140, 31.00893115100078390, 1.131784320476157264E-15 ) ) ;
#91806 = CARTESIAN_POINT ( 'NONE',  ( 3.591859063236763294, 48.29030133659708923, -11.09922568453595026 ) ) ;
#91807 = CARTESIAN_POINT ( 'NONE',  ( 0.000000000000000000, 78.33947701945625397, 8.949703107968367988 ) ) ;
#91808 = CARTESIAN_POINT ( 'NONE',  ( 17.20831665107776587, 17.88393115100078745, 7.208316651077764980 ) ) ;
#91810 = VECTOR ( 'NONE', #1486, 1000.000000000000000 ) ;
#91809 = CARTESIAN_POINT ( 'NONE',  ( 3.591859063236761518, 14.95696800326375531, 11.09922568453594849 ) ) ;
#91812 = CARTESIAN_POINT ( 'NONE',  ( -8.900000000000002132, 75.76920769491746910, 3.000000000000000000 ) ) ;
#91811 = LINE ( 'NONE', #83817, #81909 ) ;
#91813 = CARTESIAN_POINT ( 'NONE',  ( 4.559911319644449179, 32.23035201082150536, -9.422509992056141925 ) ) ;
#91814 = CARTESIAN_POINT ( 'NONE',  ( 3.591859063236761518, -0.04303199673624671928, 11.09922568453594849 ) ) ;
#91815 = PRESENTATION_STYLE_ASSIGNMENT (( #15827 ) ) ;
#91816 = CARTESIAN_POINT ( 'NONE',  ( 19.84674366389459266, 23.30059781766745530, 2.638427012816836559 ) ) ;
#91817 = CARTESIAN_POINT ( 'NONE',  ( 14.92337183194729633, 2.675597817667451750, 8.527530157486181039 ) ) ;
#91818 = CARTESIAN_POINT ( 'NONE',  ( 0.5774900079438607392, 8.480352010821505360, 5.440088680355550821 ) ) ;
#91819 = CARTESIAN_POINT ( 'NONE',  ( -2.816281873526471635, 18.91530133659708213, -3.434112377981056508 ) ) ;
#91820 = CARTESIAN_POINT ( 'NONE',  ( 2.035157376598822676, 2.438685344154837953, -7.964842623401177768 ) ) ;
#91821 =( NAMED_UNIT ( * ) PLANE_ANGLE_UNIT ( ) SI_UNIT ( $, .RADIAN. ) );
#91822 = CARTESIAN_POINT ( 'NONE',  ( 7.361572987183170547, 62.05059781766745886, 9.846743663894590881 ) ) ;
#91823 = B_SPLINE_CURVE_WITH_KNOTS ( 'NONE', 3,
 ( #27547, #90511, #88549, #73536, #67037, #6049 ),
 .UNSPECIFIED., .F., .F.,
 ( 4, 2, 4 ),
 ( 3.409110551496111717E-05, 0.0004400426677367851622, 0.0008459942299586092071 ),
 .UNSPECIFIED. ) ;
#91824 = CARTESIAN_POINT ( 'NONE',  ( 22.26659068614895176, 19.72041550158063572, -7.082119434687042414 ) ) ;
#91825 = CARTESIAN_POINT ( 'NONE',  ( -0.3689425029237881626, 67.42874883491396076, 10.36894250292379027 ) ) ;
#91826 = CARTESIAN_POINT ( 'NONE',  ( 14.92337183194729988, 39.34226448433412315, -8.527530157486177487 ) ) ;
#91827 = VERTEX_POINT ( 'NONE', #55501 ) ;
#91828 = CARTESIAN_POINT ( 'NONE',  ( -1.926860441876562025, 49.47997603579417358, -3.195792623639529761 ) ) ;
#91829 = CARTESIAN_POINT ( 'NONE',  ( 15.44008868035555260, 19.73035201082150536, 9.422509992056143702 ) ) ;
#91830 = CARTESIAN_POINT ( 'NONE',  ( -0.8801773607110990882, 12.85535201082150358, -2.915334737309924318 ) ) ;
#91831 = CARTESIAN_POINT ( 'NONE',  ( 4.559911319644449179, 28.89701867748817321, 9.422509992056141925 ) ) ;
#91833 = DIRECTION ( 'NONE',  ( 0.000000000000000000, -1.000000000000000000, 0.000000000000000000 ) ) ;
#91832 = CARTESIAN_POINT ( 'NONE',  ( -4.164238869374098151, 66.59541550158060375, -3.795296366450310543 ) ) ;
#91834 = SURFACE_STYLE_USAGE ( .BOTH. , #76818 ) ;
#91835 = EDGE_CURVE ( 'NONE', #30837, #67657, #41630, .T. ) ;
#91836 = CARTESIAN_POINT ( 'NONE',  ( 7.361572987183169658, 24.96726448433412315, -9.846743663894592657 ) ) ;
#91837 = CARTESIAN_POINT ( 'NONE',  ( 22.81628187352647785, 11.62363466993042138, 6.195893100308588602E-16 ) ) ;
#91838 = CARTESIAN_POINT ( 'NONE',  ( -46.44011323352863485, 103.5176347749360133, 6.245517546461054614 ) ) ;
#91839 = DIRECTION ( 'NONE',  ( -0.000000000000000000, 1.000000000000000000, -0.000000000000000000 ) ) ;
#91840 = EDGE_CURVE ( 'NONE', #74794, #65046, #37186, .T. ) ;
#91841 = CARTESIAN_POINT ( 'NONE',  ( 10.00000000000000000, 64.75893115100078035, -9.846743663894594434 ) ) ;
#91842 = FACE_OUTER_BOUND ( 'NONE', #72512, .T. ) ;
#91843 = CARTESIAN_POINT ( 'NONE',  ( 13.79529636645030344, 13.26208216824729824, 14.16423886937410614 ) ) ;
#91844 = CARTESIAN_POINT ( 'NONE',  ( 19.84674366389459266, 43.30059781766744464, 2.638427012816836559 ) ) ;
#91845 = PLANE ( 'NONE',  #78378 ) ;
#91846 = VERTEX_POINT ( 'NONE', #32489 ) ;
#91847 = CIRCLE ( 'NONE', #75924, 1.499999999999996669 ) ;
#91848 = CARTESIAN_POINT ( 'NONE',  ( 24.16423886937410614, 54.30374883491396787, 8.672049930838204340E-16 ) ) ;
#91849 = CARTESIAN_POINT ( 'NONE',  ( 17.20831665107776587, 4.133931151000785675, -7.208316651077762316 ) ) ;
#91851 = DIRECTION ( 'NONE',  ( 0.000000000000000000, 0.000000000000000000, 1.000000000000000000 ) ) ;
#91850 = CARTESIAN_POINT ( 'NONE',  ( -4.000000000000000000, 10.00000000000000000, -2.750000000000000000 ) ) ;
#91852 = CARTESIAN_POINT ( 'NONE',  ( 17.96484262340118221, 44.93868534415483396, 7.964842623401181321 ) ) ;
#91853 = CARTESIAN_POINT ( 'NONE',  ( -1.099225684535947600, 48.70696800326375353, -6.408140936763238038 ) ) ;
#91854 = CARTESIAN_POINT ( 'NONE',  ( 0.5774900079438607392, 18.48035201082150536, 5.440088680355550821 ) ) ;
#91855 = CARTESIAN_POINT ( 'NONE',  ( 13.43411237798106583, 42.66530133659707502, -12.81628187352647252 ) ) ;
#91856 = CARTESIAN_POINT ( 'NONE',  ( 16.40814093676323893, 0.7903013365970867898, 11.09922568453595026 ) ) ;
#91857 = EDGE_LOOP ( 'NONE', ( #59554, #21892, #17937, #76157 ) ) ;
#91858 = CARTESIAN_POINT ( 'NONE',  ( -10.84451454130491399, 15.00000000000000000, -9.625305416630974165 ) ) ;
#91859 = CARTESIAN_POINT ( 'NONE',  ( -0.3689425029237881626, 37.42874883491396787, 10.36894250292379027 ) ) ;
#91860 = CARTESIAN_POINT ( 'NONE',  ( 17.08211943468705840, 10.13708216824730179, -12.26659068614894466 ) ) ;
#91861 = CARTESIAN_POINT ( 'NONE',  ( -0.8801773607110991993, 22.85535201082150181, -2.915334737309923874 ) ) ;
#91862 = CARTESIAN_POINT ( 'NONE',  ( 4.559911319644449179, 32.23035201082150536, -9.422509992056141925 ) ) ;
#91863 = CARTESIAN_POINT ( 'NONE',  ( -14.93928340878672145, 14.76930270348881180, -0.2363597353051685723 ) ) ;
#91864 = CARTESIAN_POINT ( 'NONE',  ( 8.209432707284861408, 0.5000000000000004441, -12.55409154915486170 ) ) ;
#91865 = CARTESIAN_POINT ( 'NONE',  ( 15.44008868035555793, 66.39701867748817676, -9.422509992056140149 ) ) ;
#91866 = CARTESIAN_POINT ( 'NONE',  ( 15.44008868035555260, 59.73035201082151247, 9.422509992056143702 ) ) ;
#91867 = CARTESIAN_POINT ( 'NONE',  ( 13.43411237798106583, 22.66530133659708923, -12.81628187352647252 ) ) ;
#91868 = CARTESIAN_POINT ( 'NONE',  ( 5.376821459231094558, 14.76984886575368705, -13.93958558162744055 ) ) ;
#91869 = CARTESIAN_POINT ( 'NONE',  ( -5.925933864965021947, 1.825967504928687424, -10.35061266127159563 ) ) ;
#91870 = CARTESIAN_POINT ( 'NONE',  ( 2.791683348922237240, 40.38393115100078035, -7.208316651077763204 ) ) ;
#91871 =( GEOMETRIC_REPRESENTATION_CONTEXT ( 3 ) GLOBAL_UNCERTAINTY_ASSIGNED_CONTEXT ( ( #82264 ) ) GLOBAL_UNIT_ASSIGNED_CONTEXT ( ( #67571, #59559, #98590 ) ) REPRESENTATION_CONTEXT ( 'NONE', 'WORKASPACE' ) );
#91872 = CARTESIAN_POINT ( 'NONE',  ( -0.8801773607111009756, 8.063685344154837509, 1.068504757029289695E-15 ) ) ;
#91873 = CARTESIAN_POINT ( 'NONE',  ( -1.099225684535947600, 19.54030133659708568, 6.408140936763237150 ) ) ;
#91874 = VECTOR ( 'NONE', #35141, 1000.000000000000000 ) ;
#91875 = CARTESIAN_POINT ( 'NONE',  ( 12.63842701281683034, 12.46726448433411782, 9.846743663894596210 ) ) ;
#91876 = CARTESIAN_POINT ( 'NONE',  ( 0.5774900079438607392, 3.480352010821504027, 5.440088680355550821 ) ) ;
#91877 = CARTESIAN_POINT ( 'NONE',  ( 14.92337183194729988, 34.34226448433411605, -8.527530157486177487 ) ) ;
#91878 = CARTESIAN_POINT ( 'NONE',  ( -2.816281873526473856, 64.33196800326376774, 3.434112377981055619 ) ) ;
#91879 = CARTESIAN_POINT ( 'NONE',  ( 19.84674366389459621, 28.50893115100078745, 7.409399052514197653E-17 ) ) ;
#91880 = CARTESIAN_POINT ( 'NONE',  ( 13.79529636645031943, 20.34541550158063572, -14.16423886937409904 ) ) ;
#91881 = CARTESIAN_POINT ( 'NONE',  ( 20.88017736071110164, 35.35535201082150536, 2.915334737309930979 ) ) ;
#91882 = CARTESIAN_POINT ( 'NONE',  ( 10.00000000000000000, 11.81368534415483751, -10.88017736071110342 ) ) ;
#91883 = CARTESIAN_POINT ( 'NONE',  ( 7.084665262690076126, 27.02201867748817676, -10.88017736071110164 ) ) ;
#91884 = CARTESIAN_POINT ( 'NONE',  ( 10.00000000000000000, 31.81368534415483751, -10.88017736071110342 ) ) ;
#91885 = ORIENTED_EDGE ( 'NONE', *, *, #75170, .F. ) ;
#91886 = CARTESIAN_POINT ( 'NONE',  ( 15.44008868035555793, 46.39701867748817676, -9.422509992056140149 ) ) ;
#91887 = CARTESIAN_POINT ( 'NONE',  ( 16.40814093676324603, 62.45696800326376064, -11.09922568453594671 ) ) ;
#91888 = ADVANCED_FACE ( 'NONE', ( #40504 ), #16371, .T. ) ;
#91889 = CARTESIAN_POINT ( 'NONE',  ( 20.88017736071110164, 45.35535201082149115, 2.915334737309930979 ) ) ;
#91890 = CARTESIAN_POINT ( 'NONE',  ( 2.035157376598824452, 48.68868534415483396, 7.964842623401179544 ) ) ;
#91891 = AXIS2_PLACEMENT_3D ( 'NONE', #25499, #61991, #2516 ) ;
#91892 = ORIENTED_EDGE ( 'NONE', *, *, #87170, .F. ) ;
#91893 = CARTESIAN_POINT ( 'NONE',  ( 10.00000000000000000, 51.81368534415484106, -10.88017736071110342 ) ) ;
#91894 = PRESENTATION_STYLE_ASSIGNMENT (( #30391 ) ) ;
#91895 = CARTESIAN_POINT ( 'NONE',  ( 6.204703633549690345, 62.84541550158063927, 14.16423886937410082 ) ) ;
#91896 = CARTESIAN_POINT ( 'NONE',  ( 5.076628168052704559, 0.1755978176674514724, -8.527530157486179263 ) ) ;
#91897 = DIRECTION ( 'NONE',  ( 0.000000000000000000, 0.000000000000000000, 1.000000000000000000 ) ) ;
#91898 = CARTESIAN_POINT ( 'NONE',  ( -14.62617646268093807, 14.63606916781938594, 3.327906561566777999 ) ) ;
#91899 =( NAMED_UNIT ( * ) SI_UNIT ( $, .STERADIAN. ) SOLID_ANGLE_UNIT ( ) );
#91900 = CARTESIAN_POINT ( 'NONE',  ( 10.00000000000000000, 29.75893115100078745, -9.846743663894594434 ) ) ;
#91901 = VERTEX_POINT ( 'NONE', #14447 ) ;
#91902 = CARTESIAN_POINT ( 'NONE',  ( 0.1532563361054082862, 31.21726448433412315, 2.638427012816831674 ) ) ;
#91903 = CARTESIAN_POINT ( 'NONE',  ( 7.084665262690076126, 44.10535201082151247, 10.88017736071109987 ) ) ;
#91904 = CARTESIAN_POINT ( 'NONE',  ( 12.63842701281683922, 34.55059781766745886, -9.846743663894590881 ) ) ;
#91905 = CARTESIAN_POINT ( 'NONE',  ( 13.43411237798105340, 15.58196800326374998, 12.81628187352647963 ) ) ;
#91907 = CARTESIAN_POINT ( 'NONE',  ( 15.44008868035555260, 59.73035201082151247, 9.422509992056143702 ) ) ;
#91906 = CARTESIAN_POINT ( 'NONE',  ( 0.5774900079438590739, 67.64701867748817676, -5.440088680355550821 ) ) ;
#91909 =( NAMED_UNIT ( * ) SI_UNIT ( $, .STERADIAN. ) SOLID_ANGLE_UNIT ( ) );
#91908 = CARTESIAN_POINT ( 'NONE',  ( -0.8801773607111009756, 48.06368534415484817, 1.068504757029289695E-15 ) ) ;
#91910 = CARTESIAN_POINT ( 'NONE',  ( 6.204703633549690345, 62.84541550158063927, 14.16423886937410082 ) ) ;
#91911 = CIRCLE ( 'NONE', #68012, 14.49999999999999822 ) ;
#91912 = EDGE_CURVE ( 'NONE', #12953, #54148, #76413, .T. ) ;
#91913 = CARTESIAN_POINT ( 'NONE',  ( 19.38216949554541557, 22.24863466993041428, -9.382169495545420901 ) ) ;
#91914 = DIRECTION ( 'NONE',  ( 0.000000000000000000, 0.000000000000000000, -1.000000000000000000 ) ) ;
#91915 = ORIENTED_EDGE ( 'NONE', *, *, #79370, .F. ) ;
#91916 = CARTESIAN_POINT ( 'NONE',  ( 3.591859063236763294, 13.29030133659708746, -11.09922568453595026 ) ) ;
#91917 = CARTESIAN_POINT ( 'NONE',  ( 17.96484262340118221, 16.18868534415483396, -7.964842623401177768 ) ) ;
#91918 = CARTESIAN_POINT ( 'NONE',  ( 19.42250999205614548, 60.98035201082151247, -5.440088680355545492 ) ) ;
#91919 = EDGE_CURVE ( 'NONE', #39149, #47405, #89822, .T. ) ;
#91920 = ORIENTED_EDGE ( 'NONE', *, *, #2392, .T. ) ;
#91921 = CARTESIAN_POINT ( 'NONE',  ( 10.00000000000000000, 4.758931151000784787, -9.846743663894594434 ) ) ;
#91922 = CARTESIAN_POINT ( 'NONE',  ( 14.92337183194729633, 47.67559781766745175, 8.527530157486181039 ) ) ;
#91923 = CARTESIAN_POINT ( 'NONE',  ( 18.52753015748617571, 38.09226448433412315, 4.923371831947298993 ) ) ;
#91924 = PLANE ( 'NONE',  #71469 ) ;
#91925 = CARTESIAN_POINT ( 'NONE',  ( 2.791683348922240793, 26.63393115100078745, 7.208316651077764092 ) ) ;
#91926 = DIRECTION ( 'NONE',  ( -0.000000000000000000, 0.000000000000000000, 1.000000000000000000 ) ) ;
#91928 = CARTESIAN_POINT ( 'NONE',  ( 3.591859063236763294, 43.29030133659708923, -11.09922568453595026 ) ) ;
#91927 = FACE_OUTER_BOUND ( 'NONE', #52743, .T. ) ;
#91930 = CARTESIAN_POINT ( 'NONE',  ( 67.06412365047464164, 22.49999999999998934, -9.500000000000000000 ) ) ;
#91929 = CARTESIAN_POINT ( 'NONE',  ( 1.472469842513823179, 20.59226448433411960, -4.923371831947296329 ) ) ;
#91931 = DIRECTION ( 'NONE',  ( -0.9723699203976773342, 0.000000000000000000, 0.2334453638559024768 ) ) ;
#91933 = ORIENTED_EDGE ( 'NONE', *, *, #10881, .F. ) ;
#91932 = CARTESIAN_POINT ( 'NONE',  ( 19.84674366389459266, 43.71726448433410894, -2.638427012816827677 ) ) ;
#91934 = LINE ( 'NONE', #23462, #74098 ) ;
#91935 = CARTESIAN_POINT ( 'NONE',  ( 21.09922568453594849, 16.20696800326375353, 6.408140936763242479 ) ) ;
#91936 = CARTESIAN_POINT ( 'NONE',  ( 2.035157376598824452, 53.68868534415484817, 7.964842623401179544 ) ) ;
#91937 = CARTESIAN_POINT ( 'NONE',  ( 10.00000000000000178, 28.05374883491396787, 14.16423886937410082 ) ) ;
#91938 = CARTESIAN_POINT ( 'NONE',  ( 20.00000000000000711, 92.20777562798905080, 4.885465336749220455 ) ) ;
#91939 = CARTESIAN_POINT ( 'NONE',  ( 24.16423886937410614, 29.30374883491396787, 8.672049930838204340E-16 ) ) ;
#91940 = CARTESIAN_POINT ( 'NONE',  ( 20.36894250292379738, 59.92874883491397497, -10.36894250292379027 ) ) ;
#91941 = CARTESIAN_POINT ( 'NONE',  ( 13.79529636645031943, 15.34541550158063750, -14.16423886937409904 ) ) ;
#91943 = DIRECTION ( 'NONE',  ( -1.000000000000000000, 0.000000000000000000, 0.000000000000000000 ) ) ;
#91942 = CARTESIAN_POINT ( 'NONE',  ( 10.00000000000000000, 25.55374883491396787, -14.16423886937410082 ) ) ;
#91944 = CARTESIAN_POINT ( 'NONE',  ( 4.903136312256997087, -13.39483660680936339, -2.750000000000000000 ) ) ;
#91946 = CARTESIAN_POINT ( 'NONE',  ( 14.92337183194729988, 44.34226448433412315, -8.527530157486177487 ) ) ;
#91945 = CARTESIAN_POINT ( 'NONE',  ( 6.033511671525834785, -36.04540650298945792, 2.500000000003218315 ) ) ;
#91947 = EDGE_LOOP ( 'NONE', ( #92276, #23579, #21823, #93371 ) ) ;
#91948 = CARTESIAN_POINT ( 'NONE',  ( 20.88017736071110164, 25.35535201082150891, 2.915334737309930979 ) ) ;
#91949 = DIRECTION ( 'NONE',  ( 0.000000000000000000, 0.000000000000000000, 1.000000000000000000 ) ) ;
#91950 = CARTESIAN_POINT ( 'NONE',  ( 18.52753015748618282, 58.92559781766745886, -4.923371831947291888 ) ) ;
#91951 = CARTESIAN_POINT ( 'NONE',  ( -9.641087339108761256, 14.95077488074853456, -11.16671550067062135 ) ) ;
#91952 = EDGE_CURVE ( 'NONE', #90628, #49115, #59488, .T. ) ;
#91953 = CARTESIAN_POINT ( 'NONE',  ( 12.63842701281683922, 44.55059781766745175, -9.846743663894590881 ) ) ;
#91954 = CARTESIAN_POINT ( 'NONE',  ( 22.81628187352648496, 56.83196800326374643, -3.434112377981050290 ) ) ;
#91956 = VECTOR ( 'NONE', #93410, 1000.000000000000114 ) ;
#91955 = CARTESIAN_POINT ( 'NONE',  ( 10.36894250292379027, -6.321251165086028578, 10.36894250292378672 ) ) ;
#91957 = CARTESIAN_POINT ( 'NONE',  ( 19.84674366389459266, 43.30059781766744464, 2.638427012816836559 ) ) ;
#91958 = CARTESIAN_POINT ( 'NONE',  ( 2.791683348922237240, 55.38393115100078745, -7.208316651077763204 ) ) ;
#91959 = TOROIDAL_SURFACE ( 'NONE', #5746, 14.49999999999999822, 0.5000000000000000000 ) ;
#91960 = CARTESIAN_POINT ( 'NONE',  ( 20.36894250292379738, 39.92874883491396787, -10.36894250292379027 ) ) ;
#91961 = EDGE_LOOP ( 'NONE', ( #31885, #77648 ) ) ;
#91962 = CARTESIAN_POINT ( 'NONE',  ( 24.16423886937410614, 14.30374883491396787, 8.672049930838204340E-16 ) ) ;
#91963 = AXIS2_PLACEMENT_3D ( 'NONE', #12916, #67905, #66908 ) ;
#91964 = CARTESIAN_POINT ( 'NONE',  ( 15.44008868035555260, 59.73035201082151247, 9.422509992056143702 ) ) ;
#91965 = CARTESIAN_POINT ( 'NONE',  ( -2.266590686148945544, 56.38708216824731068, -7.082119434687050408 ) ) ;
#91966 = CARTESIAN_POINT ( 'NONE',  ( 13.43411237798106583, 17.66530133659708923, -12.81628187352647252 ) ) ;
#91967 = CARTESIAN_POINT ( 'NONE',  ( 0.2751277870542911397, 55.30223176428831522, 6.499999999999992006 ) ) ;
#91968 = CARTESIAN_POINT ( 'NONE',  ( 17.96484262340118221, 64.93868534415483396, 7.964842623401181321 ) ) ;
#91969 = CYLINDRICAL_SURFACE ( 'NONE', #21461, 0.5000000000000004441 ) ;
#91970 = DIRECTION ( 'NONE',  ( 0.9999509640662961329, 0.009903002720634834083, 0.000000000000000000 ) ) ;
#91971 = CARTESIAN_POINT ( 'NONE',  ( 24.16423886937410614, 64.51208216824728936, -3.795296366450302550 ) ) ;
#91972 = CARTESIAN_POINT ( 'NONE',  ( -14.94699059465099822, 0.5000000000000004441, -1.259949270175015013 ) ) ;
#91973 = CARTESIAN_POINT ( 'NONE',  ( -0.8801773607110991993, 27.85535201082150181, -2.915334737309923874 ) ) ;
#91974 = CARTESIAN_POINT ( 'NONE',  ( -0.8801773607111008646, 23.27201867748817676, 2.915334737309923430 ) ) ;
#91975 = CARTESIAN_POINT ( 'NONE',  ( 7.361572987183170547, 57.05059781766744464, 9.846743663894590881 ) ) ;
#91976 = CARTESIAN_POINT ( 'NONE',  ( 18.52753015748617571, 48.09226448433412315, 4.923371831947298993 ) ) ;
#91977 = CARTESIAN_POINT ( 'NONE',  ( 22.81628187352647785, 46.41530133659708213, 3.434112377981063169 ) ) ;
#91978 = DIRECTION ( 'NONE',  ( -0.000000000000000000, -1.000000000000000000, -0.000000000000000000 ) ) ;
#91979 = ORIENTED_EDGE ( 'NONE', *, *, #87612, .T. ) ;
#91980 = CARTESIAN_POINT ( 'NONE',  ( 10.00000000000000000, 21.81368534415484106, -10.88017736071110342 ) ) ;
#91981 = CARTESIAN_POINT ( 'NONE',  ( -1.099225684535947600, 19.54030133659708568, 6.408140936763237150 ) ) ;
#91982 = DIRECTION ( 'NONE',  ( -1.000000000000000000, 0.000000000000000000, 0.000000000000000000 ) ) ;
#91983 = CARTESIAN_POINT ( 'NONE',  ( 5.076628168052703671, 51.84226448433412315, 8.527530157486179263 ) ) ;
#91984 = CARTESIAN_POINT ( 'NONE',  ( 7.084665262690076126, 44.10535201082151247, 10.88017736071109987 ) ) ;
#91985 = CARTESIAN_POINT ( 'NONE',  ( 16.40814093676323893, 20.79030133659708923, 11.09922568453595026 ) ) ;
#91987 = CARTESIAN_POINT ( 'NONE',  ( 19.72487221294571569, 55.71833443783938833, -6.499999999999990230 ) ) ;
#91986 = CARTESIAN_POINT ( 'NONE',  ( 10.00000000000000178, 54.31368534415484106, 10.88017736071110342 ) ) ;
#91988 = EDGE_CURVE ( 'NONE', #39787, #64978, #98457, .T. ) ;
#91989 = SURFACE_STYLE_FILL_AREA ( #39979 ) ;
#91990 = ORIENTED_EDGE ( 'NONE', *, *, #37217, .F. ) ;
#91991 = CARTESIAN_POINT ( 'NONE',  ( 2.791683348922237240, 60.38393115100078745, -7.208316651077763204 ) ) ;
#91992 = CARTESIAN_POINT ( 'NONE',  ( 2.035157376598824452, 43.68868534415484106, 7.964842623401179544 ) ) ;
#91994 = CARTESIAN_POINT ( 'NONE',  ( 6.204703633549690345, 10.76208216824729824, -14.16423886937410259 ) ) ;
#91993 = CARTESIAN_POINT ( 'NONE',  ( -1.099225684535947600, 43.70696800326375353, -6.408140936763238038 ) ) ;
#91995 = CARTESIAN_POINT ( 'NONE',  ( 19.84674366389459266, 8.717264484334116048, -2.638427012816827677 ) ) ;
#91996 = CARTESIAN_POINT ( 'NONE',  ( 1.472469842513823179, 66.42559781766745175, 4.923371831947296329 ) ) ;
#91997 = CARTESIAN_POINT ( 'NONE',  ( 2.791683348922237240, 0.3839311510007847872, -7.208316651077763204 ) ) ;
#91998 = CARTESIAN_POINT ( 'NONE',  ( 0.000000000000000000, 0.5000000000000004441, 0.000000000000000000 ) ) ;
#91999 = CARTESIAN_POINT ( 'NONE',  ( -4.164238869374099039, 36.80374883491396787, 8.674139862899312516E-16 ) ) ;
#92000 = CARTESIAN_POINT ( 'NONE',  ( 12.91533473730993009, 6.605352010821504471, -10.88017736071109987 ) ) ;
#92001 = AXIS2_PLACEMENT_3D ( 'NONE', #48156, #78669, #2697 ) ;
#92002 = EDGE_CURVE ( 'NONE', #67942, #92547, #60418, .T. ) ;
#92003 = CARTESIAN_POINT ( 'NONE',  ( -0.8801773607111009756, 3.063685344154837509, 1.068504757029289695E-15 ) ) ;
#92004 = CARTESIAN_POINT ( 'NONE',  ( 0.000000000000000000, 0.000000000000000000, 0.000000000000000000 ) ) ;
#92005 = ORIENTED_EDGE ( 'NONE', *, *, #79097, .T. ) ;
#92006 = ORIENTED_EDGE ( 'NONE', *, *, #31026, .T. ) ;
#92007 = CARTESIAN_POINT ( 'NONE',  ( 4.559911319644449179, 7.230352010821505360, -9.422509992056141925 ) ) ;
#92008 = CARTESIAN_POINT ( 'NONE',  ( 12.91533473730993009, 11.60535201082150714, -10.88017736071109987 ) ) ;
#92009 = CARTESIAN_POINT ( 'NONE',  ( 5.076628168052704559, 45.17559781766745175, -8.527530157486179263 ) ) ;
#92010 = CARTESIAN_POINT ( 'NONE',  ( -2.816281873526473856, 39.33196800326374643, 3.434112377981055619 ) ) ;
#92011 = CARTESIAN_POINT ( 'NONE',  ( 20.15039907845753220, 64.72266099184918176, 6.262539305110077947 ) ) ;
#92013 = CARTESIAN_POINT ( 'NONE',  ( 10.00000000000000178, 13.05374883491396787, 14.16423886937410082 ) ) ;
#92012 = CARTESIAN_POINT ( 'NONE',  ( -8.665245649997663335, 87.00799529562949886, -4.320095926139194020 ) ) ;
#92014 = CARTESIAN_POINT ( 'NONE',  ( 2.035157376598822676, 22.43868534415483396, -7.964842623401177768 ) ) ;
#92015 = CARTESIAN_POINT ( 'NONE',  ( 10.00000000000000178, 4.313685344154837509, 10.88017736071110342 ) ) ;
#92016 = ADVANCED_FACE ( 'NONE', ( #22939 ), #68430, .F. ) ;
#92017 = CARTESIAN_POINT ( 'NONE',  ( 10.00000000000000000, 39.75893115100078745, -9.846743663894594434 ) ) ;
#92018 = TOROIDAL_SURFACE ( 'NONE', #98469, 3.690000000000000391, 0.2500000000000000000 ) ;
#92019 = PRESENTATION_STYLE_ASSIGNMENT (( #61510 ) ) ;
#92020 = CARTESIAN_POINT ( 'NONE',  ( 12.63842701281683034, 22.46726448433411605, 9.846743663894596210 ) ) ;
#92021 = CARTESIAN_POINT ( 'NONE',  ( -7.208316651077764980, 25.38393115100079100, -7.208316651077759651 ) ) ;
#92022 = VERTEX_POINT ( 'NONE', #15444 ) ;
#92023 = DIRECTION ( 'NONE',  ( -1.000000000000000000, 0.000000000000000000, -0.000000000000000000 ) ) ;
#92024 = B_SPLINE_CURVE_WITH_KNOTS ( 'NONE', 3,
 ( #78153, #47659, #33131, #94132, #18639, #9664 ),
 .UNSPECIFIED., .F., .F.,
 ( 4, 2, 4 ),
 ( 3.409110551494545045E-05, 0.0004400426677367704170, 0.0008459942299585954378 ),
 .UNSPECIFIED. ) ;
#92025 = ORIENTED_EDGE ( 'NONE', *, *, #31633, .T. ) ;
#92026 = CARTESIAN_POINT ( 'NONE',  ( 0.1532563361054082862, 61.21726448433412315, 2.638427012816831674 ) ) ;
#92028 = CARTESIAN_POINT ( 'NONE',  ( 15.44008868035555793, 41.39701867748817676, -9.422509992056140149 ) ) ;
#92027 = CARTESIAN_POINT ( 'NONE',  ( 20.88017736071110164, 35.35535201082150536, 2.915334737309930979 ) ) ;
#92030 = CARTESIAN_POINT ( 'NONE',  ( -1.099225684535947600, 33.70696800326375353, -6.408140936763238038 ) ) ;
#92029 = CARTESIAN_POINT ( 'NONE',  ( 0.5774900079438607392, 3.480352010821504027, 5.440088680355550821 ) ) ;
#92031 = CARTESIAN_POINT ( 'NONE',  ( 22.26659068614894466, 18.88708216824730002, 7.082119434687054849 ) ) ;
#92032 = AXIS2_PLACEMENT_3D ( 'NONE', #76328, #53828, #1343 ) ;
#92033 = EDGE_CURVE ( 'NONE', #37825, #21097, #55967, .T. ) ;
#92035 = CARTESIAN_POINT ( 'NONE',  ( 6.565887622018943937, 40.16530133659708923, 12.81628187352647430 ) ) ;
#92034 = AXIS2_PLACEMENT_3D ( 'NONE', #16670, #87114, #46660 ) ;
#92036 = VERTEX_POINT ( 'NONE', #14945 ) ;
#92037 = CARTESIAN_POINT ( 'NONE',  ( 19.84674366389459621, 38.50893115100078745, 7.409399052514197653E-17 ) ) ;
#92038 = CARTESIAN_POINT ( 'NONE',  ( 10.00000000000000178, 14.31368534415483929, 10.88017736071110342 ) ) ;
#92039 = ORIENTED_EDGE ( 'NONE', *, *, #4170, .T. ) ;
#92040 = ADVANCED_FACE ( 'NONE', ( #45414 ), #17977, .T. ) ;
#92041 = CARTESIAN_POINT ( 'NONE',  ( 0.5774900079438590739, 22.64701867748817321, -5.440088680355550821 ) ) ;
#92042 = VERTEX_POINT ( 'NONE', #451 ) ;
#92043 = CARTESIAN_POINT ( 'NONE',  ( -0.8801773607111009756, 58.06368534415484106, 1.068504757029289695E-15 ) ) ;
#92044 = CARTESIAN_POINT ( 'NONE',  ( 19.42250999205614548, 65.98035201082151957, -5.440088680355545492 ) ) ;
#92045 = CARTESIAN_POINT ( 'NONE',  ( 17.96484262340118221, 64.93868534415483396, 7.964842623401181321 ) ) ;
#92046 = CARTESIAN_POINT ( 'NONE',  ( 1.472469842513823179, 15.59226448433411960, -4.923371831947296329 ) ) ;
#92047 = CARTESIAN_POINT ( 'NONE',  ( 17.20831665107776587, 4.133931151000785675, -7.208316651077762316 ) ) ;
#92048 = CARTESIAN_POINT ( 'NONE',  ( -12.50534872682722565, 4.101355178835516792E-16, -7.339363270777700343 ) ) ;
#92050 = CARTESIAN_POINT ( 'NONE',  ( -8.000000000000000000, 1.019547802438458550, -3.750000000000000000 ) ) ;
#92049 = TOROIDAL_SURFACE ( 'NONE', #72915, 14.49999999999999822, 0.5000000000000000000 ) ;
#92052 = VERTEX_POINT ( 'NONE', #38917 ) ;
#92051 = CARTESIAN_POINT ( 'NONE',  ( 14.92337183194729633, 2.675597817667451750, 8.527530157486181039 ) ) ;
#92053 = VECTOR ( 'NONE', #46932, 1000.000000000000000 ) ;
#92054 = AXIS2_PLACEMENT_3D ( 'NONE', #63641, #56169, #25675 ) ;
#92055 = CARTESIAN_POINT ( 'NONE',  ( 5.076628168052703671, 41.84226448433411605, 8.527530157486179263 ) ) ;
#92056 = ORIENTED_EDGE ( 'NONE', *, *, #86270, .F. ) ;
#92057 = VERTEX_POINT ( 'NONE', #15916 ) ;
#92058 = CARTESIAN_POINT ( 'NONE',  ( 3.469446951953614189E-15, 8.912123368507815613, 11.92686044187656513 ) ) ;
#92059 = CARTESIAN_POINT ( 'NONE',  ( 20.20024927138669213, 69.97537705844109723, -6.181741512438952313 ) ) ;
#92060 = CARTESIAN_POINT ( 'NONE',  ( 6.204703633549690345, 12.84541550158063572, 14.16423886937410082 ) ) ;
#92061 = DIRECTION ( 'NONE',  ( 0.5547001962252290364, 0.8320502943378437211, 0.000000000000000000 ) ) ;
#92063 = CARTESIAN_POINT ( 'NONE',  ( 17.96484262340118221, 59.93868534415484106, 7.964842623401181321 ) ) ;
#92062 = CARTESIAN_POINT ( 'NONE',  ( 20.30776406404399737, 70.00000000000000000, 6.000000000000270894 ) ) ;
#92064 = CARTESIAN_POINT ( 'NONE',  ( 17.96484262340118221, 16.18868534415483396, -7.964842623401177768 ) ) ;
#92065 = ORIENTED_EDGE ( 'NONE', *, *, #45429, .F. ) ;
#92066 = CARTESIAN_POINT ( 'NONE',  ( 0.1532563361054082862, 1.217264484334117824, 2.638427012816831674 ) ) ;
#92067 = SURFACE_SIDE_STYLE ('',( #24578 ) ) ;
#92068 = MECHANICAL_DESIGN_GEOMETRIC_PRESENTATION_REPRESENTATION (  '', ( #15448 ), #18630 ) ;
#92069 = CARTESIAN_POINT ( 'NONE',  ( 21.09922568453595559, 27.04030133659708568, -6.408140936763230044 ) ) ;
#92070 = CARTESIAN_POINT ( 'NONE',  ( 12.63842701281683922, 19.55059781766745175, -9.846743663894590881 ) ) ;
#92071 = PRESENTATION_STYLE_ASSIGNMENT (( #8090 ) ) ;
#92072 = EDGE_CURVE ( 'NONE', #81875, #54039, #72263, .T. ) ;
#92073 = CARTESIAN_POINT ( 'NONE',  ( 12.63842701281683034, 17.46726448433411250, 9.846743663894596210 ) ) ;
#92074 = CARTESIAN_POINT ( 'NONE',  ( 19.38216949554541557, 12.24863466993041961, -9.382169495545420901 ) ) ;
#92075 = CARTESIAN_POINT ( 'NONE',  ( 0.000000000000000000, 0.5000000000000004441, 0.000000000000000000 ) ) ;
#92076 = MECHANICAL_DESIGN_GEOMETRIC_PRESENTATION_REPRESENTATION (  '', ( #95270 ), #64928 ) ;
#92077 = CARTESIAN_POINT ( 'NONE',  ( 19.84674366389459266, 8.717264484334116048, -2.638427012816827677 ) ) ;
#92078 = EDGE_LOOP ( 'NONE', ( #31538, #84846, #19015, #40878 ) ) ;
#92079 = ORIENTED_EDGE ( 'NONE', *, *, #26520, .F. ) ;
#92080 = CARTESIAN_POINT ( 'NONE',  ( -0.8801773607111008646, 28.27201867748817321, 2.915334737309923430 ) ) ;
#92081 = CARTESIAN_POINT ( 'NONE',  ( 10.00000000000000000, 25.55374883491396787, -14.16423886937410082 ) ) ;
#92082 = CARTESIAN_POINT ( 'NONE',  ( 2.791683348922240793, 46.63393115100077324, 7.208316651077764092 ) ) ;
#92083 = CARTESIAN_POINT ( 'NONE',  ( 0.5774900079438590739, 67.64701867748817676, -5.440088680355550821 ) ) ;
#92085 = DIRECTION ( 'NONE',  ( 0.000000000000000000, 0.000000000000000000, 1.000000000000000000 ) ) ;
#92084 = CARTESIAN_POINT ( 'NONE',  ( 16.40814093676323893, 35.79030133659708923, 11.09922568453595026 ) ) ;
#92086 = CARTESIAN_POINT ( 'NONE',  ( 10.00000000000000000, 21.81368534415484106, -10.88017736071110342 ) ) ;
#92087 = CARTESIAN_POINT ( 'NONE',  ( -5.999999999999994671, 41.24999999999999289, -6.500000000000000888 ) ) ;
#92088 = CARTESIAN_POINT ( 'NONE',  ( 21.09922568453595559, 7.040301336597086568, -6.408140936763230044 ) ) ;
#92089 = CARTESIAN_POINT ( 'NONE',  ( 19.84674366389459266, 38.71726448433412315, -2.638427012816827677 ) ) ;
#92090 = CARTESIAN_POINT ( 'NONE',  ( -7.964842623401172439, -1.311314655845159605, 7.964842623401183097 ) ) ;
#92091 = CARTESIAN_POINT ( 'NONE',  ( 6.565887622018943937, 53.08196800326374643, -12.81628187352647608 ) ) ;
#92092 =( NAMED_UNIT ( * ) PLANE_ANGLE_UNIT ( ) SI_UNIT ( $, .RADIAN. ) );
#92094 = CARTESIAN_POINT ( 'NONE',  ( -6.319286839011487800, -45.42958518191715456, -2.500000000000000000 ) ) ;
#92093 = CARTESIAN_POINT ( 'NONE',  ( 10.00000000000000178, 54.31368534415484106, 10.88017736071110342 ) ) ;
#92095 = CARTESIAN_POINT ( 'NONE',  ( 56.78206182523731371, -3.303428494291771322E-15, 0.000000000000000000 ) ) ;
#92096 = FACE_OUTER_BOUND ( 'NONE', #79451, .T. ) ;
#92097 = CARTESIAN_POINT ( 'NONE',  ( 17.96484262340118221, 36.18868534415484106, -7.964842623401177768 ) ) ;
#92098 = CARTESIAN_POINT ( 'NONE',  ( 20.88017736071110164, 50.35535201082151247, 2.915334737309930979 ) ) ;
#92099 = CARTESIAN_POINT ( 'NONE',  ( 0.1532563361054082862, 61.21726448433412315, 2.638427012816831674 ) ) ;
#92100 = B_SPLINE_CURVE_WITH_KNOTS ( 'NONE', 3,
 ( #55808, #25322, #86301, #39817, #56300, #86794 ),
 .UNSPECIFIED., .F., .F.,
 ( 4, 2, 4 ),
 ( 0.000000000000000000, 0.0002565770811490931079, 0.0005131541622981862158 ),
 .UNSPECIFIED. ) ;
#92101 = CARTESIAN_POINT ( 'NONE',  ( -0.8801773607110991993, 62.85535201082150536, -2.915334737309923874 ) ) ;
#92102 = VECTOR ( 'NONE', #68698, 1000.000000000000000 ) ;
#92103 = CARTESIAN_POINT ( 'NONE',  ( 19.84674366389459266, 53.71726448433411605, -2.638427012816827677 ) ) ;
#92105 = CARTESIAN_POINT ( 'NONE',  ( 19.84674366389459621, 23.50893115100078390, 7.409399052514197653E-17 ) ) ;
#92104 = CARTESIAN_POINT ( 'NONE',  ( -0.8801773607110991993, 2.855352010821504471, -2.915334737309923874 ) ) ;
#92106 = CARTESIAN_POINT ( 'NONE',  ( 10.00000000000000178, 5.373634669930420493, 12.81628187352647608 ) ) ;
#92107 = ORIENTED_EDGE ( 'NONE', *, *, #41920, .T. ) ;
#92108 = CARTESIAN_POINT ( 'NONE',  ( 2.035157376598822676, 37.43868534415484106, -7.964842623401177768 ) ) ;
#92110 = CARTESIAN_POINT ( 'NONE',  ( 31.00000000000000355, 44.99999999999999289, 7.000000000000000000 ) ) ;
#92109 = CARTESIAN_POINT ( 'NONE',  ( 21.09922568453595559, 2.040301336597086568, -6.408140936763230044 ) ) ;
#92111 = CARTESIAN_POINT ( 'NONE',  ( 20.88017736071110519, 10.56368534415483751, 2.639326808657452039E-16 ) ) ;
#92112 = CARTESIAN_POINT ( 'NONE',  ( -0.8801773607111008646, 23.27201867748817676, 2.915334737309923430 ) ) ;
#92113 = CARTESIAN_POINT ( 'NONE',  ( -4.164238869374098151, 36.59541550158063217, -3.795296366450310543 ) ) ;
#92114 = CARTESIAN_POINT ( 'NONE',  ( 10.00000000000000000, 24.75893115100078745, -9.846743663894594434 ) ) ;
#92115 = CARTESIAN_POINT ( 'NONE',  ( 4.559911319644449179, 57.23035201082150536, -9.422509992056141925 ) ) ;
#92116 = CARTESIAN_POINT ( 'NONE',  ( 0.7577696756375204012, 14.76984978199329568, 14.92139465029755385 ) ) ;
#92117 = CARTESIAN_POINT ( 'NONE',  ( 2.917880565312948704, 7.637082168247301794, 12.26659068614894643 ) ) ;
#92118 = EDGE_CURVE ( 'NONE', #84056, #74723, #76146, .T. ) ;
#92119 = AXIS2_PLACEMENT_3D ( 'NONE', #94285, #79292, #87763 ) ;
#92120 = AXIS2_PLACEMENT_3D ( 'NONE', #48413, #77929, #33395 ) ;
#92121 = CARTESIAN_POINT ( 'NONE',  ( 5.817157072110803462, 0.3639308157993877413, -13.82608706751090821 ) ) ;
#92122 = CARTESIAN_POINT ( 'NONE',  ( 1.472469842513823179, 56.42559781766745886, 4.923371831947296329 ) ) ;
#92123 =( GEOMETRIC_REPRESENTATION_CONTEXT ( 3 ) GLOBAL_UNCERTAINTY_ASSIGNED_CONTEXT ( ( #63204 ) ) GLOBAL_UNIT_ASSIGNED_CONTEXT ( ( #38628, #68635, #15648 ) ) REPRESENTATION_CONTEXT ( 'NONE', 'WORKASPACE' ) );
#92125 = ORIENTED_EDGE ( 'NONE', *, *, #37611, .T. ) ;
#92124 = EDGE_CURVE ( 'NONE', #65059, #49672, #29159, .T. ) ;
#92126 = ORIENTED_EDGE ( 'NONE', *, *, #14925, .T. ) ;
#92127 = CARTESIAN_POINT ( 'NONE',  ( -4.164238869374099039, 36.80374883491396787, 8.674139862899312516E-16 ) ) ;
#92129 = CIRCLE ( 'NONE', #63352, 14.49999999999999822 ) ;
#92128 = CARTESIAN_POINT ( 'NONE',  ( 2.917880565312950480, 30.97041550158063572, -12.26659068614894821 ) ) ;
#92130 = CARTESIAN_POINT ( 'NONE',  ( 4.559911319644449179, 68.89701867748817676, 9.422509992056141925 ) ) ;
#92131 = CARTESIAN_POINT ( 'NONE',  ( 2.791683348922240793, 56.63393115100078035, 7.208316651077764092 ) ) ;
#92132 = CARTESIAN_POINT ( 'NONE',  ( -10.57481851845687260, -40.44832046089691602, 3.750000000000000000 ) ) ;
#92134 = CARTESIAN_POINT ( 'NONE',  ( 6.565887622018943937, 20.16530133659708213, 12.81628187352647430 ) ) ;
#92133 = CARTESIAN_POINT ( 'NONE',  ( 20.88017736071110875, 65.77201867748817676, -2.915334737309920765 ) ) ;
#92135 = CARTESIAN_POINT ( 'NONE',  ( -2.266590686148945544, 26.38708216824730357, -7.082119434687050408 ) ) ;
#92136 = CARTESIAN_POINT ( 'NONE',  ( 15.44008868035555793, 11.39701867748817143, -9.422509992056140149 ) ) ;
#92137 = ADVANCED_FACE ( 'NONE', ( #67442 ), #90410, .T. ) ;
#92138 = CARTESIAN_POINT ( 'NONE',  ( 0.5774900079438590739, 32.64701867748816966, -5.440088680355550821 ) ) ;
#92139 = LINE ( 'NONE', #32608, #84297 ) ;
#92140 = CARTESIAN_POINT ( 'NONE',  ( 15.44008868035555260, 59.73035201082151247, 9.422509992056143702 ) ) ;
#92141 = CARTESIAN_POINT ( 'NONE',  ( 7.208316651077762316, -10.86606884899921610, -7.208316651077764980 ) ) ;
#92142 = ORIENTED_EDGE ( 'NONE', *, *, #11850, .T. ) ;
#92143 = DIRECTION ( 'NONE',  ( -0.3987490689252593534, -0.000000000000000000, 0.9170600743851183845 ) ) ;
#92144 = CARTESIAN_POINT ( 'NONE',  ( 4.873787042390699931, 15.00000000000000000, 13.39061984619922718 ) ) ;
#92145 = VERTEX_POINT ( 'NONE', #79365 ) ;
#92146 = CARTESIAN_POINT ( 'NONE',  ( -4.164238869374098151, 1.595415501580634388, -3.795296366450310543 ) ) ;
#92148 = CARTESIAN_POINT ( 'NONE',  ( 0.5774900079438607392, 3.480352010821504916, 5.440088680355550821 ) ) ;
#92147 = CARTESIAN_POINT ( 'NONE',  ( -0.3689425029237898834, 56.17874883491396076, -10.36894250292378850 ) ) ;
#92150 = CARTESIAN_POINT ( 'NONE',  ( 10.00000000000000000, 59.75893115100078745, -9.846743663894594434 ) ) ;
#92149 = CARTESIAN_POINT ( 'NONE',  ( 0.1532563361054082862, 36.21726448433410894, 2.638427012816831674 ) ) ;
#92151 = EDGE_CURVE ( 'NONE', #35492, #18106, #65916, .T. ) ;
#92152 = DIRECTION ( 'NONE',  ( 0.000000000000000000, 0.000000000000000000, 1.000000000000000000 ) ) ;
#92153 = CARTESIAN_POINT ( 'NONE',  ( 17.75000000000000000, 84.07179676972448590, 3.750000000000000000 ) ) ;
#92154 = CARTESIAN_POINT ( 'NONE',  ( 10.00000000000000178, 5.373634669930420493, 12.81628187352647608 ) ) ;
#92155 = CARTESIAN_POINT ( 'NONE',  ( 11.09922568453594671, 17.04030133659709279, -6.408140936763241591 ) ) ;
#92156 = AXIS2_PLACEMENT_3D ( 'NONE', #65276, #86825, #95297 ) ;
#92157 = ORIENTED_EDGE ( 'NONE', *, *, #73815, .F. ) ;
#92158 = CARTESIAN_POINT ( 'NONE',  ( -2.266590686148945544, 41.38708216824729647, -7.082119434687050408 ) ) ;
#92159 = ADVANCED_FACE ( 'NONE', ( #9895 ), #56379, .F. ) ;
#92160 = CARTESIAN_POINT ( 'NONE',  ( 22.26659068614895176, 44.72041550158063927, -7.082119434687042414 ) ) ;
#92161 = ORIENTED_EDGE ( 'NONE', *, *, #15724, .F. ) ;
#92162 = CARTESIAN_POINT ( 'NONE',  ( 0.6178305044545818747, 53.49863466993041072, -9.382169495545419124 ) ) ;
#92163 = CARTESIAN_POINT ( 'NONE',  ( 7.361572987183170547, 47.05059781766745175, 9.846743663894590881 ) ) ;
#92164 = CARTESIAN_POINT ( 'NONE',  ( 19.42250999205614193, 30.14701867748817321, 5.440088680355555262 ) ) ;
#92165 = DIRECTION ( 'NONE',  ( -1.000000000000000000, -2.799047438454523729E-16, 0.000000000000000000 ) ) ;
#92166 = CARTESIAN_POINT ( 'NONE',  ( 1.472469842513823179, 50.59226448433411605, -4.923371831947296329 ) ) ;
#92167 = CARTESIAN_POINT ( 'NONE',  ( 18.52753015748618282, 43.92559781766745175, -4.923371831947291888 ) ) ;
#92168 = ADVANCED_FACE ( 'NONE', ( #92880 ), #38745, .T. ) ;
#92170 = VERTEX_POINT ( 'NONE', #18377 ) ;
#92169 = CARTESIAN_POINT ( 'NONE',  ( 7.313705784284593392, 0.5000000000000004441, -13.09617149020743732 ) ) ;
#92171 = CARTESIAN_POINT ( 'NONE',  ( -14.56372689393326780, 0.04962896412619356018, -2.356940382833208059 ) ) ;
#92172 = CARTESIAN_POINT ( 'NONE',  ( 2.791683348922237240, 5.383931151000785675, -7.208316651077763204 ) ) ;
#92173 = CARTESIAN_POINT ( 'NONE',  ( -8.375939845167600595, 0.000000000000000000, -11.52849216984310310 ) ) ;
#92174 = ORIENTED_EDGE ( 'NONE', *, *, #9761, .T. ) ;
#92175 =( GEOMETRIC_REPRESENTATION_CONTEXT ( 3 ) GLOBAL_UNCERTAINTY_ASSIGNED_CONTEXT ( ( #20492 ) ) GLOBAL_UNIT_ASSIGNED_CONTEXT ( ( #9055, #41043, #64003 ) ) REPRESENTATION_CONTEXT ( 'NONE', 'WORKASPACE' ) );
#92176 = CARTESIAN_POINT ( 'NONE',  ( -8.924603092375777535, 75.06466731010172566, -2.900000000000000799 ) ) ;
#92177 = CARTESIAN_POINT ( 'NONE',  ( 14.92337183194729633, 27.67559781766745530, 8.527530157486181039 ) ) ;
#92178 = CARTESIAN_POINT ( 'NONE',  ( 6.728851239469011425, 15.00000000000000533, 12.98580270086205601 ) ) ;
#92179 = CARTESIAN_POINT ( 'NONE',  ( 19.38216949554541557, 37.24863466993041783, -9.382169495545420901 ) ) ;
#92180 = CARTESIAN_POINT ( 'NONE',  ( -5.795997163829992083, 15.00000000000000000, -13.01802277140713926 ) ) ;
#92181 = ORIENTED_EDGE ( 'NONE', *, *, #58344, .F. ) ;
#92182 = DIRECTION ( 'NONE',  ( 1.000000000000000000, 0.000000000000000000, -0.000000000000000000 ) ) ;
#92183 = CARTESIAN_POINT ( 'NONE',  ( -13.95806775979402303, 2.100641709190664841E-16, 4.371577651620636829 ) ) ;
#92184 = CARTESIAN_POINT ( 'NONE',  ( 14.92337183194729988, 59.34226448433412315, -8.527530157486177487 ) ) ;
#92185 = CARTESIAN_POINT ( 'NONE',  ( 17.08211943468705840, 30.13708216824730357, -12.26659068614894466 ) ) ;
#92186 = CARTESIAN_POINT ( 'NONE',  ( 12.63842701281683034, 62.46726448433410894, 9.846743663894596210 ) ) ;
#92187 = CARTESIAN_POINT ( 'NONE',  ( 0.2751277870542949144, 4.366073187301309666, -6.499999999999997335 ) ) ;
#92188 = CARTESIAN_POINT ( 'NONE',  ( 5.076628168052704559, 20.17559781766745175, -8.527530157486179263 ) ) ;
#92189 = VECTOR ( 'NONE', #42476, 1000.000000000000000 ) ;
#92190 = CARTESIAN_POINT ( 'NONE',  ( 16.40814093676324603, 52.45696800326375353, -11.09922568453594671 ) ) ;
#92191 = CARTESIAN_POINT ( 'NONE',  ( 24.16423886937410614, 4.303748834913967869, 8.672049930838204340E-16 ) ) ;
#92192 = CARTESIAN_POINT ( 'NONE',  ( 0.1532563361054083140, 61.00893115100078745, 1.131784320476157264E-15 ) ) ;
#92193 = CARTESIAN_POINT ( 'NONE',  ( 19.42250999205614193, 50.14701867748817676, 5.440088680355555262 ) ) ;
#92194 = AXIS2_PLACEMENT_3D ( 'NONE', #46670, #1691, #54655 ) ;
#92195 = AXIS2_PLACEMENT_3D ( 'NONE', #36038, #14544, #66541 ) ;
#92196 = CARTESIAN_POINT ( 'NONE',  ( 4.471352795669433888, -3.620003340312029749, -2.749999999999999556 ) ) ;
#92197 = CARTESIAN_POINT ( 'NONE',  ( 2.035157376598822676, 62.43868534415483396, -7.964842623401177768 ) ) ;
#92198 = ORIENTED_EDGE ( 'NONE', *, *, #82319, .T. ) ;
#92199 = LINE ( 'NONE', #14238, #44136 ) ;
#92200 = CARTESIAN_POINT ( 'NONE',  ( 17.96484262340118221, 26.18868534415483396, -7.964842623401177768 ) ) ;
#92202 = CARTESIAN_POINT ( 'NONE',  ( 20.88017736071110875, 55.77201867748816966, -2.915334737309920765 ) ) ;
#92201 = CARTESIAN_POINT ( 'NONE',  ( 16.40814093676324603, 2.456968003263753531, -11.09922568453594671 ) ) ;
#92203 = CARTESIAN_POINT ( 'NONE',  ( -0.3289641300568009741, 47.24545670184114243, -5.963430220938281678 ) ) ;
#92204 = CARTESIAN_POINT ( 'NONE',  ( 0.000000000000000000, -97.00000000000000000, 3.750000000000000000 ) ) ;
#92205 = CARTESIAN_POINT ( 'NONE',  ( 2.035157376598824452, 38.68868534415483396, 7.964842623401179544 ) ) ;
#92206 = ADVANCED_FACE ( 'NONE', ( #25878 ), #40399, .F. ) ;
#92207 = CARTESIAN_POINT ( 'NONE',  ( 18.52753015748618282, 38.92559781766745175, -4.923371831947291888 ) ) ;
#92208 = CARTESIAN_POINT ( 'NONE',  ( 3.469446951953614189E-15, 23.05374883491398563, 14.16423886937410259 ) ) ;
#92209 = CARTESIAN_POINT ( 'NONE',  ( 0.1532563361054083140, 66.00893115100079456, 1.131784320476157264E-15 ) ) ;
#92210 = CARTESIAN_POINT ( 'NONE',  ( -0.8801773607111008646, 8.272018677488171434, 2.915334737309923430 ) ) ;
#92211 = CARTESIAN_POINT ( 'NONE',  ( 3.192513988408121950, 15.00000000000000000, -14.27292421863750604 ) ) ;
#92212 = EDGE_CURVE ( 'NONE', #23913, #15375, #90472, .T. ) ;
#92213 = CARTESIAN_POINT ( 'NONE',  ( 6.204703633549690345, 17.84541550158063217, 14.16423886937410082 ) ) ;
#92214 = CARTESIAN_POINT ( 'NONE',  ( 22.26659068614894466, 58.88708216824729647, 7.082119434687054849 ) ) ;
#92215 =( BOUNDED_SURFACE ( )  B_SPLINE_SURFACE ( 3, 2, ( 
 ( #96957, #28429, #43912 ),
 ( #66923, #97444, #95957 ),
 ( #88935, #89916, #21430 ),
 ( #27439, #35433, #51927 ),
 ( #57933, #44414, #6416 ),
 ( #88442, #61874, #22922 ),
 ( #76398, #53391, #62361 ),
 ( #82914, #75404, #77367 ),
 ( #84405, #37925, #22426 ),
 ( #75903, #60402, #92379 ),
 ( #83900, #38904, #69889 ),
 ( #30889, #83410, #6922 ),
 ( #14931, #69391, #37431 ),
 ( #23905, #8395, #913 ),
 ( #90898, #39396, #45397 ),
 ( #14432, #76881, #44901 ),
 ( #92865, #45910, #1409 ),
 ( #67920, #53898, #98937 ) ),
 .UNSPECIFIED., .F., .F., .T. ) 
 B_SPLINE_SURFACE_WITH_KNOTS ( ( 4, 2, 2, 2, 2, 2, 2, 2, 4 ),
 ( 3, 3 ),
 ( 0.000000000000000000, 0.002783952809522130881, 0.005567905619044261761, 0.01113581123808852352, 0.02227162247617704705, 0.04454324495235409409, 0.06681486742853114114, 0.07795067866661967160, 0.08908648990470818818 ),
 ( 0.000000000000000000, 1.000000000000000000 ),
 .UNSPECIFIED. ) 
 GEOMETRIC_REPRESENTATION_ITEM ( )  RATIONAL_B_SPLINE_SURFACE ( (
 ( 1.000000000000000000, 0.7071067811865475727, 1.000000000000000000),
 ( 1.000000000000000000, 0.7071067811865475727, 1.000000000000000000),
 ( 1.000000000000000000, 0.7071067811865475727, 1.000000000000000000),
 ( 1.000000000000000000, 0.7071067811865475727, 1.000000000000000000),
 ( 1.000000000000000000, 0.7071067811865475727, 1.000000000000000000),
 ( 1.000000000000000000, 0.7071067811865475727, 1.000000000000000000),
 ( 1.000000000000000000, 0.7071067811865475727, 1.000000000000000000),
 ( 1.000000000000000000, 0.7071067811865475727, 1.000000000000000000),
 ( 1.000000000000000000, 0.7071067811865475727, 1.000000000000000000),
 ( 1.000000000000000000, 0.7071067811865475727, 1.000000000000000000),
 ( 1.000000000000000000, 0.7071067811865487940, 1.000000000000000000),
 ( 1.000000000000000000, 0.7071067811865487940, 1.000000000000000000),
 ( 1.000000000000000000, 0.7071067811865487940, 1.000000000000000000),
 ( 1.000000000000000000, 0.7071067811865487940, 1.000000000000000000),
 ( 1.000000000000000000, 0.7071067811865475727, 1.000000000000000000),
 ( 1.000000000000000000, 0.7071067811865475727, 1.000000000000000000),
 ( 1.000000000000000000, 0.7071067811865479058, 1.000000000000000000),
 ( 1.000000000000000000, 0.7071067811865479058, 1.000000000000000000) ) ) 
 REPRESENTATION_ITEM ( '' )  SURFACE ( )  );
#92216 = CARTESIAN_POINT ( 'NONE',  ( 19.84674366389459266, 23.71726448433412315, -2.638427012816827677 ) ) ;
#92217 = ORIENTED_EDGE ( 'NONE', *, *, #88225, .T. ) ;
#92218 = CARTESIAN_POINT ( 'NONE',  ( 7.361572987183170547, 22.05059781766745530, 9.846743663894590881 ) ) ;
#92219 = CARTESIAN_POINT ( 'NONE',  ( 12.91533473730992121, 24.52201867748816966, 10.88017736071110164 ) ) ;
#92220 = CARTESIAN_POINT ( 'NONE',  ( 19.84674366389459621, 63.50893115100078745, 7.409399052514197653E-17 ) ) ;
#92222 = CARTESIAN_POINT ( 'NONE',  ( 18.95386800104996183, 48.23810908735726599, -6.499999999999982236 ) ) ;
#92221 = CARTESIAN_POINT ( 'NONE',  ( -0.3689425029237898834, 11.17874883491396787, -10.36894250292378850 ) ) ;
#92223 = DIRECTION ( 'NONE',  ( 0.000000000000000000, -0.000000000000000000, 1.000000000000000000 ) ) ;
#92224 = AXIS2_PLACEMENT_3D ( 'NONE', #80367, #18886, #3887 ) ;
#92225 = UNCERTAINTY_MEASURE_WITH_UNIT (LENGTH_MEASURE( 1.000000000000000082E-05 ), #8539, 'distance_accuracy_value', 'NONE');
#92226 = CARTESIAN_POINT ( 'NONE',  ( 5.076628168052704559, 15.17559781766745175, -8.527530157486179263 ) ) ;
#92227 = CARTESIAN_POINT ( 'NONE',  ( 3.591859063236761518, 39.95696800326375353, 11.09922568453594849 ) ) ;
#92228 = CARTESIAN_POINT ( 'NONE',  ( 7.361572987183170547, 37.05059781766744464, 9.846743663894590881 ) ) ;
#92229 = VERTEX_POINT ( 'NONE', #93377 ) ;
#92230 = CARTESIAN_POINT ( 'NONE',  ( 14.92337183194729988, 19.34226448433411960, -8.527530157486177487 ) ) ;
#92231 = DIRECTION ( 'NONE',  ( 0.000000000000000000, -1.000000000000000000, 0.000000000000000000 ) ) ;
#92232 = CARTESIAN_POINT ( 'NONE',  ( 24.16423886937409904, 59.09541550158063217, 3.795296366450317205 ) ) ;
#92233 = CARTESIAN_POINT ( 'NONE',  ( -0.8801773607111009756, 53.06368534415484106, 1.068504757029289695E-15 ) ) ;
#92234 = SURFACE_STYLE_FILL_AREA ( #75749 ) ;
#92235 = CARTESIAN_POINT ( 'NONE',  ( 20.88017736071110519, 55.56368534415484817, 2.639326808657452039E-16 ) ) ;
#92236 = CARTESIAN_POINT ( 'NONE',  ( 1.472469842513823179, 30.59226448433411960, -4.923371831947296329 ) ) ;
#92237 = CARTESIAN_POINT ( 'NONE',  ( 19.42250999205614193, 5.147018677488171434, 5.440088680355555262 ) ) ;
#92238 = CARTESIAN_POINT ( 'NONE',  ( 17.62281668512001787, 38.28593319516822646, 6.500000000000010658 ) ) ;
#92239 = CARTESIAN_POINT ( 'NONE',  ( 18.52753015748618282, 53.92559781766745175, -4.923371831947291888 ) ) ;
#92240 = CARTESIAN_POINT ( 'NONE',  ( 19.42250999205614548, 45.98035201082150536, -5.440088680355545492 ) ) ;
#92241 = FACE_OUTER_BOUND ( 'NONE', #92278, .T. ) ;
#92242 = UNCERTAINTY_MEASURE_WITH_UNIT (LENGTH_MEASURE( 1.000000000000000082E-05 ), #4059, 'distance_accuracy_value', 'NONE');
#92243 = AXIS2_PLACEMENT_3D ( 'NONE', #43065, #34064, #80073 ) ;
#92245 = ORIENTED_EDGE ( 'NONE', *, *, #39998, .T. ) ;
#92244 = ADVANCED_FACE ( 'NONE', ( #55883 ), #23393, .T. ) ;
#92246 = ORIENTED_EDGE ( 'NONE', *, *, #70402, .F. ) ;
#92247 = DIRECTION ( 'NONE',  ( 1.000000000000000000, 0.000000000000000000, 0.000000000000000000 ) ) ;
#92248 = CARTESIAN_POINT ( 'NONE',  ( 11.25000000000000178, 5.213468844518207135, 3.014428414850127691 ) ) ;
#92249 = CARTESIAN_POINT ( 'NONE',  ( 14.92337183194729988, 24.34226448433411960, -8.527530157486177487 ) ) ;
#92250 = CARTESIAN_POINT ( 'NONE',  ( 16.40814093676324603, 57.45696800326375353, -11.09922568453594671 ) ) ;
#92252 = CARTESIAN_POINT ( 'NONE',  ( 2.791683348922237240, 50.38393115100078035, -7.208316651077763204 ) ) ;
#92251 = CARTESIAN_POINT ( 'NONE',  ( 19.42250999205614548, 20.98035201082150891, -5.440088680355545492 ) ) ;
#92253 = DIRECTION ( 'NONE',  ( 0.6755902076156591329, 0.000000000000000000, -0.7372773368101250835 ) ) ;
#92254 = CARTESIAN_POINT ( 'NONE',  ( -0.3689425029237881626, 32.42874883491395366, 10.36894250292379027 ) ) ;
#92255 = ADVANCED_FACE ( 'NONE', ( #28380 ), #5400, .T. ) ;
#92256 = CARTESIAN_POINT ( 'NONE',  ( -2.266590686148945544, 62.22041550158063927, 7.082119434687048631 ) ) ;
#92257 = CARTESIAN_POINT ( 'NONE',  ( 1.472469842513823179, 56.42559781766745886, 4.923371831947296329 ) ) ;
#92258 = CARTESIAN_POINT ( 'NONE',  ( 0.000000000000000000, 0.5000000000000004441, 0.000000000000000000 ) ) ;
#92259 = CARTESIAN_POINT ( 'NONE',  ( -0.8801773607111009756, 58.06368534415484106, 1.068504757029289695E-15 ) ) ;
#92260 = CARTESIAN_POINT ( 'NONE',  ( 17.20831665107776587, 19.13393115100078035, -7.208316651077762316 ) ) ;
#92261 = CIRCLE ( 'NONE', #71504, 0.2500000000000002220 ) ;
#92262 = DIRECTION ( 'NONE',  ( 0.000000000000000000, 0.000000000000000000, 1.000000000000000000 ) ) ;
#92263 = ORIENTED_EDGE ( 'NONE', *, *, #61633, .F. ) ;
#92264 = CARTESIAN_POINT ( 'NONE',  ( -4.000000000000000000, 10.25000000000000000, 3.750000000000000000 ) ) ;
#92265 = ORIENTED_EDGE ( 'NONE', *, *, #13694, .T. ) ;
#92266 = CARTESIAN_POINT ( 'NONE',  ( 19.84674366389459621, 13.50893115100078568, 7.409399052514197653E-17 ) ) ;
#92267 = ORIENTED_EDGE ( 'NONE', *, *, #40495, .T. ) ;
#92268 = CARTESIAN_POINT ( 'NONE',  ( 24.16423886937410614, 19.30374883491397142, 8.672049930838204340E-16 ) ) ;
#92269 = CARTESIAN_POINT ( 'NONE',  ( 0.1532563361054083140, 21.00893115100078745, 1.131784320476157264E-15 ) ) ;
#92270 = CARTESIAN_POINT ( 'NONE',  ( 20.88017736071110519, 40.56368534415484106, 2.639326808657452039E-16 ) ) ;
#92271 = AXIS2_PLACEMENT_3D ( 'NONE', #21012, #83481, #20516 ) ;
#92272 = SURFACE_STYLE_FILL_AREA ( #69283 ) ;
#92273 = ORIENTED_EDGE ( 'NONE', *, *, #51299, .F. ) ;
#92274 = CARTESIAN_POINT ( 'NONE',  ( -0.8801773607111009756, 33.06368534415484106, 1.068504757029289695E-15 ) ) ;
#92275 = ADVANCED_FACE ( 'NONE', ( #44844 ), #14841, .T. ) ;
#92276 = ORIENTED_EDGE ( 'NONE', *, *, #9646, .F. ) ;
#92277 = CARTESIAN_POINT ( 'NONE',  ( -2.393480905993250918, 15.00000000000000000, 14.80781041047749724 ) ) ;
#92278 = EDGE_LOOP ( 'NONE', ( #8665, #4626, #54475, #91071, #71854, #60070, #77752, #35312, #46884, #42499, #60768, #67154, #23969, #40815, #76641, #13490, #79699, #89801, #47427, #48088, #48005, #3430, #85643, #60885, #89500, #3737, #77049, #98707, #98086, #94611, #37309, #88567, #77696, #17752, #79012, #32123, #62791, #66310, #91033, #13578, #28015, #56520, #36569, #52841, #95598, #85613, #98675, #98484, #42268, #94217, #21667, #17415, #68233, #80884, #71795, #87779, #43465, #97335, #27889, #74757, #16915, #47249, #24518, #73181, #53922, #34621, #29771, #2155, #46686, #34657, #93200, #7062, #34398, #98329, #45065, #21553, #49111, #20974, #6219, #9100, #95684, #44991, #96570, #86888, #69089, #35691, #52336, #43773, #48496, #78651, #85274, #60308, #52779, #22692, #95555, #61624, #86665, #74141, #54462, #68930, #24036, #50462, #9162, #34159, #19454, #62751, #11629, #24299, #1659, #20860, #73690, #42088, #66593, #7678, #20321, #34410, #2512, #60537, #25378, #97599, #22114, #61514, #75306, #81636, #63469, #22052, #34075, #28793, #78509, #94625, #2020, #69747, #2667, #21027, #78060, #5961, #18247, #12364, #4118, #55049, #12543, #15209, #56504, #39945, #17456, #72474, #85751, #92751, #98250, #89685, #81900, #47119, #90138, #11828, #28796, #51167, #64394, #14379, #57614, #57351, #79016, #5708, #83777, #13368, #21572, #1861, #29142, #86150, #8772, #55246, #65088, #17562, #5824, #80586, #65495, #77515, #60063, #72384, #1310, #34827, #36760, #7715, #17547, #46241, #79468, #31755, #73752, #47638, #52370, #94700, #10261, #7584, #8276, #30636, #33750, #29011, #77808, #9728, #91162, #80783, #35046, #72931, #9561, #97955, #55025, #33634, #11708, #53032, #93390, #29533, #54705, #64175, #22080, #3193, #13968, #47640, #85899, #6700, #27551, #23991, #51151, #56017, #93, #61869, #68036, #34858, #81118, #6147, #64200, #4343, #9757, #6593, #31561, #54648, #10168, #32147, #84907, #1802, #98711, #77365, #50840, #623, #6520, #76575, #5224, #63490, #67408, #66718, #82581, #36786, #59024, #63077, #48018, #85979, #34452, #10612, #98191, #95105, #33613, #38759, #60413, #75636, #37599, #31663, #47502, #56469, #44268, #9965, #62132, #57440 ) ) ;
#92279 = EDGE_CURVE ( 'NONE', #15047, #25147, #65873, .T. ) ;
#92280 = FILL_AREA_STYLE_COLOUR ( '', #12520 ) ;
#92281 = VERTEX_POINT ( 'NONE', #83353 ) ;
#92282 = CARTESIAN_POINT ( 'NONE',  ( 0.6178305044545818747, 23.49863466993041783, -9.382169495545419124 ) ) ;
#92283 = CARTESIAN_POINT ( 'NONE',  ( 0.1532563361054100626, 10.80059781766745175, -2.638427012816831230 ) ) ;
#92284 = CARTESIAN_POINT ( 'NONE',  ( 13.99999999999999822, 60.50000000000000000, 6.500000000000000888 ) ) ;
#92285 = CARTESIAN_POINT ( 'NONE',  ( 0.1532563361054100626, 10.80059781766745175, -2.638427012816831230 ) ) ;
#92286 = CARTESIAN_POINT ( 'NONE',  ( 20.88017736071110519, 35.56368534415484106, 2.639326808657452039E-16 ) ) ;
#92287 = ORIENTED_EDGE ( 'NONE', *, *, #43046, .F. ) ;
#92288 = CARTESIAN_POINT ( 'NONE',  ( -1.099225684535947600, 64.54030133659709634, 6.408140936763237150 ) ) ;
#92289 = CARTESIAN_POINT ( 'NONE',  ( 12.91533473730993009, 51.60535201082149825, -10.88017736071109987 ) ) ;
#92290 = CYLINDRICAL_SURFACE ( 'NONE', #32402, 0.1000000000000001166 ) ;
#92291 =( NAMED_UNIT ( * ) SI_UNIT ( $, .STERADIAN. ) SOLID_ANGLE_UNIT ( ) );
#92292 = CARTESIAN_POINT ( 'NONE',  ( 15.44008868035555793, 61.39701867748817676, -9.422509992056140149 ) ) ;
#92293 = CARTESIAN_POINT ( 'NONE',  ( 7.361572987183169658, 64.96726448433412315, -9.846743663894592657 ) ) ;
#92294 = CARTESIAN_POINT ( 'NONE',  ( 3.469446951953614189E-15, 11.36803362898265135, 11.25000000000000178 ) ) ;
#92295 = CARTESIAN_POINT ( 'NONE',  ( 7.361572987183169658, 24.96726448433412315, -9.846743663894592657 ) ) ;
#92296 = CARTESIAN_POINT ( 'NONE',  ( 3.591859063236763294, 53.29030133659708923, -11.09922568453595026 ) ) ;
#92297 = CARTESIAN_POINT ( 'NONE',  ( 0.000000000000000000, 76.90945382226833260, 7.553580139337960908 ) ) ;
#92298 = CARTESIAN_POINT ( 'NONE',  ( 14.92337183194729988, 24.34226448433411960, -8.527530157486177487 ) ) ;
#92299 = CARTESIAN_POINT ( 'NONE',  ( 22.81628187352648496, 16.83196800326374998, -3.434112377981050290 ) ) ;
#92300 = CARTESIAN_POINT ( 'NONE',  ( -4.261098214579363663, -13.83547760778420077, -2.749999999999999556 ) ) ;
#92301 = CARTESIAN_POINT ( 'NONE',  ( 10.00000000000000178, 54.31368534415484106, 10.88017736071110342 ) ) ;
#92302 = CARTESIAN_POINT ( 'NONE',  ( 17.20831665107776587, 64.13393115100079456, -7.208316651077762316 ) ) ;
#92303 = DIRECTION ( 'NONE',  ( 0.000000000000000000, 0.000000000000000000, 1.000000000000000000 ) ) ;
#92304 = CARTESIAN_POINT ( 'NONE',  ( 7.361572987183169658, 24.96726448433412315, -9.846743663894592657 ) ) ;
#92305 = CARTESIAN_POINT ( 'NONE',  ( 12.63842701281683922, 14.55059781766744997, -9.846743663894590881 ) ) ;
#92306 = CARTESIAN_POINT ( 'NONE',  ( 19.42250999205614193, 10.14701867748816966, 5.440088680355555262 ) ) ;
#92307 = CARTESIAN_POINT ( 'NONE',  ( 22.81628187352647785, 16.62363466993042138, 6.195893100308588602E-16 ) ) ;
#92308 =( LENGTH_UNIT ( ) NAMED_UNIT ( * ) SI_UNIT ( .MILLI., .METRE. ) );
#92309 = CARTESIAN_POINT ( 'NONE',  ( 7.361572987183170547, 67.05059781766746596, 9.846743663894590881 ) ) ;
#92310 = CARTESIAN_POINT ( 'NONE',  ( 4.655929185074548116, -8.243906417136569686, -2.749999999999999556 ) ) ;
#92311 = CARTESIAN_POINT ( 'NONE',  ( 20.88017736071110164, 25.35535201082150891, 2.915334737309930979 ) ) ;
#92312 = CARTESIAN_POINT ( 'NONE',  ( 6.579634127946655475, -87.99828267815715321, -3.750000000000000000 ) ) ;
#92313 = CARTESIAN_POINT ( 'NONE',  ( 0.5774900079438607392, 18.48035201082150536, 5.440088680355550821 ) ) ;
#92314 = LINE ( 'NONE', #38345, #35962 ) ;
#92315 = CARTESIAN_POINT ( 'NONE',  ( 2.035157376598824452, 28.68868534415484106, 7.964842623401179544 ) ) ;
#92316 = AXIS2_PLACEMENT_3D ( 'NONE', #62154, #92660, #60687 ) ;
#92318 = DIRECTION ( 'NONE',  ( -0.06975647374412512203, -0.9975640502598241977, 0.000000000000000000 ) ) ;
#92317 = CARTESIAN_POINT ( 'NONE',  ( 17.96484262340118221, 4.938685344154837509, 7.964842623401181321 ) ) ;
#92319 = CARTESIAN_POINT ( 'NONE',  ( 14.92337183194729633, 2.675597817667451750, 8.527530157486181039 ) ) ;
#92320 = CARTESIAN_POINT ( 'NONE',  ( 14.92337183194729988, 29.34226448433411960, -8.527530157486177487 ) ) ;
#92321 = CARTESIAN_POINT ( 'NONE',  ( 13.43411237798106583, 12.66530133659708746, -12.81628187352647252 ) ) ;
#92322 = CARTESIAN_POINT ( 'NONE',  ( 18.00000000000000000, 77.62866902037677619, -4.012032253954680883 ) ) ;
#92323 = DIRECTION ( 'NONE',  ( -0.06104853953484969814, 0.000000000000000000, -0.9981347984218674751 ) ) ;
#92324 = EDGE_CURVE ( 'NONE', #65307, #80133, #66868, .T. ) ;
#92325 = CARTESIAN_POINT ( 'NONE',  ( 12.63842701281683034, 62.46726448433410894, 9.846743663894596210 ) ) ;
#92327 = CARTESIAN_POINT ( 'NONE',  ( -12.74305857943740428, -2.641472246012534819E-15, -7.177950183687037189 ) ) ;
#92326 = VECTOR ( 'NONE', #27293, 1000.000000000000000 ) ;
#92328 = CARTESIAN_POINT ( 'NONE',  ( -2.266590686148945544, 11.38708216824730179, -7.082119434687050408 ) ) ;
#92329 = B_SPLINE_CURVE_WITH_KNOTS ( 'NONE', 3,
 ( #16931, #70426, #71885, #47409 ),
 .UNSPECIFIED., .F., .F.,
 ( 4, 4 ),
 ( 3.469446951953613804E-18, 0.0001414015891011769215 ),
 .UNSPECIFIED. ) ;
#92330 = CARTESIAN_POINT ( 'NONE',  ( 17.20831665107776587, 39.13393115100079456, -7.208316651077762316 ) ) ;
#92331 = DIRECTION ( 'NONE',  ( -1.000000000000000000, 0.000000000000000000, 0.000000000000000000 ) ) ;
#92332 = ORIENTED_EDGE ( 'NONE', *, *, #52334, .F. ) ;
#92333 = CARTESIAN_POINT ( 'NONE',  ( 17.08211943468705840, 55.13708216824731068, -12.26659068614894466 ) ) ;
#92334 = CARTESIAN_POINT ( 'NONE',  ( 5.076628168052703671, 26.84226448433411960, 8.527530157486179263 ) ) ;
#92336 = CARTESIAN_POINT ( 'NONE',  ( -0.1503990784575328643, 25.12777174578613426, 6.262539305110068177 ) ) ;
#92335 = CARTESIAN_POINT ( 'NONE',  ( 0.000000000000000000, 0.5000000000000004441, 0.000000000000000000 ) ) ;
#92337 = CARTESIAN_POINT ( 'NONE',  ( 12.91533473730993009, 46.60535201082150536, -10.88017736071109987 ) ) ;
#92338 = CARTESIAN_POINT ( 'NONE',  ( 13.43411237798105340, 45.58196800326374643, 12.81628187352647963 ) ) ;
#92339 = CARTESIAN_POINT ( 'NONE',  ( 0.5774900079438590739, 17.64701867748817321, -5.440088680355550821 ) ) ;
#92340 = CARTESIAN_POINT ( 'NONE',  ( 10.00000000000000000, 52.87363466993041783, -12.81628187352647608 ) ) ;
#92341 = CARTESIAN_POINT ( 'NONE',  ( -1.099225684535947600, -1.293031996736246469, -6.408140936763238038 ) ) ;
#92342 = ORIENTED_EDGE ( 'NONE', *, *, #79976, .T. ) ;
#92343 = CARTESIAN_POINT ( 'NONE',  ( -2.913501739333859586, 15.00000000000000000, 14.20427779279530434 ) ) ;
#92344 = CARTESIAN_POINT ( 'NONE',  ( -8.647966315259102643, -15.58183027063508952, -3.999999999999999112 ) ) ;
#92345 = CARTESIAN_POINT ( 'NONE',  ( 13.79529636645031943, 60.34541550158063927, -14.16423886937409904 ) ) ;
#92346 = CARTESIAN_POINT ( 'NONE',  ( 2.917880565312948704, 7.637082168247301794, 12.26659068614894643 ) ) ;
#92347 = CARTESIAN_POINT ( 'NONE',  ( 19.42250999205614548, 15.98035201082150714, -5.440088680355545492 ) ) ;
#92348 = CARTESIAN_POINT ( 'NONE',  ( 20.88017736071110519, 35.56368534415484106, 2.639326808657452039E-16 ) ) ;
#92349 = DIRECTION ( 'NONE',  ( -0.000000000000000000, -1.000000000000000000, -0.000000000000000000 ) ) ;
#92350 = DIRECTION ( 'NONE',  ( -1.000000000000000000, 0.000000000000000000, 0.000000000000000000 ) ) ;
#92351 = CARTESIAN_POINT ( 'NONE',  ( 12.91533473730993009, 61.60535201082150536, -10.88017736071109987 ) ) ;
#92352 = CARTESIAN_POINT ( 'NONE',  ( 12.91533473730993009, 61.60535201082150536, -10.88017736071109987 ) ) ;
#92353 = CARTESIAN_POINT ( 'NONE',  ( 22.81628187352647785, 31.41530133659709279, 3.434112377981063169 ) ) ;
#92354 = DIRECTION ( 'NONE',  ( -0.000000000000000000, -0.000000000000000000, -1.000000000000000000 ) ) ;
#92355 =( NAMED_UNIT ( * ) SI_UNIT ( $, .STERADIAN. ) SOLID_ANGLE_UNIT ( ) );
#92356 = CARTESIAN_POINT ( 'NONE',  ( 7.361572987183169658, 4.967264484334119601, -9.846743663894592657 ) ) ;
#92357 = CARTESIAN_POINT ( 'NONE',  ( 2.791683348922237240, 30.38393115100078390, -7.208316651077763204 ) ) ;
#92358 = CARTESIAN_POINT ( 'NONE',  ( 4.559911319644449179, 17.23035201082150536, -9.422509992056141925 ) ) ;
#92359 = ADVANCED_FACE ( 'NONE', ( #27877 ), #59852, .T. ) ;
#92360 = CARTESIAN_POINT ( 'NONE',  ( 21.09922568453594849, 26.20696800326375353, 6.408140936763242479 ) ) ;
#92361 = CARTESIAN_POINT ( 'NONE',  ( 2.791683348922237240, 5.383931151000785675, -7.208316651077763204 ) ) ;
#92362 = CARTESIAN_POINT ( 'NONE',  ( 19.72487221294571569, 54.78217586085238366, 6.499999999999995559 ) ) ;
#92363 = CARTESIAN_POINT ( 'NONE',  ( 19.84674366389459621, 58.50893115100078745, 7.409399052514197653E-17 ) ) ;
#92364 = CARTESIAN_POINT ( 'NONE',  ( 0.1532563361054082862, 31.21726448433412315, 2.638427012816831674 ) ) ;
#92365 = EDGE_CURVE ( 'NONE', #70878, #94114, #35383, .T. ) ;
#92366 = CARTESIAN_POINT ( 'NONE',  ( 10.00000000000000178, 18.05374883491396787, 14.16423886937410082 ) ) ;
#92367 = CARTESIAN_POINT ( 'NONE',  ( -0.8801773607110991993, 37.85535201082151247, -2.915334737309923874 ) ) ;
#92368 = CARTESIAN_POINT ( 'NONE',  ( 0.5774900079438607392, 13.48035201082150358, 5.440088680355550821 ) ) ;
#92369 = CARTESIAN_POINT ( 'NONE',  ( 20.88017736071110519, 50.56368534415484106, 2.639326808657452039E-16 ) ) ;
#92370 = CARTESIAN_POINT ( 'NONE',  ( 7.084665262690076126, 32.02201867748816966, -10.88017736071110164 ) ) ;
#92371 = VERTEX_POINT ( 'NONE', #66364 ) ;
#92372 = CARTESIAN_POINT ( 'NONE',  ( 22.81628187352647785, 31.41530133659709279, 3.434112377981063169 ) ) ;
#92373 = CARTESIAN_POINT ( 'NONE',  ( 7.084665262690076126, 39.10535201082150536, 10.88017736071109987 ) ) ;
#92374 = ORIENTED_EDGE ( 'NONE', *, *, #36578, .T. ) ;
#92375 = CYLINDRICAL_SURFACE ( 'NONE', #53795, 11.25000000000000178 ) ;
#92376 = CARTESIAN_POINT ( 'NONE',  ( 20.88017736071110875, 50.77201867748817676, -2.915334737309920765 ) ) ;
#92377 = VERTEX_POINT ( 'NONE', #28853 ) ;
#92378 = CARTESIAN_POINT ( 'NONE',  ( 2.035157376598822676, 47.43868534415484817, -7.964842623401177768 ) ) ;
#92379 = CARTESIAN_POINT ( 'NONE',  ( 5.930070213854097716, -28.64748318935870941, 4.000000000000000000 ) ) ;
#92380 = CARTESIAN_POINT ( 'NONE',  ( -14.42525372082707236, 14.76984920709440452, -3.890283033989385242 ) ) ;
#92381 = CARTESIAN_POINT ( 'NONE',  ( -4.164238869374098151, 56.59541550158063927, -3.795296366450310543 ) ) ;
#92382 = CARTESIAN_POINT ( 'NONE',  ( 20.88017736071110519, 65.56368534415483396, 2.639326808657452039E-16 ) ) ;
#92383 = CARTESIAN_POINT ( 'NONE',  ( 69.60148758828984228, 0.4999999999999958922, -9.500000000000000000 ) ) ;
#92384 = CARTESIAN_POINT ( 'NONE',  ( 9.997910040112534702, 4.470079180682592273E-16, 10.50199004140724490 ) ) ;
#92385 = CARTESIAN_POINT ( 'NONE',  ( 0.5774900079438590739, 2.647018677488170990, -5.440088680355550821 ) ) ;
#92386 = CARTESIAN_POINT ( 'NONE',  ( 18.52753015748618282, 28.92559781766745175, -4.923371831947291888 ) ) ;
#92387 = B_SPLINE_CURVE_WITH_KNOTS ( 'NONE', 3,
 ( #23984, #2481, #93942, #85460 ),
 .UNSPECIFIED., .F., .F.,
 ( 4, 4 ),
 ( 1.778362592763157239E-16, 0.001060528352561988102 ),
 .UNSPECIFIED. ) ;
#92388 = ORIENTED_EDGE ( 'NONE', *, *, #53885, .F. ) ;
#92389 = CARTESIAN_POINT ( 'NONE',  ( 14.92337183194729988, 39.34226448433412315, -8.527530157486177487 ) ) ;
#92390 = CARTESIAN_POINT ( 'NONE',  ( 19.42250999205614548, 40.98035201082150536, -5.440088680355545492 ) ) ;
#92391 = CARTESIAN_POINT ( 'NONE',  ( 10.00000000000000000, 39.75893115100078745, -9.846743663894594434 ) ) ;
#92392 = CARTESIAN_POINT ( 'NONE',  ( 22.81628187352647785, 16.62363466993042138, 6.195893100308588602E-16 ) ) ;
#92394 = CARTESIAN_POINT ( 'NONE',  ( 7.347880794884118750E-16, 17.03999999999999915, 0.000000000000000000 ) ) ;
#92393 = CARTESIAN_POINT ( 'NONE',  ( -1.548803529118062405, 0.000000000000000000, 5.228673087012083442 ) ) ;
#92395 = CARTESIAN_POINT ( 'NONE',  ( -0.8801773607111008646, 43.27201867748817676, 2.915334737309923430 ) ) ;
#92396 = CARTESIAN_POINT ( 'NONE',  ( -2.266590686148945544, 52.22041550158064638, 7.082119434687048631 ) ) ;
#92397 = EDGE_CURVE ( 'NONE', #25626, #69208, #69071, .T. ) ;
#92398 = AXIS2_PLACEMENT_3D ( 'NONE', #28063, #12574, #27075 ) ;
#92399 = AXIS2_PLACEMENT_3D ( 'NONE', #41762, #73212, #12224 ) ;
#92400 = CARTESIAN_POINT ( 'NONE',  ( 6.565887622018943937, 23.08196800326375708, -12.81628187352647608 ) ) ;
#92401 = CARTESIAN_POINT ( 'NONE',  ( -8.024359497401761132, 75.03672218798435267, 2.900000000000000355 ) ) ;
#92402 = VERTEX_POINT ( 'NONE', #90342 ) ;
#92403 = CARTESIAN_POINT ( 'NONE',  ( 6.565887622018943937, 28.08196800326375353, -12.81628187352647608 ) ) ;
#92404 = CARTESIAN_POINT ( 'NONE',  ( 4.559911319644449179, 23.89701867748817321, 9.422509992056141925 ) ) ;
#92405 = CARTESIAN_POINT ( 'NONE',  ( 12.91533473730993009, 56.60535201082151247, -10.88017736071109987 ) ) ;
#92406 = EDGE_LOOP ( 'NONE', ( #45658, #92762, #51665, #35999 ) ) ;
#92407 = DIRECTION ( 'NONE',  ( -0.000000000000000000, -0.000000000000000000, -1.000000000000000000 ) ) ;
#92408 = VECTOR ( 'NONE', #43704, 1000.000000000000000 ) ;
#92409 = CARTESIAN_POINT ( 'NONE',  ( 0.1532563361054082862, 6.217264484334118713, 2.638427012816831674 ) ) ;
#92410 = CARTESIAN_POINT ( 'NONE',  ( 14.92337183194729633, 52.67559781766745175, 8.527530157486181039 ) ) ;
#92411 = CARTESIAN_POINT ( 'NONE',  ( 5.076628168052704559, 35.17559781766745175, -8.527530157486179263 ) ) ;
#92412 = CARTESIAN_POINT ( 'NONE',  ( -1.915564264621532287, 4.395349792408769378E-16, 14.37291249357989287 ) ) ;
#92413 = CARTESIAN_POINT ( 'NONE',  ( 10.00000000000000178, 32.25893115100078745, 9.846743663894594434 ) ) ;
#92414 = CARTESIAN_POINT ( 'NONE',  ( 19.80832241502127644, 54.75868815902071418, 6.499999999999992895 ) ) ;
#92415 = DIRECTION ( 'NONE',  ( 1.000000000000000000, 0.000000000000000000, 0.000000000000000000 ) ) ;
#92417 = CARTESIAN_POINT ( 'NONE',  ( 15.00000000000000000, 77.07179676972447169, -4.250000000000000000 ) ) ;
#92416 = CARTESIAN_POINT ( 'NONE',  ( 19.84674366389459266, 13.30059781766745353, 2.638427012816836559 ) ) ;
#92418 = CARTESIAN_POINT ( 'NONE',  ( 0.000000000000000000, 69.50000000000000000, -6.500000000000000888 ) ) ;
#92420 = ORIENTED_EDGE ( 'NONE', *, *, #82772, .F. ) ;
#92419 = CARTESIAN_POINT ( 'NONE',  ( 14.92337183194729633, 47.67559781766745175, 8.527530157486181039 ) ) ;
#92421 = CARTESIAN_POINT ( 'NONE',  ( 20.15039907845753220, 17.62777174578612716, -6.262539305110077947 ) ) ;
#92422 = CARTESIAN_POINT ( 'NONE',  ( -2.816281873526473856, 14.33196800326375531, 3.434112377981055619 ) ) ;
#92423 = CARTESIAN_POINT ( 'NONE',  ( 2.035157376598822676, 57.43868534415484106, -7.964842623401177768 ) ) ;
#92424 = CARTESIAN_POINT ( 'NONE',  ( 10.00000000000000178, 48.05374883491396787, 14.16423886937410082 ) ) ;
#92425 = CARTESIAN_POINT ( 'NONE',  ( -7.154372922009654800, 15.00000000000000000, 14.30707323420372035 ) ) ;
#92426 = CARTESIAN_POINT ( 'NONE',  ( 20.36894250292379382, 43.67874883491397497, 10.36894250292379205 ) ) ;
#92427 = CARTESIAN_POINT ( 'NONE',  ( 24.16423886937410614, 54.30374883491396787, 8.672049930838204340E-16 ) ) ;
#92428 = CARTESIAN_POINT ( 'NONE',  ( 24.16423886937410614, 19.51208216824729647, -3.795296366450302550 ) ) ;
#92430 = DIRECTION ( 'NONE',  ( 0.000000000000000000, 0.000000000000000000, -1.000000000000000000 ) ) ;
#92429 = CARTESIAN_POINT ( 'NONE',  ( -2.266590686148945544, 26.38708216824730357, -7.082119434687050408 ) ) ;
#92431 = CARTESIAN_POINT ( 'NONE',  ( -3.866352809136022195, 14.95037102884348634, -14.23757791217075308 ) ) ;
#92433 = CARTESIAN_POINT ( 'NONE',  ( 0.1532563361054083140, 36.00893115100078745, 1.131784320476157264E-15 ) ) ;
#92432 = CARTESIAN_POINT ( 'NONE',  ( 4.145754220390653444, -0.8370734722285972929, 2.500000000000000000 ) ) ;
#92434 = CARTESIAN_POINT ( 'NONE',  ( 0.5774900079438607392, 18.48035201082150536, 5.440088680355550821 ) ) ;
#92435 = CARTESIAN_POINT ( 'NONE',  ( 0.000000000000000000, 15.00000000000000000, 0.000000000000000000 ) ) ;
#92436 = CARTESIAN_POINT ( 'NONE',  ( 18.00000000000001776, 4.625929269271493211E-15, -6.250000000000000000 ) ) ;
#92437 = CARTESIAN_POINT ( 'NONE',  ( 19.67387888393821527, 90.60653825729899324, -5.439610960094903191 ) ) ;
#92438 = EDGE_CURVE ( 'NONE', #93321, #61288, #64258, .T. ) ;
#92439 = CARTESIAN_POINT ( 'NONE',  ( 14.92337183194729633, 42.67559781766745886, 8.527530157486181039 ) ) ;
#92440 = CARTESIAN_POINT ( 'NONE',  ( 6.565887622018943937, 55.16530133659709634, 12.81628187352647430 ) ) ;
#92441 = CARTESIAN_POINT ( 'NONE',  ( 7.082119434687047743, -4.862917831752689324, -12.26659068614894821 ) ) ;
#92442 = CARTESIAN_POINT ( 'NONE',  ( 12.63842701281683922, 39.55059781766744464, -9.846743663894590881 ) ) ;
#92443 = CARTESIAN_POINT ( 'NONE',  ( 19.84674366389459621, 58.50893115100078745, 7.409399052514197653E-17 ) ) ;
#92444 = CARTESIAN_POINT ( 'NONE',  ( 10.00000000000000000, 45.55374883491397497, -14.16423886937410082 ) ) ;
#92445 = VERTEX_POINT ( 'NONE', #81376 ) ;
#92446 = CARTESIAN_POINT ( 'NONE',  ( 24.16423886937409904, 19.09541550158063927, 3.795296366450317205 ) ) ;
#92447 = DIRECTION ( 'NONE',  ( -0.000000000000000000, -1.000000000000000000, -0.000000000000000000 ) ) ;
#92449 = DIRECTION ( 'NONE',  ( -0.6225146366376130835, 0.000000000000000000, -0.7826081568524191345 ) ) ;
#92448 = DIRECTION ( 'NONE',  ( 0.000000000000000000, -1.000000000000000000, 0.000000000000000000 ) ) ;
#92450 = CARTESIAN_POINT ( 'NONE',  ( 2.035157376598822676, 7.438685344154837509, -7.964842623401177768 ) ) ;
#92451 = CARTESIAN_POINT ( 'NONE',  ( -2.816281873526473856, 9.123634669930421381, 9.499525473075851096E-16 ) ) ;
#92452 = CARTESIAN_POINT ( 'NONE',  ( 17.96484262340118221, 66.18868534415483396, -7.964842623401177768 ) ) ;
#92453 = LINE ( 'NONE', #23979, #64542 ) ;
#92454 = CARTESIAN_POINT ( 'NONE',  ( 2.393480905993088381, 14.49999999999999112, 14.80781041047758784 ) ) ;
#92455 = CARTESIAN_POINT ( 'NONE',  ( -0.3689425029237898834, 66.17874883491396076, -10.36894250292378850 ) ) ;
#92456 = CARTESIAN_POINT ( 'NONE',  ( -12.83294900548068895, 15.00000000000000000, 7.766300266068274283 ) ) ;
#92457 = CARTESIAN_POINT ( 'NONE',  ( -0.8801773607111009756, 28.06368534415484106, 1.068504757029289695E-15 ) ) ;
#92458 = CARTESIAN_POINT ( 'NONE',  ( 12.91533473730993009, 21.60535201082150536, -10.88017736071109987 ) ) ;
#92459 = CARTESIAN_POINT ( 'NONE',  ( 1.472469842513823179, 51.42559781766745886, 4.923371831947296329 ) ) ;
#92460 = CARTESIAN_POINT ( 'NONE',  ( 18.52753015748618282, 48.92559781766745886, -4.923371831947291888 ) ) ;
#92461 = CARTESIAN_POINT ( 'NONE',  ( -2.816281873526473856, 64.33196800326376774, 3.434112377981055619 ) ) ;
#92462 = DIRECTION ( 'NONE',  ( 0.1736481776669282773, -0.9848077530122084644, 0.000000000000000000 ) ) ;
#92463 = VERTEX_POINT ( 'NONE', #98387 ) ;
#92464 = VECTOR ( 'NONE', #44050, 1000.000000000000000 ) ;
#92465 = CARTESIAN_POINT ( 'NONE',  ( 0.5774900079438607392, 33.48035201082150536, 5.440088680355550821 ) ) ;
#92466 = CARTESIAN_POINT ( 'NONE',  ( 22.81628187352648496, 21.83196800326374643, -3.434112377981050290 ) ) ;
#92467 = CARTESIAN_POINT ( 'NONE',  ( 2.059615949176877749E-15, 71.60587665882023600, 5.000000000000000000 ) ) ;
#92468 = MECHANICAL_DESIGN_GEOMETRIC_PRESENTATION_REPRESENTATION (  '', ( #31790 ), #6254 ) ;
#92469 = ADVANCED_FACE ( 'NONE', ( #60348 ), #63643, .T. ) ;
#92470 = CARTESIAN_POINT ( 'NONE',  ( 1.472469842513823179, 60.59226448433412315, -4.923371831947296329 ) ) ;
#92471 = CARTESIAN_POINT ( 'NONE',  ( 19.42250999205614193, 50.14701867748817676, 5.440088680355555262 ) ) ;
#92472 = CARTESIAN_POINT ( 'NONE',  ( 22.81628187352647785, 16.41530133659708923, 3.434112377981063169 ) ) ;
#92474 = LINE ( 'NONE', #15998, #43216 ) ;
#92473 = CARTESIAN_POINT ( 'NONE',  ( 15.44008868035555793, 61.39701867748817676, -9.422509992056140149 ) ) ;
#92475 = CARTESIAN_POINT ( 'NONE',  ( 10.70613742633251420, 4.218616272510096815E-16, 9.778988772285311271 ) ) ;
#92476 = ORIENTED_EDGE ( 'NONE', *, *, #41817, .F. ) ;
#92477 = DIRECTION ( 'NONE',  ( -0.000000000000000000, -1.000000000000000000, -0.000000000000000000 ) ) ;
#92478 = EDGE_CURVE ( 'NONE', #78529, #3611, #91734, .T. ) ;
#92479 = CARTESIAN_POINT ( 'NONE',  ( 2.035157376598822676, 47.43868534415484817, -7.964842623401177768 ) ) ;
#92481 = CARTESIAN_POINT ( 'NONE',  ( 17.08211943468705840, 20.13708216824730357, -12.26659068614894466 ) ) ;
#92480 = CARTESIAN_POINT ( 'NONE',  ( 16.40814093676323893, 40.79030133659708923, 11.09922568453595026 ) ) ;
#92482 = CARTESIAN_POINT ( 'NONE',  ( 0.1532563361054082862, 61.21726448433412315, 2.638427012816831674 ) ) ;
#92483 = CARTESIAN_POINT ( 'NONE',  ( 2.791683348922237240, 25.38393115100078390, -7.208316651077763204 ) ) ;
#92484 = DIRECTION ( 'NONE',  ( -1.000000000000000000, 0.000000000000000000, 0.000000000000000000 ) ) ;
#92485 = CARTESIAN_POINT ( 'NONE',  ( 10.00000000000000178, 63.05374883491396076, 14.16423886937410082 ) ) ;
#92486 = ORIENTED_EDGE ( 'NONE', *, *, #54653, .F. ) ;
#92487 =( BOUNDED_CURVE ( )  B_SPLINE_CURVE ( 2, ( #79951, #41489, #71488, #72438, #58418, #26947, #95456, #4467, #57448 ),
 .UNSPECIFIED., .F., .T. ) 
 B_SPLINE_CURVE_WITH_KNOTS ( ( 3, 2, 2, 2, 3 ),
 ( 0.5472837940830884707, 0.5476190476190476719, 0.5535714285714286031, 0.5595238095238095344, 0.5598590630597686246 ),
 .UNSPECIFIED. ) 
 CURVE ( )  GEOMETRIC_REPRESENTATION_ITEM ( )  RATIONAL_B_SPLINE_CURVE ( ( 0.9963778908391753841, 0.9980808541467917072, 1.000000000000000000, 0.9659258262890683122, 1.000000000000000000, 0.9659258262890683122, 1.000000000000000000, 0.9980808541467922623, 0.9963778908391764944 ) ) 
 REPRESENTATION_ITEM ( '' )  );
#92488 = CARTESIAN_POINT ( 'NONE',  ( 20.88017736071110164, 5.355352010821502695, 2.915334737309930979 ) ) ;
#92489 = CARTESIAN_POINT ( 'NONE',  ( 0.5774900079438607392, 8.480352010821505360, 5.440088680355550821 ) ) ;
#92490 = CARTESIAN_POINT ( 'NONE',  ( 5.038135815954128738, 0.000000000000000000, 2.086864184045826853 ) ) ;
#92491 =( BOUNDED_SURFACE ( )  B_SPLINE_SURFACE ( 3, 2, ( 
 ( #83253, #14776, #38257 ),
 ( #45248, #75744, #53243 ),
 ( #767, #60250, #68264 ),
 ( #75251, #76729, #7266 ),
 ( #84256, #82252, #38746 ),
 ( #21778, #68749, #281 ),
 ( #89755, #37277, #44748 ),
 ( #15759, #90247, #37768 ),
 ( #6764, #59751, #91742 ),
 ( #46243, #98784, #52257 ),
 ( #76249, #21272, #30728 ),
 ( #22762, #30232, #29254 ),
 ( #51768, #13768, #44255 ),
 ( #61235, #60736, #14275 ),
 ( #91238, #67766, #83748 ),
 ( #15271, #45752, #22271 ),
 ( #98286, #23262, #53737 ),
 ( #74759, #6267, #36772 ),
 ( #67264, #97792, #29740 ),
 ( #90743, #55203, #39732 ),
 ( #69732, #16731, #25714 ),
 ( #2733, #78707, #70226 ),
 ( #24240, #41216, #85717 ),
 ( #3206, #17232, #54218 ),
 ( #9221, #18206, #10702 ),
 ( #31713, #47709, #56207 ) ),
 .UNSPECIFIED., .F., .F., .F. ) 
 B_SPLINE_SURFACE_WITH_KNOTS ( ( 4, 2, 2, 2, 2, 2, 2, 2, 2, 2, 2, 2, 4 ),
 ( 3, 3 ),
 ( 0.000000000000000000, 0.001549856543994699394, 0.003099713087989398787, 0.006199426175978797575, 0.01239885235195759515, 0.02479770470391519030, 0.03719655705587278371, 0.04959540940783038060, 0.07439311411174556743, 0.08679196646370315738, 0.09299139263968195235, 0.09609110572767134983, 0.09919081881566076120 ),
 ( 0.000000000000000000, 1.000000000000000000 ),
 .UNSPECIFIED. ) 
 GEOMETRIC_REPRESENTATION_ITEM ( )  RATIONAL_B_SPLINE_SURFACE ( (
 ( 1.000000000000000000, 0.7071067811865475727, 1.000000000000000000),
 ( 1.000000000000000000, 0.7071067811865475727, 1.000000000000000000),
 ( 1.000000000000000000, 0.7071067811865475727, 1.000000000000000000),
 ( 1.000000000000000000, 0.7071067811865475727, 1.000000000000000000),
 ( 1.000000000000000000, 0.7071067811865475727, 1.000000000000000000),
 ( 1.000000000000000000, 0.7071067811865475727, 1.000000000000000000),
 ( 1.000000000000000000, 0.7071067811865475727, 1.000000000000000000),
 ( 1.000000000000000000, 0.7071067811865475727, 1.000000000000000000),
 ( 1.000000000000000000, 0.7071067811865475727, 1.000000000000000000),
 ( 1.000000000000000000, 0.7071067811865475727, 1.000000000000000000),
 ( 1.000000000000000000, 0.7071067811865475727, 1.000000000000000000),
 ( 1.000000000000000000, 0.7071067811865475727, 1.000000000000000000),
 ( 1.000000000000000000, 0.7071067811865475727, 1.000000000000000000),
 ( 1.000000000000000000, 0.7071067811865475727, 1.000000000000000000),
 ( 1.000000000000000000, 0.7071067811865496822, 1.000000000000000000),
 ( 1.000000000000000000, 0.7071067811865496822, 1.000000000000000000),
 ( 1.000000000000000000, 0.7071067811865475727, 1.000000000000000000),
 ( 1.000000000000000000, 0.7071067811865475727, 1.000000000000000000),
 ( 1.000000000000000000, 0.7071067811865475727, 1.000000000000000000),
 ( 1.000000000000000000, 0.7071067811865475727, 1.000000000000000000),
 ( 1.000000000000000000, 0.7071067811865475727, 1.000000000000000000),
 ( 1.000000000000000000, 0.7071067811865475727, 1.000000000000000000),
 ( 1.000000000000000000, 0.7071067811865475727, 1.000000000000000000),
 ( 1.000000000000000000, 0.7071067811865475727, 1.000000000000000000),
 ( 1.000000000000000000, 0.7071067811865475727, 1.000000000000000000),
 ( 1.000000000000000000, 0.7071067811865475727, 1.000000000000000000) ) ) 
 REPRESENTATION_ITEM ( '' )  SURFACE ( )  );
#92492 = ORIENTED_EDGE ( 'NONE', *, *, #2301, .F. ) ;
#92493 = CARTESIAN_POINT ( 'NONE',  ( 7.084665262690076126, 9.105352010821503583, 10.88017736071109987 ) ) ;
#92494 = CARTESIAN_POINT ( 'NONE',  ( 20.88017736071110164, 5.355352010821503583, 2.915334737309930979 ) ) ;
#92495 = CARTESIAN_POINT ( 'NONE',  ( 0.1532563361054082862, 41.21726448433411605, 2.638427012816831674 ) ) ;
#92496 = CARTESIAN_POINT ( 'NONE',  ( 10.00000000000000000, 42.87363466993042493, -12.81628187352647608 ) ) ;
#92498 = CARTESIAN_POINT ( 'NONE',  ( -4.164238869374098151, 26.59541550158063217, -3.795296366450310543 ) ) ;
#92497 = CARTESIAN_POINT ( 'NONE',  ( 0.9940297508537879745, 0.000000000000000000, -14.21528771620249820 ) ) ;
#92499 = CARTESIAN_POINT ( 'NONE',  ( -0.8801773607111009756, 28.06368534415484106, 1.068504757029289695E-15 ) ) ;
#92500 = CARTESIAN_POINT ( 'NONE',  ( 17.96484262340118221, 6.188685344154837509, -7.964842623401177768 ) ) ;
#92501 = CARTESIAN_POINT ( 'NONE',  ( 19.84674366389459266, 38.71726448433412315, -2.638427012816827677 ) ) ;
#92502 = CARTESIAN_POINT ( 'NONE',  ( 4.219999999999999751, 10.25000000000000000, 3.750000000000000000 ) ) ;
#92503 = CARTESIAN_POINT ( 'NONE',  ( 7.361572987183170547, 37.05059781766744464, 9.846743663894590881 ) ) ;
#92504 = CARTESIAN_POINT ( 'NONE',  ( 8.606322355891263598, 15.00000000000000000, 11.66967075398811282 ) ) ;
#92505 = CARTESIAN_POINT ( 'NONE',  ( 8.527530157486175710, 28.92559781766745886, -4.923371831947298993 ) ) ;
#92506 = ORIENTED_EDGE ( 'NONE', *, *, #89212, .F. ) ;
#92507 = PRESENTATION_LAYER_ASSIGNMENT (  '', '', ( #90863 ) ) ;
#92508 = B_SPLINE_CURVE_WITH_KNOTS ( 'NONE', 3,
 ( #38013, #15518, #23512, #38502, #75006, #14026 ),
 .UNSPECIFIED., .F., .F.,
 ( 4, 2, 4 ),
 ( 3.409110551404661974E-05, 0.0004400426677358954116, 0.0008459942299577441222 ),
 .UNSPECIFIED. ) ;
#92509 = CARTESIAN_POINT ( 'NONE',  ( -0.8801773607111009756, 3.063685344154837509, 1.068504757029289695E-15 ) ) ;
#92510 = CARTESIAN_POINT ( 'NONE',  ( 10.00000000000000000, 61.81368534415484106, -10.88017736071110342 ) ) ;
#92511 = CARTESIAN_POINT ( 'NONE',  ( 19.84674366389459266, 58.30059781766745886, 2.638427012816836559 ) ) ;
#92513 = CARTESIAN_POINT ( 'NONE',  ( -0.8801773607111008646, 48.27201867748816966, 2.915334737309923430 ) ) ;
#92512 = CARTESIAN_POINT ( 'NONE',  ( 2.035157376598822676, 37.43868534415484106, -7.964842623401177768 ) ) ;
#92515 = CARTESIAN_POINT ( 'NONE',  ( 19.38216949554541557, 32.24863466993041783, -9.382169495545420901 ) ) ;
#92514 = CARTESIAN_POINT ( 'NONE',  ( -0.8801773607111009756, 8.063685344154837509, 1.068504757029289695E-15 ) ) ;
#92516 = CARTESIAN_POINT ( 'NONE',  ( 2.917880565312948704, 22.63708216824730002, 12.26659068614894643 ) ) ;
#92517 = EDGE_CURVE ( 'NONE', #29532, #75564, #24475, .T. ) ;
#92518 = ORIENTED_EDGE ( 'NONE', *, *, #12529, .F. ) ;
#92519 = CARTESIAN_POINT ( 'NONE',  ( 6.565887622018943937, 45.16530133659708923, 12.81628187352647430 ) ) ;
#92520 = ORIENTED_EDGE ( 'NONE', *, *, #25464, .T. ) ;
#92521 = CARTESIAN_POINT ( 'NONE',  ( 19.84674366389459266, 43.71726448433410894, -2.638427012816827677 ) ) ;
#92522 = CARTESIAN_POINT ( 'NONE',  ( 10.00000000000000178, 19.31368534415484106, 10.88017736071110342 ) ) ;
#92523 = CARTESIAN_POINT ( 'NONE',  ( -0.8801773607111008646, 13.27201867748817321, 2.915334737309923430 ) ) ;
#92524 = ORIENTED_EDGE ( 'NONE', *, *, #52183, .F. ) ;
#92525 = CARTESIAN_POINT ( 'NONE',  ( 20.88017736071110875, 60.77201867748817676, -2.915334737309920765 ) ) ;
#92526 = DIRECTION ( 'NONE',  ( -0.000000000000000000, -1.000000000000000000, -0.000000000000000000 ) ) ;
#92527 = CARTESIAN_POINT ( 'NONE',  ( 19.84674366389459621, 3.508931151000785231, 7.409399052514197653E-17 ) ) ;
#92528 = CARTESIAN_POINT ( 'NONE',  ( 2.035157376598822676, 62.43868534415483396, -7.964842623401177768 ) ) ;
#92529 = CARTESIAN_POINT ( 'NONE',  ( 14.16722289976681814, 15.00000000000000000, 4.928467845925615265 ) ) ;
#92530 = DIRECTION ( 'NONE',  ( -0.4305110968082986878, 0.000000000000000000, 0.9025852843498588518 ) ) ;
#92532 = ORIENTED_EDGE ( 'NONE', *, *, #68311, .T. ) ;
#92531 = CARTESIAN_POINT ( 'NONE',  ( 18.52753015748617571, 3.092264484334118269, 4.923371831947298993 ) ) ;
#92533 = CARTESIAN_POINT ( 'NONE',  ( 2.791683348922237240, 35.38393115100079456, -7.208316651077763204 ) ) ;
#92534 = ORIENTED_EDGE ( 'NONE', *, *, #44366, .F. ) ;
#92535 = EDGE_LOOP ( 'NONE', ( #4935, #6310, #60921, #70829 ) ) ;
#92536 = CARTESIAN_POINT ( 'NONE',  ( -10.98829462902744858, 46.98606209026556968, 3.000000000000000000 ) ) ;
#92537 = CARTESIAN_POINT ( 'NONE',  ( -16.94999999999999574, 99.99999999999998579, 7.750000000000000000 ) ) ;
#92538 = CARTESIAN_POINT ( 'NONE',  ( 21.09922568453595559, 57.04030133659708923, -6.408140936763230044 ) ) ;
#92539 = CARTESIAN_POINT ( 'NONE',  ( 17.08211943468705130, 8.470415501580635720, 12.26659068614894998 ) ) ;
#92540 = VECTOR ( 'NONE', #6885, 1000.000000000000000 ) ;
#92541 = CARTESIAN_POINT ( 'NONE',  ( 20.36894250292379738, 14.92874883491396432, -10.36894250292379027 ) ) ;
#92542 = LINE ( 'NONE', #47041, #87384 ) ;
#92544 = CARTESIAN_POINT ( 'NONE',  ( 4.559911319644449179, 62.23035201082150536, -9.422509992056141925 ) ) ;
#92543 = CARTESIAN_POINT ( 'NONE',  ( 66.76470751278411342, 44.99999999999998579, 9.500000000000000000 ) ) ;
#92545 = CARTESIAN_POINT ( 'NONE',  ( 20.88017736071110519, 15.56368534415483751, 2.639326808657452039E-16 ) ) ;
#92546 = CARTESIAN_POINT ( 'NONE',  ( 20.00000000000000711, 105.0000000000000000, -4.500000000000001776 ) ) ;
#92547 = VERTEX_POINT ( 'NONE', #11161 ) ;
#92548 = CARTESIAN_POINT ( 'NONE',  ( 18.52753015748617571, 8.092264484334117824, 4.923371831947298993 ) ) ;
#92550 = VECTOR ( 'NONE', #98832, 1000.000000000000114 ) ;
#92549 = CARTESIAN_POINT ( 'NONE',  ( 10.00000000000000178, 2.258931151000784787, 9.846743663894594434 ) ) ;
#92551 = CARTESIAN_POINT ( 'NONE',  ( 21.09922568453594849, 36.20696800326375353, 6.408140936763242479 ) ) ;
#92552 = CARTESIAN_POINT ( 'NONE',  ( 18.52753015748618282, 28.92559781766745175, -4.923371831947291888 ) ) ;
#92553 = VECTOR ( 'NONE', #78467, 1000.000000000000114 ) ;
#92554 = FACE_OUTER_BOUND ( 'NONE', #69187, .T. ) ;
#92555 = ADVANCED_FACE ( 'NONE', ( #4166 ), #96154, .F. ) ;
#92556 = CARTESIAN_POINT ( 'NONE',  ( 21.09922568453594849, 11.20696800326375531, 6.408140936763242479 ) ) ;
#92557 = CARTESIAN_POINT ( 'NONE',  ( -6.091055032734486119, 3.184843881676169275E-16, 13.29802223412754003 ) ) ;
#92558 = CARTESIAN_POINT ( 'NONE',  ( 14.92337183194729633, 7.675597817667451750, 8.527530157486181039 ) ) ;
#92559 = ORIENTED_EDGE ( 'NONE', *, *, #20324, .F. ) ;
#92560 = EDGE_CURVE ( 'NONE', #15746, #63180, #89904, .T. ) ;
#92561 = VERTEX_POINT ( 'NONE', #95141 ) ;
#92562 = CARTESIAN_POINT ( 'NONE',  ( 12.91533473730992121, 24.52201867748816966, 10.88017736071110164 ) ) ;
#92563 = CARTESIAN_POINT ( 'NONE',  ( 13.79529636645030344, 38.26208216824729647, 14.16423886937410614 ) ) ;
#92564 = CARTESIAN_POINT ( 'NONE',  ( 18.52753015748617571, 38.09226448433412315, 4.923371831947298993 ) ) ;
#92565 = CARTESIAN_POINT ( 'NONE',  ( 7.084665262690076126, 64.10535201082150536, 10.88017736071109987 ) ) ;
#92567 = CARTESIAN_POINT ( 'NONE',  ( 14.62617646268088478, 0.3640475087720987935, -3.327906561566882360 ) ) ;
#92566 = CARTESIAN_POINT ( 'NONE',  ( 6.565887622018943937, 55.16530133659709634, 12.81628187352647430 ) ) ;
#92568 = CARTESIAN_POINT ( 'NONE',  ( 19.42250999205614193, 25.14701867748817321, 5.440088680355555262 ) ) ;
#92569 = B_SPLINE_CURVE_WITH_KNOTS ( 'NONE', 3,
 ( #25909, #87870, #19386, #81360, #63882, #42877 ),
 .UNSPECIFIED., .F., .F.,
 ( 4, 2, 4 ),
 ( 3.409110551496205229E-05, 0.0004400426677368001241, 0.0008459942299586382638 ),
 .UNSPECIFIED. ) ;
#92570 = SURFACE_STYLE_USAGE ( .BOTH. , #94541 ) ;
#92571 = AXIS2_PLACEMENT_3D ( 'NONE', #53328, #91833, #90332 ) ;
#92572 = CARTESIAN_POINT ( 'NONE',  ( -2.816281873526473856, 19.12363466993042138, 9.499525473075851096E-16 ) ) ;
#92573 = CARTESIAN_POINT ( 'NONE',  ( 6.565887622018943937, 10.16530133659708746, 12.81628187352647430 ) ) ;
#92574 = CARTESIAN_POINT ( 'NONE',  ( 0.1532563361054100626, 35.80059781766745175, -2.638427012816831230 ) ) ;
#92575 = CARTESIAN_POINT ( 'NONE',  ( 10.88017736071110519, -4.436314655845152721, -2.602085213965210642E-15 ) ) ;
#92576 = CARTESIAN_POINT ( 'NONE',  ( 6.565887622018943937, 50.16530133659708213, 12.81628187352647430 ) ) ;
#92577 = CARTESIAN_POINT ( 'NONE',  ( -1.780824192092276048, 14.49999999999999112, -14.89391369643522545 ) ) ;
#92578 = EDGE_CURVE ( 'NONE', #26584, #60992, #89236, .T. ) ;
#92580 = CARTESIAN_POINT ( 'NONE',  ( -11.64999999999999680, 98.49999999999998579, 8.000000000000000000 ) ) ;
#92579 = CARTESIAN_POINT ( 'NONE',  ( 12.91533473730992121, 59.52201867748816966, 10.88017736071110164 ) ) ;
#92581 = PLANE ( 'NONE',  #30507 ) ;
#92582 = CARTESIAN_POINT ( 'NONE',  ( 10.00000000000000178, 69.31368534415484817, 10.88017736071110342 ) ) ;
#92583 = CARTESIAN_POINT ( 'NONE',  ( 15.44008868035555260, 54.73035201082150536, 9.422509992056143702 ) ) ;
#92584 = CARTESIAN_POINT ( 'NONE',  ( 10.00000000000000000, 51.81368534415484106, -10.88017736071110342 ) ) ;
#92585 = DIRECTION ( 'NONE',  ( -0.000000000000000000, 1.000000000000000000, -0.000000000000000000 ) ) ;
#92586 = AXIS2_PLACEMENT_3D ( 'NONE', #47053, #46567, #31066 ) ;
#92587 = LINE ( 'NONE', #53114, #85912 ) ;
#92588 = CARTESIAN_POINT ( 'NONE',  ( 20.88017736071110875, 15.77201867748817143, -2.915334737309920765 ) ) ;
#92589 = CARTESIAN_POINT ( 'NONE',  ( 5.076628168052703671, 56.84226448433412315, 8.527530157486179263 ) ) ;
#92591 = DIRECTION ( 'NONE',  ( 0.1822355254921578793, 0.000000000000000000, -0.9832549075639526182 ) ) ;
#92590 = CARTESIAN_POINT ( 'NONE',  ( -0.8801773607110991993, 17.85535201082150536, -2.915334737309923874 ) ) ;
#92592 = CARTESIAN_POINT ( 'NONE',  ( 22.81628187352647785, 31.41530133659709279, 3.434112377981063169 ) ) ;
#92593 = ORIENTED_EDGE ( 'NONE', *, *, #26758, .F. ) ;
#92594 = CARTESIAN_POINT ( 'NONE',  ( 17.96484262340118221, 39.93868534415484106, 7.964842623401181321 ) ) ;
#92595 = EDGE_CURVE ( 'NONE', #44503, #33481, #62773, .T. ) ;
#92597 = CARTESIAN_POINT ( 'NONE',  ( -19.19000000000001194, 93.50000000000000000, 9.500000000000000000 ) ) ;
#92596 = CARTESIAN_POINT ( 'NONE',  ( 21.09922568453594849, 6.206968003263753531, 6.408140936763242479 ) ) ;
#92598 = CARTESIAN_POINT ( 'NONE',  ( 10.00000000000000000, 16.81368534415483751, -10.88017736071110342 ) ) ;
#92599 = CARTESIAN_POINT ( 'NONE',  ( -0.8801773607111008646, 43.27201867748817676, 2.915334737309923430 ) ) ;
#92600 = CARTESIAN_POINT ( 'NONE',  ( -2.266590686148945544, 42.22041550158063217, 7.082119434687048631 ) ) ;
#92601 = CARTESIAN_POINT ( 'NONE',  ( 17.20831665107776587, 22.88393115100078745, 7.208316651077764980 ) ) ;
#92602 = CARTESIAN_POINT ( 'NONE',  ( 10.00000000000000178, 59.31368534415484106, 10.88017736071110342 ) ) ;
#92603 = FILL_AREA_STYLE_COLOUR ( '', #90547 ) ;
#92604 = CARTESIAN_POINT ( 'NONE',  ( 2.917880565312948704, 22.63708216824730002, 12.26659068614894643 ) ) ;
#92605 = SURFACE_STYLE_USAGE ( .BOTH. , #62097 ) ;
#92606 = CARTESIAN_POINT ( 'NONE',  ( 2.791683348922237240, 60.38393115100078745, -7.208316651077763204 ) ) ;
#92607 = ORIENTED_EDGE ( 'NONE', *, *, #2813, .F. ) ;
#92608 = ORIENTED_EDGE ( 'NONE', *, *, #23736, .F. ) ;
#92609 = CARTESIAN_POINT ( 'NONE',  ( -2.266590686148945544, 36.38708216824730357, -7.082119434687050408 ) ) ;
#92610 = CARTESIAN_POINT ( 'NONE',  ( 20.36894250292379382, 33.67874883491396076, 10.36894250292379205 ) ) ;
#92611 = CARTESIAN_POINT ( 'NONE',  ( 17.20831665107776587, 9.133931151000787452, -7.208316651077762316 ) ) ;
#92612 = CARTESIAN_POINT ( 'NONE',  ( 19.38216949554541202, 10.99863466993042138, 9.382169495545424454 ) ) ;
#92613 = CARTESIAN_POINT ( 'NONE',  ( 7.361572987183169658, 64.96726448433412315, -9.846743663894592657 ) ) ;
#92614 = CARTESIAN_POINT ( 'NONE',  ( -8.107943641493370990, -3.126452786875834722, 4.000000000000000000 ) ) ;
#92616 = CARTESIAN_POINT ( 'NONE',  ( 21.09922568453594849, 16.20696800326375353, 6.408140936763242479 ) ) ;
#92615 = CARTESIAN_POINT ( 'NONE',  ( 0.5774900079438590739, 57.64701867748817676, -5.440088680355550821 ) ) ;
#92617 = CARTESIAN_POINT ( 'NONE',  ( -4.164238869374099039, 26.80374883491397142, 8.674139862899312516E-16 ) ) ;
#92618 = CARTESIAN_POINT ( 'NONE',  ( 0.5774900079438607392, 33.48035201082150536, 5.440088680355550821 ) ) ;
#92619 = CARTESIAN_POINT ( 'NONE',  ( 10.00000000000000178, 34.31368534415484106, 10.88017736071110342 ) ) ;
#92620 = FACE_OUTER_BOUND ( 'NONE', #33970, .T. ) ;
#92621 = CARTESIAN_POINT ( 'NONE',  ( 15.44008868035555260, 54.73035201082150536, 9.422509992056143702 ) ) ;
#92622 = VECTOR ( 'NONE', #50788, 1000.000000000000000 ) ;
#92623 = CARTESIAN_POINT ( 'NONE',  ( -9.846743663894596210, -4.199402182332548250, -2.638427012816824124 ) ) ;
#92624 = ORIENTED_EDGE ( 'NONE', *, *, #71749, .F. ) ;
#92625 = CYLINDRICAL_SURFACE ( 'NONE', #81043, 11.92686044187656513 ) ;
#92626 = ORIENTED_EDGE ( 'NONE', *, *, #76791, .F. ) ;
#92627 = CARTESIAN_POINT ( 'NONE',  ( 10.00000000000000000, 5.553748834913967869, -14.16423886937410082 ) ) ;
#92629 = CARTESIAN_POINT ( 'NONE',  ( -2.266590686148945544, 61.38708216824730357, -7.082119434687050408 ) ) ;
#92628 = CARTESIAN_POINT ( 'NONE',  ( -2.266590686148945544, 61.38708216824730357, -7.082119434687050408 ) ) ;
#92631 = CARTESIAN_POINT ( 'NONE',  ( 5.076628168052703671, 66.84226448433412315, 8.527530157486179263 ) ) ;
#92630 = CARTESIAN_POINT ( 'NONE',  ( 14.92337183194729633, 37.67559781766745175, 8.527530157486181039 ) ) ;
#92632 = PLANE ( 'NONE',  #24709 ) ;
#92633 = AXIS2_PLACEMENT_3D ( 'NONE', #37416, #91378, #97931 ) ;
#92634 = CARTESIAN_POINT ( 'NONE',  ( 6.000000000000000000, 60.50000000000000000, -6.500000000000000888 ) ) ;
#92635 = EDGE_CURVE ( 'NONE', #85529, #42599, #53462, .T. ) ;
#92636 = CARTESIAN_POINT ( 'NONE',  ( 16.40814093676323893, 0.7903013365970867898, 11.09922568453595026 ) ) ;
#92637 = ORIENTED_EDGE ( 'NONE', *, *, #4887, .F. ) ;
#92638 = CARTESIAN_POINT ( 'NONE',  ( 22.26659068614895176, 44.72041550158063927, -7.082119434687042414 ) ) ;
#92639 = CARTESIAN_POINT ( 'NONE',  ( 2.917880565312948704, 42.63708216824729647, 12.26659068614894643 ) ) ;
#92640 = ORIENTED_EDGE ( 'NONE', *, *, #79255, .T. ) ;
#92641 = CARTESIAN_POINT ( 'NONE',  ( 17.96484262340118221, 14.93868534415483751, 7.964842623401181321 ) ) ;
#92642 = CARTESIAN_POINT ( 'NONE',  ( 3.591859063236763294, 58.29030133659708923, -11.09922568453595026 ) ) ;
#92643 = CARTESIAN_POINT ( 'NONE',  ( 18.52753015748618282, 53.92559781766745175, -4.923371831947291888 ) ) ;
#92644 = CARTESIAN_POINT ( 'NONE',  ( 15.44008868035555260, 34.73035201082151247, 9.422509992056143702 ) ) ;
#92645 = DIRECTION ( 'NONE',  ( 0.000000000000000000, -1.000000000000000000, -1.734723475976805517E-15 ) ) ;
#92646 = CARTESIAN_POINT ( 'NONE',  ( 1.472469842513823179, 51.42559781766745886, 4.923371831947296329 ) ) ;
#92647 = CARTESIAN_POINT ( 'NONE',  ( 7.084665262690076126, 64.10535201082150536, 10.88017736071109987 ) ) ;
#92648 = CARTESIAN_POINT ( 'NONE',  ( -0.8801773607110991993, 32.85535201082151247, -2.915334737309923874 ) ) ;
#92649 = B_SPLINE_CURVE_WITH_KNOTS ( 'NONE', 3,
 ( #57117, #63146, #71158, #10162, #17670, #42139 ),
 .UNSPECIFIED., .F., .F.,
 ( 4, 2, 4 ),
 ( 3.409110551494519295E-05, 0.0004400426677367694954, 0.0008459942299585938115 ),
 .UNSPECIFIED. ) ;
#92650 = DIRECTION ( 'NONE',  ( 1.000000000000000000, 2.641710877122040890E-15, 0.000000000000000000 ) ) ;
#92651 = FACE_OUTER_BOUND ( 'NONE', #62507, .T. ) ;
#92652 = DIRECTION ( 'NONE',  ( -0.6038238647437471629, 0.7971177707001175783, 1.387778780781426270E-14 ) ) ;
#92653 = VERTEX_POINT ( 'NONE', #29112 ) ;
#92654 = CARTESIAN_POINT ( 'NONE',  ( 8.991948000262459217, -4.139826107007521294, 3.750000000000000000 ) ) ;
#92655 = CARTESIAN_POINT ( 'NONE',  ( 0.1532563361054083140, 36.00893115100078745, 1.131784320476157264E-15 ) ) ;
#92656 = CARTESIAN_POINT ( 'NONE',  ( -46.48928645636215151, 103.2957187381728232, 6.397878122523974476 ) ) ;
#92657 = PRESENTATION_STYLE_ASSIGNMENT (( #9665 ) ) ;
#92658 = CARTESIAN_POINT ( 'NONE',  ( -12.69000000000001371, 93.50000000000000000, 9.500000000000000000 ) ) ;
#92659 = ORIENTED_EDGE ( 'NONE', *, *, #66046, .T. ) ;
#92660 = DIRECTION ( 'NONE',  ( 0.9975640502598243087, -0.06975647374412544122, -0.000000000000000000 ) ) ;
#92661 = CARTESIAN_POINT ( 'NONE',  ( -42.83934546894332129, 106.9582108035436363, 5.000000000000000888 ) ) ;
#92662 = CARTESIAN_POINT ( 'NONE',  ( 12.63842701281683922, 49.55059781766744464, -9.846743663894590881 ) ) ;
#92663 = CARTESIAN_POINT ( 'NONE',  ( 6.204703633549690345, 52.84541550158062506, 14.16423886937410082 ) ) ;
#92664 = CARTESIAN_POINT ( 'NONE',  ( 10.00000000000000178, 62.25893115100078745, 9.846743663894594434 ) ) ;
#92665 = B_SPLINE_CURVE_WITH_KNOTS ( 'NONE', 3,
 ( #31162, #15208, #67708, #219, #23200, #53675 ),
 .UNSPECIFIED., .F., .F.,
 ( 4, 2, 4 ),
 ( 0.0002800392683685244992, 0.0006862448819815560649, 0.001092450495594587739 ),
 .UNSPECIFIED. ) ;
#92666 = FILL_AREA_STYLE_COLOUR ( '', #68765 ) ;
#92667 = CARTESIAN_POINT ( 'NONE',  ( 18.52753015748617571, 23.09226448433411960, 4.923371831947298993 ) ) ;
#92668 = CARTESIAN_POINT ( 'NONE',  ( 22.81628187352647785, 51.41530133659708923, 3.434112377981063169 ) ) ;
#92669 = CARTESIAN_POINT ( 'NONE',  ( 0.1532563361054100626, 60.80059781766744464, -2.638427012816831230 ) ) ;
#92670 = CARTESIAN_POINT ( 'NONE',  ( 7.084665262690076126, 59.10535201082150536, 10.88017736071109987 ) ) ;
#92671 = CARTESIAN_POINT ( 'NONE',  ( 14.92337183194729988, 49.34226448433411605, -8.527530157486177487 ) ) ;
#92672 = FACE_OUTER_BOUND ( 'NONE', #66563, .T. ) ;
#92673 = EDGE_CURVE ( 'NONE', #98100, #27569, #83111, .T. ) ;
#92674 = CARTESIAN_POINT ( 'NONE',  ( 15.44008868035555793, 56.39701867748817676, -9.422509992056140149 ) ) ;
#92675 = EDGE_CURVE ( 'NONE', #63379, #61498, #96349, .T. ) ;
#92676 = EDGE_CURVE ( 'NONE', #77111, #42622, #75114, .T. ) ;
#92677 = EDGE_LOOP ( 'NONE', ( #50094, #34844, #20900, #78618 ) ) ;
#92678 = DIRECTION ( 'NONE',  ( 0.000000000000000000, 0.000000000000000000, 1.000000000000000000 ) ) ;
#92679 = CARTESIAN_POINT ( 'NONE',  ( 15.44008868035555260, 24.73035201082150891, 9.422509992056143702 ) ) ;
#92680 = AXIS2_PLACEMENT_3D ( 'NONE', #28876, #50900, #14397 ) ;
#92682 = CARTESIAN_POINT ( 'NONE',  ( 12.91533473730993009, 61.60535201082150536, -10.88017736071109987 ) ) ;
#92681 = CARTESIAN_POINT ( 'NONE',  ( 6.565887622018943937, 13.08196800326374998, -12.81628187352647608 ) ) ;
#92683 = LINE ( 'NONE', #47174, #80723 ) ;
#92684 = DIRECTION ( 'NONE',  ( -0.000000000000000000, -1.000000000000000000, -0.000000000000000000 ) ) ;
#92686 = AXIS2_PLACEMENT_3D ( 'NONE', #60988, #77468, #83510 ) ;
#92685 = CARTESIAN_POINT ( 'NONE',  ( 13.21382278599133286, 15.00000000000000888, 6.271621331965612001 ) ) ;
#92688 = DIRECTION ( 'NONE',  ( 0.000000000000000000, 1.000000000000000000, 0.000000000000000000 ) ) ;
#92687 = CARTESIAN_POINT ( 'NONE',  ( 4.559911319644449179, 57.23035201082150536, -9.422509992056141925 ) ) ;
#92689 = CARTESIAN_POINT ( 'NONE',  ( 14.92337183194729988, 44.34226448433412315, -8.527530157486177487 ) ) ;
#92690 = CARTESIAN_POINT ( 'NONE',  ( 2.791683348922240793, 6.633931151000785675, 7.208316651077764092 ) ) ;
#92691 = CARTESIAN_POINT ( 'NONE',  ( -10.88017736071110342, -36.93631465584515894, 3.903127820947815962E-15 ) ) ;
#92692 = CARTESIAN_POINT ( 'NONE',  ( -2.816281873526471635, 8.915301336597083903, -3.434112377981056508 ) ) ;
#92693 = AXIS2_PLACEMENT_3D ( 'NONE', #74186, #15693, #85158 ) ;
#92695 = CARTESIAN_POINT ( 'NONE',  ( 1.602071938427537701, 67.02224192338641728, -6.500000000000075495 ) ) ;
#92694 = CARTESIAN_POINT ( 'NONE',  ( 20.88017736071110164, 15.35535201082150358, 2.915334737309930979 ) ) ;
#92696 = DIRECTION ( 'NONE',  ( -1.257568779154408793E-17, -1.000000000000000000, 0.000000000000000000 ) ) ;
#92697 = CARTESIAN_POINT ( 'NONE',  ( -2.266590686148945544, 41.38708216824729647, -7.082119434687050408 ) ) ;
#92698 = CARTESIAN_POINT ( 'NONE',  ( -4.164238869374098151, 61.59541550158063217, -3.795296366450310543 ) ) ;
#92699 = CARTESIAN_POINT ( 'NONE',  ( 5.076628168052704559, 35.17559781766745175, -8.527530157486179263 ) ) ;
#92700 = CARTESIAN_POINT ( 'NONE',  ( 18.52753015748618282, 13.92559781766745175, -4.923371831947291888 ) ) ;
#92701 = CARTESIAN_POINT ( 'NONE',  ( 7.084665262690076126, 19.10535201082150181, 10.88017736071109987 ) ) ;
#92702 = ORIENTED_EDGE ( 'NONE', *, *, #16628, .F. ) ;
#92703 = CARTESIAN_POINT ( 'NONE',  ( 19.84674366389459266, 43.30059781766744464, 2.638427012816836559 ) ) ;
#92704 = CARTESIAN_POINT ( 'NONE',  ( 17.96484262340118221, 21.18868534415483396, -7.964842623401177768 ) ) ;
#92705 = CARTESIAN_POINT ( 'NONE',  ( 7.361572987183170547, 67.05059781766746596, 9.846743663894590881 ) ) ;
#92707 = PLANE ( 'NONE',  #48727 ) ;
#92706 = CARTESIAN_POINT ( 'NONE',  ( -2.266590686148945544, 11.38708216824730179, -7.082119434687050408 ) ) ;
#92708 = CARTESIAN_POINT ( 'NONE',  ( -13.50171220565604280, 14.99999999999793943, -5.622479820949179086 ) ) ;
#92709 = CARTESIAN_POINT ( 'NONE',  ( 12.63842701281683034, 17.46726448433411250, 9.846743663894596210 ) ) ;
#92710 = CARTESIAN_POINT ( 'NONE',  ( 16.40814093676324603, 52.45696800326375353, -11.09922568453594671 ) ) ;
#92711 = CARTESIAN_POINT ( 'NONE',  ( 18.52753015748617571, 53.09226448433412315, 4.923371831947298993 ) ) ;
#92712 = ORIENTED_EDGE ( 'NONE', *, *, #56826, .F. ) ;
#92713 = CARTESIAN_POINT ( 'NONE',  ( 14.92337183194729633, 17.67559781766745175, 8.527530157486181039 ) ) ;
#92714 = EDGE_CURVE ( 'NONE', #67453, #11101, #45103, .T. ) ;
#92715 = CARTESIAN_POINT ( 'NONE',  ( 0.2751277870542967463, 70.00000000000000000, -6.000000000000000000 ) ) ;
#92716 = CARTESIAN_POINT ( 'NONE',  ( -4.164238869374098151, 56.59541550158063927, -3.795296366450310543 ) ) ;
#92717 = CARTESIAN_POINT ( 'NONE',  ( -0.8801773607111008646, 53.27201867748816966, 2.915334737309923430 ) ) ;
#92718 = CYLINDRICAL_SURFACE ( 'NONE', #87328, 11.25000000000000178 ) ;
#92719 = VECTOR ( 'NONE', #24600, 1000.000000000000000 ) ;
#92720 = CARTESIAN_POINT ( 'NONE',  ( 12.91533473730992121, 59.52201867748816966, 10.88017736071110164 ) ) ;
#92721 = CARTESIAN_POINT ( 'NONE',  ( 19.84674366389459266, 38.71726448433412315, -2.638427012816827677 ) ) ;
#92722 = CARTESIAN_POINT ( 'NONE',  ( 7.084665262690076126, 24.10535201082150181, 10.88017736071109987 ) ) ;
#92723 = CARTESIAN_POINT ( 'NONE',  ( 18.72515096720572458, 40.05509018479936145, 6.499999999999964473 ) ) ;
#92724 = CARTESIAN_POINT ( 'NONE',  ( 0.1532563361054100626, 55.80059781766745175, -2.638427012816831230 ) ) ;
#92725 = CIRCLE ( 'NONE', #64010, 15.00000000000000000 ) ;
#92726 = CARTESIAN_POINT ( 'NONE',  ( 15.44008868035555260, 54.73035201082150536, 9.422509992056143702 ) ) ;
#92727 = CARTESIAN_POINT ( 'NONE',  ( 3.969999999999999751, 37.00000000000000000, 3.750000000000000000 ) ) ;
#92728 = EDGE_CURVE ( 'NONE', #79104, #52153, #38124, .T. ) ;
#92729 = ORIENTED_EDGE ( 'NONE', *, *, #32039, .T. ) ;
#92730 = ORIENTED_EDGE ( 'NONE', *, *, #31800, .F. ) ;
#92731 = AXIS2_PLACEMENT_3D ( 'NONE', #75088, #45580, #83086 ) ;
#92732 = CARTESIAN_POINT ( 'NONE',  ( -7.750000000000000000, 41.24999999999999289, -6.250000000000000000 ) ) ;
#92733 = CARTESIAN_POINT ( 'NONE',  ( -8.000000000000001776, -7.313785530895824394, -3.750000000000000000 ) ) ;
#92734 = CARTESIAN_POINT ( 'NONE',  ( 14.92337183194729988, 44.34226448433412315, -8.527530157486177487 ) ) ;
#92735 = CARTESIAN_POINT ( 'NONE',  ( 12.63842701281683034, 22.46726448433411605, 9.846743663894596210 ) ) ;
#92736 = CARTESIAN_POINT ( 'NONE',  ( 22.81628187352648496, 61.83196800326376774, -3.434112377981050290 ) ) ;
#92738 = CARTESIAN_POINT ( 'NONE',  ( 17.20831665107776587, 49.13393115100078745, -7.208316651077762316 ) ) ;
#92737 = CARTESIAN_POINT ( 'NONE',  ( 4.559911319644449179, 17.23035201082150536, -9.422509992056141925 ) ) ;
#92739 = CARTESIAN_POINT ( 'NONE',  ( 14.35840480524204210, 14.49999999999999112, 4.340070442838943165 ) ) ;
#92740 = CARTESIAN_POINT ( 'NONE',  ( 20.36894250292379738, 39.92874883491396787, -10.36894250292379027 ) ) ;
#92741 = CARTESIAN_POINT ( 'NONE',  ( 6.204703633549690345, 55.76208216824730357, -14.16423886937410259 ) ) ;
#92742 = DIRECTION ( 'NONE',  ( 0.000000000000000000, 1.000000000000000000, -0.000000000000000000 ) ) ;
#92743 = DIRECTION ( 'NONE',  ( 0.8073289077885722476, -0.5901017155109032908, 5.601969636702199977E-15 ) ) ;
#92744 = CARTESIAN_POINT ( 'NONE',  ( -0.8801773607111008646, 53.27201867748816966, 2.915334737309923430 ) ) ;
#92745 = CARTESIAN_POINT ( 'NONE',  ( 5.076628168052703671, 21.84226448433411960, 8.527530157486179263 ) ) ;
#92746 = CARTESIAN_POINT ( 'NONE',  ( -7.330124059958221139, -69.53998168068582686, 4.000000000000000888 ) ) ;
#92747 = ORIENTED_EDGE ( 'NONE', *, *, #17431, .F. ) ;
#92748 = LINE ( 'NONE', #24272, #25121 ) ;
#92749 = ORIENTED_EDGE ( 'NONE', *, *, #90441, .F. ) ;
#92750 = CARTESIAN_POINT ( 'NONE',  ( 5.076628168052704559, 5.175597817667451750, -8.527530157486179263 ) ) ;
#92751 = ORIENTED_EDGE ( 'NONE', *, *, #67677, .T. ) ;
#92752 = CARTESIAN_POINT ( 'NONE',  ( 2.917880565312950480, 15.97041550158063217, -12.26659068614894821 ) ) ;
#92753 = CARTESIAN_POINT ( 'NONE',  ( 10.00000000000000178, 22.25893115100078745, 9.846743663894594434 ) ) ;
#92754 = CARTESIAN_POINT ( 'NONE',  ( 15.44008868035555793, 46.39701867748817676, -9.422509992056140149 ) ) ;
#92755 = DIRECTION ( 'NONE',  ( 0.000000000000000000, 1.000000000000000000, -0.000000000000000000 ) ) ;
#92756 = EDGE_LOOP ( 'NONE', ( #52555, #67562, #45787, #6117 ) ) ;
#92757 = CARTESIAN_POINT ( 'NONE',  ( 7.084665262690076126, 39.10535201082150536, 10.88017736071109987 ) ) ;
#92758 = ORIENTED_EDGE ( 'NONE', *, *, #86122, .T. ) ;
#92759 = MECHANICAL_DESIGN_GEOMETRIC_PRESENTATION_REPRESENTATION (  '', ( #59201 ), #22557 ) ;
#92760 = CARTESIAN_POINT ( 'NONE',  ( -4.164238869374099039, 11.80374883491396965, 8.674139862899312516E-16 ) ) ;
#92761 = AXIS2_PLACEMENT_3D ( 'NONE', #31389, #40400, #54880 ) ;
#92762 = ORIENTED_EDGE ( 'NONE', *, *, #64993, .T. ) ;
#92763 = CARTESIAN_POINT ( 'NONE',  ( 6.565887622018943937, 15.16530133659708568, 12.81628187352647430 ) ) ;
#92764 = CARTESIAN_POINT ( 'NONE',  ( 2.791683348922240793, 6.633931151000785675, 7.208316651077764092 ) ) ;
#92765 = DIRECTION ( 'NONE',  ( 0.000000000000000000, 1.000000000000000000, 0.000000000000000000 ) ) ;
#92766 = CARTESIAN_POINT ( 'NONE',  ( 20.88017736071110519, 10.56368534415483929, 2.639326808657452039E-16 ) ) ;
#92767 = CARTESIAN_POINT ( 'NONE',  ( 5.076628168052704559, 10.17559781766745175, -8.527530157486179263 ) ) ;
#92768 = CARTESIAN_POINT ( 'NONE',  ( 4.559911319644449179, 37.23035201082150536, -9.422509992056141925 ) ) ;
#92769 = EDGE_CURVE ( 'NONE', #75287, #32729, #45604, .T. ) ;
#92770 = ORIENTED_EDGE ( 'NONE', *, *, #3524, .F. ) ;
#92771 = ORIENTED_EDGE ( 'NONE', *, *, #17393, .F. ) ;
#92772 = CARTESIAN_POINT ( 'NONE',  ( -46.34323875807881166, 103.6109741468810483, 6.190393423093146552 ) ) ;
#92773 = CARTESIAN_POINT ( 'NONE',  ( 7.084665262690076126, 59.10535201082150536, 10.88017736071109987 ) ) ;
#92774 = DIRECTION ( 'NONE',  ( 0.000000000000000000, 1.000000000000000000, 0.000000000000000000 ) ) ;
#92775 = CARTESIAN_POINT ( 'NONE',  ( 10.00000000000000000, 62.87363466993042493, -12.81628187352647608 ) ) ;
#92776 = CARTESIAN_POINT ( 'NONE',  ( 17.96484262340118221, 54.93868534415484106, 7.964842623401181321 ) ) ;
#92777 = LINE ( 'NONE', #9783, #69069 ) ;
#92778 = CARTESIAN_POINT ( 'NONE',  ( 18.52753015748618282, 33.92559781766745886, -4.923371831947291888 ) ) ;
#92779 = CARTESIAN_POINT ( 'NONE',  ( 0.6178305044545818747, 58.49863466993042493, -9.382169495545419124 ) ) ;
#92780 = CARTESIAN_POINT ( 'NONE',  ( 10.00000000000000000, 5.553748834913967869, -14.16423886937410082 ) ) ;
#92781 = CARTESIAN_POINT ( 'NONE',  ( 2.791683348922237240, 15.38393115100078212, -7.208316651077763204 ) ) ;
#92782 = CARTESIAN_POINT ( 'NONE',  ( 10.00000000000000178, 25.37363466993041783, 12.81628187352647608 ) ) ;
#92784 = CARTESIAN_POINT ( 'NONE',  ( -6.607088223530021232, -50.94269062318750940, -2.749999999999999556 ) ) ;
#92783 = CARTESIAN_POINT ( 'NONE',  ( -9.402796353261225093, 14.49999999999999112, 11.68706210897757281 ) ) ;
#92785 = CARTESIAN_POINT ( 'NONE',  ( 4.559911319644449179, 53.89701867748817676, 9.422509992056141925 ) ) ;
#92786 = EDGE_CURVE ( 'NONE', #98319, #24768, #37625, .T. ) ;
#92787 = CARTESIAN_POINT ( 'NONE',  ( 7.361572987183170547, 57.05059781766744464, 9.846743663894590881 ) ) ;
#92788 = AXIS2_PLACEMENT_3D ( 'NONE', #9322, #85320, #56307 ) ;
#92789 = CARTESIAN_POINT ( 'NONE',  ( 19.84674366389459266, 33.71726448433410894, -2.638427012816827677 ) ) ;
#92790 = CARTESIAN_POINT ( 'NONE',  ( 5.076628168052703671, 16.84226448433411960, 8.527530157486179263 ) ) ;
#92791 = CARTESIAN_POINT ( 'NONE',  ( 20.88017736071110519, 15.56368534415483751, 2.639326808657452039E-16 ) ) ;
#92792 = CARTESIAN_POINT ( 'NONE',  ( 21.09922568453594849, 21.20696800326375353, 6.408140936763242479 ) ) ;
#92793 = CARTESIAN_POINT ( 'NONE',  ( 12.91533473730992121, 4.522018677488169658, 10.88017736071110164 ) ) ;
#92794 = FILL_AREA_STYLE_COLOUR ( '', #47055 ) ;
#92795 = CARTESIAN_POINT ( 'NONE',  ( 18.72515096720577787, 46.07228050351031357, -6.499999999999891642 ) ) ;
#92796 = EDGE_CURVE ( 'NONE', #68070, #18218, #65504, .T. ) ;
#92797 = TOROIDAL_SURFACE ( 'NONE', #6581, 14.49999999999999822, 0.5000000000000000000 ) ;
#92798 = CARTESIAN_POINT ( 'NONE',  ( 20.88017736071110519, 15.56368534415483751, 2.639326808657452039E-16 ) ) ;
#92799 = ADVANCED_FACE ( 'NONE', ( #67629 ), #15623, .F. ) ;
#92800 = ORIENTED_EDGE ( 'NONE', *, *, #5766, .F. ) ;
#92801 = FILL_AREA_STYLE_COLOUR ( '', #12153 ) ;
#92803 = CARTESIAN_POINT ( 'NONE',  ( 2.035157376598824452, 13.68868534415483751, 7.964842623401179544 ) ) ;
#92802 = CARTESIAN_POINT ( 'NONE',  ( 0.1532563361054083140, 31.00893115100078390, 1.131784320476157264E-15 ) ) ;
#92804 = SURFACE_STYLE_USAGE ( .BOTH. , #79281 ) ;
#92805 = CARTESIAN_POINT ( 'NONE',  ( -0.8801773607110991993, 37.85535201082151247, -2.915334737309923874 ) ) ;
#92806 = CARTESIAN_POINT ( 'NONE',  ( 19.42250999205614548, 5.980352010821504471, -5.440088680355545492 ) ) ;
#92807 = CARTESIAN_POINT ( 'NONE',  ( 14.92337183194729988, 19.34226448433411960, -8.527530157486177487 ) ) ;
#92808 = CARTESIAN_POINT ( 'NONE',  ( 19.84674366389459266, 33.71726448433410894, -2.638427012816827677 ) ) ;
#92809 = MECHANICAL_DESIGN_GEOMETRIC_PRESENTATION_REPRESENTATION (  '', ( #76821 ), #36944 ) ;
#92810 = CARTESIAN_POINT ( 'NONE',  ( 18.00000000000000355, 78.50171742896758076, -3.769096794058098165 ) ) ;
#92811 = DIRECTION ( 'NONE',  ( 0.000000000000000000, -1.000000000000000000, 0.000000000000000000 ) ) ;
#92812 = CARTESIAN_POINT ( 'NONE',  ( 9.641450013144391207, 0.04962892333244047632, 11.16690429682355301 ) ) ;
#92813 = CARTESIAN_POINT ( 'NONE',  ( -8.028888469223478097, -1.053269085630145208, -3.750000000000000000 ) ) ;
#92814 = CARTESIAN_POINT ( 'NONE',  ( 24.16423886937409904, 19.09541550158063927, 3.795296366450317205 ) ) ;
#92815 = CARTESIAN_POINT ( 'NONE',  ( 14.92337183194729633, 37.67559781766745175, 8.527530157486181039 ) ) ;
#92816 = DIRECTION ( 'NONE',  ( -0.000000000000000000, 0.000000000000000000, 1.000000000000000000 ) ) ;
#92817 = CARTESIAN_POINT ( 'NONE',  ( 10.00000000000000178, 53.05374883491396787, 14.16423886937410082 ) ) ;
#92818 = EDGE_CURVE ( 'NONE', #68070, #43044, #69593, .T. ) ;
#92819 = CARTESIAN_POINT ( 'NONE',  ( 0.1532563361054100626, 20.80059781766744464, -2.638427012816831230 ) ) ;
#92821 = DIRECTION ( 'NONE',  ( -1.000000000000000000, -0.000000000000000000, -0.000000000000000000 ) ) ;
#92820 = CARTESIAN_POINT ( 'NONE',  ( 0.000000000000000000, 10.25000000000000000, -2.500000000000000000 ) ) ;
#92822 = CARTESIAN_POINT ( 'NONE',  ( 4.559911319644449179, 52.23035201082151247, -9.422509992056141925 ) ) ;
#92823 = CARTESIAN_POINT ( 'NONE',  ( -2.816281873526473856, 54.33196800326376064, 3.434112377981055619 ) ) ;
#92824 = CARTESIAN_POINT ( 'NONE',  ( 20.88017736071110164, 15.35535201082150358, 2.915334737309930979 ) ) ;
#92825 = AXIS2_PLACEMENT_3D ( 'NONE', #72535, #42074, #34532 ) ;
#92826 = CARTESIAN_POINT ( 'NONE',  ( -2.816281873526471635, 53.91530133659709634, -3.434112377981056508 ) ) ;
#92827 = CARTESIAN_POINT ( 'NONE',  ( 5.076628168052703671, 66.84226448433412315, 8.527530157486179263 ) ) ;
#92828 = CARTESIAN_POINT ( 'NONE',  ( 7.361572987183169658, -0.03273551566588185635, -9.846743663894592657 ) ) ;
#92829 = VERTEX_POINT ( 'NONE', #63549 ) ;
#92830 = CARTESIAN_POINT ( 'NONE',  ( 18.00000000000001776, 4.625929269271493211E-15, -8.000000000000000000 ) ) ;
#92831 = EDGE_CURVE ( 'NONE', #9027, #74685, #51582, .T. ) ;
#92832 = CARTESIAN_POINT ( 'NONE',  ( 1.780824192092484326, 14.49999999999999112, -14.89391369643520058 ) ) ;
#92833 = CARTESIAN_POINT ( 'NONE',  ( -0.3689425029237881626, 52.42874883491396076, 10.36894250292379027 ) ) ;
#92834 = CARTESIAN_POINT ( 'NONE',  ( 24.16423886937409904, 14.09541550158063217, 3.795296366450317205 ) ) ;
#92835 = CARTESIAN_POINT ( 'NONE',  ( -0.8801773607111009756, 13.06368534415483929, 1.068504757029289695E-15 ) ) ;
#92836 = CARTESIAN_POINT ( 'NONE',  ( 15.44008868035555260, 29.73035201082150891, 9.422509992056143702 ) ) ;
#92837 = CARTESIAN_POINT ( 'NONE',  ( 14.09397099617988935, 0.04962897248923205107, 4.360881834954268399 ) ) ;
#92838 = CARTESIAN_POINT ( 'NONE',  ( 10.00000000000000000, -0.2410688489992152128, -9.846743663894594434 ) ) ;
#92839 = SURFACE_STYLE_USAGE ( .BOTH. , #93332 ) ;
#92840 = CARTESIAN_POINT ( 'NONE',  ( 1.472469842513823179, 16.42559781766745175, 4.923371831947296329 ) ) ;
#92841 = CARTESIAN_POINT ( 'NONE',  ( 14.52941021839283486, 15.00000000000000888, -1.683622718073039426 ) ) ;
#92842 = AXIS2_PLACEMENT_3D ( 'NONE', #40718, #71220, #26203 ) ;
#92843 = SURFACE_STYLE_USAGE ( .BOTH. , #62835 ) ;
#92844 = CARTESIAN_POINT ( 'NONE',  ( 12.63842701281683922, 14.55059781766744997, -9.846743663894590881 ) ) ;
#92845 = CARTESIAN_POINT ( 'NONE',  ( 14.92337183194729633, 37.67559781766745175, 8.527530157486181039 ) ) ;
#92846 = CARTESIAN_POINT ( 'NONE',  ( -0.8801773607111008646, 18.27201867748817321, 2.915334737309923430 ) ) ;
#92847 = CARTESIAN_POINT ( 'NONE',  ( 22.81628187352647785, 26.41530133659708923, 3.434112377981063169 ) ) ;
#92848 = CARTESIAN_POINT ( 'NONE',  ( 17.20831665107776587, 12.88393115100078390, 7.208316651077764980 ) ) ;
#92849 = CARTESIAN_POINT ( 'NONE',  ( 8.375939845167682307, 15.00000000000000000, 11.52849216984304448 ) ) ;
#92850 = CARTESIAN_POINT ( 'NONE',  ( 10.00000000000000178, 52.25893115100078745, 9.846743663894594434 ) ) ;
#92851 = CARTESIAN_POINT ( 'NONE',  ( 12.63842701281683034, 32.46726448433412315, 9.846743663894596210 ) ) ;
#92852 = CARTESIAN_POINT ( 'NONE',  ( -4.164238869374099927, 12.01208216824730357, 3.795296366450308767 ) ) ;
#92853 = CARTESIAN_POINT ( 'NONE',  ( -0.8801773607110991993, 52.85535201082151247, -2.915334737309923874 ) ) ;
#92854 = CARTESIAN_POINT ( 'NONE',  ( 20.88017736071110875, 10.77201867748817143, -2.915334737309920765 ) ) ;
#92855 = CARTESIAN_POINT ( 'NONE',  ( 10.00000000000000178, 49.31368534415484106, 10.88017736071110342 ) ) ;
#92856 = CARTESIAN_POINT ( 'NONE',  ( 20.88017736071110875, 35.77201867748816966, -2.915334737309920765 ) ) ;
#92857 = ORIENTED_EDGE ( 'NONE', *, *, #75291, .T. ) ;
#92858 = B_SPLINE_CURVE_WITH_KNOTS ( 'NONE', 3,
 ( #94196, #87676, #27170, #57672, #88167, #56696, #14161, #98673, #6159, #66661, #6647, #51666, #73653, #81165, #89160, #51165, #43656, #96685 ),
 .UNSPECIFIED., .F., .F.,
 ( 4, 2, 2, 2, 2, 2, 2, 2, 4 ),
 ( 6.938893903907227145E-17, 0.01113440817397474449, 0.02226881634794941958, 0.04453763269589879059, 0.06680644904384815119, 0.07794085721782283149, 0.08350806130481017164, 0.08629166334830384866, 0.08907526539179752567 ),
 .UNSPECIFIED. ) ;
#92859 = CARTESIAN_POINT ( 'NONE',  ( -0.8801773607111008646, 43.27201867748817676, 2.915334737309923430 ) ) ;
#92860 = EDGE_LOOP ( 'NONE', ( #12466, #98089, #79237, #681 ) ) ;
#92861 = CARTESIAN_POINT ( 'NONE',  ( 21.09922568453594849, 61.20696800326376064, 6.408140936763242479 ) ) ;
#92862 = CARTESIAN_POINT ( 'NONE',  ( -0.8801773607110991993, 52.85535201082151247, -2.915334737309923874 ) ) ;
#92863 = ORIENTED_EDGE ( 'NONE', *, *, #29529, .T. ) ;
#92864 = CARTESIAN_POINT ( 'NONE',  ( -0.8801773607110991993, 47.85535201082150536, -2.915334737309923874 ) ) ;
#92865 = CARTESIAN_POINT ( 'NONE',  ( 6.910361961633475936, -84.29457034760254430, 3.750000000000000000 ) ) ;
#92866 = VECTOR ( 'NONE', #26401, 1000.000000000000000 ) ;
#92867 = CARTESIAN_POINT ( 'NONE',  ( 18.04007052943772749, 8.015283700948081957, 5.767676674365838529 ) ) ;
#92868 = CARTESIAN_POINT ( 'NONE',  ( -1.926860441876564023, 24.68830936912750929, 1.004413902775740781E-15 ) ) ;
#92869 = CARTESIAN_POINT ( 'NONE',  ( 6.204703633549690345, 55.76208216824730357, -14.16423886937410259 ) ) ;
#92870 = CARTESIAN_POINT ( 'NONE',  ( 0.5774900079438607392, 68.48035201082150536, 5.440088680355550821 ) ) ;
#92871 = DIRECTION ( 'NONE',  ( 0.000000000000000000, 0.000000000000000000, -1.000000000000000000 ) ) ;
#92872 = CARTESIAN_POINT ( 'NONE',  ( 12.91533473730992121, 14.52201867748817143, 10.88017736071110164 ) ) ;
#92873 = CARTESIAN_POINT ( 'NONE',  ( 5.076628168052704559, 50.17559781766745886, -8.527530157486179263 ) ) ;
#92874 = ORIENTED_EDGE ( 'NONE', *, *, #21641, .F. ) ;
#92875 = CARTESIAN_POINT ( 'NONE',  ( 17.20831665107776587, 42.88393115100077324, 7.208316651077764980 ) ) ;
#92876 = CARTESIAN_POINT ( 'NONE',  ( 4.559911319644449179, 67.23035201082150536, -9.422509992056141925 ) ) ;
#92877 = CARTESIAN_POINT ( 'NONE',  ( 15.44008868035555793, 36.39701867748816966, -9.422509992056140149 ) ) ;
#92878 = CARTESIAN_POINT ( 'NONE',  ( 19.84674366389459266, 43.30059781766744464, 2.638427012816836559 ) ) ;
#92879 = CARTESIAN_POINT ( 'NONE',  ( 6.565887622018943937, 28.08196800326375353, -12.81628187352647608 ) ) ;
#92881 = CARTESIAN_POINT ( 'NONE',  ( -14.16722289976683946, 14.49999999999999112, -4.928467845925748492 ) ) ;
#92880 = FACE_OUTER_BOUND ( 'NONE', #5811, .T. ) ;
#92882 = CARTESIAN_POINT ( 'NONE',  ( 7.084665262690076126, 44.10535201082151247, 10.88017736071109987 ) ) ;
#92883 = CARTESIAN_POINT ( 'NONE',  ( 13.79529636645031943, 60.34541550158063927, -14.16423886937409904 ) ) ;
#92884 = EDGE_CURVE ( 'NONE', #93159, #73208, #11670, .T. ) ;
#92885 = AXIS2_PLACEMENT_3D ( 'NONE', #29505, #84506, #15534 ) ;
#92886 = CARTESIAN_POINT ( 'NONE',  ( 16.40814093676323893, 25.79030133659708923, 11.09922568453595026 ) ) ;
#92887 = CARTESIAN_POINT ( 'NONE',  ( 2.603489959281614308, 51.58210964143330557, 6.500000000000031086 ) ) ;
#92888 = ORIENTED_EDGE ( 'NONE', *, *, #29040, .T. ) ;
#92889 = CARTESIAN_POINT ( 'NONE',  ( 3.591859063236763294, 23.29030133659708568, -11.09922568453595026 ) ) ;
#92890 = CARTESIAN_POINT ( 'NONE',  ( 12.91533473730993009, 26.60535201082150536, -10.88017736071109987 ) ) ;
#92891 = VECTOR ( 'NONE', #45302, 1000.000000000000000 ) ;
#92892 = VERTEX_POINT ( 'NONE', #46586 ) ;
#92893 = FACE_OUTER_BOUND ( 'NONE', #92078, .T. ) ;
#92894 = CARTESIAN_POINT ( 'NONE',  ( 2.791683348922240793, 1.633931151000784565, 7.208316651077764092 ) ) ;
#92895 = STYLED_ITEM ( 'NONE', ( #36041 ), #74512 ) ;
#92896 = CARTESIAN_POINT ( 'NONE',  ( 0.1532563361054083140, 51.00893115100078745, 1.131784320476157264E-15 ) ) ;
#92898 = CARTESIAN_POINT ( 'NONE',  ( 12.63842701281683922, 34.55059781766745886, -9.846743663894590881 ) ) ;
#92897 = CARTESIAN_POINT ( 'NONE',  ( 19.84674366389459621, 8.508931151000785675, 7.409399052514197653E-17 ) ) ;
#92899 = CARTESIAN_POINT ( 'NONE',  ( -11.62814530702576477, -77.87069291667818050, 3.750000000000000888 ) ) ;
#92900 = CARTESIAN_POINT ( 'NONE',  ( -2.816281873526471635, 63.91530133659708923, -3.434112377981056508 ) ) ;
#92901 = CARTESIAN_POINT ( 'NONE',  ( 0.1532563361054082862, 26.21726448433411605, 2.638427012816831674 ) ) ;
#92902 = CARTESIAN_POINT ( 'NONE',  ( 0.1143410931637268563, 40.21691075486302225, 6.480892540919860778 ) ) ;
#92903 = DIRECTION ( 'NONE',  ( 0.08715574274765151841, 0.9961946980917462113, 0.000000000000000000 ) ) ;
#92905 = CYLINDRICAL_SURFACE ( 'NONE', #14807, 0.5000000000000004441 ) ;
#92904 = CARTESIAN_POINT ( 'NONE',  ( 14.92337183194729633, 12.67559781766745353, 8.527530157486181039 ) ) ;
#92907 = ORIENTED_EDGE ( 'NONE', *, *, #14315, .T. ) ;
#92906 = CARTESIAN_POINT ( 'NONE',  ( 5.076628168052704559, 45.17559781766745175, -8.527530157486179263 ) ) ;
#92908 = CARTESIAN_POINT ( 'NONE',  ( 6.565887622018943937, 63.08196800326376064, -12.81628187352647608 ) ) ;
#92909 = CARTESIAN_POINT ( 'NONE',  ( 2.888814634336794640, -2.736763452578643607E-15, -14.33747749179068620 ) ) ;
#92910 = EDGE_CURVE ( 'NONE', #6038, #26787, #77084, .T. ) ;
#92911 = CARTESIAN_POINT ( 'NONE',  ( 0.6178305044545818747, 28.49863466993041783, -9.382169495545419124 ) ) ;
#92912 = CYLINDRICAL_SURFACE ( 'NONE', #13729, 0.5000000000000004441 ) ;
#92913 = CARTESIAN_POINT ( 'NONE',  ( 22.26659068614894466, 43.88708216824729647, 7.082119434687054849 ) ) ;
#92914 = ADVANCED_FACE ( 'NONE', ( #62563 ), #70087, .F. ) ;
#92915 = CARTESIAN_POINT ( 'NONE',  ( -14.16722289976691407, 0.3639312946971456353, 4.928467845925445623 ) ) ;
#92916 = CARTESIAN_POINT ( 'NONE',  ( 6.204703633549690345, 37.84541550158063927, 14.16423886937410082 ) ) ;
#92917 = CARTESIAN_POINT ( 'NONE',  ( -2.266590686148945544, 62.22041550158063927, 7.082119434687048631 ) ) ;
#92918 = CARTESIAN_POINT ( 'NONE',  ( 2.917880565312950480, 20.97041550158063217, -12.26659068614894821 ) ) ;
#92919 = CARTESIAN_POINT ( 'NONE',  ( 22.26659068614894466, 28.88708216824730357, 7.082119434687054849 ) ) ;
#92920 = LINE ( 'NONE', #54917, #96264 ) ;
#92922 = CARTESIAN_POINT ( 'NONE',  ( 5.076628168052704559, 45.17559781766745175, -8.527530157486179263 ) ) ;
#92921 = CARTESIAN_POINT ( 'NONE',  ( 4.380000001225145212, 0.09385850578814242118, 2.500000000000000000 ) ) ;
#92923 = EDGE_LOOP ( 'NONE', ( #84767, #25516, #2563, #75579, #11821, #49819, #54235, #49215, #66598, #13409, #8258, #2457, #13861, #7199, #31474, #80320, #64822, #24296, #21489, #81094, #82298, #88932, #74087, #54656, #61391, #41534, #76288, #39066, #27245, #53270 ) ) ;
#92924 = CARTESIAN_POINT ( 'NONE',  ( 19.42250999205614548, 40.98035201082150536, -5.440088680355545492 ) ) ;
#92925 = CARTESIAN_POINT ( 'NONE',  ( -12.60589901313210071, 0.5000000000000004441, -8.129656208642224158 ) ) ;
#92926 = CARTESIAN_POINT ( 'NONE',  ( 19.54721792061789643, 80.97117139608940306, -5.000000000000000888 ) ) ;
#92927 = CARTESIAN_POINT ( 'NONE',  ( 16.40814093676323893, 55.79030133659708923, 11.09922568453595026 ) ) ;
#92928 = CARTESIAN_POINT ( 'NONE',  ( -3.795296366450322534, -9.237917831752689324, -14.16423886937409904 ) ) ;
#92929 = CARTESIAN_POINT ( 'NONE',  ( 2.791683348922237240, 40.38393115100078035, -7.208316651077763204 ) ) ;
#92930 = CARTESIAN_POINT ( 'NONE',  ( 10.00000000000000178, 62.25893115100078745, 9.846743663894594434 ) ) ;
#92931 = MECHANICAL_DESIGN_GEOMETRIC_PRESENTATION_REPRESENTATION (  '', ( #97751 ), #56265 ) ;
#92932 = ORIENTED_EDGE ( 'NONE', *, *, #53955, .F. ) ;
#92933 = CARTESIAN_POINT ( 'NONE',  ( -0.3689425029237881626, 7.428748834913967869, 10.36894250292379027 ) ) ;
#92934 = DIRECTION ( 'NONE',  ( 1.000000000000000000, 0.000000000000000000, 0.000000000000000000 ) ) ;
#92936 = DIRECTION ( 'NONE',  ( -3.907985046680550391E-14, 0.000000000000000000, 1.000000000000000000 ) ) ;
#92935 = DIRECTION ( 'NONE',  ( 0.000000000000000000, 0.000000000000000000, 1.000000000000000000 ) ) ;
#92937 = CARTESIAN_POINT ( 'NONE',  ( 2.035157376598822676, 12.43868534415483751, -7.964842623401177768 ) ) ;
#92938 = CARTESIAN_POINT ( 'NONE',  ( 10.00000000000000000, 12.87363466993042138, -12.81628187352647608 ) ) ;
#92939 = CARTESIAN_POINT ( 'NONE',  ( 17.88942758462985338, 78.22945624030553802, 4.041088224284109742 ) ) ;
#92940 = CARTESIAN_POINT ( 'NONE',  ( 0.5774900079438607392, 63.48035201082149825, 5.440088680355550821 ) ) ;
#92941 = FILL_AREA_STYLE ('',( #47448 ) ) ;
#92942 = CARTESIAN_POINT ( 'NONE',  ( 0.000000000000000000, 0.5000000000000004441, 0.000000000000000000 ) ) ;
#92943 = DIRECTION ( 'NONE',  ( 1.000000000000000000, 0.000000000000000000, 0.000000000000000000 ) ) ;
#92944 = CARTESIAN_POINT ( 'NONE',  ( 2.035157376598822676, 2.438685344154838397, -7.964842623401177768 ) ) ;
#92945 = CARTESIAN_POINT ( 'NONE',  ( -14.94699059465103730, 0.3639308806416579611, -1.259949270175004132 ) ) ;
#92946 = CARTESIAN_POINT ( 'NONE',  ( 4.559911319644449179, 22.23035201082150536, -9.422509992056141925 ) ) ;
#92947 = CARTESIAN_POINT ( 'NONE',  ( 15.44008868035555260, 29.73035201082150891, 9.422509992056143702 ) ) ;
#92948 = CARTESIAN_POINT ( 'NONE',  ( 0.6178305044545818747, 3.498634669930420049, -9.382169495545419124 ) ) ;
#92949 = CARTESIAN_POINT ( 'NONE',  ( 1.472469842513823179, 55.59226448433412315, -4.923371831947296329 ) ) ;
#92950 = CARTESIAN_POINT ( 'NONE',  ( 22.81628187352648496, 61.83196800326376774, -3.434112377981050290 ) ) ;
#92951 = CARTESIAN_POINT ( 'NONE',  ( 2.791683348922237240, 0.3839311510007847872, -7.208316651077763204 ) ) ;
#92952 = EDGE_LOOP ( 'NONE', ( #46503, #61028, #2896, #54751 ) ) ;
#92953 = CARTESIAN_POINT ( 'NONE',  ( -0.8801773607111009756, 33.06368534415484106, 1.068504757029289695E-15 ) ) ;
#92954 = CARTESIAN_POINT ( 'NONE',  ( 16.40814093676323893, 30.79030133659708923, 11.09922568453595026 ) ) ;
#92955 = CARTESIAN_POINT ( 'NONE',  ( 0.000000000000000000, 14.49999999999999822, 0.000000000000000000 ) ) ;
#92956 = VECTOR ( 'NONE', #31380, 1000.000000000000000 ) ;
#92957 = CARTESIAN_POINT ( 'NONE',  ( 12.63842701281683034, 62.46726448433410894, 9.846743663894596210 ) ) ;
#92958 = CARTESIAN_POINT ( 'NONE',  ( 10.00000000000000178, 49.31368534415484106, 10.88017736071110342 ) ) ;
#92959 = CARTESIAN_POINT ( 'NONE',  ( 19.84674366389459266, 8.300597817667451750, 2.638427012816836559 ) ) ;
#92960 = CARTESIAN_POINT ( 'NONE',  ( 21.09922568453595559, 37.04030133659708923, -6.408140936763230044 ) ) ;
#92961 =( GEOMETRIC_REPRESENTATION_CONTEXT ( 3 ) GLOBAL_UNCERTAINTY_ASSIGNED_CONTEXT ( ( #40210 ) ) GLOBAL_UNIT_ASSIGNED_CONTEXT ( ( #97851, #89823, #30793 ) ) REPRESENTATION_CONTEXT ( 'NONE', 'WORKASPACE' ) );
#92963 = DIRECTION ( 'NONE',  ( 0.000000000000000000, 0.000000000000000000, 1.000000000000000000 ) ) ;
#92962 = CARTESIAN_POINT ( 'NONE',  ( 10.00000000000000000, 61.81368534415484106, -10.88017736071110342 ) ) ;
#92964 = DIRECTION ( 'NONE',  ( 0.000000000000000000, 0.000000000000000000, 1.000000000000000000 ) ) ;
#92965 = PRESENTATION_LAYER_ASSIGNMENT (  '', '', ( #86627 ) ) ;
#92966 = CARTESIAN_POINT ( 'NONE',  ( -2.816281873526473856, 59.12363466993042493, 9.499525473075851096E-16 ) ) ;
#92967 = ORIENTED_EDGE ( 'NONE', *, *, #81961, .F. ) ;
#92968 = CARTESIAN_POINT ( 'NONE',  ( 5.129999999999991900, 76.07179676972444327, -6.250000000000000000 ) ) ;
#92969 = DIRECTION ( 'NONE',  ( 0.06975647374412544122, 0.9975640502598243087, -0.000000000000000000 ) ) ;
#92970 = CARTESIAN_POINT ( 'NONE',  ( 15.44008868035555793, 6.397018677488170546, -9.422509992056140149 ) ) ;
#92972 = CARTESIAN_POINT ( 'NONE',  ( -2.266590686148945544, 16.38708216824730357, -7.082119434687050408 ) ) ;
#92971 = CARTESIAN_POINT ( 'NONE',  ( 0.6178305044545838731, 49.74863466993041072, 9.382169495545420901 ) ) ;
#92973 = CARTESIAN_POINT ( 'NONE',  ( 19.84674366389459266, 13.30059781766745353, 2.638427012816836559 ) ) ;
#92974 = CIRCLE ( 'NONE', #13097, 14.49999999999999822 ) ;
#92975 = CARTESIAN_POINT ( 'NONE',  ( 0.5774900079438607392, 8.480352010821505360, 5.440088680355550821 ) ) ;
#92976 = CARTESIAN_POINT ( 'NONE',  ( 19.84674366389459266, 13.71726448433411782, -2.638427012816827677 ) ) ;
#92977 = CARTESIAN_POINT ( 'NONE',  ( 0.000000000000000000, 0.000000000000000000, 3.000000000000000000 ) ) ;
#92978 = CARTESIAN_POINT ( 'NONE',  ( 2.917880565312948704, 62.63708216824730357, 12.26659068614894643 ) ) ;
#92979 = VERTEX_POINT ( 'NONE', #93561 ) ;
#92980 = AXIS2_PLACEMENT_3D ( 'NONE', #13884, #74867, #29851 ) ;
#92981 = CARTESIAN_POINT ( 'NONE',  ( 15.44008868035555260, 9.730352010821505360, 9.422509992056143702 ) ) ;
#92982 = CARTESIAN_POINT ( 'NONE',  ( 2.603489959281591659, 15.43575266056827999, -6.500000000000006217 ) ) ;
#92983 = PRESENTATION_LAYER_ASSIGNMENT (  '', '', ( #64270 ) ) ;
#92984 = ORIENTED_EDGE ( 'NONE', *, *, #80540, .T. ) ;
#92985 = ORIENTED_EDGE ( 'NONE', *, *, #73348, .T. ) ;
#92986 = CARTESIAN_POINT ( 'NONE',  ( 10.00000000000000000, 11.81368534415483751, -10.88017736071110342 ) ) ;
#92987 = CARTESIAN_POINT ( 'NONE',  ( 15.44008868035555793, 16.39701867748817321, -9.422509992056140149 ) ) ;
#92988 = CARTESIAN_POINT ( 'NONE',  ( 19.84674366389459266, 38.30059781766745175, 2.638427012816836559 ) ) ;
#92989 = CARTESIAN_POINT ( 'NONE',  ( -1.099225684535947600, 53.70696800326376064, -6.408140936763238038 ) ) ;
#92990 = CARTESIAN_POINT ( 'NONE',  ( 4.880290883660371115, 0.000000000000000000, -2.433223276543791780 ) ) ;
#92992 = CARTESIAN_POINT ( 'NONE',  ( 6.204703633549690345, 20.76208216824730357, -14.16423886937410259 ) ) ;
#92991 = CARTESIAN_POINT ( 'NONE',  ( 19.72487221294570858, 16.86607318730074567, 6.500000000000000888 ) ) ;
#92993 = CARTESIAN_POINT ( 'NONE',  ( -0.8801773607110991993, 27.85535201082150181, -2.915334737309923874 ) ) ;
#92994 = CARTESIAN_POINT ( 'NONE',  ( 17.08211943468705840, 65.13708216824730357, -12.26659068614894466 ) ) ;
#92995 = CARTESIAN_POINT ( 'NONE',  ( 10.00000000000000178, 57.25893115100078745, 9.846743663894594434 ) ) ;
#92996 = CARTESIAN_POINT ( 'NONE',  ( -6.000000000000014211, 80.32179676972448590, -4.000000000000000000 ) ) ;
#92997 = CARTESIAN_POINT ( 'NONE',  ( 1.472469842513823179, 36.42559781766745175, 4.923371831947296329 ) ) ;
#92998 = VECTOR ( 'NONE', #91437, 1000.000000000000000 ) ;
#92999 = CARTESIAN_POINT ( 'NONE',  ( 1.983216688680936812, -0.03417435944610275333, -14.11131997956737649 ) ) ;
#93000 = CARTESIAN_POINT ( 'NONE',  ( -2.638427012816824124, 27.05059781766745886, 9.846743663894596210 ) ) ;
#93001 = EDGE_LOOP ( 'NONE', ( #34579, #90741, #43795, #48362, #69417, #86748 ) ) ;
#93002 = DIRECTION ( 'NONE',  ( 0.000000000000000000, 1.000000000000000000, 0.000000000000000000 ) ) ;
#93003 = CARTESIAN_POINT ( 'NONE',  ( 12.91533473730993009, 61.60535201082150536, -10.88017736071109987 ) ) ;
#93004 = CARTESIAN_POINT ( 'NONE',  ( 1.472469842513823179, 60.59226448433412315, -4.923371831947296329 ) ) ;
#93005 = CARTESIAN_POINT ( 'NONE',  ( 4.559911319644449179, 52.23035201082151247, -9.422509992056141925 ) ) ;
#93007 = CARTESIAN_POINT ( 'NONE',  ( 6.565887622018943937, 38.08196800326376064, -12.81628187352647608 ) ) ;
#93006 = CARTESIAN_POINT ( 'NONE',  ( 12.91533473730993009, 11.60535201082150536, -10.88017736071109987 ) ) ;
#93008 = CARTESIAN_POINT ( 'NONE',  ( 2.917880565312948704, 12.63708216824730179, 12.26659068614894643 ) ) ;
#93009 = EDGE_CURVE ( 'NONE', #11604, #4363, #70128, .T. ) ;
#93010 = TOROIDAL_SURFACE ( 'NONE', #40354, 14.49999999999999822, 0.5000000000000000000 ) ;
#93011 = CARTESIAN_POINT ( 'NONE',  ( 19.38216949554541202, 50.99863466993042493, 9.382169495545424454 ) ) ;
#93012 = ORIENTED_EDGE ( 'NONE', *, *, #73699, .T. ) ;
#93013 = CARTESIAN_POINT ( 'NONE',  ( 17.20831665107776587, 64.13393115100079456, -7.208316651077762316 ) ) ;
#93014 = CARTESIAN_POINT ( 'NONE',  ( -0.8801773607111009756, 18.06368534415484106, 1.068504757029289695E-15 ) ) ;
#93015 = ORIENTED_EDGE ( 'NONE', *, *, #51977, .T. ) ;
#93016 = CARTESIAN_POINT ( 'NONE',  ( 10.00000000000000000, 31.81368534415483751, -10.88017736071110342 ) ) ;
#93017 = ORIENTED_EDGE ( 'NONE', *, *, #78846, .F. ) ;
#93018 = CARTESIAN_POINT ( 'NONE',  ( 20.88017736071110519, 65.56368534415483396, 2.639326808657452039E-16 ) ) ;
#93019 = CARTESIAN_POINT ( 'NONE',  ( 4.559911319644449179, 2.230352010821504471, -9.422509992056141925 ) ) ;
#93020 = CARTESIAN_POINT ( 'NONE',  ( 0.6076426042653030324, 42.37576471608601025, -6.499999999999984901 ) ) ;
#93021 = CARTESIAN_POINT ( 'NONE',  ( 0.1532563361054082862, 6.217264484334118713, 2.638427012816831674 ) ) ;
#93022 = CARTESIAN_POINT ( 'NONE',  ( 19.84674366389459266, 3.300597817667451750, 2.638427012816836559 ) ) ;
#93023 = CARTESIAN_POINT ( 'NONE',  ( -10.19513985507817821, 0.5000000000000004441, -11.00268709613231088 ) ) ;
#93024 = SURFACE_SIDE_STYLE ('',( #86031 ) ) ;
#93026 = EDGE_LOOP ( 'NONE', ( #58543, #63514, #61528, #11526 ) ) ;
#93025 = CARTESIAN_POINT ( 'NONE',  ( 19.84674366389459266, 8.717264484334116048, -2.638427012816827677 ) ) ;
#93027 = EDGE_CURVE ( 'NONE', #92445, #85917, #31576, .T. ) ;
#93028 = CARTESIAN_POINT ( 'NONE',  ( 0.1532563361054083140, 36.00893115100078745, 1.131784320476157264E-15 ) ) ;
#93029 = EDGE_LOOP ( 'NONE', ( #75854, #43375, #86019, #32596 ) ) ;
#93030 = EDGE_LOOP ( 'NONE', ( #98317, #22023, #35016, #59691 ) ) ;
#93031 = DIRECTION ( 'NONE',  ( 0.000000000000000000, 1.000000000000000000, 0.000000000000000000 ) ) ;
#93032 = CARTESIAN_POINT ( 'NONE',  ( 24.16423886937409904, 9.095415501580633943, 3.795296366450317205 ) ) ;
#93033 = CIRCLE ( 'NONE', #19594, 0.2000000000000000944 ) ;
#93034 = CIRCLE ( 'NONE', #13236, 0.2500000000000002220 ) ;
#93035 = CARTESIAN_POINT ( 'NONE',  ( -2.816281873526473856, 59.33196800326374643, 3.434112377981055619 ) ) ;
#93036 =( GEOMETRIC_REPRESENTATION_CONTEXT ( 3 ) GLOBAL_UNCERTAINTY_ASSIGNED_CONTEXT ( ( #34487 ) ) GLOBAL_UNIT_ASSIGNED_CONTEXT ( ( #88319, #73310, #73799 ) ) REPRESENTATION_CONTEXT ( 'NONE', 'WORKASPACE' ) );
#93037 = CARTESIAN_POINT ( 'NONE',  ( 17.08211943468705840, 10.13708216824730179, -12.26659068614894466 ) ) ;
#93038 = CARTESIAN_POINT ( 'NONE',  ( 22.26659068614894466, 18.88708216824730002, 7.082119434687054849 ) ) ;
#93039 = FACE_OUTER_BOUND ( 'NONE', #76486, .T. ) ;
#93040 = CARTESIAN_POINT ( 'NONE',  ( -12.34086200392816757, -0.03417435944610275333, -7.125000000000143885 ) ) ;
#93041 = CARTESIAN_POINT ( 'NONE',  ( 7.084665262690076126, 19.10535201082150181, 10.88017736071109987 ) ) ;
#93042 = CARTESIAN_POINT ( 'NONE',  ( 15.00000000000000178, 73.00000000000000000, -6.250000000000000000 ) ) ;
#93043 = ORIENTED_EDGE ( 'NONE', *, *, #95980, .T. ) ;
#93044 = COLOUR_RGB ( '', 0.40784314, 0.44705882, 0.49803922) ;
#93045 = CARTESIAN_POINT ( 'NONE',  ( 7.361572987183170547, 2.050597817667451750, 9.846743663894590881 ) ) ;
#93046 = CARTESIAN_POINT ( 'NONE',  ( 3.591859063236761518, 29.95696800326375708, 11.09922568453594849 ) ) ;
#93047 = CARTESIAN_POINT ( 'NONE',  ( 12.63842701281683922, 39.55059781766744464, -9.846743663894590881 ) ) ;
#93048 = CARTESIAN_POINT ( 'NONE',  ( 6.565887622018943937, 20.16530133659708213, 12.81628187352647430 ) ) ;
#93049 = DIRECTION ( 'NONE',  ( 0.000000000000000000, 0.000000000000000000, -1.000000000000000000 ) ) ;
#93050 = CARTESIAN_POINT ( 'NONE',  ( 0.1532563361054082862, 31.21726448433412315, 2.638427012816831674 ) ) ;
#93051 = CARTESIAN_POINT ( 'NONE',  ( 5.076628168052703671, 11.84226448433411960, 8.527530157486179263 ) ) ;
#93052 = VERTEX_POINT ( 'NONE', #92577 ) ;
#93053 = ORIENTED_EDGE ( 'NONE', *, *, #62783, .F. ) ;
#93054 = CARTESIAN_POINT ( 'NONE',  ( 7.084665262690076126, 32.02201867748816966, -10.88017736071110164 ) ) ;
#93055 = CARTESIAN_POINT ( 'NONE',  ( -2.266590686148945544, 27.22041550158063572, 7.082119434687048631 ) ) ;
#93056 = CARTESIAN_POINT ( 'NONE',  ( 19.84674366389459621, 43.50893115100078745, 7.409399052514197653E-17 ) ) ;
#93057 = CARTESIAN_POINT ( 'NONE',  ( 19.84674366389459266, 3.717264484334118713, -2.638427012816827677 ) ) ;
#93059 = CARTESIAN_POINT ( 'NONE',  ( 14.99999999999997868, 80.07179676972448590, -6.500000000000000888 ) ) ;
#93058 = CARTESIAN_POINT ( 'NONE',  ( 6.565887622018943937, 50.16530133659708213, 12.81628187352647430 ) ) ;
#93060 = CARTESIAN_POINT ( 'NONE',  ( 0.5774900079438590739, 32.64701867748816966, -5.440088680355550821 ) ) ;
#93061 = CARTESIAN_POINT ( 'NONE',  ( 0.000000000000000000, 0.5000000000000004441, 0.000000000000000000 ) ) ;
#93062 = ADVANCED_FACE ( 'NONE', ( #40578 ), #48053, .F. ) ;
#93063 = CARTESIAN_POINT ( 'NONE',  ( -1.099225684535947600, 19.54030133659708568, 6.408140936763237150 ) ) ;
#93064 = CARTESIAN_POINT ( 'NONE',  ( 1.472469842513823179, 36.42559781766745175, 4.923371831947296329 ) ) ;
#93065 = CARTESIAN_POINT ( 'NONE',  ( 10.88017736071110164, 5.355352010821507136, 2.915334737309921209 ) ) ;
#93066 = CARTESIAN_POINT ( 'NONE',  ( -1.099225684535947600, 43.70696800326375353, -6.408140936763238038 ) ) ;
#93067 = CARTESIAN_POINT ( 'NONE',  ( 12.30000000000000249, 99.99999999999998579, -8.525133428036873795 ) ) ;
#93069 = CARTESIAN_POINT ( 'NONE',  ( 0.000000000000000000, 14.49999999999999822, 0.000000000000000000 ) ) ;
#93068 = CARTESIAN_POINT ( 'NONE',  ( 2.035157376598824452, 53.68868534415484817, 7.964842623401179544 ) ) ;
#93070 = ADVANCED_FACE ( 'NONE', ( #79050 ), #56372, .T. ) ;
#93071 = CARTESIAN_POINT ( 'NONE',  ( 13.99999999999999822, 60.50000000000000711, -5.000000000000000000 ) ) ;
#93072 = DIRECTION ( 'NONE',  ( 1.000000000000000000, 0.000000000000000000, -0.000000000000000000 ) ) ;
#93073 =( BOUNDED_SURFACE ( )  B_SPLINE_SURFACE ( 1, 2, ( 
 ( #21662, #7657, #38150, #16125, #23146, #76618, #53130, #67656, #77108, #52634, #60626, #82642, #15649, #44643, #59642, #90626, #54108, #75137, #29622, #165, #6643, #98166, #60128, #68636, #22151, #53619, #8136, #84621, #14662, #37650, #8621, #61603, #45128, #38629, #92117, #69130, #31109, #91127, #23648, #39130, #69617, #1139, #22650, #83638, #45631, #76130, #54597, #70113, #10591, #40106, #49079, #56587, #9603, #2133, #85110, #47606, #93587, #47097, #78595, #41103, #10107, #86102, #70607, #72070, #17612, #71101, #48579, #93092, #32593, #63088, #55607, #79078, #40604, #17124, #71599, #87077, #3111, #62587, #48082, #25125, #39624, #85609, #31601, #33565, #2627, #86593, #33081, #78100, #63578, #64061, #24623, #1638, #18102, #94573, #94088, #24128, #25607, #56100, #18586, #79582, #26091, #32089, #11082, #41602, #62096, #55089, #92604, #16621, #77595, #9110, #59036, #66039, #72549, #58538, #96568, #87564, #96066, #5063, #28043, #81048, #82032, #74032, #43058, #21051, #13042, #51542, #73537, #12555, #20557, #42086, #5563, #65542, #27548, #89045, #19565, #42560, #51042, #4082, #20051, #89540, #3595, #43538, #13542, #44026, #12059, #58042, #35548, #50553, #73044, #81535, #34054, #36039, #66542, #95566, #4579, #34545, #57063, #64550, #35041, #95057, #26566, #65040, #88550, #97070, #28543, #19074, #49552, #80064, #11569, #27055, #57553, #88052, #50061, #80565, #91999, #37039, #15538, #76509, #29509, #7035, #60515, #30503, #14045, #30009, #59530, #44527, #91007, #61005, #29021, #91516, #23033, #90512, #67538, #84510, #37541, #30995, #53505, #23530, #84016, #54002, #7543, #46021, #36548, #38034, #52037, #68031, #52522, #53009, #75026, #61493, #60017, #98558, #6531, #75519, #22538, #68525, #83524, #16008, #56, #98053, #8023, #38520, #90025, #15042, #76014, #69018, #45514, #74529, #549, #6050, #67038, #97560, #21546, #82529, #22047, #83028, #14545, #45015, #9486, #70492, #9990, #62472, #85492, #70989, #46986, #62972, #2995, #46497, #86482, #33445, #86954, #54971, #2012, #47965, #93477, #17001, #17500, #76997, #17980, #78474, #39508, #47480, #77480, #1022, #63940, #77980, #8509, #39012, #84994, #32477, #39989, #48464, #69506, #63468, #25003, #78961, #69998, #94452, #55488, #85988, #54483, #25968, #8991, #10473, #40982, #1524, #40491, #2511, #32963, #16509, #93970, #31482, #31970, #25494, #55981, #61986, #71479, #56468, #92978, #24509, #92485, #24013, #73917, #96447, #66416, #65918, #96947, #50427, #73416, #79461, #80934, #94943, #11942, #95448, #80445, #26444, #72432, #18467, #20435, #19447, #4943, #42447, #3958, #95946, #27918 ),
 ( #43417, #72930, #12428, #34428, #57439, #42935, #18960, #34925, #5446, #48952, #58410, #35917, #58916, #26939, #4459, #19932, #65423, #87930, #88433, #10959, #88926, #35423, #11449, #49939, #49439, #71951, #28420, #27429, #41483, #3473, #56943, #57923, #50923, #81419, #33930, #12920, #64435, #87446, #41966, #79943, #64920, #37422, #97432, #7904, #51916, #30381, #91383, #44403, #21923, #75392, #45388, #28897, #44889, #74402, #59402, #6911, #75894, #43902, #7419, #37916, #6404, #82400, #429, #52402, #45902, #68404, #38398, #98924, #68900, #22414, #60884, #51418, #52888, #66912, #82903, #67407, #14420, #89906, #74904, #89415, #22913, #90386, #53380, #67909, #36915, #98432, #83891, #13925, #21421, #15420, #76389, #29888, #81907, #90887, #97937, #30879, #20929, #60390, #29393, #13417, #59895, #83400, #14920, #5927, #36419, #93352, #16878, #17857, #24877, #31365, #17377, #55360, #46383, #54852, #62856, #85864, #39868, #40856, #32840, #1893, #78848, #70871, #10357, #32351, #70376, #78350, #904, #63342, #24385, #47353, #47846, #77855, #69879, #9871, #61375, #2387, #40370, #54364, #1399, #61865, #15895, #71361, #31854, #2878, #91884, #92370, #9365, #62353, #93848, #84396, #25375, #55860, #86356, #84874, #48343, #23406, #53890, #69381, #76869, #23896, #8385, #38895, #16382, #92856, #46866, #77358, #8868, #39385, #85365, #71837, #20691, #89670, #86847, #51683, #21183, #50692, #94826, #44662, #66171, #90153, #13675, #82662, #82162, #14178, #66680, #44158, #94336, #97204, #10848, #28183, #12685, #96705, #41369, #87325, #33328, #36681, #35687, #74667, #58679, #18842, #13179, #6177, #26329, #3345, #67169, #97694, #89178, #25853, #36179, #81185, #21683, #75156, #43673, #33808, #52168, #43184, #51183, #64314, #81666, #74160, #28673, #5694, #63822, #59165, #56828, #29157, #59662, #18351, #56350, #48828, #79338, #73671, #5201, #77127, #46149, #24144, #16141, #54612, #76635, #15666, #23664, #45150, #8637, #68653, #30630, #69150, #22670, #45653, #31126, #7166, #23165, #62111, #6667, #46627, #92621, #47114, #15172, #37669, #1160, #37185, #75656, #8154, #98186, #60150, #68169, #84160, #67676, #676, #54126, #31621, #98688, #83656, #85130, #39146, #30137, #38647, #69636, #61622, #92140, #7674, #84638, #16641, #29643, #90647, #60644, #22172, #52654, #83157, #14681, #91144, #53148, #76149, #38166, #182, #61139, #91647, #53643, #93608, #40620, #93110, #25622, #87092, #56114, #33100, #17630, #19090, #63594, #18119, #94591, #40123, #86119, #10123, #2646, #26107, #86611, #63105, #56601, #34072, #18603, #9624, #94100, #48102, #10609, #48593, #71612 ) ),
 .UNSPECIFIED., .F., .F., .T. ) 
 B_SPLINE_SURFACE_WITH_KNOTS ( ( 2, 2 ),
 ( 3, 2, 2, 2, 2, 2, 2, 2, 2, 2, 2, 2, 2, 2, 2, 2, 2, 2, 2, 2, 2, 2, 2, 2, 2, 2, 2, 2, 2, 2, 2, 2, 2, 2, 2, 2, 2, 2, 2, 2, 2, 2, 2, 2, 2, 2, 2, 2, 2, 2, 2, 2, 2, 2, 2, 2, 2, 2, 2, 2, 2, 2, 2, 2, 2, 2, 2, 2, 2, 2, 2, 2, 2, 2, 2, 2, 2, 2, 2, 2, 2, 2, 2, 2, 2, 2, 2, 2, 2, 2, 2, 2, 2, 2, 2, 2, 2, 2, 2, 2, 2, 2, 2, 2, 2, 2, 2, 2, 2, 2, 2, 2, 2, 2, 2, 2, 2, 2, 2, 2, 2, 2, 2, 2, 2, 2, 2, 2, 2, 2, 2, 2, 2, 2, 2, 2, 2, 2, 2, 2, 2, 2, 2, 2, 2, 2, 2, 2, 2, 2, 2, 2, 2, 2, 2, 2, 2, 2, 2, 2, 2, 2, 3 ),
 ( 0.000000000000000000, 1.000000000000000000 ),
 ( 0.000000000000000000, 0.005952380952380952051, 0.01190476190476190410, 0.01785714285714285615, 0.02380952380952380820, 0.02976190476190476025, 0.03571428571428571230, 0.04166666666666666435, 0.04761904761904761640, 0.05357142857142856845, 0.05952380952380952051, 0.06547619047619047949, 0.07142857142857142461, 0.07738095238095238360, 0.08333333333333332871, 0.08928571428571428770, 0.09523809523809523281, 0.1011904761904761918, 0.1071428571428571369, 0.1130952380952380959, 0.1190476190476190410, 0.1250000000000000000, 0.1309523809523809590, 0.1369047619047619180, 0.1428571428571428492, 0.1488095238095238082, 0.1547619047619047672, 0.1607142857142857262, 0.1666666666666666574, 0.1726190476190476164, 0.1785714285714285754, 0.1845238095238095344, 0.1904761904761904656, 0.1964285714285714246, 0.2023809523809523836, 0.2083333333333333426, 0.2142857142857142738, 0.2202380952380952328, 0.2261904761904761918, 0.2321428571428571508, 0.2380952380952380820, 0.2440476190476190410, 0.2500000000000000000, 0.2559523809523809312, 0.2619047619047619180, 0.2678571428571428492, 0.2738095238095238360, 0.2797619047619047672, 0.2857142857142856984, 0.2916666666666666852, 0.2976190476190476164, 0.3035714285714285476, 0.3095238095238095344, 0.3154761904761904656, 0.3214285714285714524, 0.3273809523809523836, 0.3333333333333333148, 0.3392857142857143016, 0.3452380952380952328, 0.3511904761904761640, 0.3571428571428571508, 0.3630952380952380820, 0.3690476190476190688, 0.3750000000000000000, 0.3809523809523809312, 0.3869047619047619180, 0.3928571428571428492, 0.3988095238095238360, 0.4047619047619047672, 0.4107142857142856984, 0.4166666666666666852, 0.4226190476190476164, 0.4285714285714285476, 0.4345238095238095344, 0.4404761904761904656, 0.4464285714285714524, 0.4523809523809523836, 0.4583333333333333148, 0.4642857142857143016, 0.4702380952380952328, 0.4761904761904761640, 0.4821428571428571508, 0.4880952380952380820, 0.4940476190476190688, 0.5000000000000000000, 0.5059523809523809312, 0.5119047619047618625, 0.5178571428571429047, 0.5238095238095238360, 0.5297619047619047672, 0.5357142857142856984, 0.5416666666666666297, 0.5476190476190476719, 0.5535714285714286031, 0.5595238095238095344, 0.5654761904761904656, 0.5714285714285713969, 0.5773809523809523281, 0.5833333333333333703, 0.5892857142857143016, 0.5952380952380952328, 0.6011904761904761640, 0.6071428571428570953, 0.6130952380952381375, 0.6190476190476190688, 0.6250000000000000000, 0.6309523809523809312, 0.6369047619047618625, 0.6428571428571429047, 0.6488095238095238360, 0.6547619047619047672, 0.6607142857142856984, 0.6666666666666666297, 0.6726190476190476719, 0.6785714285714286031, 0.6845238095238095344, 0.6904761904761904656, 0.6964285714285713969, 0.7023809523809523281, 0.7083333333333333703, 0.7142857142857143016, 0.7202380952380952328, 0.7261904761904761640, 0.7321428571428570953, 0.7380952380952381375, 0.7440476190476190688, 0.7500000000000000000, 0.7559523809523809312, 0.7619047619047618625, 0.7678571428571429047, 0.7738095238095238360, 0.7797619047619047672, 0.7857142857142856984, 0.7916666666666666297, 0.7976190476190476719, 0.8035714285714286031, 0.8095238095238095344, 0.8154761904761904656, 0.8214285714285713969, 0.8273809523809523281, 0.8333333333333333703, 0.8392857142857143016, 0.8452380952380952328, 0.8511904761904761640, 0.8571428571428570953, 0.8630952380952381375, 0.8690476190476190688, 0.8750000000000000000, 0.8809523809523809312, 0.8869047619047618625, 0.8928571428571429047, 0.8988095238095238360, 0.9047619047619047672, 0.9107142857142856984, 0.9166666666666666297, 0.9226190476190476719, 0.9285714285714286031, 0.9345238095238095344, 0.9404761904761904656, 0.9464285714285713969, 0.9523809523809523281, 0.9583333333333333703, 0.9642857142857143016 ),
 .UNSPECIFIED. ) 
 GEOMETRIC_REPRESENTATION_ITEM ( )  RATIONAL_B_SPLINE_SURFACE ( (
 ( 1.000000000000000000, 0.9659258262890683122, 1.000000000000000000, 0.9659258262890683122, 1.000000000000000000, 0.9659258262890683122, 1.000000000000000000, 0.9659258262890683122, 1.000000000000000000, 0.9659258262890683122, 1.000000000000000000, 0.9659258262890683122, 1.000000000000000000, 0.9659258262890683122, 1.000000000000000000, 0.9659258262890683122, 1.000000000000000000, 0.9659258262890683122, 1.000000000000000000, 0.9659258262890683122, 1.000000000000000000, 0.9659258262890683122, 1.000000000000000000, 0.9659258262890683122, 1.000000000000000000, 0.9659258262890683122, 1.000000000000000000, 0.9659258262890683122, 1.000000000000000000, 0.9659258262890683122, 1.000000000000000000, 0.9659258262890683122, 1.000000000000000000, 0.9659258262890683122, 1.000000000000000000, 0.9659258262890683122, 1.000000000000000000, 0.9659258262890683122, 1.000000000000000000, 0.9659258262890683122, 1.000000000000000000, 0.9659258262890683122, 1.000000000000000000, 0.9659258262890683122, 1.000000000000000000, 0.9659258262890683122, 1.000000000000000000, 0.9659258262890683122, 1.000000000000000000, 0.9659258262890683122, 1.000000000000000000, 0.9659258262890683122, 1.000000000000000000, 0.9659258262890683122, 1.000000000000000000, 0.9659258262890683122, 1.000000000000000000, 0.9659258262890683122, 1.000000000000000000, 0.9659258262890683122, 1.000000000000000000, 0.9659258262890683122, 1.000000000000000000, 0.9659258262890683122, 1.000000000000000000, 0.9659258262890683122, 1.000000000000000000, 0.9659258262890683122, 1.000000000000000000, 0.9659258262890683122, 1.000000000000000000, 0.9659258262890683122, 1.000000000000000000, 0.9659258262890683122, 1.000000000000000000, 0.9659258262890683122, 1.000000000000000000, 0.9659258262890683122, 1.000000000000000000, 0.9659258262890683122, 1.000000000000000000, 0.9659258262890683122, 1.000000000000000000, 0.9659258262890683122, 1.000000000000000000, 0.9659258262890683122, 1.000000000000000000, 0.9659258262890683122, 1.000000000000000000, 0.9659258262890683122, 1.000000000000000000, 0.9659258262890683122, 1.000000000000000000, 0.9659258262890683122, 1.000000000000000000, 0.9659258262890683122, 1.000000000000000000, 0.9659258262890683122, 1.000000000000000000, 0.9659258262890683122, 1.000000000000000000, 0.9659258262890683122, 1.000000000000000000, 0.9659258262890683122, 1.000000000000000000, 0.9659258262890683122, 1.000000000000000000, 0.9659258262890683122, 1.000000000000000000, 0.9659258262890683122, 1.000000000000000000, 0.9659258262890683122, 1.000000000000000000, 0.9659258262890683122, 1.000000000000000000, 0.9659258262890683122, 1.000000000000000000, 0.9659258262890683122, 1.000000000000000000, 0.9659258262890683122, 1.000000000000000000, 0.9659258262890683122, 1.000000000000000000, 0.9659258262890683122, 1.000000000000000000, 0.9659258262890683122, 1.000000000000000000, 0.9659258262890683122, 1.000000000000000000, 0.9659258262890683122, 1.000000000000000000, 0.9659258262890683122, 1.000000000000000000, 0.9659258262890683122, 1.000000000000000000, 0.9659258262890683122, 1.000000000000000000, 0.9659258262890683122, 1.000000000000000000, 0.9659258262890683122, 1.000000000000000000, 0.9659258262890683122, 1.000000000000000000, 0.9659258262890683122, 1.000000000000000000, 0.9659258262890683122, 1.000000000000000000, 0.9659258262890683122, 1.000000000000000000, 0.9659258262890683122, 1.000000000000000000, 0.9659258262890683122, 1.000000000000000000, 0.9659258262890683122, 1.000000000000000000, 0.9659258262890683122, 1.000000000000000000, 0.9659258262890683122, 1.000000000000000000, 0.9659258262890683122, 1.000000000000000000, 0.9659258262890683122, 1.000000000000000000, 0.9659258262890683122, 1.000000000000000000, 0.9659258262890683122, 1.000000000000000000, 0.9659258262890683122, 1.000000000000000000, 0.9659258262890683122, 1.000000000000000000, 0.9659258262890683122, 1.000000000000000000, 0.9659258262890683122, 1.000000000000000000, 0.9659258262890683122, 1.000000000000000000, 0.9659258262890683122, 1.000000000000000000, 0.9659258262890683122, 1.000000000000000000, 0.9659258262890683122, 1.000000000000000000, 0.9659258262890683122, 1.000000000000000000, 0.9659258262890683122, 1.000000000000000000, 0.9659258262890683122, 1.000000000000000000, 0.9659258262890683122, 1.000000000000000000, 0.9659258262890683122, 1.000000000000000000, 0.9659258262890683122, 1.000000000000000000, 0.9659258262890683122, 1.000000000000000000, 0.9659258262890683122, 1.000000000000000000, 0.9659258262890683122, 1.000000000000000000, 0.9659258262890683122, 1.000000000000000000, 0.9659258262890683122, 1.000000000000000000, 0.9659258262890683122, 1.000000000000000000, 0.9659258262890683122, 1.000000000000000000, 0.9659258262890683122, 1.000000000000000000, 0.9659258262890683122, 1.000000000000000000, 0.9659258262890683122, 1.000000000000000000, 0.9659258262890683122, 1.000000000000000000, 0.9659258262890683122, 1.000000000000000000, 0.9659258262890683122, 1.000000000000000000, 0.9659258262890683122, 1.000000000000000000, 0.9659258262890683122, 1.000000000000000000, 0.9659258262890683122, 1.000000000000000000, 0.9659258262890683122, 1.000000000000000000, 0.9659258262890683122, 1.000000000000000000, 0.9659258262890683122, 1.000000000000000000, 0.9659258262890683122, 1.000000000000000000, 0.9659258262890683122, 1.000000000000000000, 0.9659258262890683122, 1.000000000000000000, 0.9659258262890683122, 1.000000000000000000, 0.9659258262890683122, 1.000000000000000000, 0.9659258262890683122, 1.000000000000000000, 0.9659258262890683122, 1.000000000000000000, 0.9659258262890683122, 1.000000000000000000, 0.9659258262890683122, 1.000000000000000000, 0.9659258262890683122, 1.000000000000000000, 0.9659258262890683122, 1.000000000000000000, 0.9659258262890683122, 1.000000000000000000, 0.9659258262890683122, 1.000000000000000000, 0.9659258262890683122, 1.000000000000000000, 0.9659258262890683122, 1.000000000000000000, 0.9659258262890683122, 1.000000000000000000, 0.9659258262890683122, 1.000000000000000000, 0.9659258262890683122, 1.000000000000000000, 0.9659258262890683122, 1.000000000000000000, 0.9659258262890683122, 1.000000000000000000, 0.9659258262890683122, 1.000000000000000000, 0.9659258262890683122, 1.000000000000000000, 0.9659258262890683122, 1.000000000000000000, 0.9659258262890683122, 1.000000000000000000, 0.9659258262890683122, 1.000000000000000000, 0.9659258262890683122, 1.000000000000000000, 0.9659258262890683122, 1.000000000000000000, 0.9659258262890683122, 1.000000000000000000, 0.9659258262890683122, 1.000000000000000000, 0.9659258262890683122, 1.000000000000000000, 0.9659258262890683122, 1.000000000000000000, 0.9659258262890683122, 1.000000000000000000, 0.9659258262890683122, 1.000000000000000000, 0.9659258262890683122, 1.000000000000000000, 0.9659258262890683122, 1.000000000000000000, 0.9659258262890683122, 1.000000000000000000, 0.9659258262890683122, 1.000000000000000000, 0.9659258262890683122, 1.000000000000000000, 0.9659258262890683122, 1.000000000000000000, 0.9659258262890683122, 1.000000000000000000, 0.9659258262890683122, 1.000000000000000000, 0.9659258262890683122, 1.000000000000000000, 0.9659258262890683122, 1.000000000000000000, 0.9659258262890683122, 1.000000000000000000, 0.9659258262890683122, 1.000000000000000000, 0.9659258262890683122, 1.000000000000000000),
 ( 1.000000000000000000, 0.9659258262890683122, 1.000000000000000000, 0.9659258262890683122, 1.000000000000000000, 0.9659258262890683122, 1.000000000000000000, 0.9659258262890683122, 1.000000000000000000, 0.9659258262890683122, 1.000000000000000000, 0.9659258262890683122, 1.000000000000000000, 0.9659258262890683122, 1.000000000000000000, 0.9659258262890683122, 1.000000000000000000, 0.9659258262890683122, 1.000000000000000000, 0.9659258262890683122, 1.000000000000000000, 0.9659258262890683122, 1.000000000000000000, 0.9659258262890683122, 1.000000000000000000, 0.9659258262890683122, 1.000000000000000000, 0.9659258262890683122, 1.000000000000000000, 0.9659258262890683122, 1.000000000000000000, 0.9659258262890683122, 1.000000000000000000, 0.9659258262890683122, 1.000000000000000000, 0.9659258262890683122, 1.000000000000000000, 0.9659258262890683122, 1.000000000000000000, 0.9659258262890683122, 1.000000000000000000, 0.9659258262890683122, 1.000000000000000000, 0.9659258262890683122, 1.000000000000000000, 0.9659258262890683122, 1.000000000000000000, 0.9659258262890683122, 1.000000000000000000, 0.9659258262890683122, 1.000000000000000000, 0.9659258262890683122, 1.000000000000000000, 0.9659258262890683122, 1.000000000000000000, 0.9659258262890683122, 1.000000000000000000, 0.9659258262890683122, 1.000000000000000000, 0.9659258262890683122, 1.000000000000000000, 0.9659258262890683122, 1.000000000000000000, 0.9659258262890683122, 1.000000000000000000, 0.9659258262890683122, 1.000000000000000000, 0.9659258262890683122, 1.000000000000000000, 0.9659258262890683122, 1.000000000000000000, 0.9659258262890683122, 1.000000000000000000, 0.9659258262890683122, 1.000000000000000000, 0.9659258262890683122, 1.000000000000000000, 0.9659258262890683122, 1.000000000000000000, 0.9659258262890683122, 1.000000000000000000, 0.9659258262890683122, 1.000000000000000000, 0.9659258262890683122, 1.000000000000000000, 0.9659258262890683122, 1.000000000000000000, 0.9659258262890683122, 1.000000000000000000, 0.9659258262890683122, 1.000000000000000000, 0.9659258262890683122, 1.000000000000000000, 0.9659258262890683122, 1.000000000000000000, 0.9659258262890683122, 1.000000000000000000, 0.9659258262890683122, 1.000000000000000000, 0.9659258262890683122, 1.000000000000000000, 0.9659258262890683122, 1.000000000000000000, 0.9659258262890683122, 1.000000000000000000, 0.9659258262890683122, 1.000000000000000000, 0.9659258262890683122, 1.000000000000000000, 0.9659258262890683122, 1.000000000000000000, 0.9659258262890683122, 1.000000000000000000, 0.9659258262890683122, 1.000000000000000000, 0.9659258262890683122, 1.000000000000000000, 0.9659258262890683122, 1.000000000000000000, 0.9659258262890683122, 1.000000000000000000, 0.9659258262890683122, 1.000000000000000000, 0.9659258262890683122, 1.000000000000000000, 0.9659258262890683122, 1.000000000000000000, 0.9659258262890683122, 1.000000000000000000, 0.9659258262890683122, 1.000000000000000000, 0.9659258262890683122, 1.000000000000000000, 0.9659258262890683122, 1.000000000000000000, 0.9659258262890683122, 1.000000000000000000, 0.9659258262890683122, 1.000000000000000000, 0.9659258262890683122, 1.000000000000000000, 0.9659258262890683122, 1.000000000000000000, 0.9659258262890683122, 1.000000000000000000, 0.9659258262890683122, 1.000000000000000000, 0.9659258262890683122, 1.000000000000000000, 0.9659258262890683122, 1.000000000000000000, 0.9659258262890683122, 1.000000000000000000, 0.9659258262890683122, 1.000000000000000000, 0.9659258262890683122, 1.000000000000000000, 0.9659258262890683122, 1.000000000000000000, 0.9659258262890683122, 1.000000000000000000, 0.9659258262890683122, 1.000000000000000000, 0.9659258262890683122, 1.000000000000000000, 0.9659258262890683122, 1.000000000000000000, 0.9659258262890683122, 1.000000000000000000, 0.9659258262890683122, 1.000000000000000000, 0.9659258262890683122, 1.000000000000000000, 0.9659258262890683122, 1.000000000000000000, 0.9659258262890683122, 1.000000000000000000, 0.9659258262890683122, 1.000000000000000000, 0.9659258262890683122, 1.000000000000000000, 0.9659258262890683122, 1.000000000000000000, 0.9659258262890683122, 1.000000000000000000, 0.9659258262890683122, 1.000000000000000000, 0.9659258262890683122, 1.000000000000000000, 0.9659258262890683122, 1.000000000000000000, 0.9659258262890683122, 1.000000000000000000, 0.9659258262890683122, 1.000000000000000000, 0.9659258262890683122, 1.000000000000000000, 0.9659258262890683122, 1.000000000000000000, 0.9659258262890683122, 1.000000000000000000, 0.9659258262890683122, 1.000000000000000000, 0.9659258262890683122, 1.000000000000000000, 0.9659258262890683122, 1.000000000000000000, 0.9659258262890683122, 1.000000000000000000, 0.9659258262890683122, 1.000000000000000000, 0.9659258262890683122, 1.000000000000000000, 0.9659258262890683122, 1.000000000000000000, 0.9659258262890683122, 1.000000000000000000, 0.9659258262890683122, 1.000000000000000000, 0.9659258262890683122, 1.000000000000000000, 0.9659258262890683122, 1.000000000000000000, 0.9659258262890683122, 1.000000000000000000, 0.9659258262890683122, 1.000000000000000000, 0.9659258262890683122, 1.000000000000000000, 0.9659258262890683122, 1.000000000000000000, 0.9659258262890683122, 1.000000000000000000, 0.9659258262890683122, 1.000000000000000000, 0.9659258262890683122, 1.000000000000000000, 0.9659258262890683122, 1.000000000000000000, 0.9659258262890683122, 1.000000000000000000, 0.9659258262890683122, 1.000000000000000000, 0.9659258262890683122, 1.000000000000000000, 0.9659258262890683122, 1.000000000000000000, 0.9659258262890683122, 1.000000000000000000, 0.9659258262890683122, 1.000000000000000000, 0.9659258262890683122, 1.000000000000000000, 0.9659258262890683122, 1.000000000000000000, 0.9659258262890683122, 1.000000000000000000, 0.9659258262890683122, 1.000000000000000000, 0.9659258262890683122, 1.000000000000000000, 0.9659258262890683122, 1.000000000000000000, 0.9659258262890683122, 1.000000000000000000, 0.9659258262890683122, 1.000000000000000000, 0.9659258262890683122, 1.000000000000000000, 0.9659258262890683122, 1.000000000000000000, 0.9659258262890683122, 1.000000000000000000, 0.9659258262890683122, 1.000000000000000000, 0.9659258262890683122, 1.000000000000000000, 0.9659258262890683122, 1.000000000000000000, 0.9659258262890683122, 1.000000000000000000, 0.9659258262890683122, 1.000000000000000000, 0.9659258262890683122, 1.000000000000000000, 0.9659258262890683122, 1.000000000000000000, 0.9659258262890683122, 1.000000000000000000, 0.9659258262890683122, 1.000000000000000000, 0.9659258262890683122, 1.000000000000000000, 0.9659258262890683122, 1.000000000000000000, 0.9659258262890683122, 1.000000000000000000, 0.9659258262890683122, 1.000000000000000000, 0.9659258262890683122, 1.000000000000000000, 0.9659258262890683122, 1.000000000000000000, 0.9659258262890683122, 1.000000000000000000, 0.9659258262890683122, 1.000000000000000000, 0.9659258262890683122, 1.000000000000000000, 0.9659258262890683122, 1.000000000000000000, 0.9659258262890683122, 1.000000000000000000, 0.9659258262890683122, 1.000000000000000000, 0.9659258262890683122, 1.000000000000000000, 0.9659258262890683122, 1.000000000000000000, 0.9659258262890683122, 1.000000000000000000, 0.9659258262890683122, 1.000000000000000000, 0.9659258262890683122, 1.000000000000000000) ) ) 
 REPRESENTATION_ITEM ( '' )  SURFACE ( )  );
#93074 = CARTESIAN_POINT ( 'NONE',  ( 2.035157376598824452, 48.68868534415483396, 7.964842623401179544 ) ) ;
#93075 = CARTESIAN_POINT ( 'NONE',  ( 17.96484262340118221, 61.18868534415482685, -7.964842623401177768 ) ) ;
#93076 = CARTESIAN_POINT ( 'NONE',  ( 12.80781515976310203, 0.000000000000000000, 6.246788841744411513 ) ) ;
#93077 = CARTESIAN_POINT ( 'NONE',  ( 17.96484262340118221, 6.188685344154837509, -7.964842623401177768 ) ) ;
#93078 = CARTESIAN_POINT ( 'NONE',  ( 0.1532563361054083140, 46.00893115100079456, 1.131784320476157264E-15 ) ) ;
#93080 = CARTESIAN_POINT ( 'NONE',  ( 18.52753015748617571, 23.09226448433411960, 4.923371831947298993 ) ) ;
#93079 = CARTESIAN_POINT ( 'NONE',  ( 15.44008868035555793, 21.39701867748817321, -9.422509992056140149 ) ) ;
#93081 = CARTESIAN_POINT ( 'NONE',  ( 10.00000000000000178, 20.37363466993042138, 12.81628187352647608 ) ) ;
#93082 = ORIENTED_EDGE ( 'NONE', *, *, #16714, .F. ) ;
#93083 = CARTESIAN_POINT ( 'NONE',  ( 10.00000000000000178, 44.31368534415484106, 10.88017736071110342 ) ) ;
#93085 = DIRECTION ( 'NONE',  ( -0.000000000000000000, -0.000000000000000000, 1.000000000000000000 ) ) ;
#93084 = CARTESIAN_POINT ( 'NONE',  ( 22.81628187352647785, 6.623634669930420493, 6.195893100308588602E-16 ) ) ;
#93086 = CARTESIAN_POINT ( 'NONE',  ( 12.91533473730992121, 9.522018677488171434, 10.88017736071110164 ) ) ;
#93087 = CARTESIAN_POINT ( 'NONE',  ( 17.96484262340118221, 44.93868534415483396, 7.964842623401181321 ) ) ;
#93088 = CARTESIAN_POINT ( 'NONE',  ( 13.79529636645031943, 50.34541550158064638, -14.16423886937409904 ) ) ;
#93089 = CARTESIAN_POINT ( 'NONE',  ( 18.52753015748618282, 38.92559781766745175, -4.923371831947291888 ) ) ;
#93090 = CARTESIAN_POINT ( 'NONE',  ( 12.91533473730992121, 54.52201867748816255, 10.88017736071110164 ) ) ;
#93091 = CARTESIAN_POINT ( 'NONE',  ( 64.56412365047462742, 13.99999999999999467, 9.500000000000000000 ) ) ;
#93092 = CARTESIAN_POINT ( 'NONE',  ( 24.16423886937410614, 14.51208216824730179, -3.795296366450302550 ) ) ;
#93093 = UNCERTAINTY_MEASURE_WITH_UNIT (LENGTH_MEASURE( 1.000000000000000082E-05 ), #26035, 'distance_accuracy_value', 'NONE');
#93094 = FILL_AREA_STYLE_COLOUR ( '', #22626 ) ;
#93095 = DIRECTION ( 'NONE',  ( 0.6246950475544238435, 0.7808688094430307203, 0.000000000000000000 ) ) ;
#93096 = ORIENTED_EDGE ( 'NONE', *, *, #80127, .T. ) ;
#93097 = ORIENTED_EDGE ( 'NONE', *, *, #94597, .F. ) ;
#93098 = CARTESIAN_POINT ( 'NONE',  ( 20.36894250292379382, 38.67874883491396076, 10.36894250292379205 ) ) ;
#93099 = CARTESIAN_POINT ( 'NONE',  ( -4.164238869374098151, 36.59541550158063217, -3.795296366450310543 ) ) ;
#93100 = CARTESIAN_POINT ( 'NONE',  ( 2.035157376598822676, 67.43868534415484817, -7.964842623401177768 ) ) ;
#93101 = CARTESIAN_POINT ( 'NONE',  ( 0.1532563361054083140, 56.00893115100078745, 1.131784320476157264E-15 ) ) ;
#93102 = LINE ( 'NONE', #70618, #43436 ) ;
#93104 = CARTESIAN_POINT ( 'NONE',  ( 16.40814093676324603, 27.45696800326375708, -11.09922568453594671 ) ) ;
#93103 = CARTESIAN_POINT ( 'NONE',  ( -0.8801773607111008646, 58.27201867748816966, 2.915334737309923430 ) ) ;
#93105 = CARTESIAN_POINT ( 'NONE',  ( 2.917880565312950480, 25.97041550158063572, -12.26659068614894821 ) ) ;
#93106 = CARTESIAN_POINT ( 'NONE',  ( 12.91533473730992121, 24.52201867748816966, 10.88017736071110164 ) ) ;
#93107 = AXIS2_PLACEMENT_3D ( 'NONE', #96617, #59582, #4136 ) ;
#93108 = COLOUR_RGB ( '', 0.31764706, 0.68627451, 0.89019608) ;
#93109 = CYLINDRICAL_SURFACE ( 'NONE', #44358, 15.00000000000000000 ) ;
#93110 = CARTESIAN_POINT ( 'NONE',  ( 7.084665262690076126, 64.10535201082150536, 10.88017736071109987 ) ) ;
#93111 = AXIS2_PLACEMENT_3D ( 'NONE', #98647, #44618, #75610 ) ;
#93112 = CARTESIAN_POINT ( 'NONE',  ( 7.208316651077764980, -12.11606884899921255, 7.208316651077762316 ) ) ;
#93113 = EDGE_LOOP ( 'NONE', ( #17755, #32876, #33359, #29401 ) ) ;
#93114 = CARTESIAN_POINT ( 'NONE',  ( 10.82078848414219330, 15.00000000000000000, -11.78082904627298433 ) ) ;
#93115 = AXIS2_PLACEMENT_3D ( 'NONE', #66833, #58330, #51341 ) ;
#93116 =( NAMED_UNIT ( * ) PLANE_ANGLE_UNIT ( ) SI_UNIT ( $, .RADIAN. ) );
#93117 = ORIENTED_EDGE ( 'NONE', *, *, #86594, .T. ) ;
#93119 = CARTESIAN_POINT ( 'NONE',  ( 2.035157376598822676, 17.43868534415483751, -7.964842623401177768 ) ) ;
#93118 = CARTESIAN_POINT ( 'NONE',  ( -0.8801773607110991993, 7.855352010821506248, -2.915334737309923874 ) ) ;
#93121 = CARTESIAN_POINT ( 'NONE',  ( 19.84674366389459266, 58.71726448433411605, -2.638427012816827677 ) ) ;
#93120 = CARTESIAN_POINT ( 'NONE',  ( 0.1532563361054100626, 40.80059781766745886, -2.638427012816831230 ) ) ;
#93122 = CARTESIAN_POINT ( 'NONE',  ( 0.000000000000000000, 15.00000000000000000, 0.000000000000000000 ) ) ;
#93123 = CARTESIAN_POINT ( 'NONE',  ( 6.880000000000011440, 40.74999999999999289, -4.250000000000000000 ) ) ;
#93124 = EDGE_CURVE ( 'NONE', #3849, #79719, #10562, .T. ) ;
#93125 = ADVANCED_FACE ( 'NONE', ( #50525 ), #54031, .T. ) ;
#93126 = CARTESIAN_POINT ( 'NONE',  ( 13.43411237798105340, 5.581968003263753531, 12.81628187352647963 ) ) ;
#93127 = VERTEX_POINT ( 'NONE', #51659 ) ;
#93128 = CARTESIAN_POINT ( 'NONE',  ( 17.08211943468705130, 43.47041550158063927, 12.26659068614894998 ) ) ;
#93129 = VERTEX_POINT ( 'NONE', #43650 ) ;
#93130 = CARTESIAN_POINT ( 'NONE',  ( -0.3689425029237898834, 46.17874883491397497, -10.36894250292378850 ) ) ;
#93131 = ORIENTED_EDGE ( 'NONE', *, *, #48685, .T. ) ;
#93132 = CARTESIAN_POINT ( 'NONE',  ( 17.96484262340118221, 26.18868534415483396, -7.964842623401177768 ) ) ;
#93133 = DIRECTION ( 'NONE',  ( 0.1650476058606878405, 0.000000000000000000, -0.9862856015372296614 ) ) ;
#93134 = CARTESIAN_POINT ( 'NONE',  ( 10.00000000000000000, 36.81368534415484106, -10.88017736071110342 ) ) ;
#93135 = CARTESIAN_POINT ( 'NONE',  ( 14.92337183194729633, 52.67559781766745175, 8.527530157486181039 ) ) ;
#93136 = CARTESIAN_POINT ( 'NONE',  ( 20.88017736071110875, 35.77201867748816966, -2.915334737309920765 ) ) ;
#93137 = CARTESIAN_POINT ( 'NONE',  ( 15.44008868035555793, 61.39701867748817676, -9.422509992056140149 ) ) ;
#93138 = CARTESIAN_POINT ( 'NONE',  ( 4.559911319644449179, 33.89701867748817676, 9.422509992056141925 ) ) ;
#93139 = CIRCLE ( 'NONE', #38843, 0.5000000000000004441 ) ;
#93141 = ORIENTED_EDGE ( 'NONE', *, *, #47309, .F. ) ;
#93140 = PLANE ( 'NONE',  #58472 ) ;
#93142 = CIRCLE ( 'NONE', #97967, 0.5000000000000004441 ) ;
#93143 = ADVANCED_FACE ( 'NONE', ( #50164 ), #66656, .F. ) ;
#93144 = CARTESIAN_POINT ( 'NONE',  ( 7.361572987183169658, 4.967264484334119601, -9.846743663894592657 ) ) ;
#93145 = DIRECTION ( 'NONE',  ( -0.7971177707001109169, -0.6038238647437560447, -1.358445972092650111E-13 ) ) ;
#93146 = ORIENTED_EDGE ( 'NONE', *, *, #18270, .F. ) ;
#93147 = DIRECTION ( 'NONE',  ( -1.000000000000000000, 0.000000000000000000, 0.000000000000000000 ) ) ;
#93148 = CARTESIAN_POINT ( 'NONE',  ( 19.84674366389459266, 43.30059781766744464, 2.638427012816836559 ) ) ;
#93149 = DIRECTION ( 'NONE',  ( 0.000000000000000000, 0.000000000000000000, 1.000000000000000000 ) ) ;
#93150 = EDGE_CURVE ( 'NONE', #82102, #96688, #539, .T. ) ;
#93151 = CARTESIAN_POINT ( 'NONE',  ( -51.18902439024388684, 40.95121951219505974, -8.000000000000000000 ) ) ;
#93152 = CARTESIAN_POINT ( 'NONE',  ( 5.171435456984235124, 0.000000000000000000, -1.730338099013976727 ) ) ;
#93153 = ORIENTED_EDGE ( 'NONE', *, *, #2661, .T. ) ;
#93154 = DIRECTION ( 'NONE',  ( 0.000000000000000000, 0.000000000000000000, 1.000000000000000000 ) ) ;
#93155 = CARTESIAN_POINT ( 'NONE',  ( 9.879999999999990123, 20.99999999999999645, 1.249999999999987121 ) ) ;
#93156 = CARTESIAN_POINT ( 'NONE',  ( 14.92337183194729633, 47.67559781766745175, 8.527530157486181039 ) ) ;
#93157 = CARTESIAN_POINT ( 'NONE',  ( 24.16423886937409904, 49.09541550158063217, 3.795296366450317205 ) ) ;
#93158 = CARTESIAN_POINT ( 'NONE',  ( 10.00000000000000178, 57.25893115100078745, 9.846743663894594434 ) ) ;
#93159 = VERTEX_POINT ( 'NONE', #38511 ) ;
#93160 = CARTESIAN_POINT ( 'NONE',  ( 19.84674366389459621, 18.50893115100078745, 7.409399052514197653E-17 ) ) ;
#93161 = CARTESIAN_POINT ( 'NONE',  ( 16.40814093676324603, 57.45696800326375353, -11.09922568453594671 ) ) ;
#93162 = CARTESIAN_POINT ( 'NONE',  ( 0.1532563361054083140, 56.00893115100078745, 1.131784320476157264E-15 ) ) ;
#93163 = CARTESIAN_POINT ( 'NONE',  ( -0.8801773607111009756, 58.06368534415484106, 1.068504757029289695E-15 ) ) ;
#93164 = CARTESIAN_POINT ( 'NONE',  ( 19.39188664607694790, 30.83703382326399378, -6.499999999999962697 ) ) ;
#93165 = STYLED_ITEM ( 'NONE', ( #70841 ), #96833 ) ;
#93166 = ORIENTED_EDGE ( 'NONE', *, *, #78458, .T. ) ;
#93167 = CARTESIAN_POINT ( 'NONE',  ( -4.164238869374099039, 66.80374883491396076, 8.674139862899312516E-16 ) ) ;
#93168 = DIRECTION ( 'NONE',  ( 0.000000000000000000, 0.000000000000000000, 1.000000000000000000 ) ) ;
#93169 = CARTESIAN_POINT ( 'NONE',  ( 10.00000000000000000, 26.81368534415484106, -10.88017736071110342 ) ) ;
#93171 = CARTESIAN_POINT ( 'NONE',  ( 2.035157376598822676, 57.43868534415484106, -7.964842623401177768 ) ) ;
#93170 = CARTESIAN_POINT ( 'NONE',  ( 10.00000000000000000, 12.87363466993042138, -12.81628187352647608 ) ) ;
#93172 = CARTESIAN_POINT ( 'NONE',  ( -0.3289641300567998083, 63.07879003517447103, 5.963430220938281678 ) ) ;
#93173 = CARTESIAN_POINT ( 'NONE',  ( 3.969999999999999751, 10.25000000000000000, -2.750000000000000000 ) ) ;
#93174 = DIRECTION ( 'NONE',  ( -0.9366721892483947931, 0.000000000000000000, -0.3502073812594747593 ) ) ;
#93176 = CARTESIAN_POINT ( 'NONE',  ( -14.11917416961171945, 14.76930270348881002, 4.887430353538848138 ) ) ;
#93175 = CARTESIAN_POINT ( 'NONE',  ( 2.035157376598822676, 52.43868534415483396, -7.964842623401177768 ) ) ;
#93177 = CARTESIAN_POINT ( 'NONE',  ( 1.472469842513823179, 35.59226448433412315, -4.923371831947296329 ) ) ;
#93178 = CARTESIAN_POINT ( 'NONE',  ( 19.84674366389459621, 3.508931151000785231, 7.409399052514197653E-17 ) ) ;
#93179 = CARTESIAN_POINT ( 'NONE',  ( -14.16423886937410437, 31.59541550158062861, -3.795296366450299885 ) ) ;
#93180 = CARTESIAN_POINT ( 'NONE',  ( 13.43411237798106583, 2.665301336597086568, -12.81628187352647252 ) ) ;
#93182 = CARTESIAN_POINT ( 'NONE',  ( 1.932340009482190313, 66.49127512925448968, -6.500000000000079048 ) ) ;
#93181 = CARTESIAN_POINT ( 'NONE',  ( 0.5774900079438607392, 18.48035201082150536, 5.440088680355550821 ) ) ;
#93183 = CARTESIAN_POINT ( 'NONE',  ( -4.164238869374099039, 41.80374883491397497, 8.674139862899312516E-16 ) ) ;
#93184 = ADVANCED_FACE ( 'NONE', ( #58147 ), #69009, .T. ) ;
#93185 = CARTESIAN_POINT ( 'NONE',  ( 22.26659068614894466, 33.88708216824730357, 7.082119434687054849 ) ) ;
#93186 = CARTESIAN_POINT ( 'NONE',  ( 0.5774900079438590739, 2.647018677488171434, -5.440088680355550821 ) ) ;
#93187 = CARTESIAN_POINT ( 'NONE',  ( 12.63842701281683034, 17.46726448433411250, 9.846743663894596210 ) ) ;
#93188 = CARTESIAN_POINT ( 'NONE',  ( 12.91533473730992121, 19.52201867748816611, 10.88017736071110164 ) ) ;
#93189 = ORIENTED_EDGE ( 'NONE', *, *, #73026, .T. ) ;
#93190 = CARTESIAN_POINT ( 'NONE',  ( 14.92337183194729988, 44.34226448433412315, -8.527530157486177487 ) ) ;
#93191 = CARTESIAN_POINT ( 'NONE',  ( 17.96484262340118221, 34.93868534415482685, 7.964842623401181321 ) ) ;
#93192 = CARTESIAN_POINT ( 'NONE',  ( 2.791683348922240793, 61.63393115100079456, 7.208316651077764092 ) ) ;
#93194 = CARTESIAN_POINT ( 'NONE',  ( 1.959929470562281395, 60.51528370094807485, -5.767676674365853629 ) ) ;
#93193 = CARTESIAN_POINT ( 'NONE',  ( 6.204703633549690345, 17.84541550158063217, 14.16423886937410082 ) ) ;
#93195 = CARTESIAN_POINT ( 'NONE',  ( -13.78891971893204804, 14.49999999999999112, -5.904717858191772528 ) ) ;
#93196 = UNCERTAINTY_MEASURE_WITH_UNIT (LENGTH_MEASURE( 1.000000000000000082E-05 ), #25423, 'distance_accuracy_value', 'NONE');
#93197 = CARTESIAN_POINT ( 'NONE',  ( 7.361572987183169658, 9.967264484334119601, -9.846743663894592657 ) ) ;
#93198 = CARTESIAN_POINT ( 'NONE',  ( 6.565887622018943937, 50.16530133659708213, 12.81628187352647430 ) ) ;
#93199 = CARTESIAN_POINT ( 'NONE',  ( 17.20831665107776587, 54.13393115100079456, -7.208316651077762316 ) ) ;
#93200 = ORIENTED_EDGE ( 'NONE', *, *, #9817, .T. ) ;
#93201 = LINE ( 'NONE', #48686, #58893 ) ;
#93202 = DIRECTION ( 'NONE',  ( 1.000000000000000000, 1.257402221000611116E-16, -0.000000000000000000 ) ) ;
#93203 = CARTESIAN_POINT ( 'NONE',  ( 22.26659068614895176, 64.72041550158064638, -7.082119434687042414 ) ) ;
#93204 = CARTESIAN_POINT ( 'NONE',  ( 15.44008868035555260, 54.73035201082150536, 9.422509992056143702 ) ) ;
#93205 = CARTESIAN_POINT ( 'NONE',  ( 22.26659068614894466, 8.887082168247300018, 7.082119434687054849 ) ) ;
#93206 = CARTESIAN_POINT ( 'NONE',  ( 17.96484262340118221, 61.18868534415482685, -7.964842623401177768 ) ) ;
#93207 = CARTESIAN_POINT ( 'NONE',  ( 1.472469842513823179, 36.42559781766745175, 4.923371831947296329 ) ) ;
#93208 = CARTESIAN_POINT ( 'NONE',  ( 7.084665262690076126, 14.10535201082150358, 10.88017736071109987 ) ) ;
#93209 = CARTESIAN_POINT ( 'NONE',  ( 0.000000000000000000, 15.00000000000000000, 0.000000000000000000 ) ) ;
#93210 = CARTESIAN_POINT ( 'NONE',  ( 10.00000000000000000, 59.75893115100078745, -9.846743663894594434 ) ) ;
#93211 = CARTESIAN_POINT ( 'NONE',  ( 5.076628168052703671, 1.842264484334118047, 8.527530157486179263 ) ) ;
#93212 = UNCERTAINTY_MEASURE_WITH_UNIT (LENGTH_MEASURE( 1.000000000000000082E-05 ), #69301, 'distance_accuracy_value', 'NONE');
#93213 = ORIENTED_EDGE ( 'NONE', *, *, #36345, .F. ) ;
#93214 = VERTEX_POINT ( 'NONE', #31961 ) ;
#93215 = CARTESIAN_POINT ( 'NONE',  ( -3.949999999999997069, 99.99999999999998579, -8.000000000000000000 ) ) ;
#93216 = CARTESIAN_POINT ( 'NONE',  ( 12.60874940350940321, 15.00000000000000000, 7.160268045227115685 ) ) ;
#93217 = CARTESIAN_POINT ( 'NONE',  ( -11.81797300553251162, -43.76346696326814367, -3.750000000000000000 ) ) ;
#93218 = CARTESIAN_POINT ( 'NONE',  ( 6.204703633549690345, 47.84541550158064638, 14.16423886937410082 ) ) ;
#93219 = CARTESIAN_POINT ( 'NONE',  ( 0.1532563361054083140, 41.00893115100078745, 1.131784320476157264E-15 ) ) ;
#93220 = CARTESIAN_POINT ( 'NONE',  ( 7.361572987183169658, 19.96726448433411960, -9.846743663894592657 ) ) ;
#93221 = CARTESIAN_POINT ( 'NONE',  ( 0.1089645850229087609, 38.16234555792571115, 6.479102184480833415 ) ) ;
#93223 = CARTESIAN_POINT ( 'NONE',  ( 19.84674366389459621, 43.50893115100078745, 7.409399052514197653E-17 ) ) ;
#93222 = CARTESIAN_POINT ( 'NONE',  ( 10.00000000000000000, 16.81368534415483751, -10.88017736071110342 ) ) ;
#93224 = DIRECTION ( 'NONE',  ( 0.02617694830786938473, 0.000000000000000000, 0.9996573249755573709 ) ) ;
#93225 = CARTESIAN_POINT ( 'NONE',  ( 2.917880565312950480, 40.97041550158063217, -12.26659068614894821 ) ) ;
#93226 = CARTESIAN_POINT ( 'NONE',  ( -4.164238869374099927, 57.01208216824731068, 3.795296366450308767 ) ) ;
#93227 = CARTESIAN_POINT ( 'NONE',  ( 7.361572987183170547, 67.05059781766746596, 9.846743663894590881 ) ) ;
#93228 = EDGE_CURVE ( 'NONE', #52174, #89575, #60550, .T. ) ;
#93229 = CARTESIAN_POINT ( 'NONE',  ( -10.84451454131299997, 15.00000000000000000, 9.625305416633544553 ) ) ;
#93230 = CARTESIAN_POINT ( 'NONE',  ( -0.8801773607111009756, 48.06368534415484817, 1.068504757029289695E-15 ) ) ;
#93231 = CARTESIAN_POINT ( 'NONE',  ( 10.00000000000000000, 9.758931151000785675, -9.846743663894594434 ) ) ;
#93232 = CARTESIAN_POINT ( 'NONE',  ( -6.857667818328269327, -50.95147662124757915, 3.999999999999999112 ) ) ;
#93233 = ORIENTED_EDGE ( 'NONE', *, *, #42484, .F. ) ;
#93234 = CARTESIAN_POINT ( 'NONE',  ( 21.92686044187657046, 30.16212336850780673, 4.562052436263912550E-16 ) ) ;
#93235 = ORIENTED_EDGE ( 'NONE', *, *, #70253, .T. ) ;
#93236 = CARTESIAN_POINT ( 'NONE',  ( 17.20831665107776587, 12.88393115100078390, 7.208316651077764980 ) ) ;
#93237 = EDGE_LOOP ( 'NONE', ( #56351, #88866, #92967, #31134 ) ) ;
#93238 = CARTESIAN_POINT ( 'NONE',  ( 24.16423886937409904, 24.09541550158063927, 3.795296366450317205 ) ) ;
#93239 = CARTESIAN_POINT ( 'NONE',  ( 17.20831665107776587, 22.88393115100078745, 7.208316651077764980 ) ) ;
#93240 = CARTESIAN_POINT ( 'NONE',  ( 10.00000000000000000, 46.81368534415484106, -10.88017736071110342 ) ) ;
#93241 = CARTESIAN_POINT ( 'NONE',  ( 0.000000000000000000, 14.49999999999999822, 0.000000000000000000 ) ) ;
#93242 = EDGE_CURVE ( 'NONE', #28267, #94977, #37322, .T. ) ;
#93243 = ORIENTED_EDGE ( 'NONE', *, *, #82866, .F. ) ;
#93244 = CARTESIAN_POINT ( 'NONE',  ( 12.91533473730992121, 44.52201867748816966, 10.88017736071110164 ) ) ;
#93245 = CARTESIAN_POINT ( 'NONE',  ( 20.10239578412224759, 37.63377557478296609, -6.340343622311915617 ) ) ;
#93246 = CIRCLE ( 'NONE', #91614, 15.00000000000000000 ) ;
#93247 = EDGE_CURVE ( 'NONE', #9027, #16419, #55973, .T. ) ;
#93248 = ADVANCED_FACE ( 'NONE', ( #63932 ), #84501, .F. ) ;
#93249 = CARTESIAN_POINT ( 'NONE',  ( 6.408140936763243367, 0.7903013365970906756, 11.09922568453594494 ) ) ;
#93250 = ORIENTED_EDGE ( 'NONE', *, *, #58058, .T. ) ;
#93251 = CARTESIAN_POINT ( 'NONE',  ( 10.00000000000000000, 46.81368534415484106, -10.88017736071110342 ) ) ;
#93252 = CARTESIAN_POINT ( 'NONE',  ( 10.00000000000000000, 0.5537488349139675359, -14.16423886937410082 ) ) ;
#93253 = MECHANICAL_DESIGN_GEOMETRIC_PRESENTATION_REPRESENTATION (  '', ( #32584 ), #54912 ) ;
#93254 = ORIENTED_EDGE ( 'NONE', *, *, #93150, .T. ) ;
#93255 = CARTESIAN_POINT ( 'NONE',  ( 10.00000000000000178, 25.37363466993041783, 12.81628187352647608 ) ) ;
#93256 = CARTESIAN_POINT ( 'NONE',  ( -2.266590686148945544, 1.387082168247301128, -7.082119434687050408 ) ) ;
#93257 = CARTESIAN_POINT ( 'NONE',  ( 17.20831665107776587, 12.88393115100078390, 7.208316651077764980 ) ) ;
#93258 = CARTESIAN_POINT ( 'NONE',  ( 15.44008868035555260, 4.730352010821504471, 9.422509992056143702 ) ) ;
#93259 = CARTESIAN_POINT ( 'NONE',  ( -2.816281873526473856, 44.33196800326375353, 3.434112377981055619 ) ) ;
#93260 = LINE ( 'NONE', #84784, #4855 ) ;
#93261 = CARTESIAN_POINT ( 'NONE',  ( 7.361572987183169658, 9.967264484334119601, -9.846743663894592657 ) ) ;
#93262 = CARTESIAN_POINT ( 'NONE',  ( 12.91533473730993009, 41.60535201082149825, -10.88017736071109987 ) ) ;
#93263 = VERTEX_POINT ( 'NONE', #16001 ) ;
#93264 = ORIENTED_EDGE ( 'NONE', *, *, #8493, .T. ) ;
#93265 = ADVANCED_FACE ( 'NONE', ( #85980 ), #73975, .T. ) ;
#93266 = CARTESIAN_POINT ( 'NONE',  ( 1.711636803080571090, 46.84492782695772206, -6.500000000000077272 ) ) ;
#93267 = CARTESIAN_POINT ( 'NONE',  ( 10.00000000000000000, 61.81368534415484106, -10.88017736071110342 ) ) ;
#93268 = CARTESIAN_POINT ( 'NONE',  ( 9.322910753577883014, 0.04922511925147178558, 11.43369735623883621 ) ) ;
#93269 = CARTESIAN_POINT ( 'NONE',  ( -1.099225684535947600, 63.70696800326376774, -6.408140936763238038 ) ) ;
#93270 = CARTESIAN_POINT ( 'NONE',  ( 19.42250999205614548, 55.98035201082150536, -5.440088680355545492 ) ) ;
#93271 = CARTESIAN_POINT ( 'NONE',  ( 16.40814093676323893, 10.79030133659708923, 11.09922568453595026 ) ) ;
#93272 = EDGE_CURVE ( 'NONE', #79142, #49345, #77189, .T. ) ;
#93273 = LINE ( 'NONE', #47771, #59492 ) ;
#93274 = CARTESIAN_POINT ( 'NONE',  ( 0.1532563361054083140, 26.00893115100078745, 1.131784320476157264E-15 ) ) ;
#93275 = CARTESIAN_POINT ( 'NONE',  ( 6.879999999999995453, 43.00000000000000000, 4.000000000000000000 ) ) ;
#93276 = CARTESIAN_POINT ( 'NONE',  ( 13.79529636645030344, 8.262082168247300018, 14.16423886937410614 ) ) ;
#93277 = CARTESIAN_POINT ( 'NONE',  ( 0.1532563361054082862, 16.21726448433411960, 2.638427012816831674 ) ) ;
#93278 = CARTESIAN_POINT ( 'NONE',  ( 19.38216949554541202, 15.99863466993042138, 9.382169495545424454 ) ) ;
#93279 = LINE ( 'NONE', #8315, #13090 ) ;
#93280 = CARTESIAN_POINT ( 'NONE',  ( 20.88017736071110519, 45.56368534415484106, 2.639326808657452039E-16 ) ) ;
#93281 = CARTESIAN_POINT ( 'NONE',  ( 5.076628168052703671, 66.84226448433412315, 8.527530157486179263 ) ) ;
#93282 = CARTESIAN_POINT ( 'NONE',  ( -0.1503990784575247319, 32.22266099184917465, -6.262539305110083276 ) ) ;
#93283 = CARTESIAN_POINT ( 'NONE',  ( 18.52753015748618282, 33.92559781766745886, -4.923371831947291888 ) ) ;
#93284 = CARTESIAN_POINT ( 'NONE',  ( 10.00000000000000178, 22.25893115100078745, 9.846743663894594434 ) ) ;
#93285 = CARTESIAN_POINT ( 'NONE',  ( 7.084665262690076126, 19.10535201082150181, 10.88017736071109987 ) ) ;
#93286 = CARTESIAN_POINT ( 'NONE',  ( 16.40814093676323893, 10.79030133659708923, 11.09922568453595026 ) ) ;
#93287 = CARTESIAN_POINT ( 'NONE',  ( 0.1532563361054082862, 26.21726448433411605, 2.638427012816831674 ) ) ;
#93288 =( LENGTH_UNIT ( ) NAMED_UNIT ( * ) SI_UNIT ( .MILLI., .METRE. ) );
#93289 = CARTESIAN_POINT ( 'NONE',  ( -8.048010592883702685, 84.92462609336300261, 4.034077756265262771 ) ) ;
#93290 = CARTESIAN_POINT ( 'NONE',  ( 7.084665262690076126, 14.10535201082150358, 10.88017736071109987 ) ) ;
#93291 = ORIENTED_EDGE ( 'NONE', *, *, #90193, .T. ) ;
#93292 = CARTESIAN_POINT ( 'NONE',  ( -0.8801773607111008646, 63.27201867748817676, 2.915334737309923430 ) ) ;
#93293 = CARTESIAN_POINT ( 'NONE',  ( -0.2418659066527711621, 49.26028685723175471, -6.114288769123046308 ) ) ;
#93295 = CARTESIAN_POINT ( 'NONE',  ( 19.42250999205614548, 10.98035201082150536, -5.440088680355545492 ) ) ;
#93294 = CARTESIAN_POINT ( 'NONE',  ( 2.791683348922237240, 45.38393115100079456, -7.208316651077763204 ) ) ;
#93296 = DIRECTION ( 'NONE',  ( -1.000000000000000000, 0.000000000000000000, 0.000000000000000000 ) ) ;
#93297 = CARTESIAN_POINT ( 'NONE',  ( 0.5774900079438607392, 43.48035201082151247, 5.440088680355550821 ) ) ;
#93299 = FACE_OUTER_BOUND ( 'NONE', #22313, .T. ) ;
#93298 = CARTESIAN_POINT ( 'NONE',  ( 20.88017736071110519, 15.56368534415483751, 2.639326808657452039E-16 ) ) ;
#93300 = CARTESIAN_POINT ( 'NONE',  ( 10.00000000000000000, 14.75893115100078568, -9.846743663894594434 ) ) ;
#93301 = CARTESIAN_POINT ( 'NONE',  ( 10.00000000000000178, 32.25893115100078745, 9.846743663894594434 ) ) ;
#93302 = CARTESIAN_POINT ( 'NONE',  ( -16.80847703285585482, 99.89644660940670917, -8.000000000000001776 ) ) ;
#93303 = CARTESIAN_POINT ( 'NONE',  ( 0.000000000000000000, 0.5000000000000004441, 0.000000000000000000 ) ) ;
#93304 = CARTESIAN_POINT ( 'NONE',  ( 18.52753015748618282, 63.92559781766745886, -4.923371831947291888 ) ) ;
#93305 = CARTESIAN_POINT ( 'NONE',  ( -4.164238869374099927, 2.012082168247300906, 3.795296366450308767 ) ) ;
#93306 = CARTESIAN_POINT ( 'NONE',  ( 24.16423886937410614, 29.30374883491396787, 8.672049930838204340E-16 ) ) ;
#93307 = CARTESIAN_POINT ( 'NONE',  ( 14.92337183194729633, 32.67559781766745175, 8.527530157486181039 ) ) ;
#93308 = FACE_OUTER_BOUND ( 'NONE', #1435, .T. ) ;
#93309 = AXIS2_PLACEMENT_3D ( 'NONE', #65852, #28355, #35359 ) ;
#93310 = CARTESIAN_POINT ( 'NONE',  ( 13.79529636645031943, 55.34541550158062506, -14.16423886937409904 ) ) ;
#93311 = CARTESIAN_POINT ( 'NONE',  ( 17.20831665107776587, 22.88393115100078745, 7.208316651077764980 ) ) ;
#93313 = CARTESIAN_POINT ( 'NONE',  ( -10.00219152607946604, 88.91691738930978772, -5.623636179944087488 ) ) ;
#93312 = DIRECTION ( 'NONE',  ( -0.000000000000000000, -1.000000000000000000, -0.000000000000000000 ) ) ;
#93314 = CARTESIAN_POINT ( 'NONE',  ( 4.559911319644449179, 48.89701867748817676, 9.422509992056141925 ) ) ;
#93315 = DIRECTION ( 'NONE',  ( -0.8788171126619616080, 0.000000000000000000, -0.4771587602596153999 ) ) ;
#93316 = CARTESIAN_POINT ( 'NONE',  ( 20.88017736071110875, 20.77201867748816611, -2.915334737309920765 ) ) ;
#93317 = CARTESIAN_POINT ( 'NONE',  ( -2.816281873526473856, 44.33196800326375353, 3.434112377981055619 ) ) ;
#93318 = CARTESIAN_POINT ( 'NONE',  ( 13.43411237798106583, 17.66530133659708923, -12.81628187352647252 ) ) ;
#93319 = CARTESIAN_POINT ( 'NONE',  ( 9.879999999999990123, 20.99999999999999645, 2.900000000000000355 ) ) ;
#93320 = CARTESIAN_POINT ( 'NONE',  ( 12.63842701281683034, 12.46726448433411782, 9.846743663894596210 ) ) ;
#93321 = VERTEX_POINT ( 'NONE', #47472 ) ;
#93322 = AXIS2_PLACEMENT_3D ( 'NONE', #23116, #29592, #135 ) ;
#93323 = DIRECTION ( 'NONE',  ( -0.1132032137679106348, 0.000000000000000000, 0.9935718556765870124 ) ) ;
#93324 = CARTESIAN_POINT ( 'NONE',  ( -8.024359497401761132, 75.03672218798435267, -2.900000000000000799 ) ) ;
#93325 = CARTESIAN_POINT ( 'NONE',  ( -2.266590686148945544, 51.38708216824730357, -7.082119434687050408 ) ) ;
#93326 = CARTESIAN_POINT ( 'NONE',  ( 13.79529636645030344, 28.26208216824729647, 14.16423886937410614 ) ) ;
#93327 = CARTESIAN_POINT ( 'NONE',  ( 0.5774900079438607392, 23.48035201082150536, 5.440088680355550821 ) ) ;
#93328 = CARTESIAN_POINT ( 'NONE',  ( 15.44008868035555260, 54.73035201082150536, 9.422509992056143702 ) ) ;
#93329 = PLANE ( 'NONE',  #62270 ) ;
#93330 = CARTESIAN_POINT ( 'NONE',  ( 6.284583270191197002, -88.40194713205143273, 4.000000000000000000 ) ) ;
#93331 = CARTESIAN_POINT ( 'NONE',  ( 0.5774900079438590739, 67.64701867748817676, -5.440088680355550821 ) ) ;
#93332 = SURFACE_SIDE_STYLE ('',( #78326 ) ) ;
#93333 = CARTESIAN_POINT ( 'NONE',  ( 2.791683348922237240, 25.38393115100078390, -7.208316651077763204 ) ) ;
#93334 = CARTESIAN_POINT ( 'NONE',  ( 2.148416515056627674, 62.23726573380440641, 6.499999999999959144 ) ) ;
#93335 = FACE_OUTER_BOUND ( 'NONE', #63107, .T. ) ;
#93336 = CARTESIAN_POINT ( 'NONE',  ( 14.92337183194729633, 22.67559781766745175, 8.527530157486181039 ) ) ;
#93337 = CARTESIAN_POINT ( 'NONE',  ( 0.1532563361054100626, 45.80059781766745886, -2.638427012816831230 ) ) ;
#93338 = CARTESIAN_POINT ( 'NONE',  ( 10.00000000000000000, 11.81368534415483751, -10.88017736071110342 ) ) ;
#93339 = UNCERTAINTY_MEASURE_WITH_UNIT (LENGTH_MEASURE( 1.000000000000000082E-05 ), #54088, 'distance_accuracy_value', 'NONE');
#93340 = CARTESIAN_POINT ( 'NONE',  ( -1.099225684535947600, 29.54030133659708923, 6.408140936763237150 ) ) ;
#93341 = CARTESIAN_POINT ( 'NONE',  ( -0.8801773607111009756, 53.06368534415484106, 1.068504757029289695E-15 ) ) ;
#93343 = CARTESIAN_POINT ( 'NONE',  ( 5.076628168052704559, 10.17559781766745175, -8.527530157486179263 ) ) ;
#93342 = CARTESIAN_POINT ( 'NONE',  ( 2.917880565312950480, 45.97041550158063927, -12.26659068614894821 ) ) ;
#93344 = CARTESIAN_POINT ( 'NONE',  ( 19.05914839598885635, 54.96693863883976405, 6.499999999999962697 ) ) ;
#93345 = CARTESIAN_POINT ( 'NONE',  ( 0.1532563361054082862, 51.21726448433412315, 2.638427012816831674 ) ) ;
#93346 = CARTESIAN_POINT ( 'NONE',  ( 18.52753015748617571, 38.09226448433412315, 4.923371831947298993 ) ) ;
#93347 = CARTESIAN_POINT ( 'NONE',  ( 22.26659068614895176, 19.72041550158063572, -7.082119434687042414 ) ) ;
#93348 = CARTESIAN_POINT ( 'NONE',  ( 10.00000000000000000, 34.75893115100078745, -9.846743663894594434 ) ) ;
#93349 = CARTESIAN_POINT ( 'NONE',  ( 12.91533473730992121, 49.52201867748817676, 10.88017736071110164 ) ) ;
#93350 = CARTESIAN_POINT ( 'NONE',  ( 19.42250999205614193, 10.14701867748816966, 5.440088680355555262 ) ) ;
#93351 = CARTESIAN_POINT ( 'NONE',  ( 0.5774900079438607392, 43.48035201082151247, 5.440088680355550821 ) ) ;
#93352 = CARTESIAN_POINT ( 'NONE',  ( 2.035157376598824452, 23.68868534415484461, 7.964842623401179544 ) ) ;
#93353 = ORIENTED_EDGE ( 'NONE', *, *, #40495, .F. ) ;
#93354 = EDGE_CURVE ( 'NONE', #39731, #47627, #11741, .T. ) ;
#93355 = CARTESIAN_POINT ( 'NONE',  ( 20.88017736071110875, 35.77201867748816966, -2.915334737309920765 ) ) ;
#93356 = ORIENTED_EDGE ( 'NONE', *, *, #90871, .F. ) ;
#93357 = CARTESIAN_POINT ( 'NONE',  ( 6.565887622018943937, 53.08196800326374643, -12.81628187352647608 ) ) ;
#93358 = DIRECTION ( 'NONE',  ( -0.000000000000000000, -1.000000000000000000, -0.000000000000000000 ) ) ;
#93359 = ORIENTED_EDGE ( 'NONE', *, *, #28024, .T. ) ;
#93361 = ADVANCED_FACE ( 'NONE', ( #77471 ), #74047, .T. ) ;
#93360 = CARTESIAN_POINT ( 'NONE',  ( 17.96484262340118221, 56.18868534415484817, -7.964842623401177768 ) ) ;
#93362 = CARTESIAN_POINT ( 'NONE',  ( 2.035157376598822676, 2.438685344154837953, -7.964842623401177768 ) ) ;
#93363 = CARTESIAN_POINT ( 'NONE',  ( 0.000000000000000000, 0.5000000000000004441, 0.000000000000000000 ) ) ;
#93364 = CARTESIAN_POINT ( 'NONE',  ( 24.16423886937409904, 54.09541550158063217, 3.795296366450317205 ) ) ;
#93365 = CARTESIAN_POINT ( 'NONE',  ( 2.791683348922240793, 1.633931151000784565, 7.208316651077764092 ) ) ;
#93366 = CARTESIAN_POINT ( 'NONE',  ( -2.266590686148945544, 7.220415501580634832, 7.082119434687048631 ) ) ;
#93367 = EDGE_CURVE ( 'NONE', #26718, #74552, #74454, .T. ) ;
#93368 = CARTESIAN_POINT ( 'NONE',  ( 19.84674366389459621, 3.508931151000785231, 7.409399052514197653E-17 ) ) ;
#93369 = CARTESIAN_POINT ( 'NONE',  ( 7.084665262690076126, 14.10535201082150358, 10.88017736071109987 ) ) ;
#93370 = CARTESIAN_POINT ( 'NONE',  ( 10.00000000000000000, 44.75893115100078745, -9.846743663894594434 ) ) ;
#93371 = ORIENTED_EDGE ( 'NONE', *, *, #31638, .F. ) ;
#93372 = CARTESIAN_POINT ( 'NONE',  ( 12.63842701281683034, 52.46726448433413026, 9.846743663894596210 ) ) ;
#93373 = DIRECTION ( 'NONE',  ( 0.000000000000000000, 0.000000000000000000, 1.000000000000000000 ) ) ;
#93374 =( GEOMETRIC_REPRESENTATION_CONTEXT ( 3 ) GLOBAL_UNCERTAINTY_ASSIGNED_CONTEXT ( ( #18201 ) ) GLOBAL_UNIT_ASSIGNED_CONTEXT ( ( #30257, #90265, #28782 ) ) REPRESENTATION_CONTEXT ( 'NONE', 'WORKASPACE' ) );
#93375 = CARTESIAN_POINT ( 'NONE',  ( 2.035157376598822676, 42.43868534415483396, -7.964842623401177768 ) ) ;
#93376 = CARTESIAN_POINT ( 'NONE',  ( 19.84674366389459621, 53.50893115100078745, 7.409399052514197653E-17 ) ) ;
#93378 = CARTESIAN_POINT ( 'NONE',  ( 0.5774900079438590739, 67.64701867748817676, -5.440088680355550821 ) ) ;
#93377 = CARTESIAN_POINT ( 'NONE',  ( 38.04706783004212411, -5.848780422071338384E-15, 7.000000000000000000 ) ) ;
#93379 = CARTESIAN_POINT ( 'NONE',  ( 12.91533473730993009, 46.60535201082150536, -10.88017736071109987 ) ) ;
#93380 = CARTESIAN_POINT ( 'NONE',  ( 13.79529636645030344, 58.26208216824728936, 14.16423886937410614 ) ) ;
#93381 =( GEOMETRIC_REPRESENTATION_CONTEXT ( 3 ) GLOBAL_UNCERTAINTY_ASSIGNED_CONTEXT ( ( #4516 ) ) GLOBAL_UNIT_ASSIGNED_CONTEXT ( ( #93288, #24324, #32777 ) ) REPRESENTATION_CONTEXT ( 'NONE', 'WORKASPACE' ) );
#93382 = CARTESIAN_POINT ( 'NONE',  ( 6.565887622018943937, 28.08196800326375353, -12.81628187352647608 ) ) ;
#93383 = DIRECTION ( 'NONE',  ( -0.000000000000000000, -1.000000000000000000, -0.000000000000000000 ) ) ;
#93384 = B_SPLINE_CURVE_WITH_KNOTS ( 'NONE', 3,
 ( #18071, #48551, #79556, #81878 ),
 .UNSPECIFIED., .F., .F.,
 ( 4, 4 ),
 ( 0.000000000000000000, 0.002657014572710779919 ),
 .UNSPECIFIED. ) ;
#93385 = ORIENTED_EDGE ( 'NONE', *, *, #81489, .F. ) ;
#93386 =( GEOMETRIC_REPRESENTATION_CONTEXT ( 3 ) GLOBAL_UNCERTAINTY_ASSIGNED_CONTEXT ( ( #22470 ) ) GLOBAL_UNIT_ASSIGNED_CONTEXT ( ( #95002, #87994, #79523 ) ) REPRESENTATION_CONTEXT ( 'NONE', 'WORKASPACE' ) );
#93387 = CARTESIAN_POINT ( 'NONE',  ( 6.565887622018943937, 23.08196800326375708, -12.81628187352647608 ) ) ;
#93388 = CARTESIAN_POINT ( 'NONE',  ( 17.96484262340118221, 14.93868534415483751, 7.964842623401181321 ) ) ;
#93390 = ORIENTED_EDGE ( 'NONE', *, *, #51139, .T. ) ;
#93389 = EDGE_CURVE ( 'NONE', #48771, #94701, #96440, .T. ) ;
#93391 = CARTESIAN_POINT ( 'NONE',  ( 0.5774900079438607392, 68.48035201082150536, 5.440088680355550821 ) ) ;
#93392 = CARTESIAN_POINT ( 'NONE',  ( 17.20831665107776587, 47.88393115100078745, 7.208316651077764980 ) ) ;
#93394 = CARTESIAN_POINT ( 'NONE',  ( 5.076628168052703671, 36.84226448433412315, 8.527530157486179263 ) ) ;
#93393 = CARTESIAN_POINT ( 'NONE',  ( 1.472469842513823179, 16.42559781766745175, 4.923371831947296329 ) ) ;
#93395 = CARTESIAN_POINT ( 'NONE',  ( 10.27090289957535596, 15.00000000000000711, -10.41235154178105127 ) ) ;
#93396 = CARTESIAN_POINT ( 'NONE',  ( -0.1298530154764001854, 80.39370036920264795, 5.000000000000000000 ) ) ;
#93397 = CARTESIAN_POINT ( 'NONE',  ( 0.1532563361054083140, 21.00893115100078745, 1.131784320476157264E-15 ) ) ;
#93398 = DIRECTION ( 'NONE',  ( 0.6087614290087297597, 0.000000000000000000, -0.7933533402912281707 ) ) ;
#93399 = FACE_OUTER_BOUND ( 'NONE', #85240, .T. ) ;
#93401 = DIRECTION ( 'NONE',  ( -0.000000000000000000, 1.000000000000000000, -0.000000000000000000 ) ) ;
#93400 = CARTESIAN_POINT ( 'NONE',  ( 1.472469842513823179, 26.42559781766745175, 4.923371831947296329 ) ) ;
#93402 = SURFACE_STYLE_FILL_AREA ( #48392 ) ;
#93404 = ORIENTED_EDGE ( 'NONE', *, *, #18708, .T. ) ;
#93403 = CARTESIAN_POINT ( 'NONE',  ( 7.361572987183170547, 42.05059781766745886, 9.846743663894590881 ) ) ;
#93405 = EDGE_CURVE ( 'NONE', #2183, #7152, #89965, .T. ) ;
#93406 = CARTESIAN_POINT ( 'NONE',  ( -1.099225684535947600, 64.54030133659709634, 6.408140936763237150 ) ) ;
#93407 = CARTESIAN_POINT ( 'NONE',  ( 20.15039907845753575, 7.627771745786129820, -6.262539305110077059 ) ) ;
#93408 = CARTESIAN_POINT ( 'NONE',  ( -1.099225684535947600, 28.70696800326375353, -6.408140936763238038 ) ) ;
#93409 = CIRCLE ( 'NONE', #8771, 15.00000000000000000 ) ;
#93410 = DIRECTION ( 'NONE',  ( 0.5547001962252290364, 0.8320502943378437211, 0.000000000000000000 ) ) ;
#93411 = CARTESIAN_POINT ( 'NONE',  ( -2.266590686148945544, 42.22041550158063217, 7.082119434687048631 ) ) ;
#93412 = CARTESIAN_POINT ( 'NONE',  ( 0.1532563361054083140, 16.00893115100078390, 1.131784320476157264E-15 ) ) ;
#93413 = SURFACE_STYLE_USAGE ( .BOTH. , #48402 ) ;
#93414 = CARTESIAN_POINT ( 'NONE',  ( 19.99999999999715072, 95.48020498407724688, 5.046714348925600113 ) ) ;
#93415 = CARTESIAN_POINT ( 'NONE',  ( -0.3689425029237881626, 47.42874883491396787, 10.36894250292379027 ) ) ;
#93416 = CARTESIAN_POINT ( 'NONE',  ( 5.076628168052703671, 56.84226448433412315, 8.527530157486179263 ) ) ;
#93417 = CARTESIAN_POINT ( 'NONE',  ( 6.204703633549690345, 62.84541550158063927, 14.16423886937410082 ) ) ;
#93418 = CARTESIAN_POINT ( 'NONE',  ( 13.79529636645030344, 18.26208216824730002, 14.16423886937410614 ) ) ;
#93420 = CARTESIAN_POINT ( 'NONE',  ( -45.10972591793716191, 105.3622991512831675, -4.928873526103649816 ) ) ;
#93419 = CARTESIAN_POINT ( 'NONE',  ( -2.266590686148945544, 37.22041550158063217, 7.082119434687048631 ) ) ;
#93421 = CARTESIAN_POINT ( 'NONE',  ( 12.07856007377828078, 15.00000000000000000, -8.022367888854837759 ) ) ;
#93423 = CARTESIAN_POINT ( 'NONE',  ( 12.63842701281683034, 62.46726448433410894, 9.846743663894596210 ) ) ;
#93422 = CARTESIAN_POINT ( 'NONE',  ( 5.113979357148443761, -17.50950876261946121, 2.500000000000000000 ) ) ;
#93424 = ORIENTED_EDGE ( 'NONE', *, *, #41137, .F. ) ;
#93425 = CARTESIAN_POINT ( 'NONE',  ( -0.8801773607111009756, 33.06368534415484106, 1.068504757029289695E-15 ) ) ;
#93426 = CARTESIAN_POINT ( 'NONE',  ( 10.93781366033347346, 14.63595249122789177, -10.26470809774066417 ) ) ;
#93427 =( GEOMETRIC_REPRESENTATION_CONTEXT ( 3 ) GLOBAL_UNCERTAINTY_ASSIGNED_CONTEXT ( ( #36283 ) ) GLOBAL_UNIT_ASSIGNED_CONTEXT ( ( #16551, #2054, #63014 ) ) REPRESENTATION_CONTEXT ( 'NONE', 'WORKASPACE' ) );
#93428 = CARTESIAN_POINT ( 'NONE',  ( 19.67858290521089160, 89.80068721897295347, -5.461713021790606248 ) ) ;
#93429 = CARTESIAN_POINT ( 'NONE',  ( 14.92337183194729988, 34.34226448433411605, -8.527530157486177487 ) ) ;
#93430 = CARTESIAN_POINT ( 'NONE',  ( -7.313705784284680433, 0.5000000000000004441, 13.09617149020738935 ) ) ;
#93431 = CARTESIAN_POINT ( 'NONE',  ( 3.795296366450314540, -1.737917831752697317, 14.16423886937410082 ) ) ;
#93432 = CARTESIAN_POINT ( 'NONE',  ( 17.20831665107776587, 42.88393115100077324, 7.208316651077764980 ) ) ;
#93433 = DIRECTION ( 'NONE',  ( -0.3502073812594687086, 0.000000000000000000, 0.9366721892483971246 ) ) ;
#93434 = ORIENTED_EDGE ( 'NONE', *, *, #37851, .T. ) ;
#93435 = CARTESIAN_POINT ( 'NONE',  ( 17.08211943468705840, 10.13708216824730179, -12.26659068614894466 ) ) ;
#93436 = FACE_OUTER_BOUND ( 'NONE', #88193, .T. ) ;
#93438 = CARTESIAN_POINT ( 'NONE',  ( 70.08911253270098030, 0.3894472361808988259, 9.500000000000000000 ) ) ;
#93437 = CARTESIAN_POINT ( 'NONE',  ( 1.780824192092492986, 0.3639308653491441503, -14.89391369643516860 ) ) ;
#93439 = CARTESIAN_POINT ( 'NONE',  ( 10.00000000000000000, 11.81368534415483751, -10.88017736071110342 ) ) ;
#93440 = CARTESIAN_POINT ( 'NONE',  ( 16.40814093676323893, 20.79030133659708923, 11.09922568453595026 ) ) ;
#93441 = CARTESIAN_POINT ( 'NONE',  ( 17.97673312326547901, 77.65179697821409377, 4.136170292160840312 ) ) ;
#93442 = CARTESIAN_POINT ( 'NONE',  ( 2.035157376598824452, 68.68868534415484817, 7.964842623401179544 ) ) ;
#93443 = CARTESIAN_POINT ( 'NONE',  ( -46.48928645636214441, 103.2957187381728232, -6.397878122523972699 ) ) ;
#93444 = EDGE_CURVE ( 'NONE', #24768, #11943, #94936, .T. ) ;
#93445 = DIRECTION ( 'NONE',  ( -0.000000000000000000, -1.000000000000000000, -0.000000000000000000 ) ) ;
#93446 = CARTESIAN_POINT ( 'NONE',  ( -2.266590686148945544, 66.38708216824730357, -7.082119434687050408 ) ) ;
#93447 = CIRCLE ( 'NONE', #7238, 11.15000000000026326 ) ;
#93448 = CARTESIAN_POINT ( 'NONE',  ( 19.42250999205614193, 20.14701867748817321, 5.440088680355555262 ) ) ;
#93449 = CARTESIAN_POINT ( 'NONE',  ( 7.084665262690076126, 34.10535201082151247, 10.88017736071109987 ) ) ;
#93450 = CARTESIAN_POINT ( 'NONE',  ( 1.472469842513823179, 66.42559781766745175, 4.923371831947296329 ) ) ;
#93451 = CARTESIAN_POINT ( 'NONE',  ( 12.63842701281683922, 59.55059781766744464, -9.846743663894590881 ) ) ;
#93452 = CARTESIAN_POINT ( 'NONE',  ( 19.38216949554541557, 62.24863466993041072, -9.382169495545420901 ) ) ;
#93453 = CARTESIAN_POINT ( 'NONE',  ( -1.761054936948033056, 12.86682408883346440, -9.500000000000000000 ) ) ;
#93454 = ORIENTED_EDGE ( 'NONE', *, *, #24581, .T. ) ;
#93455 = EDGE_CURVE ( 'NONE', #17335, #83513, #80438, .T. ) ;
#93456 = CARTESIAN_POINT ( 'NONE',  ( 2.035157376598822676, 32.43868534415483396, -7.964842623401177768 ) ) ;
#93457 = CARTESIAN_POINT ( 'NONE',  ( 22.81628187352647785, 36.62363466993041783, 6.195893100308588602E-16 ) ) ;
#93458 = CARTESIAN_POINT ( 'NONE',  ( 0.000000000000000000, 74.63951520916478444, 5.933331309799314113 ) ) ;
#93459 = UNCERTAINTY_MEASURE_WITH_UNIT (LENGTH_MEASURE( 1.000000000000000082E-05 ), #2289, 'distance_accuracy_value', 'NONE');
#93460 = CARTESIAN_POINT ( 'NONE',  ( 12.63842701281683922, 59.55059781766744464, -9.846743663894590881 ) ) ;
#93461 = CARTESIAN_POINT ( 'NONE',  ( 7.084665262690076126, 47.02201867748818387, -10.88017736071110164 ) ) ;
#93462 = AXIS2_PLACEMENT_3D ( 'NONE', #40292, #2318, #93776 ) ;
#93463 = CARTESIAN_POINT ( 'NONE',  ( 12.63842701281683034, 7.467264484334118713, 9.846743663894596210 ) ) ;
#93464 = CARTESIAN_POINT ( 'NONE',  ( 21.09922568453594849, 31.20696800326375353, 6.408140936763242479 ) ) ;
#93466 = CARTESIAN_POINT ( 'NONE',  ( 0.000000000000000000, 15.00000000000000000, 0.000000000000000000 ) ) ;
#93465 = CARTESIAN_POINT ( 'NONE',  ( 4.559911319644449179, 62.23035201082150536, -9.422509992056141925 ) ) ;
#93467 = CARTESIAN_POINT ( 'NONE',  ( -1.099225684535947600, 59.54030133659708923, 6.408140936763237150 ) ) ;
#93468 = VERTEX_POINT ( 'NONE', #50420 ) ;
#93469 = SURFACE_STYLE_FILL_AREA ( #53992 ) ;
#93470 = CARTESIAN_POINT ( 'NONE',  ( 0.2751277870542983006, 13.21833443783938122, 6.500000000000002665 ) ) ;
#93471 = CARTESIAN_POINT ( 'NONE',  ( 0.5774900079438607392, 3.480352010821504027, 5.440088680355550821 ) ) ;
#93473 = CARTESIAN_POINT ( 'NONE',  ( 10.00000000000000178, 18.05374883491396787, 14.16423886937410082 ) ) ;
#93472 = CARTESIAN_POINT ( 'NONE',  ( 6.565887622018943937, 45.16530133659708923, 12.81628187352647430 ) ) ;
#93474 = CARTESIAN_POINT ( 'NONE',  ( 19.84674366389459266, 13.71726448433411782, -2.638427012816827677 ) ) ;
#93475 = CARTESIAN_POINT ( 'NONE',  ( 19.42250999205614548, 5.980352010821504471, -5.440088680355545492 ) ) ;
#93476 = CARTESIAN_POINT ( 'NONE',  ( 19.84674366389459621, 18.50893115100078745, 7.409399052514197653E-17 ) ) ;
#93477 = CARTESIAN_POINT ( 'NONE',  ( 17.08211943468705130, 53.47041550158063217, 12.26659068614894998 ) ) ;
#93478 = ORIENTED_EDGE ( 'NONE', *, *, #67747, .T. ) ;
#93479 = DIRECTION ( 'NONE',  ( 0.000000000000000000, 0.000000000000000000, 1.000000000000000000 ) ) ;
#93480 = CARTESIAN_POINT ( 'NONE',  ( 10.00000000000000000, 26.81368534415484106, -10.88017736071110342 ) ) ;
#93481 = CARTESIAN_POINT ( 'NONE',  ( -6.319286839011487800, -45.42958518191715456, 2.500000000000000000 ) ) ;
#93482 = ORIENTED_EDGE ( 'NONE', *, *, #28919, .T. ) ;
#93483 = CARTESIAN_POINT ( 'NONE',  ( 20.88017736071110875, 15.77201867748817143, -2.915334737309920765 ) ) ;
#93485 = EDGE_CURVE ( 'NONE', #47944, #11778, #48679, .T. ) ;
#93484 = CARTESIAN_POINT ( 'NONE',  ( 10.00000000000000000, 16.81368534415483751, -10.88017736071110342 ) ) ;
#93486 = CARTESIAN_POINT ( 'NONE',  ( 19.84674366389459266, 53.30059781766744464, 2.638427012816836559 ) ) ;
#93487 = VECTOR ( 'NONE', #18511, 1000.000000000000114 ) ;
#93488 = CARTESIAN_POINT ( 'NONE',  ( 19.38216949554541202, 55.99863466993041072, 9.382169495545424454 ) ) ;
#93489 = CARTESIAN_POINT ( 'NONE',  ( -5.204170427930421283E-15, 11.67180217785154817, -11.25000000000000178 ) ) ;
#93491 = CARTESIAN_POINT ( 'NONE',  ( 24.16423886937410614, 19.30374883491397142, 8.672049930838204340E-16 ) ) ;
#93490 = FILL_AREA_STYLE ('',( #34815 ) ) ;
#93492 = CARTESIAN_POINT ( 'NONE',  ( -0.8801773607111008646, 28.27201867748817321, 2.915334737309923430 ) ) ;
#93493 = CARTESIAN_POINT ( 'NONE',  ( 15.44008868035555260, 9.730352010821505360, 9.422509992056143702 ) ) ;
#93494 = CARTESIAN_POINT ( 'NONE',  ( 17.20831665107776587, 52.88393115100078035, 7.208316651077764980 ) ) ;
#93495 = ADVANCED_FACE ( 'NONE', ( #35416 ), #2209, .T. ) ;
#93496 = CARTESIAN_POINT ( 'NONE',  ( -9.065164099344370285, 15.00000000000000000, -11.95084933600779564 ) ) ;
#93497 = CARTESIAN_POINT ( 'NONE',  ( 19.84674366389459266, 38.71726448433412315, -2.638427012816827677 ) ) ;
#93498 = CARTESIAN_POINT ( 'NONE',  ( 1.472469842513823179, 10.59226448433411782, -4.923371831947296329 ) ) ;
#93499 = CARTESIAN_POINT ( 'NONE',  ( -9.382169495545422677, -41.50136533006958217, -9.382169495545417348 ) ) ;
#93500 = VERTEX_POINT ( 'NONE', #81411 ) ;
#93501 = CARTESIAN_POINT ( 'NONE',  ( 15.44008868035555260, 4.730352010821504471, 9.422509992056143702 ) ) ;
#93502 = CARTESIAN_POINT ( 'NONE',  ( 4.559911319644449179, 62.23035201082150536, -9.422509992056141925 ) ) ;
#93503 = CARTESIAN_POINT ( 'NONE',  ( 0.6178305044545838731, 4.748634669930420493, 9.382169495545420901 ) ) ;
#93504 = CARTESIAN_POINT ( 'NONE',  ( -0.8801773607111008646, 48.27201867748816966, 2.915334737309923430 ) ) ;
#93505 = CARTESIAN_POINT ( 'NONE',  ( 19.38216949554541202, 40.99863466993042493, 9.382169495545424454 ) ) ;
#93506 = CARTESIAN_POINT ( 'NONE',  ( 20.36894250292379738, 24.92874883491396787, -10.36894250292379027 ) ) ;
#93507 = CIRCLE ( 'NONE', #44027, 0.5000000000000004441 ) ;
#93508 = VECTOR ( 'NONE', #35764, 1000.000000000000000 ) ;
#93509 = EDGE_CURVE ( 'NONE', #4363, #73542, #4453, .T. ) ;
#93510 = CARTESIAN_POINT ( 'NONE',  ( 3.591859063236761518, 64.95696800326376774, 11.09922568453594849 ) ) ;
#93511 = EDGE_LOOP ( 'NONE', ( #2138, #38311, #68975, #96590 ) ) ;
#93512 = CARTESIAN_POINT ( 'NONE',  ( 19.84674366389459266, 58.30059781766745886, 2.638427012816836559 ) ) ;
#93513 = CARTESIAN_POINT ( 'NONE',  ( 15.44008868035555793, 16.39701867748817321, -9.422509992056140149 ) ) ;
#93515 = ORIENTED_EDGE ( 'NONE', *, *, #62975, .T. ) ;
#93514 = EDGE_CURVE ( 'NONE', #49695, #69049, #95440, .T. ) ;
#93516 = CARTESIAN_POINT ( 'NONE',  ( 2.791683348922240793, 6.633931151000785675, 7.208316651077764092 ) ) ;
#93517 = CARTESIAN_POINT ( 'NONE',  ( 19.84674366389459266, 13.71726448433411782, -2.638427012816827677 ) ) ;
#93518 = CARTESIAN_POINT ( 'NONE',  ( 2.791683348922240793, 1.633931151000784565, 7.208316651077764092 ) ) ;
#93519 = DIRECTION ( 'NONE',  ( 0.7253743710122775301, 0.000000000000000000, 0.6883545756937645699 ) ) ;
#93521 = CARTESIAN_POINT ( 'NONE',  ( 4.130000000000002558, 1.019547802438462547, 2.500000000000000000 ) ) ;
#93520 = CARTESIAN_POINT ( 'NONE',  ( 19.42250999205614193, 55.14701867748817676, 5.440088680355555262 ) ) ;
#93522 = CARTESIAN_POINT ( 'NONE',  ( 10.00000000000000178, 64.31368534415483396, 10.88017736071110342 ) ) ;
#93523 = CARTESIAN_POINT ( 'NONE',  ( 18.52753015748617571, 8.092264484334117824, 4.923371831947298993 ) ) ;
#93524 = CARTESIAN_POINT ( 'NONE',  ( 14.09394518620610270, 4.258544466044566969E-16, 3.407449058785454898 ) ) ;
#93525 = CARTESIAN_POINT ( 'NONE',  ( 19.84674366389459266, 58.71726448433411605, -2.638427012816827677 ) ) ;
#93526 = ORIENTED_EDGE ( 'NONE', *, *, #95242, .T. ) ;
#93527 = DIRECTION ( 'NONE',  ( 1.000000000000000000, 1.636349903325072848E-16, -0.000000000000000000 ) ) ;
#93528 = CARTESIAN_POINT ( 'NONE',  ( 6.204703633549690345, 10.76208216824729824, -14.16423886937410259 ) ) ;
#93529 = CARTESIAN_POINT ( 'NONE',  ( 6.565887622018943937, 60.16530133659707502, 12.81628187352647430 ) ) ;
#93530 = CARTESIAN_POINT ( 'NONE',  ( -4.164238869374099927, 17.01208216824730357, 3.795296366450308767 ) ) ;
#93531 = B_SPLINE_CURVE_WITH_KNOTS ( 'NONE', 3,
 ( #14535, #75511, #68021, #2005, #47957, #26439, #62965, #32470, #33925, #10952 ),
 .UNSPECIFIED., .F., .F.,
 ( 4, 3, 3, 4 ),
 ( 8.182674270850422113E-18, 0.0006253016069560709969, 0.001250604074564918905, 0.002501455912506541333 ),
 .UNSPECIFIED. ) ;
#93532 = CARTESIAN_POINT ( 'NONE',  ( -0.1023957841222446069, 45.13377557478297319, 6.340343622311912952 ) ) ;
#93533 = CARTESIAN_POINT ( 'NONE',  ( 13.61464873478166737, 0.5000000000000004441, -6.296136897217838424 ) ) ;
#93534 = CARTESIAN_POINT ( 'NONE',  ( 2.035157376598822676, 17.43868534415483751, -7.964842623401177768 ) ) ;
#93535 = PLANE ( 'NONE',  #29155 ) ;
#93536 = VERTEX_POINT ( 'NONE', #12421 ) ;
#93537 = CARTESIAN_POINT ( 'NONE',  ( 10.00000000000000000, 9.758931151000785675, -9.846743663894594434 ) ) ;
#93538 = CARTESIAN_POINT ( 'NONE',  ( 2.791683348922240793, 21.63393115100078745, 7.208316651077764092 ) ) ;
#93539 = CARTESIAN_POINT ( 'NONE',  ( 16.40814093676324603, 27.45696800326375708, -11.09922568453594671 ) ) ;
#93540 = CARTESIAN_POINT ( 'NONE',  ( 12.63842701281683034, 32.46726448433412315, 9.846743663894596210 ) ) ;
#93541 = CARTESIAN_POINT ( 'NONE',  ( -19.19000000000001194, 93.50000000000000000, -9.500000000000000000 ) ) ;
#93542 = CARTESIAN_POINT ( 'NONE',  ( 6.565887622018943937, 18.08196800326375708, -12.81628187352647608 ) ) ;
#93543 = CARTESIAN_POINT ( 'NONE',  ( 0.2851577207221809851, 14.76930270348882068, 14.93843163678289443 ) ) ;
#93544 = CARTESIAN_POINT ( 'NONE',  ( 10.00000000000000000, 24.75893115100078745, -9.846743663894594434 ) ) ;
#93545 = AXIS2_PLACEMENT_3D ( 'NONE', #82727, #68242, #75721 ) ;
#93546 = CARTESIAN_POINT ( 'NONE',  ( 5.076628168052703671, 6.842264484334118713, 8.527530157486179263 ) ) ;
#93547 = ORIENTED_EDGE ( 'NONE', *, *, #39686, .T. ) ;
#93548 = VERTEX_POINT ( 'NONE', #79935 ) ;
#93549 = CARTESIAN_POINT ( 'NONE',  ( 17.96484262340118221, 39.93868534415484106, 7.964842623401181321 ) ) ;
#93550 = CARTESIAN_POINT ( 'NONE',  ( 20.36894250292379738, 29.92874883491396432, -10.36894250292379027 ) ) ;
#93551 = CARTESIAN_POINT ( 'NONE',  ( 12.63842701281683034, 37.46726448433411605, 9.846743663894596210 ) ) ;
#93552 = CARTESIAN_POINT ( 'NONE',  ( 19.84674366389459621, 18.50893115100078745, 7.409399052514197653E-17 ) ) ;
#93554 = CARTESIAN_POINT ( 'NONE',  ( -7.984789763142470242, 85.83064272735667544, 4.183481735294424020 ) ) ;
#93553 = CARTESIAN_POINT ( 'NONE',  ( 21.09922568453595559, 57.04030133659708923, -6.408140936763230044 ) ) ;
#93555 = CARTESIAN_POINT ( 'NONE',  ( -0.8801773607110991993, 27.85535201082150181, -2.915334737309923874 ) ) ;
#93556 = CARTESIAN_POINT ( 'NONE',  ( 14.24131928502211686, 0.000000000000000000, -0.4973178280105898241 ) ) ;
#93557 = CARTESIAN_POINT ( 'NONE',  ( 6.565887622018943937, 25.16530133659708213, 12.81628187352647430 ) ) ;
#93558 = CARTESIAN_POINT ( 'NONE',  ( 7.361572987183169658, 44.96726448433412315, -9.846743663894592657 ) ) ;
#93559 = CARTESIAN_POINT ( 'NONE',  ( 9.422509992056141925, 5.980352010821511577, -5.440088680355554374 ) ) ;
#93560 = CARTESIAN_POINT ( 'NONE',  ( 0.6178305044545818747, 48.49863466993042493, -9.382169495545419124 ) ) ;
#93561 = CARTESIAN_POINT ( 'NONE',  ( 4.431036607602602651, 14.49999999999999112, -14.33059365769916305 ) ) ;
#93563 = PLANE ( 'NONE',  #67170 ) ;
#93562 = CARTESIAN_POINT ( 'NONE',  ( 19.42250999205614193, 55.14701867748817676, 5.440088680355555262 ) ) ;
#93564 = ADVANCED_FACE ( 'NONE', ( #42928 ), #73910, .T. ) ;
#93565 = CARTESIAN_POINT ( 'NONE',  ( -8.957287532561966970, -19.72663685366165254, 4.000000000000000000 ) ) ;
#93566 = DIRECTION ( 'NONE',  ( 0.000000000000000000, -1.000000000000000000, 0.000000000000000000 ) ) ;
#93567 = CARTESIAN_POINT ( 'NONE',  ( 20.88017736071110875, 55.77201867748816966, -2.915334737309920765 ) ) ;
#93568 = CARTESIAN_POINT ( 'NONE',  ( 12.91533473730993009, 56.60535201082151247, -10.88017736071109987 ) ) ;
#93569 = DIRECTION ( 'NONE',  ( -1.000000000000000000, -1.257402221000611116E-16, 0.000000000000000000 ) ) ;
#93570 = PRESENTATION_STYLE_ASSIGNMENT (( #62572 ) ) ;
#93571 = B_SPLINE_CURVE_WITH_KNOTS ( 'NONE', 3,
 ( #45345, #30831, #92812, #67864, #54804, #76340 ),
 .UNSPECIFIED., .F., .F.,
 ( 4, 2, 4 ),
 ( 0.0002800289709865101998, 0.0006862344838253363246, 0.001092439996664162612 ),
 .UNSPECIFIED. ) ;
#93572 = CARTESIAN_POINT ( 'NONE',  ( 15.44008868035555793, 11.39701867748817143, -9.422509992056140149 ) ) ;
#93573 = CARTESIAN_POINT ( 'NONE',  ( 19.84674366389459266, 63.30059781766745886, 2.638427012816836559 ) ) ;
#93575 = CARTESIAN_POINT ( 'NONE',  ( -2.621477372531479055, -0.03417435944610275333, -15.77990027919564575 ) ) ;
#93574 = CARTESIAN_POINT ( 'NONE',  ( 15.44008868035555260, 24.73035201082150891, 9.422509992056143702 ) ) ;
#93576 = DIRECTION ( 'NONE',  ( 0.8070303256584298035, -0.5905099943842175847, 0.000000000000000000 ) ) ;
#93577 = CARTESIAN_POINT ( 'NONE',  ( 3.591859063236763294, 23.29030133659708568, -11.09922568453595026 ) ) ;
#93578 = EDGE_LOOP ( 'NONE', ( #52299, #16342, #47720, #2064, #98782, #21071 ) ) ;
#93579 = CARTESIAN_POINT ( 'NONE',  ( 7.084665262690076126, 57.02201867748817676, -10.88017736071110164 ) ) ;
#93580 = CARTESIAN_POINT ( 'NONE',  ( 14.92337183194729633, 37.67559781766745175, 8.527530157486181039 ) ) ;
#93581 = CARTESIAN_POINT ( 'NONE',  ( 0.6178305044545818747, 13.49863466993041783, -9.382169495545419124 ) ) ;
#93582 = CARTESIAN_POINT ( 'NONE',  ( 12.91533473730993009, 11.60535201082150536, -10.88017736071109987 ) ) ;
#93583 = CARTESIAN_POINT ( 'NONE',  ( 10.00000000000000178, 39.31368534415484106, 10.88017736071110342 ) ) ;
#93584 = CARTESIAN_POINT ( 'NONE',  ( -4.164238869374099039, 51.80374883491396787, 8.674139862899312516E-16 ) ) ;
#93585 = CARTESIAN_POINT ( 'NONE',  ( 17.20831665107776587, 34.13393115100078745, -7.208316651077762316 ) ) ;
#93586 = CARTESIAN_POINT ( 'NONE',  ( 20.88017736071110875, 55.77201867748816966, -2.915334737309920765 ) ) ;
#93587 = CARTESIAN_POINT ( 'NONE',  ( -2.266590686148945544, 12.22041550158063394, 7.082119434687048631 ) ) ;
#93588 = AXIS2_PLACEMENT_3D ( 'NONE', #11144, #72131, #77297 ) ;
#93589 = CARTESIAN_POINT ( 'NONE',  ( 7.079515573063599021, -88.00917032380691296, 3.750000000000000000 ) ) ;
#93590 = CARTESIAN_POINT ( 'NONE',  ( 5.076628168052703671, 66.84226448433412315, 8.527530157486179263 ) ) ;
#93591 = CIRCLE ( 'NONE', #50481, 0.5000000000000066613 ) ;
#93592 = TOROIDAL_SURFACE ( 'NONE', #24957, 14.49999999999999822, 0.5000000000000000000 ) ;
#93593 = ORIENTED_EDGE ( 'NONE', *, *, #4446, .T. ) ;
#93594 = ORIENTED_EDGE ( 'NONE', *, *, #59478, .T. ) ;
#93595 = CARTESIAN_POINT ( 'NONE',  ( 24.16423886937410614, 34.30374883491396787, 8.672049930838204340E-16 ) ) ;
#93597 = EDGE_CURVE ( 'NONE', #55430, #64082, #11442, .T. ) ;
#93596 = CARTESIAN_POINT ( 'NONE',  ( -0.3689425029237898834, 36.17874883491396787, -10.36894250292378850 ) ) ;
#93598 = CARTESIAN_POINT ( 'NONE',  ( 17.20831665107776587, 14.13393115100078568, -7.208316651077762316 ) ) ;
#93599 = CARTESIAN_POINT ( 'NONE',  ( 22.81628187352647785, 11.41530133659708390, 3.434112377981063169 ) ) ;
#93600 = CARTESIAN_POINT ( 'NONE',  ( 12.63842701281683922, 64.55059781766745175, -9.846743663894590881 ) ) ;
#93601 = DIRECTION ( 'NONE',  ( 0.000000000000000000, -1.000000000000000000, -0.000000000000000000 ) ) ;
#93603 = CARTESIAN_POINT ( 'NONE',  ( 22.81628187352647785, 36.62363466993041783, 6.195893100308588602E-16 ) ) ;
#93602 = CARTESIAN_POINT ( 'NONE',  ( 19.42250999205614548, 55.98035201082150536, -5.440088680355545492 ) ) ;
#93604 = CARTESIAN_POINT ( 'NONE',  ( 24.16423886937410614, 29.30374883491396787, 8.672049930838204340E-16 ) ) ;
#93605 = CARTESIAN_POINT ( 'NONE',  ( 19.42250999205614193, 25.14701867748817321, 5.440088680355555262 ) ) ;
#93606 = MECHANICAL_DESIGN_GEOMETRIC_PRESENTATION_REPRESENTATION (  '', ( #85624 ), #20151 ) ;
#93607 = EDGE_CURVE ( 'NONE', #86221, #95526, #73408, .T. ) ;
#93608 = CARTESIAN_POINT ( 'NONE',  ( 2.035157376598824452, 63.68868534415484106, 7.964842623401179544 ) ) ;
#93609 = CARTESIAN_POINT ( 'NONE',  ( -8.527530157486173934, -8.574402182332546474, 4.923371831947302546 ) ) ;
#93610 = ORIENTED_EDGE ( 'NONE', *, *, #84556, .F. ) ;
#93611 = CARTESIAN_POINT ( 'NONE',  ( 10.00000000000000178, 70.00000000000000000, 0.000000000000000000 ) ) ;
#93612 = VERTEX_POINT ( 'NONE', #5439 ) ;
#93613 = CARTESIAN_POINT ( 'NONE',  ( 0.000000000000000000, 0.000000000000000000, -13.74999999999999467 ) ) ;
#93614 = VERTEX_POINT ( 'NONE', #58403 ) ;
#93615 = CARTESIAN_POINT ( 'NONE',  ( 2.917880565312950480, 0.9704155015806342766, -12.26659068614894821 ) ) ;
#93617 = CARTESIAN_POINT ( 'NONE',  ( 0.5774900079438590739, 17.64701867748817321, -5.440088680355550821 ) ) ;
#93616 = CARTESIAN_POINT ( 'NONE',  ( 10.00000000000000000, 1.813685344154838175, -10.88017736071110342 ) ) ;
#93619 = CARTESIAN_POINT ( 'NONE',  ( 6.565887622018943937, 10.16530133659708746, 12.81628187352647430 ) ) ;
#93618 = CARTESIAN_POINT ( 'NONE',  ( 17.20831665107776587, 32.88393115100078745, 7.208316651077764980 ) ) ;
#93620 = CARTESIAN_POINT ( 'NONE',  ( -13.34948392230367453, 14.95077488074854166, -6.279918722515163587 ) ) ;
#93621 = CARTESIAN_POINT ( 'NONE',  ( -9.641450013144547526, 14.95037107666755816, 11.16690429682342511 ) ) ;
#93622 = VECTOR ( 'NONE', #54186, 1000.000000000000000 ) ;
#93623 = VECTOR ( 'NONE', #66840, 1000.000000000000000 ) ;
#93624 = CIRCLE ( 'NONE', #84069, 15.00000000000000000 ) ;
#93625 = CARTESIAN_POINT ( 'NONE',  ( -1.099225684535947600, 9.540301336597087456, 6.408140936763237150 ) ) ;
#93626 = VERTEX_POINT ( 'NONE', #86947 ) ;
#93627 = CARTESIAN_POINT ( 'NONE',  ( 6.204703633549690345, 42.84541550158063217, 14.16423886937410082 ) ) ;
#93628 = ORIENTED_EDGE ( 'NONE', *, *, #51264, .F. ) ;
#93629 = CARTESIAN_POINT ( 'NONE',  ( 20.36894250292379738, 54.92874883491396076, -10.36894250292379027 ) ) ;
#93630 = VERTEX_POINT ( 'NONE', #88921 ) ;
#93631 = CARTESIAN_POINT ( 'NONE',  ( 19.42250999205614193, 40.14701867748817676, 5.440088680355555262 ) ) ;
#93632 = CARTESIAN_POINT ( 'NONE',  ( -0.8801773607111008646, 38.27201867748816255, 2.915334737309923430 ) ) ;
#93633 = CARTESIAN_POINT ( 'NONE',  ( -0.3093388210927896509, 14.49999999999999112, 14.99680997725072373 ) ) ;
#93634 = CARTESIAN_POINT ( 'NONE',  ( 2.035157376598822676, 42.43868534415483396, -7.964842623401177768 ) ) ;
#93635 = CARTESIAN_POINT ( 'NONE',  ( 13.99999999999999822, 11.00000000000000000, 5.000000000000000000 ) ) ;
#93636 = CARTESIAN_POINT ( 'NONE',  ( 19.42250999205614548, 20.98035201082150891, -5.440088680355545492 ) ) ;
#93637 = ADVANCED_FACE ( 'NONE', ( #35911 ), #84692, .T. ) ;
#93638 = CARTESIAN_POINT ( 'NONE',  ( -1.983216688680738082, -0.03417435944610275333, -14.11131997956740491 ) ) ;
#93639 = CARTESIAN_POINT ( 'NONE',  ( 0.1532563361054083140, 16.00893115100078390, 1.131784320476157264E-15 ) ) ;
#93640 = CARTESIAN_POINT ( 'NONE',  ( -3.887834249507322593, -8.254296980867463773, 2.500000000000001776 ) ) ;
#93641 = ORIENTED_EDGE ( 'NONE', *, *, #9691, .T. ) ;
#93642 = DIRECTION ( 'NONE',  ( 0.5075383629607025382, 0.000000000000000000, -0.8616291604415267091 ) ) ;
#93643 = CARTESIAN_POINT ( 'NONE',  ( 2.791683348922237240, 40.38393115100078035, -7.208316651077763204 ) ) ;
#93644 = FACE_OUTER_BOUND ( 'NONE', #21809, .T. ) ;
#93645 = DIRECTION ( 'NONE',  ( 0.000000000000000000, 0.000000000000000000, -1.000000000000000000 ) ) ;
#93646 = VERTEX_POINT ( 'NONE', #44474 ) ;
#93647 = DIRECTION ( 'NONE',  ( -1.000000000000000000, 0.000000000000000000, 0.000000000000000000 ) ) ;
#93648 = DIRECTION ( 'NONE',  ( -0.000000000000000000, -1.000000000000000000, -0.000000000000000000 ) ) ;
#93649 = CARTESIAN_POINT ( 'NONE',  ( 1.472469842513823179, 56.42559781766745886, 4.923371831947296329 ) ) ;
#93650 = CARTESIAN_POINT ( 'NONE',  ( 22.26659068614895176, 49.72041550158063927, -7.082119434687042414 ) ) ;
#93651 = CARTESIAN_POINT ( 'NONE',  ( 19.84674366389459266, 58.30059781766745886, 2.638427012816836559 ) ) ;
#93652 = ORIENTED_EDGE ( 'NONE', *, *, #70253, .F. ) ;
#93653 = LINE ( 'NONE', #70675, #49597 ) ;
#93654 = CARTESIAN_POINT ( 'NONE',  ( 1.472469842513823179, 15.59226448433411960, -4.923371831947296329 ) ) ;
#93655 = CARTESIAN_POINT ( 'NONE',  ( 3.591859063236763294, 58.29030133659708923, -11.09922568453595026 ) ) ;
#93656 = CARTESIAN_POINT ( 'NONE',  ( 5.076628168052704559, 60.17559781766745175, -8.527530157486179263 ) ) ;
#93657 = CARTESIAN_POINT ( 'NONE',  ( 5.076628168052703671, 1.842264484334118047, 8.527530157486179263 ) ) ;
#93658 = AXIS2_PLACEMENT_3D ( 'NONE', #3300, #95272, #81733 ) ;
#93659 = CARTESIAN_POINT ( 'NONE',  ( 18.52753015748618282, 48.92559781766745886, -4.923371831947291888 ) ) ;
#93660 =( BOUNDED_SURFACE ( )  B_SPLINE_SURFACE ( 1, 2, ( 
 ( #39642, #70624, #79096, #70134, #1654, #32104, #24638, #55106, #85626, #17142, #47621, #78116, #2150, #32609, #25145, #55622, #88067, #28558, #58056, #67053, #74547, #27564, #20066, #72564, #65554, #12568, #65057, #96582, #59053, #28058, #5077, #88563, #90043, #35564, #89060, #66559, #12074, #20575, #73551, #50570, #59548, #73060, #80079, #4101, #6065, #19579, #81548, #35056, #50076, #51561, #4594, #57568, #89555, #58554, #5582, #36565, #97578, #29039, #34562, #95584, #49568, #36057, #97087, #81066, #11585, #51058, #13058, #42101, #43552, #21065, #43069, #80579, #27070, #42580, #66055, #96082, #74046, #82046, #13558, #44045, #16027, #52055, #90531, #61023, #14064, #75042, #60034, #75, #82548, #15555, #69034, #46515, #52538, #98576, #77016, #23548, #83045, #91535, #54020, #23050, #53523, #22556, #46039, #84034, #76524, #569, #22065, #69525, #1040, #92020, #44546, #14562, #31015, #30027, #39030, #8529, #60534, #91025, #6548, #37558, #83541, #37060, #68543, #61511, #30520, #76031, #53026, #62004, #7564, #8040, #38539, #45031, #15062, #45533, #38051, #84529, #31503, #7054, #21566, #67557, #98068, #75540, #29527, #68048, #25512, #47985, #86501, #40510, #71969, #85016, #40007, #78981, #25020, #47005, #54501, #62493, #24531, #17020, #70019, #25989, #93990, #1543, #18485, #3013, #62991, #63486, #2530, #10490, #31987, #94471, #55507, #17518, #55998, #9506, #32495, #17999, #92997, #10008, #48972, #92503, #33462, #79480, #33949, #2033, #78494, #48481, #71007, #93497, #41001, #24033, #63959, #71500, #85509, #86006, #54991, #77497, #10980, #32984, #16530, #9009, #47497, #56485, #86972, #41500, #39525, #3492, #78000, #70509, #57458, #51435, #42956, #12448, #72449, #81926, #26958, #5464, #66432, #19466, #95966, #50445, #20453, #3980, #19951, #49458, #34447, #80951, #50942, #18979, #81436, #12940, #80463, #87952, #74418, #27449, #20949, #43434, #13434, #73935, #43922, #96466, #35936, #26462, #27938, #41985, #57942, #42466, #88450, #64940, #49958, #64454, #96967, #65442, #28438, #73435, #11960, #4962, #58936, #72948, #95467, #89436, #5948, #35442, #56963, #65939, #4477, #94960, #87464, #58431, #34944, #79963, #88944, #11467, #74924, #82920, #67928, #52904, #37437, #15436, #83415, #44420, #75910, #14936, #89924, #75413, #22433, #45404, #29904, #7919, #60901, #90905, #45915, #98943, #76404, #7435, #91401, #37931, #68420, #14438, #30397, #22930, #53398, #83907, #6422, #38416, #68914, #36438, #59418, #36936, #66931, #44908, #97452, #28917, #6929, #98448, #13944, #60410, #21438, #67428, #51936, #82420, #97952, #29409, #59913, #90402, #21943 ),
 ( #52421, #36256, #44240, #96780, #35758, #43749, #65253, #28750, #88759, #50769, #89256, #42775, #65754, #51255, #27261, #43256, #82241, #26774, #66753, #13754, #67251, #35256, #81260, #28256, #73751, #96280, #58752, #57271, #97277, #20767, #19768, #27757, #57761, #80275, #74744, #58240, #87766, #19280, #95781, #12758, #20271, #59241, #49766, #74235, #5282, #89740, #50254, #6256, #66246, #81741, #34764, #36759, #88264, #21259, #51756, #80771, #13257, #5768, #11776, #12266, #42284, #72756, #73258, #4291, #4783, #91789, #54754, #37325, #68308, #31763, #67815, #7313, #76777, #29789, #90794, #75794, #15803, #98331, #31266, #84781, #62257, #98829, #15319, #92763, #39292, #30283, #60785, #23310, #76293, #69292, #53788, #61766, #84304, #16780, #60301, #83797, #23804, #68801, #22320, #52794, #37814, #91286, #22809, #14824, #69782, #38792, #45299, #24288, #46770, #7807, #8294, #61280, #38305, #47256, #53289, #83299, #45802, #85275, #331, #813, #30775, #46288, #1312, #92282, #54265, #77264, #16290, #8775, #77756, #64704, #57216, #32250, #93255, #26720, #94735, #64217, #78756, #70279, #56258, #86751, #95215, #10750, #26241, #2784, #17281, #87713, #2290, #17770, #1796, #63733, #19229, #9271, #40266, #3752, #39780, #78254, #48733, #62752, #24779, #47755, #18256, #55255, #3251, #56734, #34212, #70774, #86256, #49708, #11232, #32747, #79238, #41751, #41270, #71743, #10264, #33718, #87226, #18748, #49232, #9771, #85769, #63244, #79734, #93747, #25282, #72222, #48246, #55764, #40757, #71260, #33239, #94233, #25765, #43201, #95722, #28200, #89690, #58696, #35705, #20210, #21705, #66190, #20712, #97226, #42720, #88701, #12707, #5226, #28693, #89200, #65700, #59186, #36705, #21206, #97719, #51704, #29183, #51204, #81687, #82186, #19717, #13697, #73691, #96724, #43694, #96226, #50714, #5712, #80717, #13202, #67194, #80219, #44181, #59682, #11723, #81207, #74182, #36201, #66698, #74690, #6201, #42236, #90175, #72702, #73201, #4238, #12213, #34706, #65202, #27207, #57708, #88207, #50205, #4732, #35197, #27704, #58189, #69174, #30655, #84658, #45177, #39169, #61162, #204, #60176, #69658, #14704, #92162, #54149, #7190, #83678, #38190, #8178, #90672, #7693, #37209, #22198, #46174, #15688, #1184, #52678, #38672, #68192, #75677, #62134, #15193, #8656, #31150, #31642, #697, #92642, #84181, #61641, #14202, #76657, #29667, #45675, #30163, #76173, #83179, #37693, #52190, #16167, #53173, #23685, #68677, #98712, #91670, #46651, #60666, #91166, #77147, #82684, #23189, #44683, #53665, #22693, #75179, #6690, #67697, #98209, #12468, #79499, #56978, #24660 ) ),
 .UNSPECIFIED., .F., .F., .T. ) 
 B_SPLINE_SURFACE_WITH_KNOTS ( ( 2, 2 ),
 ( 3, 2, 2, 2, 2, 2, 2, 2, 2, 2, 2, 2, 2, 2, 2, 2, 2, 2, 2, 2, 2, 2, 2, 2, 2, 2, 2, 2, 2, 2, 2, 2, 2, 2, 2, 2, 2, 2, 2, 2, 2, 2, 2, 2, 2, 2, 2, 2, 2, 2, 2, 2, 2, 2, 2, 2, 2, 2, 2, 2, 2, 2, 2, 2, 2, 2, 2, 2, 2, 2, 2, 2, 2, 2, 2, 2, 2, 2, 2, 2, 2, 2, 2, 2, 2, 2, 2, 2, 2, 2, 2, 2, 2, 2, 2, 2, 2, 2, 2, 2, 2, 2, 2, 2, 2, 2, 2, 2, 2, 2, 2, 2, 2, 2, 2, 2, 2, 2, 2, 2, 2, 2, 2, 2, 2, 2, 2, 2, 2, 2, 2, 2, 2, 2, 2, 2, 2, 2, 2, 2, 2, 2, 2, 2, 2, 2, 2, 2, 2, 2, 2, 2, 2, 2, 2, 2, 2, 2, 2, 2, 2, 2, 3 ),
 ( 0.000000000000000000, 1.000000000000000000 ),
 ( 0.000000000000000000, 0.005952380952380952051, 0.01190476190476190410, 0.01785714285714285615, 0.02380952380952380820, 0.02976190476190476025, 0.03571428571428571230, 0.04166666666666666435, 0.04761904761904761640, 0.05357142857142856845, 0.05952380952380952051, 0.06547619047619047949, 0.07142857142857142461, 0.07738095238095238360, 0.08333333333333332871, 0.08928571428571428770, 0.09523809523809523281, 0.1011904761904761918, 0.1071428571428571369, 0.1130952380952380959, 0.1190476190476190410, 0.1250000000000000000, 0.1309523809523809590, 0.1369047619047619180, 0.1428571428571428492, 0.1488095238095238082, 0.1547619047619047672, 0.1607142857142857262, 0.1666666666666666574, 0.1726190476190476164, 0.1785714285714285754, 0.1845238095238095344, 0.1904761904761904656, 0.1964285714285714246, 0.2023809523809523836, 0.2083333333333333426, 0.2142857142857142738, 0.2202380952380952328, 0.2261904761904761918, 0.2321428571428571508, 0.2380952380952380820, 0.2440476190476190410, 0.2500000000000000000, 0.2559523809523809312, 0.2619047619047619180, 0.2678571428571428492, 0.2738095238095238360, 0.2797619047619047672, 0.2857142857142856984, 0.2916666666666666852, 0.2976190476190476164, 0.3035714285714285476, 0.3095238095238095344, 0.3154761904761904656, 0.3214285714285714524, 0.3273809523809523836, 0.3333333333333333148, 0.3392857142857143016, 0.3452380952380952328, 0.3511904761904761640, 0.3571428571428571508, 0.3630952380952380820, 0.3690476190476190688, 0.3750000000000000000, 0.3809523809523809312, 0.3869047619047619180, 0.3928571428571428492, 0.3988095238095238360, 0.4047619047619047672, 0.4107142857142856984, 0.4166666666666666852, 0.4226190476190476164, 0.4285714285714285476, 0.4345238095238095344, 0.4404761904761904656, 0.4464285714285714524, 0.4523809523809523836, 0.4583333333333333148, 0.4642857142857143016, 0.4702380952380952328, 0.4761904761904761640, 0.4821428571428571508, 0.4880952380952380820, 0.4940476190476190688, 0.5000000000000000000, 0.5059523809523809312, 0.5119047619047618625, 0.5178571428571429047, 0.5238095238095238360, 0.5297619047619047672, 0.5357142857142856984, 0.5416666666666666297, 0.5476190476190476719, 0.5535714285714286031, 0.5595238095238095344, 0.5654761904761904656, 0.5714285714285713969, 0.5773809523809523281, 0.5833333333333333703, 0.5892857142857143016, 0.5952380952380952328, 0.6011904761904761640, 0.6071428571428570953, 0.6130952380952381375, 0.6190476190476190688, 0.6250000000000000000, 0.6309523809523809312, 0.6369047619047618625, 0.6428571428571429047, 0.6488095238095238360, 0.6547619047619047672, 0.6607142857142856984, 0.6666666666666666297, 0.6726190476190476719, 0.6785714285714286031, 0.6845238095238095344, 0.6904761904761904656, 0.6964285714285713969, 0.7023809523809523281, 0.7083333333333333703, 0.7142857142857143016, 0.7202380952380952328, 0.7261904761904761640, 0.7321428571428570953, 0.7380952380952381375, 0.7440476190476190688, 0.7500000000000000000, 0.7559523809523809312, 0.7619047619047618625, 0.7678571428571429047, 0.7738095238095238360, 0.7797619047619047672, 0.7857142857142856984, 0.7916666666666666297, 0.7976190476190476719, 0.8035714285714286031, 0.8095238095238095344, 0.8154761904761904656, 0.8214285714285713969, 0.8273809523809523281, 0.8333333333333333703, 0.8392857142857143016, 0.8452380952380952328, 0.8511904761904761640, 0.8571428571428570953, 0.8630952380952381375, 0.8690476190476190688, 0.8750000000000000000, 0.8809523809523809312, 0.8869047619047618625, 0.8928571428571429047, 0.8988095238095238360, 0.9047619047619047672, 0.9107142857142856984, 0.9166666666666666297, 0.9226190476190476719, 0.9285714285714286031, 0.9345238095238095344, 0.9404761904761904656, 0.9464285714285713969, 0.9523809523809523281, 0.9583333333333333703, 0.9642857142857143016 ),
 .UNSPECIFIED. ) 
 GEOMETRIC_REPRESENTATION_ITEM ( )  RATIONAL_B_SPLINE_SURFACE ( (
 ( 1.000000000000000000, 0.9659258262890683122, 1.000000000000000000, 0.9659258262890683122, 1.000000000000000000, 0.9659258262890683122, 1.000000000000000000, 0.9659258262890683122, 1.000000000000000000, 0.9659258262890683122, 1.000000000000000000, 0.9659258262890683122, 1.000000000000000000, 0.9659258262890683122, 1.000000000000000000, 0.9659258262890683122, 1.000000000000000000, 0.9659258262890683122, 1.000000000000000000, 0.9659258262890683122, 1.000000000000000000, 0.9659258262890683122, 1.000000000000000000, 0.9659258262890683122, 1.000000000000000000, 0.9659258262890683122, 1.000000000000000000, 0.9659258262890683122, 1.000000000000000000, 0.9659258262890683122, 1.000000000000000000, 0.9659258262890683122, 1.000000000000000000, 0.9659258262890683122, 1.000000000000000000, 0.9659258262890683122, 1.000000000000000000, 0.9659258262890683122, 1.000000000000000000, 0.9659258262890683122, 1.000000000000000000, 0.9659258262890683122, 1.000000000000000000, 0.9659258262890683122, 1.000000000000000000, 0.9659258262890683122, 1.000000000000000000, 0.9659258262890683122, 1.000000000000000000, 0.9659258262890683122, 1.000000000000000000, 0.9659258262890683122, 1.000000000000000000, 0.9659258262890683122, 1.000000000000000000, 0.9659258262890683122, 1.000000000000000000, 0.9659258262890683122, 1.000000000000000000, 0.9659258262890683122, 1.000000000000000000, 0.9659258262890683122, 1.000000000000000000, 0.9659258262890683122, 1.000000000000000000, 0.9659258262890683122, 1.000000000000000000, 0.9659258262890683122, 1.000000000000000000, 0.9659258262890683122, 1.000000000000000000, 0.9659258262890683122, 1.000000000000000000, 0.9659258262890683122, 1.000000000000000000, 0.9659258262890683122, 1.000000000000000000, 0.9659258262890683122, 1.000000000000000000, 0.9659258262890683122, 1.000000000000000000, 0.9659258262890683122, 1.000000000000000000, 0.9659258262890683122, 1.000000000000000000, 0.9659258262890683122, 1.000000000000000000, 0.9659258262890683122, 1.000000000000000000, 0.9659258262890683122, 1.000000000000000000, 0.9659258262890683122, 1.000000000000000000, 0.9659258262890683122, 1.000000000000000000, 0.9659258262890683122, 1.000000000000000000, 0.9659258262890683122, 1.000000000000000000, 0.9659258262890683122, 1.000000000000000000, 0.9659258262890683122, 1.000000000000000000, 0.9659258262890683122, 1.000000000000000000, 0.9659258262890683122, 1.000000000000000000, 0.9659258262890683122, 1.000000000000000000, 0.9659258262890683122, 1.000000000000000000, 0.9659258262890683122, 1.000000000000000000, 0.9659258262890683122, 1.000000000000000000, 0.9659258262890683122, 1.000000000000000000, 0.9659258262890683122, 1.000000000000000000, 0.9659258262890683122, 1.000000000000000000, 0.9659258262890683122, 1.000000000000000000, 0.9659258262890683122, 1.000000000000000000, 0.9659258262890683122, 1.000000000000000000, 0.9659258262890683122, 1.000000000000000000, 0.9659258262890683122, 1.000000000000000000, 0.9659258262890683122, 1.000000000000000000, 0.9659258262890683122, 1.000000000000000000, 0.9659258262890683122, 1.000000000000000000, 0.9659258262890683122, 1.000000000000000000, 0.9659258262890683122, 1.000000000000000000, 0.9659258262890683122, 1.000000000000000000, 0.9659258262890683122, 1.000000000000000000, 0.9659258262890683122, 1.000000000000000000, 0.9659258262890683122, 1.000000000000000000, 0.9659258262890683122, 1.000000000000000000, 0.9659258262890683122, 1.000000000000000000, 0.9659258262890683122, 1.000000000000000000, 0.9659258262890683122, 1.000000000000000000, 0.9659258262890683122, 1.000000000000000000, 0.9659258262890683122, 1.000000000000000000, 0.9659258262890683122, 1.000000000000000000, 0.9659258262890683122, 1.000000000000000000, 0.9659258262890683122, 1.000000000000000000, 0.9659258262890683122, 1.000000000000000000, 0.9659258262890683122, 1.000000000000000000, 0.9659258262890683122, 1.000000000000000000, 0.9659258262890683122, 1.000000000000000000, 0.9659258262890683122, 1.000000000000000000, 0.9659258262890683122, 1.000000000000000000, 0.9659258262890683122, 1.000000000000000000, 0.9659258262890683122, 1.000000000000000000, 0.9659258262890683122, 1.000000000000000000, 0.9659258262890683122, 1.000000000000000000, 0.9659258262890683122, 1.000000000000000000, 0.9659258262890683122, 1.000000000000000000, 0.9659258262890683122, 1.000000000000000000, 0.9659258262890683122, 1.000000000000000000, 0.9659258262890683122, 1.000000000000000000, 0.9659258262890683122, 1.000000000000000000, 0.9659258262890683122, 1.000000000000000000, 0.9659258262890683122, 1.000000000000000000, 0.9659258262890683122, 1.000000000000000000, 0.9659258262890683122, 1.000000000000000000, 0.9659258262890683122, 1.000000000000000000, 0.9659258262890683122, 1.000000000000000000, 0.9659258262890683122, 1.000000000000000000, 0.9659258262890683122, 1.000000000000000000, 0.9659258262890683122, 1.000000000000000000, 0.9659258262890683122, 1.000000000000000000, 0.9659258262890683122, 1.000000000000000000, 0.9659258262890683122, 1.000000000000000000, 0.9659258262890683122, 1.000000000000000000, 0.9659258262890683122, 1.000000000000000000, 0.9659258262890683122, 1.000000000000000000, 0.9659258262890683122, 1.000000000000000000, 0.9659258262890683122, 1.000000000000000000, 0.9659258262890683122, 1.000000000000000000, 0.9659258262890683122, 1.000000000000000000, 0.9659258262890683122, 1.000000000000000000, 0.9659258262890683122, 1.000000000000000000, 0.9659258262890683122, 1.000000000000000000, 0.9659258262890683122, 1.000000000000000000, 0.9659258262890683122, 1.000000000000000000, 0.9659258262890683122, 1.000000000000000000, 0.9659258262890683122, 1.000000000000000000, 0.9659258262890683122, 1.000000000000000000, 0.9659258262890683122, 1.000000000000000000, 0.9659258262890683122, 1.000000000000000000, 0.9659258262890683122, 1.000000000000000000, 0.9659258262890683122, 1.000000000000000000, 0.9659258262890683122, 1.000000000000000000, 0.9659258262890683122, 1.000000000000000000, 0.9659258262890683122, 1.000000000000000000, 0.9659258262890683122, 1.000000000000000000, 0.9659258262890683122, 1.000000000000000000, 0.9659258262890683122, 1.000000000000000000, 0.9659258262890683122, 1.000000000000000000, 0.9659258262890683122, 1.000000000000000000, 0.9659258262890683122, 1.000000000000000000, 0.9659258262890683122, 1.000000000000000000, 0.9659258262890683122, 1.000000000000000000, 0.9659258262890683122, 1.000000000000000000, 0.9659258262890683122, 1.000000000000000000, 0.9659258262890683122, 1.000000000000000000, 0.9659258262890683122, 1.000000000000000000, 0.9659258262890683122, 1.000000000000000000, 0.9659258262890683122, 1.000000000000000000, 0.9659258262890683122, 1.000000000000000000, 0.9659258262890683122, 1.000000000000000000, 0.9659258262890683122, 1.000000000000000000, 0.9659258262890683122, 1.000000000000000000, 0.9659258262890683122, 1.000000000000000000, 0.9659258262890683122, 1.000000000000000000, 0.9659258262890683122, 1.000000000000000000, 0.9659258262890683122, 1.000000000000000000, 0.9659258262890683122, 1.000000000000000000, 0.9659258262890683122, 1.000000000000000000, 0.9659258262890683122, 1.000000000000000000, 0.9659258262890683122, 1.000000000000000000, 0.9659258262890683122, 1.000000000000000000, 0.9659258262890683122, 1.000000000000000000, 0.9659258262890683122, 1.000000000000000000),
 ( 1.000000000000000000, 0.9659258262890683122, 1.000000000000000000, 0.9659258262890683122, 1.000000000000000000, 0.9659258262890683122, 1.000000000000000000, 0.9659258262890683122, 1.000000000000000000, 0.9659258262890683122, 1.000000000000000000, 0.9659258262890683122, 1.000000000000000000, 0.9659258262890683122, 1.000000000000000000, 0.9659258262890683122, 1.000000000000000000, 0.9659258262890683122, 1.000000000000000000, 0.9659258262890683122, 1.000000000000000000, 0.9659258262890683122, 1.000000000000000000, 0.9659258262890683122, 1.000000000000000000, 0.9659258262890683122, 1.000000000000000000, 0.9659258262890683122, 1.000000000000000000, 0.9659258262890683122, 1.000000000000000000, 0.9659258262890683122, 1.000000000000000000, 0.9659258262890683122, 1.000000000000000000, 0.9659258262890683122, 1.000000000000000000, 0.9659258262890683122, 1.000000000000000000, 0.9659258262890683122, 1.000000000000000000, 0.9659258262890683122, 1.000000000000000000, 0.9659258262890683122, 1.000000000000000000, 0.9659258262890683122, 1.000000000000000000, 0.9659258262890683122, 1.000000000000000000, 0.9659258262890683122, 1.000000000000000000, 0.9659258262890683122, 1.000000000000000000, 0.9659258262890683122, 1.000000000000000000, 0.9659258262890683122, 1.000000000000000000, 0.9659258262890683122, 1.000000000000000000, 0.9659258262890683122, 1.000000000000000000, 0.9659258262890683122, 1.000000000000000000, 0.9659258262890683122, 1.000000000000000000, 0.9659258262890683122, 1.000000000000000000, 0.9659258262890683122, 1.000000000000000000, 0.9659258262890683122, 1.000000000000000000, 0.9659258262890683122, 1.000000000000000000, 0.9659258262890683122, 1.000000000000000000, 0.9659258262890683122, 1.000000000000000000, 0.9659258262890683122, 1.000000000000000000, 0.9659258262890683122, 1.000000000000000000, 0.9659258262890683122, 1.000000000000000000, 0.9659258262890683122, 1.000000000000000000, 0.9659258262890683122, 1.000000000000000000, 0.9659258262890683122, 1.000000000000000000, 0.9659258262890683122, 1.000000000000000000, 0.9659258262890683122, 1.000000000000000000, 0.9659258262890683122, 1.000000000000000000, 0.9659258262890683122, 1.000000000000000000, 0.9659258262890683122, 1.000000000000000000, 0.9659258262890683122, 1.000000000000000000, 0.9659258262890683122, 1.000000000000000000, 0.9659258262890683122, 1.000000000000000000, 0.9659258262890683122, 1.000000000000000000, 0.9659258262890683122, 1.000000000000000000, 0.9659258262890683122, 1.000000000000000000, 0.9659258262890683122, 1.000000000000000000, 0.9659258262890683122, 1.000000000000000000, 0.9659258262890683122, 1.000000000000000000, 0.9659258262890683122, 1.000000000000000000, 0.9659258262890683122, 1.000000000000000000, 0.9659258262890683122, 1.000000000000000000, 0.9659258262890683122, 1.000000000000000000, 0.9659258262890683122, 1.000000000000000000, 0.9659258262890683122, 1.000000000000000000, 0.9659258262890683122, 1.000000000000000000, 0.9659258262890683122, 1.000000000000000000, 0.9659258262890683122, 1.000000000000000000, 0.9659258262890683122, 1.000000000000000000, 0.9659258262890683122, 1.000000000000000000, 0.9659258262890683122, 1.000000000000000000, 0.9659258262890683122, 1.000000000000000000, 0.9659258262890683122, 1.000000000000000000, 0.9659258262890683122, 1.000000000000000000, 0.9659258262890683122, 1.000000000000000000, 0.9659258262890683122, 1.000000000000000000, 0.9659258262890683122, 1.000000000000000000, 0.9659258262890683122, 1.000000000000000000, 0.9659258262890683122, 1.000000000000000000, 0.9659258262890683122, 1.000000000000000000, 0.9659258262890683122, 1.000000000000000000, 0.9659258262890683122, 1.000000000000000000, 0.9659258262890683122, 1.000000000000000000, 0.9659258262890683122, 1.000000000000000000, 0.9659258262890683122, 1.000000000000000000, 0.9659258262890683122, 1.000000000000000000, 0.9659258262890683122, 1.000000000000000000, 0.9659258262890683122, 1.000000000000000000, 0.9659258262890683122, 1.000000000000000000, 0.9659258262890683122, 1.000000000000000000, 0.9659258262890683122, 1.000000000000000000, 0.9659258262890683122, 1.000000000000000000, 0.9659258262890683122, 1.000000000000000000, 0.9659258262890683122, 1.000000000000000000, 0.9659258262890683122, 1.000000000000000000, 0.9659258262890683122, 1.000000000000000000, 0.9659258262890683122, 1.000000000000000000, 0.9659258262890683122, 1.000000000000000000, 0.9659258262890683122, 1.000000000000000000, 0.9659258262890683122, 1.000000000000000000, 0.9659258262890683122, 1.000000000000000000, 0.9659258262890683122, 1.000000000000000000, 0.9659258262890683122, 1.000000000000000000, 0.9659258262890683122, 1.000000000000000000, 0.9659258262890683122, 1.000000000000000000, 0.9659258262890683122, 1.000000000000000000, 0.9659258262890683122, 1.000000000000000000, 0.9659258262890683122, 1.000000000000000000, 0.9659258262890683122, 1.000000000000000000, 0.9659258262890683122, 1.000000000000000000, 0.9659258262890683122, 1.000000000000000000, 0.9659258262890683122, 1.000000000000000000, 0.9659258262890683122, 1.000000000000000000, 0.9659258262890683122, 1.000000000000000000, 0.9659258262890683122, 1.000000000000000000, 0.9659258262890683122, 1.000000000000000000, 0.9659258262890683122, 1.000000000000000000, 0.9659258262890683122, 1.000000000000000000, 0.9659258262890683122, 1.000000000000000000, 0.9659258262890683122, 1.000000000000000000, 0.9659258262890683122, 1.000000000000000000, 0.9659258262890683122, 1.000000000000000000, 0.9659258262890683122, 1.000000000000000000, 0.9659258262890683122, 1.000000000000000000, 0.9659258262890683122, 1.000000000000000000, 0.9659258262890683122, 1.000000000000000000, 0.9659258262890683122, 1.000000000000000000, 0.9659258262890683122, 1.000000000000000000, 0.9659258262890683122, 1.000000000000000000, 0.9659258262890683122, 1.000000000000000000, 0.9659258262890683122, 1.000000000000000000, 0.9659258262890683122, 1.000000000000000000, 0.9659258262890683122, 1.000000000000000000, 0.9659258262890683122, 1.000000000000000000, 0.9659258262890683122, 1.000000000000000000, 0.9659258262890683122, 1.000000000000000000, 0.9659258262890683122, 1.000000000000000000, 0.9659258262890683122, 1.000000000000000000, 0.9659258262890683122, 1.000000000000000000, 0.9659258262890683122, 1.000000000000000000, 0.9659258262890683122, 1.000000000000000000, 0.9659258262890683122, 1.000000000000000000, 0.9659258262890683122, 1.000000000000000000, 0.9659258262890683122, 1.000000000000000000, 0.9659258262890683122, 1.000000000000000000, 0.9659258262890683122, 1.000000000000000000, 0.9659258262890683122, 1.000000000000000000, 0.9659258262890683122, 1.000000000000000000, 0.9659258262890683122, 1.000000000000000000, 0.9659258262890683122, 1.000000000000000000, 0.9659258262890683122, 1.000000000000000000, 0.9659258262890683122, 1.000000000000000000, 0.9659258262890683122, 1.000000000000000000, 0.9659258262890683122, 1.000000000000000000, 0.9659258262890683122, 1.000000000000000000, 0.9659258262890683122, 1.000000000000000000, 0.9659258262890683122, 1.000000000000000000, 0.9659258262890683122, 1.000000000000000000, 0.9659258262890683122, 1.000000000000000000, 0.9659258262890683122, 1.000000000000000000, 0.9659258262890683122, 1.000000000000000000, 0.9659258262890683122, 1.000000000000000000, 0.9659258262890683122, 1.000000000000000000) ) ) 
 REPRESENTATION_ITEM ( '' )  SURFACE ( )  );
#93661 = CARTESIAN_POINT ( 'NONE',  ( 20.15039907845753575, 15.60158574516642815, -6.262539305110077059 ) ) ;
#93662 =( GEOMETRIC_REPRESENTATION_CONTEXT ( 3 ) GLOBAL_UNCERTAINTY_ASSIGNED_CONTEXT ( ( #11176 ) ) GLOBAL_UNIT_ASSIGNED_CONTEXT ( ( #16772, #46281, #30765 ) ) REPRESENTATION_CONTEXT ( 'NONE', 'WORKASPACE' ) );
#93663 = CIRCLE ( 'NONE', #1054, 3.940000000000000835 ) ;
#93664 = ORIENTED_EDGE ( 'NONE', *, *, #73087, .F. ) ;
#93665 = CARTESIAN_POINT ( 'NONE',  ( 22.26659068614895176, 64.72041550158064638, -7.082119434687042414 ) ) ;
#93666 = DIRECTION ( 'NONE',  ( -1.000000000000000000, -2.799047438454523729E-16, -0.000000000000000000 ) ) ;
#93667 = CARTESIAN_POINT ( 'NONE',  ( 15.44008868035555260, 39.73035201082150536, 9.422509992056143702 ) ) ;
#93669 = CARTESIAN_POINT ( 'NONE',  ( 17.96484262340118221, 56.18868534415484817, -7.964842623401177768 ) ) ;
#93668 = CARTESIAN_POINT ( 'NONE',  ( 19.38216949554541557, 7.248634669930421381, -9.382169495545420901 ) ) ;
#93670 = CARTESIAN_POINT ( 'NONE',  ( 13.96521320569125102, 14.95077488074853456, -4.755935267939162436 ) ) ;
#93671 = CARTESIAN_POINT ( 'NONE',  ( 0.000000000000000000, 15.00000000000000000, 0.000000000000000000 ) ) ;
#93672 = CARTESIAN_POINT ( 'NONE',  ( -3.243710765982268818, 0.000000000000000000, -4.383623511354931779 ) ) ;
#93673 = CARTESIAN_POINT ( 'NONE',  ( 0.4400000000000020006, 1.019547802438468986, -2.750000000000000000 ) ) ;
#93674 = CARTESIAN_POINT ( 'NONE',  ( 5.076628168052703671, 46.84226448433412315, 8.527530157486179263 ) ) ;
#93675 = CARTESIAN_POINT ( 'NONE',  ( 10.88017736071110164, -34.64464798917848753, 2.915334737309921209 ) ) ;
#93676 = CARTESIAN_POINT ( 'NONE',  ( 10.00000000000000178, 10.37363466993041961, 12.81628187352647608 ) ) ;
#93678 = LINE ( 'NONE', #10195, #17031 ) ;
#93677 = CARTESIAN_POINT ( 'NONE',  ( 12.91533473730992121, 14.52201867748817143, 10.88017736071110164 ) ) ;
#93679 = DIRECTION ( 'NONE',  ( 0.000000000000000000, 0.000000000000000000, 1.000000000000000000 ) ) ;
#93680 = CARTESIAN_POINT ( 'NONE',  ( 6.204703633549690345, 32.84541550158063927, 14.16423886937410082 ) ) ;
#93681 = EDGE_CURVE ( 'NONE', #68278, #94075, #74473, .T. ) ;
#93682 = CARTESIAN_POINT ( 'NONE',  ( -4.164238869374099927, 32.01208216824730357, 3.795296366450308767 ) ) ;
#93683 = CARTESIAN_POINT ( 'NONE',  ( 6.204703633549690345, 67.84541550158060375, 14.16423886937410082 ) ) ;
#93684 = TOROIDAL_SURFACE ( 'NONE', #85701, 14.49999999999999822, 0.5000000000000000000 ) ;
#93685 = CARTESIAN_POINT ( 'NONE',  ( 0.6178305044545838731, 39.74863466993041072, 9.382169495545420901 ) ) ;
#93686 = CARTESIAN_POINT ( 'NONE',  ( 2.035157376598824452, 18.68868534415484106, 7.964842623401179544 ) ) ;
#93687 = EDGE_LOOP ( 'NONE', ( #55026, #556, #22453, #74578 ) ) ;
#93688 = CARTESIAN_POINT ( 'NONE',  ( 5.076628168052703671, 36.84226448433412315, 8.527530157486179263 ) ) ;
#93689 = CARTESIAN_POINT ( 'NONE',  ( 20.88017736071110875, 35.77201867748816966, -2.915334737309920765 ) ) ;
#93690 = CARTESIAN_POINT ( 'NONE',  ( 18.52753015748617571, 58.09226448433411605, 4.923371831947298993 ) ) ;
#93692 = CARTESIAN_POINT ( 'NONE',  ( -0.2418659066527499291, 17.23410085661204150, -6.114288769123083611 ) ) ;
#93691 = CARTESIAN_POINT ( 'NONE',  ( 10.00000000000000000, 25.55374883491396787, -14.16423886937410082 ) ) ;
#93693 = CARTESIAN_POINT ( 'NONE',  ( 18.72515096720573879, 35.05509018479936145, 6.499999999999937828 ) ) ;
#93694 = CARTESIAN_POINT ( 'NONE',  ( 0.1532563361054082862, 26.21726448433411605, 2.638427012816831674 ) ) ;
#93695 = CARTESIAN_POINT ( 'NONE',  ( 16.40814093676323893, 55.79030133659708923, 11.09922568453595026 ) ) ;
#93696 = CARTESIAN_POINT ( 'NONE',  ( 0.1532563361054083140, 56.00893115100078745, 1.131784320476157264E-15 ) ) ;
#93697 = VERTEX_POINT ( 'NONE', #67976 ) ;
#93698 = CARTESIAN_POINT ( 'NONE',  ( 8.375939845167682307, -0.03417435944610275333, 11.52849216984304448 ) ) ;
#93699 = DIRECTION ( 'NONE',  ( 0.000000000000000000, -1.000000000000000000, 0.000000000000000000 ) ) ;
#93700 = CARTESIAN_POINT ( 'NONE',  ( 2.917880565312950480, 65.97041550158063217, -12.26659068614894821 ) ) ;
#93701 = CARTESIAN_POINT ( 'NONE',  ( 20.36894250292379738, 14.92874883491396432, -10.36894250292379027 ) ) ;
#93702 = CARTESIAN_POINT ( 'NONE',  ( 17.96484262340118221, 66.18868534415483396, -7.964842623401177768 ) ) ;
#93703 = CARTESIAN_POINT ( 'NONE',  ( 1.472469842513823179, 56.42559781766745886, 4.923371831947296329 ) ) ;
#93704 = CARTESIAN_POINT ( 'NONE',  ( 10.00000000000000178, 24.31368534415484106, 10.88017736071110342 ) ) ;
#93705 = CARTESIAN_POINT ( 'NONE',  ( 27.50000000000000355, 35.99999999999997158, 10.00000000000000000 ) ) ;
#93706 = CYLINDRICAL_SURFACE ( 'NONE', #39413, 0.5000000000000004441 ) ;
#93707 = CARTESIAN_POINT ( 'NONE',  ( 18.52753015748618282, 3.925597817667451306, -4.923371831947291888 ) ) ;
#93708 = CARTESIAN_POINT ( 'NONE',  ( 10.00000000000000000, 62.87363466993042493, -12.81628187352647608 ) ) ;
#93709 = VERTEX_POINT ( 'NONE', #36982 ) ;
#93710 = EDGE_LOOP ( 'NONE', ( #25376, #40865, #436, #64690, #16285, #81573 ) ) ;
#93711 = CARTESIAN_POINT ( 'NONE',  ( 20.15039907845753930, 70.00000000000000000, -6.262539305110068177 ) ) ;
#93712 = PLANE ( 'NONE',  #73421 ) ;
#93713 = EDGE_CURVE ( 'NONE', #49375, #34270, #98501, .T. ) ;
#93714 = CARTESIAN_POINT ( 'NONE',  ( -0.3689425029237881626, 47.42874883491396787, 10.36894250292379027 ) ) ;
#93715 = CARTESIAN_POINT ( 'NONE',  ( 2.791683348922240793, 51.63393115100078745, 7.208316651077764092 ) ) ;
#93716 = CARTESIAN_POINT ( 'NONE',  ( 7.361572987183169658, 24.96726448433412315, -9.846743663894592657 ) ) ;
#93717 =( NAMED_UNIT ( * ) PLANE_ANGLE_UNIT ( ) SI_UNIT ( $, .RADIAN. ) );
#93719 = CARTESIAN_POINT ( 'NONE',  ( 12.63842701281683922, 59.55059781766744464, -9.846743663894590881 ) ) ;
#93718 = CARTESIAN_POINT ( 'NONE',  ( 19.42250999205614548, 25.98035201082150891, -5.440088680355545492 ) ) ;
#93720 = CARTESIAN_POINT ( 'NONE',  ( 13.95806775979394487, 15.00000000000000888, 4.371577651620829563 ) ) ;
#93721 = CARTESIAN_POINT ( 'NONE',  ( -4.164238869374099927, 37.01208216824731068, 3.795296366450308767 ) ) ;
#93722 = AXIS2_PLACEMENT_3D ( 'NONE', #8024, #25496, #46988 ) ;
#93723 = CARTESIAN_POINT ( 'NONE',  ( -4.164238869374099039, 51.80374883491396787, 8.674139862899312516E-16 ) ) ;
#93724 = CYLINDRICAL_SURFACE ( 'NONE', #13072, 0.5000000000000004441 ) ;
#93725 = LINE ( 'NONE', #55231, #68364 ) ;
#93726 = CARTESIAN_POINT ( 'NONE',  ( 12.91533473730992121, 59.52201867748816966, 10.88017736071110164 ) ) ;
#93727 = EDGE_CURVE ( 'NONE', #62035, #38580, #89974, .T. ) ;
#93728 = CARTESIAN_POINT ( 'NONE',  ( 14.92337183194729988, 14.34226448433411782, -8.527530157486177487 ) ) ;
#93729 = CARTESIAN_POINT ( 'NONE',  ( -7.287642027973244119, -86.26866148728002770, 4.000000000000000000 ) ) ;
#93730 = ORIENTED_EDGE ( 'NONE', *, *, #55674, .T. ) ;
#93731 = CARTESIAN_POINT ( 'NONE',  ( -14.04391541078765826, 15.00000000000000000, 3.608107528142729503 ) ) ;
#93732 = ORIENTED_EDGE ( 'NONE', *, *, #26045, .T. ) ;
#93733 = CARTESIAN_POINT ( 'NONE',  ( 7.361572987183169658, 29.96726448433411960, -9.846743663894592657 ) ) ;
#93734 = VERTEX_POINT ( 'NONE', #67481 ) ;
#93735 = CARTESIAN_POINT ( 'NONE',  ( -0.3689425029237881626, 37.42874883491396787, 10.36894250292379027 ) ) ;
#93736 = CARTESIAN_POINT ( 'NONE',  ( 17.20831665107776587, 27.88393115100078390, 7.208316651077764980 ) ) ;
#93737 = CARTESIAN_POINT ( 'NONE',  ( 20.88017736071110164, 40.35535201082150536, 2.915334737309930979 ) ) ;
#93738 = FACE_OUTER_BOUND ( 'NONE', #49212, .T. ) ;
#93739 = EDGE_LOOP ( 'NONE', ( #88195, #82911, #32848, #40974 ) ) ;
#93740 = CARTESIAN_POINT ( 'NONE',  ( -0.8801773607111009756, 43.06368534415484106, 1.068504757029289695E-15 ) ) ;
#93741 = CARTESIAN_POINT ( 'NONE',  ( 0.000000000000000000, 15.00000000000000000, 0.000000000000000000 ) ) ;
#93742 = VECTOR ( 'NONE', #50611, 1000.000000000000227 ) ;
#93743 = CARTESIAN_POINT ( 'NONE',  ( -11.09922568453594316, -5.459698663402908103, 6.408140936763246920 ) ) ;
#93744 = ORIENTED_EDGE ( 'NONE', *, *, #43586, .T. ) ;
#93745 = CARTESIAN_POINT ( 'NONE',  ( -4.164238869374099039, 6.803748834913967869, 8.674139862899312516E-16 ) ) ;
#93746 = VERTEX_POINT ( 'NONE', #21993 ) ;
#93747 = CARTESIAN_POINT ( 'NONE',  ( 19.38216949554541202, 35.99863466993041072, 9.382169495545424454 ) ) ;
#93748 = AXIS2_PLACEMENT_3D ( 'NONE', #86735, #8277, #38775 ) ;
#93749 =( NAMED_UNIT ( * ) SI_UNIT ( $, .STERADIAN. ) SOLID_ANGLE_UNIT ( ) );
#93750 = CARTESIAN_POINT ( 'NONE',  ( 12.63842701281683034, 27.46726448433411250, 9.846743663894596210 ) ) ;
#93751 =( LENGTH_UNIT ( ) NAMED_UNIT ( * ) SI_UNIT ( .MILLI., .METRE. ) );
#93752 = CARTESIAN_POINT ( 'NONE',  ( 20.88017736071110875, 10.77201867748817143, -2.915334737309920321 ) ) ;
#93753 = CARTESIAN_POINT ( 'NONE',  ( 19.84674366389459621, 33.50893115100078745, 7.409399052514197653E-17 ) ) ;
#93754 = VECTOR ( 'NONE', #64953, 1000.000000000000000 ) ;
#93755 = EDGE_CURVE ( 'NONE', #10984, #36088, #16547, .T. ) ;
#93756 = CIRCLE ( 'NONE', #28310, 0.2500000000000002220 ) ;
#93757 = MECHANICAL_DESIGN_GEOMETRIC_PRESENTATION_REPRESENTATION (  '', ( #72981 ), #42657 ) ;
#93758 = ORIENTED_EDGE ( 'NONE', *, *, #32285, .F. ) ;
#93759 = CARTESIAN_POINT ( 'NONE',  ( 1.326261724322855828, 0.2301504087165518186, 14.88164196614421186 ) ) ;
#93760 = CARTESIAN_POINT ( 'NONE',  ( 4.559911319644449179, 58.89701867748817676, 9.422509992056141925 ) ) ;
#93761 = CARTESIAN_POINT ( 'NONE',  ( 9.240973841163532043, 4.236086333263440692E-16, 11.17382667070378943 ) ) ;
#93762 = SURFACE_SIDE_STYLE ('',( #77770 ) ) ;
#93763 = CARTESIAN_POINT ( 'NONE',  ( 17.20831665107776587, 7.883931151000784787, 7.208316651077764980 ) ) ;
#93764 = CARTESIAN_POINT ( 'NONE',  ( 19.38216949554541557, 12.24863466993041961, -9.382169495545420901 ) ) ;
#93765 = DIRECTION ( 'NONE',  ( -0.7372773368101205316, 0.000000000000000000, -0.6755902076156641289 ) ) ;
#93766 = EDGE_CURVE ( 'NONE', #76727, #22152, #6982, .T. ) ;
#93767 = CARTESIAN_POINT ( 'NONE',  ( 14.92337183194729633, 47.67559781766745175, 8.527530157486181039 ) ) ;
#93768 = DIRECTION ( 'NONE',  ( -0.000000000000000000, -1.000000000000000000, -0.000000000000000000 ) ) ;
#93769 = CARTESIAN_POINT ( 'NONE',  ( 2.917880565312948704, 12.63708216824730179, 12.26659068614894643 ) ) ;
#93770 = CARTESIAN_POINT ( 'NONE',  ( 18.52753015748618282, 18.92559781766745175, -4.923371831947291888 ) ) ;
#93771 = CARTESIAN_POINT ( 'NONE',  ( 6.565887622018943937, 33.08196800326374643, -12.81628187352647608 ) ) ;
#93773 = DIRECTION ( 'NONE',  ( -0.000000000000000000, -1.000000000000000000, -0.000000000000000000 ) ) ;
#93772 = CARTESIAN_POINT ( 'NONE',  ( 14.42956166533735640, -2.687212025164267037E-15, 2.386684097925098502 ) ) ;
#93774 = CARTESIAN_POINT ( 'NONE',  ( -0.8801773607111009756, 48.06368534415484817, 1.068504757029289695E-15 ) ) ;
#93775 = CARTESIAN_POINT ( 'NONE',  ( 21.09922568453594849, 11.20696800326375531, 6.408140936763242479 ) ) ;
#93776 = DIRECTION ( 'NONE',  ( -1.000000000000000000, 0.000000000000000000, 0.000000000000000000 ) ) ;
#93777 = CARTESIAN_POINT ( 'NONE',  ( 7.361572987183170547, 22.05059781766745530, 9.846743663894590881 ) ) ;
#93778 = CARTESIAN_POINT ( 'NONE',  ( 19.42250999205614548, 30.98035201082150536, -5.440088680355545492 ) ) ;
#93779 = CARTESIAN_POINT ( 'NONE',  ( 16.40814093676323893, 25.79030133659708923, 11.09922568453595026 ) ) ;
#93780 = CARTESIAN_POINT ( 'NONE',  ( 0.1532563361054100626, 20.80059781766744464, -2.638427012816831230 ) ) ;
#93781 = CARTESIAN_POINT ( 'NONE',  ( -8.114998381645635916, 86.24535146302233102, 4.289708087854926077 ) ) ;
#93782 = CARTESIAN_POINT ( 'NONE',  ( 0.5774900079438607392, 18.48035201082150536, 5.440088680355550821 ) ) ;
#93783 =( GEOMETRIC_REPRESENTATION_CONTEXT ( 3 ) GLOBAL_UNCERTAINTY_ASSIGNED_CONTEXT ( ( #72417 ) ) GLOBAL_UNIT_ASSIGNED_CONTEXT ( ( #64780, #49792, #94310 ) ) REPRESENTATION_CONTEXT ( 'NONE', 'WORKASPACE' ) );
#93784 = ADVANCED_FACE ( 'NONE', ( #8810 ), #40527, .T. ) ;
#93785 = CARTESIAN_POINT ( 'NONE',  ( 2.035157376598822676, 57.43868534415484106, -7.964842623401177768 ) ) ;
#93786 = CARTESIAN_POINT ( 'NONE',  ( 4.395797040798986366, -0.8371465525320274104, 2.750000000000000444 ) ) ;
#93788 = CARTESIAN_POINT ( 'NONE',  ( -0.8801773607111009756, 23.06368534415484106, 1.068504757029289695E-15 ) ) ;
#93787 = CARTESIAN_POINT ( 'NONE',  ( 0.1532563361054082862, 41.21726448433411605, 2.638427012816831674 ) ) ;
#93789 = DIRECTION ( 'NONE',  ( 0.000000000000000000, -0.000000000000000000, 1.000000000000000000 ) ) ;
#93790 = CARTESIAN_POINT ( 'NONE',  ( 20.88017736071110519, 50.56368534415484106, 2.639326808657452039E-16 ) ) ;
#93792 =( NAMED_UNIT ( * ) PLANE_ANGLE_UNIT ( ) SI_UNIT ( $, .RADIAN. ) );
#93791 = CARTESIAN_POINT ( 'NONE',  ( 2.035157376598822676, 17.43868534415483751, -7.964842623401177768 ) ) ;
#93793 = CARTESIAN_POINT ( 'NONE',  ( 12.63842701281683034, 17.46726448433411250, 9.846743663894596210 ) ) ;
#93794 = CARTESIAN_POINT ( 'NONE',  ( 5.076628168052704559, 40.17559781766745175, -8.527530157486179263 ) ) ;
#93795 = CARTESIAN_POINT ( 'NONE',  ( -16.94999999999999574, 99.99999999999998579, -7.750000000000000000 ) ) ;
#93796 = CARTESIAN_POINT ( 'NONE',  ( 1.602071938427511721, 7.022241923386403961, -6.500000000000008882 ) ) ;
#93797 = CARTESIAN_POINT ( 'NONE',  ( 18.52753015748617571, 63.09226448433412315, 4.923371831947298993 ) ) ;
#93798 = EDGE_CURVE ( 'NONE', #86051, #83178, #78430, .T. ) ;
#93799 = CARTESIAN_POINT ( 'NONE',  ( 10.00000000000000000, 25.55374883491396787, -14.16423886937410082 ) ) ;
#93800 = CARTESIAN_POINT ( 'NONE',  ( 1.472469842513823179, 41.42559781766745886, 4.923371831947296329 ) ) ;
#93801 = CARTESIAN_POINT ( 'NONE',  ( 34.56412365047463453, 13.99999999999999645, 9.500000000000000000 ) ) ;
#93802 = ORIENTED_EDGE ( 'NONE', *, *, #9899, .F. ) ;
#93803 = CARTESIAN_POINT ( 'NONE',  ( 10.00000000000000000, 6.813685344154838397, -10.88017736071110342 ) ) ;
#93804 = EDGE_CURVE ( 'NONE', #37334, #56877, #61781, .T. ) ;
#93805 = ADVANCED_FACE ( 'NONE', ( #68961 ), #84457, .T. ) ;
#93806 = CARTESIAN_POINT ( 'NONE',  ( 7.361572987183170547, 27.05059781766745175, 9.846743663894590881 ) ) ;
#93807 = CARTESIAN_POINT ( 'NONE',  ( -7.803778109523453743, 84.96281847254653030, -4.037836297607493741 ) ) ;
#93808 = CARTESIAN_POINT ( 'NONE',  ( 15.44008868035555793, 46.39701867748817676, -9.422509992056140149 ) ) ;
#93809 = CARTESIAN_POINT ( 'NONE',  ( 3.420591144908454950, 14.63595249122788999, 14.60477854057959490 ) ) ;
#93810 = CARTESIAN_POINT ( 'NONE',  ( 17.96484262340118221, 16.18868534415483396, -7.964842623401177768 ) ) ;
#93811 = CARTESIAN_POINT ( 'NONE',  ( -2.816281873526473856, 44.12363466993042493, 9.499525473075851096E-16 ) ) ;
#93812 = CARTESIAN_POINT ( 'NONE',  ( -1.099225684535947600, 14.54030133659708568, 6.408140936763237150 ) ) ;
#93813 = CARTESIAN_POINT ( 'NONE',  ( 0.1532563361054083140, 21.00893115100078745, 1.131784320476157264E-15 ) ) ;
#93814 = ORIENTED_EDGE ( 'NONE', *, *, #63242, .T. ) ;
#93815 = DIRECTION ( 'NONE',  ( 1.000000000000000000, 0.000000000000000000, 0.000000000000000000 ) ) ;
#93816 = CARTESIAN_POINT ( 'NONE',  ( 2.815433093577111467, 14.49999999999999112, -14.73340885523756683 ) ) ;
#93817 = CARTESIAN_POINT ( 'NONE',  ( 22.26659068614894466, 48.88708216824730357, 7.082119434687054849 ) ) ;
#93818 = CARTESIAN_POINT ( 'NONE',  ( 6.204703633549690345, 22.84541550158062861, 14.16423886937410082 ) ) ;
#93819 = CARTESIAN_POINT ( 'NONE',  ( 12.91533473730992121, 24.52201867748816966, 10.88017736071110164 ) ) ;
#93820 = COLOUR_RGB ( '', 0.31764706, 0.68627451, 0.89019608) ;
#93821 = CARTESIAN_POINT ( 'NONE',  ( 10.00000000000000000, 51.81368534415484106, -10.88017736071110342 ) ) ;
#93822 = SURFACE_STYLE_FILL_AREA ( #48806 ) ;
#93823 = CARTESIAN_POINT ( 'NONE',  ( 11.15633344610952804, -69.21805206901655083, -4.000000000000000000 ) ) ;
#93824 = CARTESIAN_POINT ( 'NONE',  ( 0.1532563361054100626, 10.80059781766745175, -2.638427012816831230 ) ) ;
#93825 = CARTESIAN_POINT ( 'NONE',  ( 5.076628168052704559, 15.17559781766745175, -8.527530157486179263 ) ) ;
#93826 =( NAMED_UNIT ( * ) SI_UNIT ( $, .STERADIAN. ) SOLID_ANGLE_UNIT ( ) );
#93827 = CARTESIAN_POINT ( 'NONE',  ( 0.1532563361054082862, 21.21726448433412315, 2.638427012816831674 ) ) ;
#93828 = CARTESIAN_POINT ( 'NONE',  ( 17.20831665107776587, 47.88393115100078745, 7.208316651077764980 ) ) ;
#93829 = AXIS2_PLACEMENT_3D ( 'NONE', #8339, #15370, #16827 ) ;
#93830 = CARTESIAN_POINT ( 'NONE',  ( 0.5774900079438607392, 13.48035201082150358, 5.440088680355550821 ) ) ;
#93831 = VECTOR ( 'NONE', #2188, 1000.000000000000114 ) ;
#93832 = AXIS2_PLACEMENT_3D ( 'NONE', #24012, #98557, #84509 ) ;
#93833 = CARTESIAN_POINT ( 'NONE',  ( 19.38216949554541202, 25.99863466993042138, 9.382169495545424454 ) ) ;
#93834 = CARTESIAN_POINT ( 'NONE',  ( 20.88017736071110875, 55.77201867748816966, -2.915334737309920765 ) ) ;
#93835 = CARTESIAN_POINT ( 'NONE',  ( 0.1532563361054100626, 30.80059781766744820, -2.638427012816831230 ) ) ;
#93837 = CARTESIAN_POINT ( 'NONE',  ( 18.52753015748617571, 28.09226448433411960, 4.923371831947298993 ) ) ;
#93836 = CARTESIAN_POINT ( 'NONE',  ( 10.00000000000000000, 50.55374883491396787, -14.16423886937410082 ) ) ;
#93838 = LINE ( 'NONE', #32831, #79150 ) ;
#93839 = CARTESIAN_POINT ( 'NONE',  ( 19.84674366389459266, 48.71726448433413026, -2.638427012816827677 ) ) ;
#93841 = CARTESIAN_POINT ( 'NONE',  ( 6.204703633549690345, 15.76208216824730179, -14.16423886937410259 ) ) ;
#93840 = CARTESIAN_POINT ( 'NONE',  ( 2.791683348922237240, 35.38393115100079456, -7.208316651077763204 ) ) ;
#93842 = CARTESIAN_POINT ( 'NONE',  ( -4.164238869374099039, 16.80374883491396787, 8.674139862899312516E-16 ) ) ;
#93843 = CARTESIAN_POINT ( 'NONE',  ( 2.791683348922240793, 36.63393115100078035, 7.208316651077764092 ) ) ;
#93844 = CARTESIAN_POINT ( 'NONE',  ( 17.96484262340118221, 49.93868534415484106, 7.964842623401181321 ) ) ;
#93845 = CARTESIAN_POINT ( 'NONE',  ( -0.8801773607111009756, 28.06368534415484106, 1.068504757029289695E-15 ) ) ;
#93846 = EDGE_CURVE ( 'NONE', #67150, #41155, #9854, .T. ) ;
#93847 = CARTESIAN_POINT ( 'NONE',  ( -0.8801773607110991993, 47.85535201082150536, -2.915334737309923874 ) ) ;
#93848 = CARTESIAN_POINT ( 'NONE',  ( 0.5774900079438590739, 32.64701867748816966, -5.440088680355550821 ) ) ;
#93849 = ORIENTED_EDGE ( 'NONE', *, *, #12536, .T. ) ;
#93850 = CARTESIAN_POINT ( 'NONE',  ( 19.42250999205614193, 50.14701867748817676, 5.440088680355555262 ) ) ;
#93851 = VERTEX_POINT ( 'NONE', #46448 ) ;
#93852 = CARTESIAN_POINT ( 'NONE',  ( 6.565887622018943937, 60.16530133659707502, 12.81628187352647430 ) ) ;
#93853 = CARTESIAN_POINT ( 'NONE',  ( 15.44008868035555260, 59.73035201082151247, 9.422509992056143702 ) ) ;
#93854 = VERTEX_POINT ( 'NONE', #45965 ) ;
#93855 = CARTESIAN_POINT ( 'NONE',  ( -7.750000000000000000, 43.00000000000000000, -6.500000000000000888 ) ) ;
#93856 = CARTESIAN_POINT ( 'NONE',  ( 10.00000000000000000, 1.813685344154837731, -10.88017736071110342 ) ) ;
#93857 = CARTESIAN_POINT ( 'NONE',  ( -5.149999999999996803, 98.49999999999998579, 8.000000000000000000 ) ) ;
#93858 = DIRECTION ( 'NONE',  ( 0.000000000000000000, 0.000000000000000000, 1.000000000000000000 ) ) ;
#93859 = CARTESIAN_POINT ( 'NONE',  ( 17.08211943468705840, 55.13708216824731068, -12.26659068614894466 ) ) ;
#93860 = CARTESIAN_POINT ( 'NONE',  ( 19.84674366389459266, 8.717264484334116048, -2.638427012816827677 ) ) ;
#93861 = CARTESIAN_POINT ( 'NONE',  ( -0.3689425029237881626, 7.428748834913967869, 10.36894250292379027 ) ) ;
#93862 = CARTESIAN_POINT ( 'NONE',  ( 19.84674366389459621, 8.508931151000785675, 7.409399052514197653E-17 ) ) ;
#93863 = CARTESIAN_POINT ( 'NONE',  ( 12.91533473730993009, 11.60535201082150536, -10.88017736071109987 ) ) ;
#93864 = CARTESIAN_POINT ( 'NONE',  ( 7.361572987183170547, 47.05059781766745175, 9.846743663894590881 ) ) ;
#93865 = ORIENTED_EDGE ( 'NONE', *, *, #46328, .F. ) ;
#93866 = CARTESIAN_POINT ( 'NONE',  ( 17.20831665107776587, 52.88393115100078035, 7.208316651077764980 ) ) ;
#93867 = ORIENTED_EDGE ( 'NONE', *, *, #30963, .T. ) ;
#93868 = FACE_OUTER_BOUND ( 'NONE', #25762, .T. ) ;
#93869 = CARTESIAN_POINT ( 'NONE',  ( 20.88017736071110875, 40.77201867748818387, -2.915334737309920765 ) ) ;
#93870 = CARTESIAN_POINT ( 'NONE',  ( 14.92337183194729633, 47.67559781766745175, 8.527530157486181039 ) ) ;
#93871 = CARTESIAN_POINT ( 'NONE',  ( 21.09922568453594849, 31.20696800326375353, 6.408140936763242479 ) ) ;
#93873 = CARTESIAN_POINT ( 'NONE',  ( 19.88701968852526392, 1.794273331840863683, 6.480634945678604986 ) ) ;
#93872 = PRESENTATION_STYLE_ASSIGNMENT (( #86381 ) ) ;
#93874 = CARTESIAN_POINT ( 'NONE',  ( 15.44008868035555793, 56.39701867748817676, -9.422509992056140149 ) ) ;
#93875 = CARTESIAN_POINT ( 'NONE',  ( 12.91533473730992121, 9.522018677488171434, 10.88017736071110164 ) ) ;
#93876 = EDGE_CURVE ( 'NONE', #69049, #55236, #8448, .T. ) ;
#93877 = CARTESIAN_POINT ( 'NONE',  ( 10.00000000000000000, 47.87363466993042493, -12.81628187352647608 ) ) ;
#93878 = DIRECTION ( 'NONE',  ( 1.000000000000000000, 0.000000000000000000, 0.000000000000000000 ) ) ;
#93879 = ORIENTED_EDGE ( 'NONE', *, *, #88542, .T. ) ;
#93880 = CARTESIAN_POINT ( 'NONE',  ( -2.816281873526471635, 28.91530133659708213, -3.434112377981056508 ) ) ;
#93881 = CARTESIAN_POINT ( 'NONE',  ( -0.8801773607110991993, 27.85535201082150181, -2.915334737309923874 ) ) ;
#93882 = ORIENTED_EDGE ( 'NONE', *, *, #71711, .T. ) ;
#93883 = DIRECTION ( 'NONE',  ( -0.8616291604415338146, -0.000000000000000000, 0.5075383629606904368 ) ) ;
#93884 = VECTOR ( 'NONE', #51100, 1000.000000000000000 ) ;
#93885 = CARTESIAN_POINT ( 'NONE',  ( 1.472469842513823179, 0.5922644843341181575, -4.923371831947296329 ) ) ;
#93886 = CARTESIAN_POINT ( 'NONE',  ( 10.00000000000000178, 52.25893115100078745, 9.846743663894594434 ) ) ;
#93888 = CARTESIAN_POINT ( 'NONE',  ( 18.52753015748617571, 33.09226448433411605, 4.923371831947298993 ) ) ;
#93887 = CARTESIAN_POINT ( 'NONE',  ( 10.00000000000000178, 12.25893115100078568, 9.846743663894594434 ) ) ;
#93889 = CARTESIAN_POINT ( 'NONE',  ( -11.62550287597698784, -75.79306049738043782, 3.750000000000000444 ) ) ;
#93890 = CARTESIAN_POINT ( 'NONE',  ( -1.881645754503963541, -3.304699043712651590E-15, 14.50406564081095162 ) ) ;
#93891 = CARTESIAN_POINT ( 'NONE',  ( 5.076628168052704559, 25.17559781766745175, -8.527530157486179263 ) ) ;
#93892 = DIRECTION ( 'NONE',  ( 0.9942165912674658657, -0.1073935270325955399, 0.000000000000000000 ) ) ;
#93893 = LINE ( 'NONE', #25420, #32484 ) ;
#93896 = FILL_AREA_STYLE ('',( #40909 ) ) ;
#93895 = VECTOR ( 'NONE', #69602, 1000.000000000000000 ) ;
#93894 = CARTESIAN_POINT ( 'NONE',  ( 2.791683348922237240, 30.38393115100078390, -7.208316651077763204 ) ) ;
#93897 = DIRECTION ( 'NONE',  ( -0.000000000000000000, -0.000000000000000000, -1.000000000000000000 ) ) ;
#93899 = ORIENTED_EDGE ( 'NONE', *, *, #4880, .T. ) ;
#93898 = CARTESIAN_POINT ( 'NONE',  ( 14.92337183194729633, 52.67559781766745175, 8.527530157486181039 ) ) ;
#93900 = CIRCLE ( 'NONE', #55584, 15.00000000000000000 ) ;
#93901 = SURFACE_STYLE_USAGE ( .BOTH. , #10899 ) ;
#93902 = CARTESIAN_POINT ( 'NONE',  ( 3.591859063236763294, 28.29030133659708568, -11.09922568453595026 ) ) ;
#93903 = CARTESIAN_POINT ( 'NONE',  ( 19.84674366389459621, 38.50893115100078745, 7.409399052514197653E-17 ) ) ;
#93904 = CARTESIAN_POINT ( 'NONE',  ( -0.1042174387088646015, 8.107361737662019507, 6.337391062633415117 ) ) ;
#93905 = CARTESIAN_POINT ( 'NONE',  ( 2.917880565312948704, 42.63708216824729647, 12.26659068614894643 ) ) ;
#93906 = CARTESIAN_POINT ( 'NONE',  ( 19.84674366389459266, 18.30059781766745175, 2.638427012816836559 ) ) ;
#93907 = CARTESIAN_POINT ( 'NONE',  ( 0.1532563361054082862, 1.217264484334117824, 2.638427012816831674 ) ) ;
#93908 = CARTESIAN_POINT ( 'NONE',  ( 20.00000000000000711, 90.60976979464389558, 4.970182471799130752 ) ) ;
#93909 = CARTESIAN_POINT ( 'NONE',  ( 17.08211943468705840, 50.13708216824730357, -12.26659068614894466 ) ) ;
#93910 = CARTESIAN_POINT ( 'NONE',  ( 0.1532563361054100626, 55.80059781766745175, -2.638427012816831230 ) ) ;
#93911 = CARTESIAN_POINT ( 'NONE',  ( 0.5774900079438590739, 12.64701867748817321, -5.440088680355550821 ) ) ;
#93912 = CARTESIAN_POINT ( 'NONE',  ( 17.08211943468705840, 25.13708216824730357, -12.26659068614894466 ) ) ;
#93913 = CARTESIAN_POINT ( 'NONE',  ( 22.26659068614894466, 33.88708216824730357, 7.082119434687054849 ) ) ;
#93914 = CARTESIAN_POINT ( 'NONE',  ( -9.898881779040587858, -0.03417435944610275333, -10.25059215482589714 ) ) ;
#93915 = EDGE_CURVE ( 'NONE', #86159, #48470, #76939, .T. ) ;
#93917 = CARTESIAN_POINT ( 'NONE',  ( 14.92337183194729633, 52.67559781766745175, 8.527530157486181039 ) ) ;
#93916 = CARTESIAN_POINT ( 'NONE',  ( 4.191189844333585768, -2.692444605319266326, 2.500000000000000000 ) ) ;
#93918 = B_SPLINE_CURVE_WITH_KNOTS ( 'NONE', 3,
 ( #88598, #20109, #50612, #94138, #4141, #11135 ),
 .UNSPECIFIED., .F., .F.,
 ( 4, 2, 4 ),
 ( 0.0002800484630363999933, 0.0006862541666483234701, 0.001092459870260246947 ),
 .UNSPECIFIED. ) ;
#93919 = ORIENTED_EDGE ( 'NONE', *, *, #46382, .F. ) ;
#93920 = CARTESIAN_POINT ( 'NONE',  ( -0.8801773607110991993, 32.85535201082151247, -2.915334737309923874 ) ) ;
#93921 = DIRECTION ( 'NONE',  ( -0.000000000000000000, -1.000000000000000000, -0.000000000000000000 ) ) ;
#93922 = CYLINDRICAL_SURFACE ( 'NONE', #44893, 15.00000000000000000 ) ;
#93923 = CARTESIAN_POINT ( 'NONE',  ( 14.92337183194729988, 44.34226448433412315, -8.527530157486177487 ) ) ;
#93924 = LINE ( 'NONE', #25450, #52217 ) ;
#93925 = CARTESIAN_POINT ( 'NONE',  ( 12.26659068614894821, 8.887082168247301794, 7.082119434687044190 ) ) ;
#93926 = CARTESIAN_POINT ( 'NONE',  ( 7.361572987183169658, 49.96726448433410894, -9.846743663894592657 ) ) ;
#93927 = CARTESIAN_POINT ( 'NONE',  ( 6.880000000000009663, 40.99999999999999289, 4.250000000000000000 ) ) ;
#93928 = ADVANCED_FACE ( 'NONE', ( #2455 ), #26568, .F. ) ;
#93929 = ORIENTED_EDGE ( 'NONE', *, *, #89464, .F. ) ;
#93930 = CARTESIAN_POINT ( 'NONE',  ( -2.266590686148945544, 27.22041550158063572, 7.082119434687048631 ) ) ;
#93931 = EDGE_CURVE ( 'NONE', #12953, #48484, #38552, .T. ) ;
#93932 = EDGE_CURVE ( 'NONE', #97330, #9538, #30877, .T. ) ;
#93933 = CARTESIAN_POINT ( 'NONE',  ( -6.382347221874242749, 0.5000000000000004441, -13.57444820018235987 ) ) ;
#93934 = CARTESIAN_POINT ( 'NONE',  ( -3.521809513897767641, -0.8352226969158469405, -2.749999999999595879 ) ) ;
#93935 = CARTESIAN_POINT ( 'NONE',  ( 10.00000000000000178, 9.313685344154839285, 10.88017736071110342 ) ) ;
#93936 = CARTESIAN_POINT ( 'NONE',  ( 13.43411237798105340, 30.58196800326374998, 12.81628187352647963 ) ) ;
#93937 = CARTESIAN_POINT ( 'NONE',  ( -19.64999999999999858, 98.99999999999998579, -8.000000000000000000 ) ) ;
#93938 = CARTESIAN_POINT ( 'NONE',  ( 0.5774900079438590739, 67.64701867748817676, -5.440088680355550821 ) ) ;
#93939 = CARTESIAN_POINT ( 'NONE',  ( 20.24186590665277308, 42.61633188102327807, -6.114288769123051637 ) ) ;
#93940 = CARTESIAN_POINT ( 'NONE',  ( -15.00000000000000000, 83.99999999999998579, 3.750000000000000000 ) ) ;
#93941 = CARTESIAN_POINT ( 'NONE',  ( 12.91533473730992121, 14.52201867748817143, 10.88017736071110164 ) ) ;
#93942 = CARTESIAN_POINT ( 'NONE',  ( 0.6081133539230610952, 3.337033823263999111, 6.500000000000004441 ) ) ;
#93943 =( BOUNDED_SURFACE ( )  B_SPLINE_SURFACE ( 1, 2, ( 
 ( #18330, #9848, #63317, #6772, #96305, #20293, #67273, #66775, #5303, #67773, #59759, #21281, #42800, #51280, #59263, #51777, #36278, #37283, #29263, #57784, #13277, #50791, #89764, #28769, #97296, #74768, #27782, #90253, #20790, #81764, #82259, #19790, #98294, #28280, #13776, #43768, #58775, #4807, #74258, #75259, #35780, #12781, #21786, #82762, #58267, #5787, #89278, #88291, #50279, #88783, #36782, #73284, #81282, #43279, #73774, #52266, #44262, #6276, #97801, #96804, #14284, #44757, #66269, #80795, #12291, #35281, #65775, #24853, #33310, #78327, #85844, #33787, #25833, #84857, #93825, #1382, #70851, #9847, #55336, #17358, #92840, #78827, #40835, #62333, #40348, #16364, #71336, #71817, #55838, #10337, #46845, #86333, #31836, #47826, #1872, #2364, #24369, #77832, #56331, #54831, #85344, #63804, #2856, #32328, #32818, #16856, #3323, #63316, #17837, #64293, #25355, #77340, #48319, #70353, #79318, #23880, #94309, #47331, #86824, #9344, #39848, #62833, #54344, #93333, #18329, #48810, #10827, #41347, #8852, #39366, #69861, #94805, #87303, #18823, #49303, #26306, #56807, #25217, #23247, #47189, #54203, #24713, #55185, #1729, #9701, #84719, #55698, #54690, #16716, #47696, #53721, #2718, #62189, #70210, #85211, #39227, #10200, #77692, #70705, #48177, #84238, #71195, #33172, #46229, #76715, #38728, #69228, #753, #16223, #69715, #92699, #1242, #78188, #31698, #24223, #40197, #97533, #90000, #64151, #57154, #34146, #6503, #63665, #3190, #43999, #48670, #56670, #94670, #33656, #28992, #87652, #4173, #64640, #3685, #21517, #34642, #26179, #19165, #82502, #25701, #44500, #95149, #74501, #49644, #26659, #75001, #67012, #56191, #65139, #41200, #11663, #80151, #42176, #72640, #87159, #21025, #82006, #18683, #95660, #86685, #13518, #14020, #27145, #51514, #18189, #57647, #71680, #88143, #41687, #6024, #49169, #79671, #59503, #11168, #72157, #36520, #52013, #94170, #79171, #10686, #16483, #27, #68989, #77452, #60975, #29482, #38494, #83498, #92459, #84966, #15511, #7007, #46472, #60489, #37513, #68005, #46958, #75496, #98531, #76968, #45993, #15016, #37011, #38986, #525, #22020, #30474, #30971, #61468, #76482, #67508, #8481, #98027, #91488, #29984, #91975, #7996, #23504, #53975, #90978, #69479, #23008, #53476, #84484, #59990, #90483, #7516, #15985, #83986, #22511, #23987, #997, #52494, #83001, #52983, #31458, #45485, #54458, #61960, #75987, #38007, #14519, #44988, #68500, #33419, #47939, #63918, #94921, #25944, #87423, #17953, #85963, #25473, #56446, #70463, #17472, #40467, #32938, #86932, #86455, #93450, #10937, #33907, #1491, #78940 ),
 ( #78445, #48440, #2485, #24975, #26420, #63439, #18445, #3450, #31944, #56921, #64415, #79439, #9960, #54946, #93946, #18940, #55460, #62947, #41461, #49417, #9461, #55955, #70965, #8966, #39482, #47455, #48927, #92948, #1985, #39962, #77954, #71929, #10450, #40958, #71455, #2969, #69972, #94429, #32451, #62445, #24483, #85463, #16975, #80914, #89395, #35402, #42915, #89885, #81887, #41947, #50903, #57416, #27899, #65895, #12408, #73396, #49915, #35896, #96924, #19423, #96426, #72411, #28402, #28879, #12900, #66391, #3937, #43397, #87909, #4924, #57899, #58388, #80426, #34906, #13399, #11922, #42426, #20911, #58897, #88413, #88906, #72907, #59381, #20417, #73895, #4440, #43882, #5426, #74378, #97412, #21403, #81398, #51400, #79918, #5905, #65402, #36400, #95928, #34406, #26919, #27408, #66893, #64895, #11427, #95423, #19913, #50404, #6889, #90867, #67890, #76852, #82884, #22397, #52380, #83379, #31346, #21903, #75876, #52873, #91867, #6383, #98412, #45881, #90366, #30358, #82379, #76371, #409, #46364, #14400, #29868, #8366, #53870, #44871, #22892, #7397, #59877, #60370, #69365, #61847, #14901, #45372, #23385, #84380, #75374, #61358, #44386, #74885, #37402, #30861, #37895, #886, #38874, #68387, #98907, #60866, #91366, #15880, #7886, #53364, #38378, #92353, #68879, #51897, #83871, #15395, #13901, #36899, #67387, #97916, #29376, #76166, #69167, #66461, #97980, #83935, #7950, #74448, #52935, #37466, #21971, #14967, #67955, #7463, #29933, #61418, #5975, #82952, #22962, #29436, #90431, #74951, #38445, #68452, #14465, #36468, #82451, #13974, #472, #44450, #6454, #59941, #98974, #89950, #59449, #44940, #98478, #30427, #60438, #90931, #22459, #60929, #91435, #53427, #15463, #45944, #76434, #30919, #91928, #23454, #13468, #97481, #28947, #19208, #183, #21684, #37670, #52169, #44159, #6179, #75157, #76150, #74669, #90648, #68170, #98689, #30631, #6668, #29644, #37187, #84162, #60151, #22174, #52655, #83158, #69152, #14682, #30138, #60646, #61140, #67171, #91145, #53150, #97695, #22671, #89672, #15173, #91648, #53644, #23166, #15667, #46152, #76636, #8155, #677, #51684, #73062, #42712, #51697, #13690, #80710, #73194, #5706, #36194, #27202, #43687, #26714, #57210, #72696, #13193, #35190, #82179, #59179, #12205, #96217, #88694, #12700, #81678, #89193, #20202, #20704, #21199, #51197, #44174, #43195, #50706, #81199, #66692, #95717, #73682, #5218, #28194, #97219, #28686, #19712, #34206, #64696, #19222, #95208, #49703, #11717, #42230, #57702, #88202, #50199, #71403, #84436, #92900, #32887, #39428, #1442, #84917, #48385, #62897, #31894 ) ),
 .UNSPECIFIED., .F., .F., .F. ) 
 B_SPLINE_SURFACE_WITH_KNOTS ( ( 2, 2 ),
 ( 3, 2, 2, 2, 2, 2, 2, 2, 2, 2, 2, 2, 2, 2, 2, 2, 2, 2, 2, 2, 2, 2, 2, 2, 2, 2, 2, 2, 2, 2, 2, 2, 2, 2, 2, 2, 2, 2, 2, 2, 2, 2, 2, 2, 2, 2, 2, 2, 2, 2, 2, 2, 2, 2, 2, 2, 2, 2, 2, 2, 2, 2, 2, 2, 2, 2, 2, 2, 2, 2, 2, 2, 2, 2, 2, 2, 2, 2, 2, 2, 2, 2, 2, 2, 2, 2, 2, 2, 2, 2, 2, 2, 2, 2, 2, 2, 2, 2, 2, 2, 2, 2, 2, 2, 2, 2, 2, 2, 2, 2, 2, 2, 2, 2, 2, 2, 2, 2, 2, 2, 2, 2, 2, 2, 2, 2, 2, 2, 2, 2, 2, 2, 2, 2, 2, 2, 2, 2, 2, 2, 2, 2, 2, 2, 2, 2, 2, 2, 2, 2, 2, 2, 2, 2, 2, 2, 2, 2, 2, 2, 2, 2, 3 ),
 ( 0.000000000000000000, 1.000000000000000000 ),
 ( 0.000000000000000000, 0.005952380952380952051, 0.01190476190476190410, 0.01785714285714285615, 0.02380952380952380820, 0.02976190476190476025, 0.03571428571428571230, 0.04166666666666666435, 0.04761904761904761640, 0.05357142857142856845, 0.05952380952380952051, 0.06547619047619047949, 0.07142857142857142461, 0.07738095238095238360, 0.08333333333333332871, 0.08928571428571428770, 0.09523809523809523281, 0.1011904761904761918, 0.1071428571428571369, 0.1130952380952380959, 0.1190476190476190410, 0.1250000000000000000, 0.1309523809523809590, 0.1369047619047619180, 0.1428571428571428492, 0.1488095238095238082, 0.1547619047619047672, 0.1607142857142857262, 0.1666666666666666574, 0.1726190476190476164, 0.1785714285714285754, 0.1845238095238095344, 0.1904761904761904656, 0.1964285714285714246, 0.2023809523809523836, 0.2083333333333333426, 0.2142857142857142738, 0.2202380952380952328, 0.2261904761904761918, 0.2321428571428571508, 0.2380952380952380820, 0.2440476190476190410, 0.2500000000000000000, 0.2559523809523809312, 0.2619047619047619180, 0.2678571428571428492, 0.2738095238095238360, 0.2797619047619047672, 0.2857142857142856984, 0.2916666666666666852, 0.2976190476190476164, 0.3035714285714285476, 0.3095238095238095344, 0.3154761904761904656, 0.3214285714285714524, 0.3273809523809523836, 0.3333333333333333148, 0.3392857142857143016, 0.3452380952380952328, 0.3511904761904761640, 0.3571428571428571508, 0.3630952380952380820, 0.3690476190476190688, 0.3750000000000000000, 0.3809523809523809312, 0.3869047619047619180, 0.3928571428571428492, 0.3988095238095238360, 0.4047619047619047672, 0.4107142857142856984, 0.4166666666666666852, 0.4226190476190476164, 0.4285714285714285476, 0.4345238095238095344, 0.4404761904761904656, 0.4464285714285714524, 0.4523809523809523836, 0.4583333333333333148, 0.4642857142857143016, 0.4702380952380952328, 0.4761904761904761640, 0.4821428571428571508, 0.4880952380952380820, 0.4940476190476190688, 0.5000000000000000000, 0.5059523809523809312, 0.5119047619047618625, 0.5178571428571429047, 0.5238095238095238360, 0.5297619047619047672, 0.5357142857142856984, 0.5416666666666666297, 0.5476190476190476719, 0.5535714285714286031, 0.5595238095238095344, 0.5654761904761904656, 0.5714285714285713969, 0.5773809523809523281, 0.5833333333333333703, 0.5892857142857143016, 0.5952380952380952328, 0.6011904761904761640, 0.6071428571428570953, 0.6130952380952381375, 0.6190476190476190688, 0.6250000000000000000, 0.6309523809523809312, 0.6369047619047618625, 0.6428571428571429047, 0.6488095238095238360, 0.6547619047619047672, 0.6607142857142856984, 0.6666666666666666297, 0.6726190476190476719, 0.6785714285714286031, 0.6845238095238095344, 0.6904761904761904656, 0.6964285714285713969, 0.7023809523809523281, 0.7083333333333333703, 0.7142857142857143016, 0.7202380952380952328, 0.7261904761904761640, 0.7321428571428570953, 0.7380952380952381375, 0.7440476190476190688, 0.7500000000000000000, 0.7559523809523809312, 0.7619047619047618625, 0.7678571428571429047, 0.7738095238095238360, 0.7797619047619047672, 0.7857142857142856984, 0.7916666666666666297, 0.7976190476190476719, 0.8035714285714286031, 0.8095238095238095344, 0.8154761904761904656, 0.8214285714285713969, 0.8273809523809523281, 0.8333333333333333703, 0.8392857142857143016, 0.8452380952380952328, 0.8511904761904761640, 0.8571428571428570953, 0.8630952380952381375, 0.8690476190476190688, 0.8750000000000000000, 0.8809523809523809312, 0.8869047619047618625, 0.8928571428571429047, 0.8988095238095238360, 0.9047619047619047672, 0.9107142857142856984, 0.9166666666666666297, 0.9226190476190476719, 0.9285714285714286031, 0.9345238095238095344, 0.9404761904761904656, 0.9464285714285713969, 0.9523809523809523281, 0.9583333333333333703, 0.9642857142857143016 ),
 .UNSPECIFIED. ) 
 GEOMETRIC_REPRESENTATION_ITEM ( )  RATIONAL_B_SPLINE_SURFACE ( (
 ( 1.000000000000000000, 0.9659258262890683122, 1.000000000000000000, 0.9659258262890683122, 1.000000000000000000, 0.9659258262890683122, 1.000000000000000000, 0.9659258262890683122, 1.000000000000000000, 0.9659258262890683122, 1.000000000000000000, 0.9659258262890683122, 1.000000000000000000, 0.9659258262890683122, 1.000000000000000000, 0.9659258262890683122, 1.000000000000000000, 0.9659258262890683122, 1.000000000000000000, 0.9659258262890683122, 1.000000000000000000, 0.9659258262890683122, 1.000000000000000000, 0.9659258262890683122, 1.000000000000000000, 0.9659258262890683122, 1.000000000000000000, 0.9659258262890683122, 1.000000000000000000, 0.9659258262890683122, 1.000000000000000000, 0.9659258262890683122, 1.000000000000000000, 0.9659258262890683122, 1.000000000000000000, 0.9659258262890683122, 1.000000000000000000, 0.9659258262890683122, 1.000000000000000000, 0.9659258262890683122, 1.000000000000000000, 0.9659258262890683122, 1.000000000000000000, 0.9659258262890683122, 1.000000000000000000, 0.9659258262890683122, 1.000000000000000000, 0.9659258262890683122, 1.000000000000000000, 0.9659258262890683122, 1.000000000000000000, 0.9659258262890683122, 1.000000000000000000, 0.9659258262890683122, 1.000000000000000000, 0.9659258262890683122, 1.000000000000000000, 0.9659258262890683122, 1.000000000000000000, 0.9659258262890683122, 1.000000000000000000, 0.9659258262890683122, 1.000000000000000000, 0.9659258262890683122, 1.000000000000000000, 0.9659258262890683122, 1.000000000000000000, 0.9659258262890683122, 1.000000000000000000, 0.9659258262890683122, 1.000000000000000000, 0.9659258262890683122, 1.000000000000000000, 0.9659258262890683122, 1.000000000000000000, 0.9659258262890683122, 1.000000000000000000, 0.9659258262890683122, 1.000000000000000000, 0.9659258262890683122, 1.000000000000000000, 0.9659258262890683122, 1.000000000000000000, 0.9659258262890683122, 1.000000000000000000, 0.9659258262890683122, 1.000000000000000000, 0.9659258262890683122, 1.000000000000000000, 0.9659258262890683122, 1.000000000000000000, 0.9659258262890683122, 1.000000000000000000, 0.9659258262890683122, 1.000000000000000000, 0.9659258262890683122, 1.000000000000000000, 0.9659258262890683122, 1.000000000000000000, 0.9659258262890683122, 1.000000000000000000, 0.9659258262890683122, 1.000000000000000000, 0.9659258262890683122, 1.000000000000000000, 0.9659258262890683122, 1.000000000000000000, 0.9659258262890683122, 1.000000000000000000, 0.9659258262890683122, 1.000000000000000000, 0.9659258262890683122, 1.000000000000000000, 0.9659258262890683122, 1.000000000000000000, 0.9659258262890683122, 1.000000000000000000, 0.9659258262890683122, 1.000000000000000000, 0.9659258262890683122, 1.000000000000000000, 0.9659258262890683122, 1.000000000000000000, 0.9659258262890683122, 1.000000000000000000, 0.9659258262890683122, 1.000000000000000000, 0.9659258262890683122, 1.000000000000000000, 0.9659258262890683122, 1.000000000000000000, 0.9659258262890683122, 1.000000000000000000, 0.9659258262890683122, 1.000000000000000000, 0.9659258262890683122, 1.000000000000000000, 0.9659258262890683122, 1.000000000000000000, 0.9659258262890683122, 1.000000000000000000, 0.9659258262890683122, 1.000000000000000000, 0.9659258262890683122, 1.000000000000000000, 0.9659258262890683122, 1.000000000000000000, 0.9659258262890683122, 1.000000000000000000, 0.9659258262890683122, 1.000000000000000000, 0.9659258262890683122, 1.000000000000000000, 0.9659258262890683122, 1.000000000000000000, 0.9659258262890683122, 1.000000000000000000, 0.9659258262890683122, 1.000000000000000000, 0.9659258262890683122, 1.000000000000000000, 0.9659258262890683122, 1.000000000000000000, 0.9659258262890683122, 1.000000000000000000, 0.9659258262890683122, 1.000000000000000000, 0.9659258262890683122, 1.000000000000000000, 0.9659258262890683122, 1.000000000000000000, 0.9659258262890683122, 1.000000000000000000, 0.9659258262890683122, 1.000000000000000000, 0.9659258262890683122, 1.000000000000000000, 0.9659258262890683122, 1.000000000000000000, 0.9659258262890683122, 1.000000000000000000, 0.9659258262890683122, 1.000000000000000000, 0.9659258262890683122, 1.000000000000000000, 0.9659258262890683122, 1.000000000000000000, 0.9659258262890683122, 1.000000000000000000, 0.9659258262890683122, 1.000000000000000000, 0.9659258262890683122, 1.000000000000000000, 0.9659258262890683122, 1.000000000000000000, 0.9659258262890683122, 1.000000000000000000, 0.9659258262890683122, 1.000000000000000000, 0.9659258262890683122, 1.000000000000000000, 0.9659258262890683122, 1.000000000000000000, 0.9659258262890683122, 1.000000000000000000, 0.9659258262890683122, 1.000000000000000000, 0.9659258262890683122, 1.000000000000000000, 0.9659258262890683122, 1.000000000000000000, 0.9659258262890683122, 1.000000000000000000, 0.9659258262890683122, 1.000000000000000000, 0.9659258262890683122, 1.000000000000000000, 0.9659258262890683122, 1.000000000000000000, 0.9659258262890683122, 1.000000000000000000, 0.9659258262890683122, 1.000000000000000000, 0.9659258262890683122, 1.000000000000000000, 0.9659258262890683122, 1.000000000000000000, 0.9659258262890683122, 1.000000000000000000, 0.9659258262890683122, 1.000000000000000000, 0.9659258262890683122, 1.000000000000000000, 0.9659258262890683122, 1.000000000000000000, 0.9659258262890683122, 1.000000000000000000, 0.9659258262890683122, 1.000000000000000000, 0.9659258262890683122, 1.000000000000000000, 0.9659258262890683122, 1.000000000000000000, 0.9659258262890683122, 1.000000000000000000, 0.9659258262890683122, 1.000000000000000000, 0.9659258262890683122, 1.000000000000000000, 0.9659258262890683122, 1.000000000000000000, 0.9659258262890683122, 1.000000000000000000, 0.9659258262890683122, 1.000000000000000000, 0.9659258262890683122, 1.000000000000000000, 0.9659258262890683122, 1.000000000000000000, 0.9659258262890683122, 1.000000000000000000, 0.9659258262890683122, 1.000000000000000000, 0.9659258262890683122, 1.000000000000000000, 0.9659258262890683122, 1.000000000000000000, 0.9659258262890683122, 1.000000000000000000, 0.9659258262890683122, 1.000000000000000000, 0.9659258262890683122, 1.000000000000000000, 0.9659258262890683122, 1.000000000000000000, 0.9659258262890683122, 1.000000000000000000, 0.9659258262890683122, 1.000000000000000000, 0.9659258262890683122, 1.000000000000000000, 0.9659258262890683122, 1.000000000000000000, 0.9659258262890683122, 1.000000000000000000, 0.9659258262890683122, 1.000000000000000000, 0.9659258262890683122, 1.000000000000000000, 0.9659258262890683122, 1.000000000000000000, 0.9659258262890683122, 1.000000000000000000, 0.9659258262890683122, 1.000000000000000000, 0.9659258262890683122, 1.000000000000000000, 0.9659258262890683122, 1.000000000000000000, 0.9659258262890683122, 1.000000000000000000, 0.9659258262890683122, 1.000000000000000000, 0.9659258262890683122, 1.000000000000000000, 0.9659258262890683122, 1.000000000000000000, 0.9659258262890683122, 1.000000000000000000, 0.9659258262890683122, 1.000000000000000000, 0.9659258262890683122, 1.000000000000000000, 0.9659258262890683122, 1.000000000000000000, 0.9659258262890683122, 1.000000000000000000, 0.9659258262890683122, 1.000000000000000000, 0.9659258262890683122, 1.000000000000000000, 0.9659258262890683122, 1.000000000000000000, 0.9659258262890683122, 1.000000000000000000),
 ( 1.000000000000000000, 0.9659258262890683122, 1.000000000000000000, 0.9659258262890683122, 1.000000000000000000, 0.9659258262890683122, 1.000000000000000000, 0.9659258262890683122, 1.000000000000000000, 0.9659258262890683122, 1.000000000000000000, 0.9659258262890683122, 1.000000000000000000, 0.9659258262890683122, 1.000000000000000000, 0.9659258262890683122, 1.000000000000000000, 0.9659258262890683122, 1.000000000000000000, 0.9659258262890683122, 1.000000000000000000, 0.9659258262890683122, 1.000000000000000000, 0.9659258262890683122, 1.000000000000000000, 0.9659258262890683122, 1.000000000000000000, 0.9659258262890683122, 1.000000000000000000, 0.9659258262890683122, 1.000000000000000000, 0.9659258262890683122, 1.000000000000000000, 0.9659258262890683122, 1.000000000000000000, 0.9659258262890683122, 1.000000000000000000, 0.9659258262890683122, 1.000000000000000000, 0.9659258262890683122, 1.000000000000000000, 0.9659258262890683122, 1.000000000000000000, 0.9659258262890683122, 1.000000000000000000, 0.9659258262890683122, 1.000000000000000000, 0.9659258262890683122, 1.000000000000000000, 0.9659258262890683122, 1.000000000000000000, 0.9659258262890683122, 1.000000000000000000, 0.9659258262890683122, 1.000000000000000000, 0.9659258262890683122, 1.000000000000000000, 0.9659258262890683122, 1.000000000000000000, 0.9659258262890683122, 1.000000000000000000, 0.9659258262890683122, 1.000000000000000000, 0.9659258262890683122, 1.000000000000000000, 0.9659258262890683122, 1.000000000000000000, 0.9659258262890683122, 1.000000000000000000, 0.9659258262890683122, 1.000000000000000000, 0.9659258262890683122, 1.000000000000000000, 0.9659258262890683122, 1.000000000000000000, 0.9659258262890683122, 1.000000000000000000, 0.9659258262890683122, 1.000000000000000000, 0.9659258262890683122, 1.000000000000000000, 0.9659258262890683122, 1.000000000000000000, 0.9659258262890683122, 1.000000000000000000, 0.9659258262890683122, 1.000000000000000000, 0.9659258262890683122, 1.000000000000000000, 0.9659258262890683122, 1.000000000000000000, 0.9659258262890683122, 1.000000000000000000, 0.9659258262890683122, 1.000000000000000000, 0.9659258262890683122, 1.000000000000000000, 0.9659258262890683122, 1.000000000000000000, 0.9659258262890683122, 1.000000000000000000, 0.9659258262890683122, 1.000000000000000000, 0.9659258262890683122, 1.000000000000000000, 0.9659258262890683122, 1.000000000000000000, 0.9659258262890683122, 1.000000000000000000, 0.9659258262890683122, 1.000000000000000000, 0.9659258262890683122, 1.000000000000000000, 0.9659258262890683122, 1.000000000000000000, 0.9659258262890683122, 1.000000000000000000, 0.9659258262890683122, 1.000000000000000000, 0.9659258262890683122, 1.000000000000000000, 0.9659258262890683122, 1.000000000000000000, 0.9659258262890683122, 1.000000000000000000, 0.9659258262890683122, 1.000000000000000000, 0.9659258262890683122, 1.000000000000000000, 0.9659258262890683122, 1.000000000000000000, 0.9659258262890683122, 1.000000000000000000, 0.9659258262890683122, 1.000000000000000000, 0.9659258262890683122, 1.000000000000000000, 0.9659258262890683122, 1.000000000000000000, 0.9659258262890683122, 1.000000000000000000, 0.9659258262890683122, 1.000000000000000000, 0.9659258262890683122, 1.000000000000000000, 0.9659258262890683122, 1.000000000000000000, 0.9659258262890683122, 1.000000000000000000, 0.9659258262890683122, 1.000000000000000000, 0.9659258262890683122, 1.000000000000000000, 0.9659258262890683122, 1.000000000000000000, 0.9659258262890683122, 1.000000000000000000, 0.9659258262890683122, 1.000000000000000000, 0.9659258262890683122, 1.000000000000000000, 0.9659258262890683122, 1.000000000000000000, 0.9659258262890683122, 1.000000000000000000, 0.9659258262890683122, 1.000000000000000000, 0.9659258262890683122, 1.000000000000000000, 0.9659258262890683122, 1.000000000000000000, 0.9659258262890683122, 1.000000000000000000, 0.9659258262890683122, 1.000000000000000000, 0.9659258262890683122, 1.000000000000000000, 0.9659258262890683122, 1.000000000000000000, 0.9659258262890683122, 1.000000000000000000, 0.9659258262890683122, 1.000000000000000000, 0.9659258262890683122, 1.000000000000000000, 0.9659258262890683122, 1.000000000000000000, 0.9659258262890683122, 1.000000000000000000, 0.9659258262890683122, 1.000000000000000000, 0.9659258262890683122, 1.000000000000000000, 0.9659258262890683122, 1.000000000000000000, 0.9659258262890683122, 1.000000000000000000, 0.9659258262890683122, 1.000000000000000000, 0.9659258262890683122, 1.000000000000000000, 0.9659258262890683122, 1.000000000000000000, 0.9659258262890683122, 1.000000000000000000, 0.9659258262890683122, 1.000000000000000000, 0.9659258262890683122, 1.000000000000000000, 0.9659258262890683122, 1.000000000000000000, 0.9659258262890683122, 1.000000000000000000, 0.9659258262890683122, 1.000000000000000000, 0.9659258262890683122, 1.000000000000000000, 0.9659258262890683122, 1.000000000000000000, 0.9659258262890683122, 1.000000000000000000, 0.9659258262890683122, 1.000000000000000000, 0.9659258262890683122, 1.000000000000000000, 0.9659258262890683122, 1.000000000000000000, 0.9659258262890683122, 1.000000000000000000, 0.9659258262890683122, 1.000000000000000000, 0.9659258262890683122, 1.000000000000000000, 0.9659258262890683122, 1.000000000000000000, 0.9659258262890683122, 1.000000000000000000, 0.9659258262890683122, 1.000000000000000000, 0.9659258262890683122, 1.000000000000000000, 0.9659258262890683122, 1.000000000000000000, 0.9659258262890683122, 1.000000000000000000, 0.9659258262890683122, 1.000000000000000000, 0.9659258262890683122, 1.000000000000000000, 0.9659258262890683122, 1.000000000000000000, 0.9659258262890683122, 1.000000000000000000, 0.9659258262890683122, 1.000000000000000000, 0.9659258262890683122, 1.000000000000000000, 0.9659258262890683122, 1.000000000000000000, 0.9659258262890683122, 1.000000000000000000, 0.9659258262890683122, 1.000000000000000000, 0.9659258262890683122, 1.000000000000000000, 0.9659258262890683122, 1.000000000000000000, 0.9659258262890683122, 1.000000000000000000, 0.9659258262890683122, 1.000000000000000000, 0.9659258262890683122, 1.000000000000000000, 0.9659258262890683122, 1.000000000000000000, 0.9659258262890683122, 1.000000000000000000, 0.9659258262890683122, 1.000000000000000000, 0.9659258262890683122, 1.000000000000000000, 0.9659258262890683122, 1.000000000000000000, 0.9659258262890683122, 1.000000000000000000, 0.9659258262890683122, 1.000000000000000000, 0.9659258262890683122, 1.000000000000000000, 0.9659258262890683122, 1.000000000000000000, 0.9659258262890683122, 1.000000000000000000, 0.9659258262890683122, 1.000000000000000000, 0.9659258262890683122, 1.000000000000000000, 0.9659258262890683122, 1.000000000000000000, 0.9659258262890683122, 1.000000000000000000, 0.9659258262890683122, 1.000000000000000000, 0.9659258262890683122, 1.000000000000000000, 0.9659258262890683122, 1.000000000000000000, 0.9659258262890683122, 1.000000000000000000, 0.9659258262890683122, 1.000000000000000000, 0.9659258262890683122, 1.000000000000000000, 0.9659258262890683122, 1.000000000000000000, 0.9659258262890683122, 1.000000000000000000, 0.9659258262890683122, 1.000000000000000000, 0.9659258262890683122, 1.000000000000000000, 0.9659258262890683122, 1.000000000000000000, 0.9659258262890683122, 1.000000000000000000) ) ) 
 REPRESENTATION_ITEM ( '' )  SURFACE ( )  );
#93944 = CARTESIAN_POINT ( 'NONE',  ( 19.42250999205614193, 30.14701867748817321, 5.440088680355555262 ) ) ;
#93945 = CARTESIAN_POINT ( 'NONE',  ( 15.44008868035555793, 41.39701867748817676, -9.422509992056140149 ) ) ;
#93946 = CARTESIAN_POINT ( 'NONE',  ( 16.40814093676323893, 0.7903013365970867898, 11.09922568453595026 ) ) ;
#93947 = SURFACE_STYLE_FILL_AREA ( #87424 ) ;
#93948 = CARTESIAN_POINT ( 'NONE',  ( 16.40814093676324603, 62.45696800326376064, -11.09922568453594671 ) ) ;
#93949 = CARTESIAN_POINT ( 'NONE',  ( 5.076628168052704559, 15.17559781766745175, -8.527530157486179263 ) ) ;
#93950 = ORIENTED_EDGE ( 'NONE', *, *, #16980, .F. ) ;
#93951 = ADVANCED_FACE ( 'NONE', ( #88383, #36746 ), #48899, .F. ) ;
#93952 = CARTESIAN_POINT ( 'NONE',  ( -0.8801773607111008646, 28.27201867748817321, 2.915334737309923430 ) ) ;
#93953 = CARTESIAN_POINT ( 'NONE',  ( -1.099225684535947600, 29.54030133659708923, 6.408140936763237150 ) ) ;
#93954 = CARTESIAN_POINT ( 'NONE',  ( -0.2418659066527710233, 55.11633188102327807, 6.114288769123046308 ) ) ;
#93955 = AXIS2_PLACEMENT_3D ( 'NONE', #31494, #46996, #17012 ) ;
#93956 = CARTESIAN_POINT ( 'NONE',  ( 0.1532563361054083140, 61.00893115100078745, 1.131784320476157264E-15 ) ) ;
#93957 = CARTESIAN_POINT ( 'NONE',  ( 10.00000000000000178, 54.31368534415484106, 10.88017736071110342 ) ) ;
#93958 = CARTESIAN_POINT ( 'NONE',  ( 5.076628168052703671, 16.84226448433411960, 8.527530157486179263 ) ) ;
#93959 = CARTESIAN_POINT ( 'NONE',  ( 10.00000000000000178, 30.37363466993042138, 12.81628187352647608 ) ) ;
#93960 = CARTESIAN_POINT ( 'NONE',  ( 10.00000000000000178, 59.31368534415484106, 10.88017736071110342 ) ) ;
#93961 = DIRECTION ( 'NONE',  ( -0.000000000000000000, -1.000000000000000000, -0.000000000000000000 ) ) ;
#93962 = ORIENTED_EDGE ( 'NONE', *, *, #75438, .F. ) ;
#93963 = CARTESIAN_POINT ( 'NONE',  ( 0.5774900079438590739, 2.647018677488170990, -5.440088680355550821 ) ) ;
#93965 = CARTESIAN_POINT ( 'NONE',  ( 20.36894250292379738, 24.92874883491396787, -10.36894250292379027 ) ) ;
#93964 = CARTESIAN_POINT ( 'NONE',  ( -2.816281873526473856, 59.12363466993042493, 9.499525473075851096E-16 ) ) ;
#93966 = EDGE_CURVE ( 'NONE', #25008, #32248, #17926, .T. ) ;
#93967 = CARTESIAN_POINT ( 'NONE',  ( 7.361572987183170547, 17.05059781766745530, 9.846743663894590881 ) ) ;
#93968 = CARTESIAN_POINT ( 'NONE',  ( 17.96484262340118221, 9.938685344154837509, 7.964842623401181321 ) ) ;
#93969 = CARTESIAN_POINT ( 'NONE',  ( 5.076628168052703671, 16.84226448433411960, 8.527530157486179263 ) ) ;
#93970 = CARTESIAN_POINT ( 'NONE',  ( 2.917880565312950480, 60.97041550158063927, -12.26659068614894821 ) ) ;
#93971 = ORIENTED_EDGE ( 'NONE', *, *, #28646, .T. ) ;
#93972 = CARTESIAN_POINT ( 'NONE',  ( -0.8801773607110991993, 2.855352010821504471, -2.915334737309923874 ) ) ;
#93973 = MECHANICAL_DESIGN_GEOMETRIC_PRESENTATION_REPRESENTATION (  '', ( #66781 ), #79557 ) ;
#93974 = CARTESIAN_POINT ( 'NONE',  ( 17.96484262340118221, 24.93868534415484461, 7.964842623401181321 ) ) ;
#93975 = ADVANCED_FACE ( 'NONE', ( #48410 ), #95901, .T. ) ;
#93976 = CARTESIAN_POINT ( 'NONE',  ( 0.000000000000000000, 0.000000000000000000, 0.000000000000000000 ) ) ;
#93977 = AXIS2_PLACEMENT_3D ( 'NONE', #37059, #90042, #51057 ) ;
#93978 = ORIENTED_EDGE ( 'NONE', *, *, #28684, .F. ) ;
#93979 = ORIENTED_EDGE ( 'NONE', *, *, #52861, .T. ) ;
#93980 = CARTESIAN_POINT ( 'NONE',  ( 19.42250999205614548, 15.98035201082150714, -5.440088680355545492 ) ) ;
#93981 = CARTESIAN_POINT ( 'NONE',  ( 5.076628168052703671, 56.84226448433412315, 8.527530157486179263 ) ) ;
#93982 = CARTESIAN_POINT ( 'NONE',  ( 19.38216949554541202, 45.99863466993041072, 9.382169495545424454 ) ) ;
#93983 = CARTESIAN_POINT ( 'NONE',  ( 13.78891971893204804, 0.3640475087720924097, 5.904717858191625979 ) ) ;
#93985 = CARTESIAN_POINT ( 'NONE',  ( 13.79529636645030344, 23.26208216824730002, 14.16423886937410614 ) ) ;
#93984 = PLANE ( 'NONE',  #3627 ) ;
#93986 = CARTESIAN_POINT ( 'NONE',  ( 15.44008868035555260, 34.73035201082151247, 9.422509992056143702 ) ) ;
#93987 = CARTESIAN_POINT ( 'NONE',  ( 20.88017736071110875, 15.77201867748817143, -2.915334737309920765 ) ) ;
#93988 = CARTESIAN_POINT ( 'NONE',  ( 14.92337183194729988, 54.34226448433412315, -8.527530157486177487 ) ) ;
#93989 = CARTESIAN_POINT ( 'NONE',  ( -11.16114668437453084, -52.93485207676555149, -3.749999999999999556 ) ) ;
#93990 = CARTESIAN_POINT ( 'NONE',  ( 18.52753015748617571, 33.09226448433411605, 4.923371831947298993 ) ) ;
#93991 = CARTESIAN_POINT ( 'NONE',  ( 10.00000000000000178, 12.25893115100078568, 9.846743663894594434 ) ) ;
#93992 = CARTESIAN_POINT ( 'NONE',  ( 8.527530157486175710, 23.92559781766745530, -4.923371831947298993 ) ) ;
#93993 = ORIENTED_EDGE ( 'NONE', *, *, #18074, .F. ) ;
#93994 = CARTESIAN_POINT ( 'NONE',  ( -8.564643372776448160, 15.00000000000000000, -12.31449893000752205 ) ) ;
#93995 = CARTESIAN_POINT ( 'NONE',  ( 2.791683348922237240, 10.38393115100078390, -7.208316651077763204 ) ) ;
#93996 = CARTESIAN_POINT ( 'NONE',  ( 19.84674366389459266, 63.71726448433412315, -2.638427012816827677 ) ) ;
#93997 = CARTESIAN_POINT ( 'NONE',  ( 0.5774900079438607392, 48.48035201082150536, 5.440088680355550821 ) ) ;
#93999 = CARTESIAN_POINT ( 'NONE',  ( -2.816281873526473856, 39.12363466993041783, 9.499525473075851096E-16 ) ) ;
#93998 = CARTESIAN_POINT ( 'NONE',  ( 4.559911319644449179, 8.897018677488171434, 9.422509992056141925 ) ) ;
#94000 = CARTESIAN_POINT ( 'NONE',  ( 20.36894250292379738, 34.92874883491396076, -10.36894250292379027 ) ) ;
#94001 = CARTESIAN_POINT ( 'NONE',  ( -14.73513795193453824, 0.04922511925147073086, -0.7223639599948814549 ) ) ;
#94002 = CARTESIAN_POINT ( 'NONE',  ( 19.38216949554541557, 57.24863466993042493, -9.382169495545420901 ) ) ;
#94003 = EDGE_LOOP ( 'NONE', ( #65264, #46762, #96402, #34258 ) ) ;
#94004 = CARTESIAN_POINT ( 'NONE',  ( 7.361572987183170547, 62.05059781766745886, 9.846743663894590881 ) ) ;
#94005 = CARTESIAN_POINT ( 'NONE',  ( 19.42250999205614193, 20.14701867748817321, 5.440088680355555262 ) ) ;
#94006 = ORIENTED_EDGE ( 'NONE', *, *, #3637, .T. ) ;
#94007 = CARTESIAN_POINT ( 'NONE',  ( 5.076628168052704559, 5.175597817667451750, -8.527530157486179263 ) ) ;
#94008 = DIRECTION ( 'NONE',  ( 1.000000000000000000, 0.000000000000000000, 0.000000000000000000 ) ) ;
#94009 = CIRCLE ( 'NONE', #22148, 15.00000000000000000 ) ;
#94010 = CARTESIAN_POINT ( 'NONE',  ( 7.361572987183170547, 7.050597817667451750, 9.846743663894590881 ) ) ;
#94011 = CARTESIAN_POINT ( 'NONE',  ( 0.5774900079438607392, 63.48035201082149825, 5.440088680355550821 ) ) ;
#94012 = DIRECTION ( 'NONE',  ( 0.000000000000000000, 0.000000000000000000, -1.000000000000000000 ) ) ;
#94013 = EDGE_CURVE ( 'NONE', #97221, #77130, #38893, .T. ) ;
#94015 =( LENGTH_UNIT ( ) NAMED_UNIT ( * ) SI_UNIT ( .MILLI., .METRE. ) );
#94014 = CARTESIAN_POINT ( 'NONE',  ( -0.8801773607111008646, 53.27201867748816966, 2.915334737309923430 ) ) ;
#94016 = CARTESIAN_POINT ( 'NONE',  ( -0.8801773607110991993, 62.85535201082150536, -2.915334737309923874 ) ) ;
#94018 = ORIENTED_EDGE ( 'NONE', *, *, #37137, .F. ) ;
#94017 = CARTESIAN_POINT ( 'NONE',  ( 5.076628168052704559, 0.1755978176674514724, -8.527530157486179263 ) ) ;
#94019 = DIRECTION ( 'NONE',  ( 0.9832549075639562819, 0.000000000000000000, -0.1822355254921381451 ) ) ;
#94020 = CARTESIAN_POINT ( 'NONE',  ( 2.791683348922237240, 55.38393115100078745, -7.208316651077763204 ) ) ;
#94021 = EDGE_LOOP ( 'NONE', ( #58871, #24930, #72804, #86377, #66883, #33679, #58139 ) ) ;
#94022 = CARTESIAN_POINT ( 'NONE',  ( 11.35178980618980304, 14.49999999999999112, -9.804941009311946232 ) ) ;
#94023 = B_SPLINE_CURVE_WITH_KNOTS ( 'NONE', 3,
 ( #98568, #37052, #61017, #91017, #21560, #7048, #52532, #83040, #90523, #31495, #37552, #69519, #15548, #67551, #92012, #60527, #54014, #68537, #22058, #38532 ),
 .UNSPECIFIED., .F., .F.,
 ( 4, 2, 2, 2, 2, 2, 2, 2, 2, 4 ),
 ( 0.001219073179698296813, 0.001886422127363689919, 0.002553771075029083026, 0.003888468970359869239, 0.005223166865690655886, 0.006557864761021442099, 0.007892562656352228312, 0.009227260551683014525, 0.01056195844701380074, 0.01189665634234458695 ),
 .UNSPECIFIED. ) ;
#94024 = CARTESIAN_POINT ( 'NONE',  ( -0.3689425029237881626, 7.428748834913967869, 10.36894250292379027 ) ) ;
#94025 = CARTESIAN_POINT ( 'NONE',  ( 16.40814093676324603, 62.45696800326376064, -11.09922568453594671 ) ) ;
#94026 = CARTESIAN_POINT ( 'NONE',  ( 22.26659068614894466, 3.887082168247300906, 7.082119434687054849 ) ) ;
#94027 = B_SPLINE_CURVE_WITH_KNOTS ( 'NONE', 3,
 ( #97282, #49776, #19775, #58758 ),
 .UNSPECIFIED., .F., .F.,
 ( 4, 4 ),
 ( 2.070562745361082850E-16, 0.003685997162761518991 ),
 .UNSPECIFIED. ) ;
#94028 = CARTESIAN_POINT ( 'NONE',  ( -2.266590686148945544, 31.38708216824730002, -7.082119434687050408 ) ) ;
#94029 = STYLED_ITEM ( 'NONE', ( #6793 ), #14479 ) ;
#94030 = CARTESIAN_POINT ( 'NONE',  ( 18.95785429995050819, 57.24216108172005590, 6.499999999999926281 ) ) ;
#94031 = CARTESIAN_POINT ( 'NONE',  ( 13.79529636645031943, 5.345415501580634832, -14.16423886937409904 ) ) ;
#94032 = CARTESIAN_POINT ( 'NONE',  ( 15.44008868035555260, 14.73035201082150536, 9.422509992056143702 ) ) ;
#94033 = CARTESIAN_POINT ( 'NONE',  ( 3.969999999999999751, 9.750000000000000000, 3.750000000000000000 ) ) ;
#94034 = ORIENTED_EDGE ( 'NONE', *, *, #14952, .F. ) ;
#94035 =( NAMED_UNIT ( * ) SI_UNIT ( $, .STERADIAN. ) SOLID_ANGLE_UNIT ( ) );
#94036 = CARTESIAN_POINT ( 'NONE',  ( 10.00000000000000000, 14.75893115100078568, -9.846743663894594434 ) ) ;
#94037 = CARTESIAN_POINT ( 'NONE',  ( 13.43411237798106583, 37.66530133659708923, -12.81628187352647252 ) ) ;
#94038 = CARTESIAN_POINT ( 'NONE',  ( 2.791683348922240793, 31.63393115100078745, 7.208316651077764092 ) ) ;
#94039 = FACE_OUTER_BOUND ( 'NONE', #9803, .T. ) ;
#94040 = CARTESIAN_POINT ( 'NONE',  ( -2.816281873526473856, 34.33196800326376064, 3.434112377981055619 ) ) ;
#94041 = CARTESIAN_POINT ( 'NONE',  ( -3.750000000000000000, 10.00000000000000000, 4.000000000000000000 ) ) ;
#94042 = CARTESIAN_POINT ( 'NONE',  ( 12.63842701281683922, 24.55059781766745175, -9.846743663894590881 ) ) ;
#94043 = EDGE_CURVE ( 'NONE', #9024, #60175, #3843, .T. ) ;
#94044 = CARTESIAN_POINT ( 'NONE',  ( -4.164238869374099927, 17.01208216824730357, 3.795296366450308767 ) ) ;
#94045 = ORIENTED_EDGE ( 'NONE', *, *, #32680, .F. ) ;
#94046 = EDGE_CURVE ( 'NONE', #39776, #31701, #64384, .T. ) ;
#94047 = CARTESIAN_POINT ( 'NONE',  ( 15.44008868035555260, 34.73035201082151247, 9.422509992056143702 ) ) ;
#94048 = CARTESIAN_POINT ( 'NONE',  ( 10.00000000000000178, 28.05374883491396787, 14.16423886937410082 ) ) ;
#94049 = CARTESIAN_POINT ( 'NONE',  ( 18.52753015748617571, 58.09226448433411605, 4.923371831947298993 ) ) ;
#94050 = CARTESIAN_POINT ( 'NONE',  ( 5.076628168052703671, 6.842264484334118713, 8.527530157486179263 ) ) ;
#94052 = CARTESIAN_POINT ( 'NONE',  ( -9.098828036256710661, 88.10682954397124433, 5.081100641017341601 ) ) ;
#94051 = CARTESIAN_POINT ( 'NONE',  ( 10.00000000000000000, 57.87363466993042493, -12.81628187352647608 ) ) ;
#94053 = CARTESIAN_POINT ( 'NONE',  ( 0.5774900079438607392, 23.48035201082150536, 5.440088680355550821 ) ) ;
#94054 = CARTESIAN_POINT ( 'NONE',  ( 22.81628187352648496, 16.83196800326374998, -3.434112377981050290 ) ) ;
#94055 = CARTESIAN_POINT ( 'NONE',  ( -2.816281873526473856, 24.33196800326375353, 3.434112377981055619 ) ) ;
#94056 = CARTESIAN_POINT ( 'NONE',  ( 10.00000000000000178, 42.25893115100078745, 9.846743663894594434 ) ) ;
#94057 = CARTESIAN_POINT ( 'NONE',  ( -5.440088680355558814, 7.230352010821512465, -9.422509992056136596 ) ) ;
#94058 = DIRECTION ( 'NONE',  ( 0.000000000000000000, -1.000000000000000000, 0.000000000000000000 ) ) ;
#94060 = CARTESIAN_POINT ( 'NONE',  ( 0.000000000000000000, 69.99999999999998579, -6.250000000000000000 ) ) ;
#94059 = DIRECTION ( 'NONE',  ( -0.000000000000000000, 1.000000000000000000, -0.000000000000000000 ) ) ;
#94061 = MECHANICAL_DESIGN_GEOMETRIC_PRESENTATION_REPRESENTATION (  '', ( #38198 ), #4645 ) ;
#94062 = CARTESIAN_POINT ( 'NONE',  ( 18.00000000000000000, 84.07179676972448590, 12.00000000000000000 ) ) ;
#94063 = CARTESIAN_POINT ( 'NONE',  ( 11.22915323889580463, -0.03417435944610275333, -8.773176023390609757 ) ) ;
#94064 = CARTESIAN_POINT ( 'NONE',  ( 20.88017736071110164, 50.35535201082151247, 2.915334737309930979 ) ) ;
#94065 = CARTESIAN_POINT ( 'NONE',  ( 2.035157376598822676, 57.43868534415484106, -7.964842623401177768 ) ) ;
#94066 = CARTESIAN_POINT ( 'NONE',  ( 8.157527544166590872, 14.76984925469195886, -12.51706795611453593 ) ) ;
#94067 = CARTESIAN_POINT ( 'NONE',  ( 11.92686044187656336, 11.97997603579417891, 3.195792623639526653 ) ) ;
#94068 = EDGE_CURVE ( 'NONE', #91046, #29895, #36810, .T. ) ;
#94069 = CARTESIAN_POINT ( 'NONE',  ( 20.88017736071110164, 5.355352010821503583, 2.915334737309930979 ) ) ;
#94070 = CARTESIAN_POINT ( 'NONE',  ( 21.09922568453594849, 1.206968003263753531, 6.408140936763242479 ) ) ;
#94072 = CARTESIAN_POINT ( 'NONE',  ( -5.069238243371155583, -24.95996232635749834, -3.750000000000000888 ) ) ;
#94071 = CARTESIAN_POINT ( 'NONE',  ( 20.88017736071110875, 15.77201867748817143, -2.915334737309920765 ) ) ;
#94073 = FACE_OUTER_BOUND ( 'NONE', #11719, .T. ) ;
#94074 = CARTESIAN_POINT ( 'NONE',  ( -2.816281873526473856, 19.33196800326375708, 3.434112377981055619 ) ) ;
#94075 = VERTEX_POINT ( 'NONE', #34379 ) ;
#94076 = CARTESIAN_POINT ( 'NONE',  ( 12.91533473730993009, 56.60535201082151247, -10.88017736071109987 ) ) ;
#94077 = CARTESIAN_POINT ( 'NONE',  ( 19.84674366389459621, 43.50893115100078745, 7.409399052514197653E-17 ) ) ;
#94079 = DIRECTION ( 'NONE',  ( -0.000000000000000000, -0.000000000000000000, -1.000000000000000000 ) ) ;
#94078 = CARTESIAN_POINT ( 'NONE',  ( 10.00000000000000000, 2.873634669930420049, -12.81628187352647608 ) ) ;
#94080 = EDGE_CURVE ( 'NONE', #58432, #54272, #73048, .T. ) ;
#94081 = CARTESIAN_POINT ( 'NONE',  ( 7.084665262690076126, 32.02201867748816966, -10.88017736071110164 ) ) ;
#94082 = CARTESIAN_POINT ( 'NONE',  ( 4.559911319644449179, 37.23035201082150536, -9.422509992056141925 ) ) ;
#94083 = CARTESIAN_POINT ( 'NONE',  ( 22.26659068614895176, 49.72041550158063927, -7.082119434687042414 ) ) ;
#94084 = CARTESIAN_POINT ( 'NONE',  ( 0.1532563361054100626, 35.80059781766745175, -2.638427012816831230 ) ) ;
#94085 = AXIS2_PLACEMENT_3D ( 'NONE', #46446, #24450, #91943 ) ;
#94086 = CARTESIAN_POINT ( 'NONE',  ( -0.8801773607110991993, 62.85535201082150536, -2.915334737309923874 ) ) ;
#94087 = LINE ( 'NONE', #49078, #96931 ) ;
#94088 = CARTESIAN_POINT ( 'NONE',  ( 17.08211943468705840, 20.13708216824730357, -12.26659068614894466 ) ) ;
#94089 = DIRECTION ( 'NONE',  ( 0.000000000000000000, 0.000000000000000000, 1.000000000000000000 ) ) ;
#94090 = EDGE_LOOP ( 'NONE', ( #34990, #37307, #66043 ) ) ;
#94091 = CARTESIAN_POINT ( 'NONE',  ( 17.08211943468705840, 45.13708216824730357, -12.26659068614894466 ) ) ;
#94092 = CARTESIAN_POINT ( 'NONE',  ( 24.16423886937409904, 39.09541550158062506, 3.795296366450317205 ) ) ;
#94093 = CARTESIAN_POINT ( 'NONE',  ( 19.84674366389459621, 13.50893115100078568, 7.409399052514197653E-17 ) ) ;
#94094 = CARTESIAN_POINT ( 'NONE',  ( -2.816281873526473856, 19.12363466993042138, 9.499525473075851096E-16 ) ) ;
#94095 = PLANE ( 'NONE',  #28354 ) ;
#94096 = DIRECTION ( 'NONE',  ( 0.000000000000000000, 1.000000000000000000, 0.000000000000000000 ) ) ;
#94098 = CARTESIAN_POINT ( 'NONE',  ( 19.38216949554541557, 32.24863466993041783, -9.382169495545420901 ) ) ;
#94097 = CARTESIAN_POINT ( 'NONE',  ( -0.8801773607110991993, 57.85535201082149825, -2.915334737309923874 ) ) ;
#94099 = CARTESIAN_POINT ( 'NONE',  ( 17.08211943468705130, 48.47041550158063927, 12.26659068614894998 ) ) ;
#94100 = CARTESIAN_POINT ( 'NONE',  ( 0.5774900079438607392, 68.48035201082150536, 5.440088680355550821 ) ) ;
#94101 = CARTESIAN_POINT ( 'NONE',  ( -4.923371831947302546, -9.824402182332548250, -8.527530157486173934 ) ) ;
#94102 = EDGE_LOOP ( 'NONE', ( #15001, #57606, #57695, #61178 ) ) ;
#94103 = DIRECTION ( 'NONE',  ( -0.000000000000000000, 1.000000000000000000, -0.000000000000000000 ) ) ;
#94104 = ORIENTED_EDGE ( 'NONE', *, *, #40008, .F. ) ;
#94105 = CARTESIAN_POINT ( 'NONE',  ( 13.79529636645031943, 5.345415501580634832, -14.16423886937409904 ) ) ;
#94107 = CARTESIAN_POINT ( 'NONE',  ( -0.8801773607111008646, 8.272018677488171434, 2.915334737309923430 ) ) ;
#94106 = CARTESIAN_POINT ( 'NONE',  ( 4.559911319644449179, 8.897018677488173211, 9.422509992056141925 ) ) ;
#94109 = CARTESIAN_POINT ( 'NONE',  ( 0.6178305044545838731, -0.2513653300695798953, 9.382169495545420901 ) ) ;
#94108 = CARTESIAN_POINT ( 'NONE',  ( 19.84674366389459621, 38.50893115100078745, 7.409399052514197653E-17 ) ) ;
#94110 = FILL_AREA_STYLE ('',( #78627 ) ) ;
#94111 = CARTESIAN_POINT ( 'NONE',  ( 24.35999999999999233, 37.99999999999997868, 10.00000000000000000 ) ) ;
#94112 = B_SPLINE_CURVE_WITH_KNOTS ( 'NONE', 3,
 ( #94822, #27303, #88310, #81782, #18839, #45779, #14804, #89783, #74786, #6295, #82279, #98811, #75279, #36296, #30260, #60274, #43783, #66793 ),
 .UNSPECIFIED., .F., .F.,
 ( 4, 2, 2, 2, 2, 2, 2, 2, 4 ),
 ( 0.000000000000000000, 0.002783400404998704388, 0.005566800809997408776, 0.01113360161999481755, 0.02226720323998963511, 0.04453440647997927021, 0.06680160971996890185, 0.07793521133996370032, 0.08906881295995849879 ),
 .UNSPECIFIED. ) ;
#94113 = CARTESIAN_POINT ( 'NONE',  ( 13.43411237798105340, 20.58196800326374643, 12.81628187352647963 ) ) ;
#94114 = VERTEX_POINT ( 'NONE', #74730 ) ;
#94115 = CARTESIAN_POINT ( 'NONE',  ( 6.204703633549690345, 52.84541550158062506, 14.16423886937410082 ) ) ;
#94116 = ORIENTED_EDGE ( 'NONE', *, *, #79248, .T. ) ;
#94117 = CARTESIAN_POINT ( 'NONE',  ( 24.16423886937410614, 59.51208216824728936, -3.795296366450302550 ) ) ;
#94118 = VERTEX_POINT ( 'NONE', #67237 ) ;
#94119 = CARTESIAN_POINT ( 'NONE',  ( 17.96484262340118221, 36.18868534415484106, -7.964842623401177768 ) ) ;
#94120 = VECTOR ( 'NONE', #20702, 1000.000000000000000 ) ;
#94121 = CARTESIAN_POINT ( 'NONE',  ( 17.96484262340118221, 36.18868534415484106, -7.964842623401177768 ) ) ;
#94122 = CARTESIAN_POINT ( 'NONE',  ( 17.96484262340118221, 41.18868534415484106, -7.964842623401177768 ) ) ;
#94123 = CARTESIAN_POINT ( 'NONE',  ( 15.44008868035555260, 64.73035201082151957, 9.422509992056143702 ) ) ;
#94124 = CARTESIAN_POINT ( 'NONE',  ( 17.96484262340118221, 29.93868534415484106, 7.964842623401181321 ) ) ;
#94125 = EDGE_CURVE ( 'NONE', #70377, #58998, #14756, .T. ) ;
#94126 = CARTESIAN_POINT ( 'NONE',  ( -0.1503990784575277573, 33.10158574516643171, 6.262539305110076171 ) ) ;
#94127 = CARTESIAN_POINT ( 'NONE',  ( 17.20831665107776587, 19.13393115100078035, -7.208316651077762316 ) ) ;
#94128 = DIRECTION ( 'NONE',  ( 0.000000000000000000, 1.000000000000000000, 0.000000000000000000 ) ) ;
#94129 = VERTEX_POINT ( 'NONE', #68720 ) ;
#94130 = CARTESIAN_POINT ( 'NONE',  ( 10.72176212051081734, -40.27637155869391705, 4.000000000000000888 ) ) ;
#94131 = CARTESIAN_POINT ( 'NONE',  ( 10.00000000000000178, 42.25893115100078745, 9.846743663894594434 ) ) ;
#94132 = CARTESIAN_POINT ( 'NONE',  ( -14.49120296996854940, 0.04922511925147123046, -2.766068805437723377 ) ) ;
#94133 = CARTESIAN_POINT ( 'NONE',  ( 19.38216949554541557, 47.24863466993041783, -9.382169495545420901 ) ) ;
#94134 = LINE ( 'NONE', #55147, #93831 ) ;
#94135 = VECTOR ( 'NONE', #68354, 1000.000000000000000 ) ;
#94136 = CARTESIAN_POINT ( 'NONE',  ( -45.94000000000001904, 103.9981609152045507, 5.961202730336936817 ) ) ;
#94137 = CARTESIAN_POINT ( 'NONE',  ( 0.5774900079438607392, 53.48035201082151247, 5.440088680355550821 ) ) ;
#94138 = CARTESIAN_POINT ( 'NONE',  ( -3.384479038598111167, 0.2301507000107681222, -14.55223509985382435 ) ) ;
#94139 = CARTESIAN_POINT ( 'NONE',  ( -2.266590686148945544, 46.38708216824730357, -7.082119434687050408 ) ) ;
#94140 = DIRECTION ( 'NONE',  ( 0.000000000000000000, 1.000000000000000000, 0.000000000000000000 ) ) ;
#94141 = ORIENTED_EDGE ( 'NONE', *, *, #85796, .F. ) ;
#94142 = CARTESIAN_POINT ( 'NONE',  ( 5.817157072110804350, 14.49999999999999112, -13.82608706751093663 ) ) ;
#94143 = CARTESIAN_POINT ( 'NONE',  ( 19.84674366389459266, 13.71726448433411782, -2.638427012816827677 ) ) ;
#94144 = SURFACE_STYLE_USAGE ( .BOTH. , #63637 ) ;
#94145 = VECTOR ( 'NONE', #22388, 1000.000000000000000 ) ;
#94146 = CARTESIAN_POINT ( 'NONE',  ( 12.63842701281683034, 57.46726448433411605, 9.846743663894596210 ) ) ;
#94147 = CARTESIAN_POINT ( 'NONE',  ( 20.88017736071110519, 65.56368534415483396, 2.639326808657452039E-16 ) ) ;
#94148 = CARTESIAN_POINT ( 'NONE',  ( -0.1503990784575328643, 65.12777174578613426, 6.262539305110068177 ) ) ;
#94149 = CARTESIAN_POINT ( 'NONE',  ( 19.84674366389459266, 53.71726448433411605, -2.638427012816827677 ) ) ;
#94150 = CARTESIAN_POINT ( 'NONE',  ( 12.67147417979171031, 14.95037112956503655, 7.555862176155596188 ) ) ;
#94151 = EDGE_CURVE ( 'NONE', #27398, #87174, #60710, .T. ) ;
#94152 = ORIENTED_EDGE ( 'NONE', *, *, #80380, .T. ) ;
#94153 = EDGE_CURVE ( 'NONE', #58602, #28561, #87404, .T. ) ;
#94154 = CARTESIAN_POINT ( 'NONE',  ( 24.16423886937409904, 64.09541550158064638, 3.795296366450317205 ) ) ;
#94155 = DIRECTION ( 'NONE',  ( 0.000000000000000000, 0.000000000000000000, 1.000000000000000000 ) ) ;
#94156 = CARTESIAN_POINT ( 'NONE',  ( 12.91533473730993009, 41.60535201082149825, -10.88017736071109987 ) ) ;
#94158 = CARTESIAN_POINT ( 'NONE',  ( 10.00676502675680446, 12.82908929790087527, -5.835523404638878198 ) ) ;
#94157 = CARTESIAN_POINT ( 'NONE',  ( 19.38216949554541557, 12.24863466993041961, -9.382169495545420901 ) ) ;
#94159 = CARTESIAN_POINT ( 'NONE',  ( 10.93781366033348768, 0.3639309795253655722, -10.26470809774068371 ) ) ;
#94160 = DIRECTION ( 'NONE',  ( -0.000000000000000000, -1.000000000000000000, -0.000000000000000000 ) ) ;
#94161 = CARTESIAN_POINT ( 'NONE',  ( -12.80781515976305762, -0.03417435944610275333, -6.246788841744501219 ) ) ;
#94162 = CARTESIAN_POINT ( 'NONE',  ( 2.791683348922240793, 56.63393115100078035, 7.208316651077764092 ) ) ;
#94163 = CARTESIAN_POINT ( 'NONE',  ( 9.422509992056141925, -34.85298132251183034, 5.440088680355547268 ) ) ;
#94164 = CARTESIAN_POINT ( 'NONE',  ( 0.6178305044545818747, 13.49863466993041783, -9.382169495545419124 ) ) ;
#94166 = CARTESIAN_POINT ( 'NONE',  ( -11.22915323889568562, -0.03417435944610275333, -8.773176023390764300 ) ) ;
#94165 = CARTESIAN_POINT ( 'NONE',  ( 4.559911319644449179, 18.89701867748817321, 9.422509992056141925 ) ) ;
#94167 = CARTESIAN_POINT ( 'NONE',  ( 17.08211943468705840, 35.13708216824730357, -12.26659068614894466 ) ) ;
#94168 = CARTESIAN_POINT ( 'NONE',  ( 24.16423886937410614, 34.30374883491396787, 8.672049930838204340E-16 ) ) ;
#94169 = CARTESIAN_POINT ( 'NONE',  ( 10.00000000000000178, 4.313685344154837509, 10.88017736071110342 ) ) ;
#94170 = CARTESIAN_POINT ( 'NONE',  ( 17.20831665107776587, 49.13393115100078745, -7.208316651077762316 ) ) ;
#94171 = CARTESIAN_POINT ( 'NONE',  ( -1.099225684535947600, 38.70696800326375353, -6.408140936763238038 ) ) ;
#94172 = CARTESIAN_POINT ( 'NONE',  ( 12.91533473730992121, 14.52201867748817143, 10.88017736071110164 ) ) ;
#94173 = EDGE_LOOP ( 'NONE', ( #76259, #39063, #80983, #25313 ) ) ;
#94174 = CARTESIAN_POINT ( 'NONE',  ( 12.63842701281683922, 34.55059781766745886, -9.846743663894590881 ) ) ;
#94175 = CARTESIAN_POINT ( 'NONE',  ( -0.8801773607110991993, 42.85535201082150536, -2.915334737309923874 ) ) ;
#94176 = CARTESIAN_POINT ( 'NONE',  ( 3.591859063236763294, 8.290301336597087456, -11.09922568453595026 ) ) ;
#94178 = CARTESIAN_POINT ( 'NONE',  ( -14.04867373755345561, 15.00000000000000000, -7.649324326489842285 ) ) ;
#94177 = CARTESIAN_POINT ( 'NONE',  ( 24.16423886937410614, 19.30374883491397142, 8.672049930838204340E-16 ) ) ;
#94179 = DIRECTION ( 'NONE',  ( -1.257402221000611116E-16, 1.000000000000000000, -0.000000000000000000 ) ) ;
#94180 = UNCERTAINTY_MEASURE_WITH_UNIT (LENGTH_MEASURE( 1.000000000000000082E-05 ), #15588, 'distance_accuracy_value', 'NONE');
#94181 = CARTESIAN_POINT ( 'NONE',  ( 14.92337183194729988, 29.34226448433411960, -8.527530157486177487 ) ) ;
#94182 = CARTESIAN_POINT ( 'NONE',  ( -2.816281873526473856, 49.12363466993042493, 9.499525473075851096E-16 ) ) ;
#94183 = CARTESIAN_POINT ( 'NONE',  ( 12.63842701281683034, 52.46726448433413026, 9.846743663894596210 ) ) ;
#94184 = ORIENTED_EDGE ( 'NONE', *, *, #76649, .F. ) ;
#94185 = CARTESIAN_POINT ( 'NONE',  ( 6.004190426492125532, -34.81345361117713111, 3.750000000000001776 ) ) ;
#94186 = CARTESIAN_POINT ( 'NONE',  ( 12.91533473730992121, 4.522018677488170546, 10.88017736071110164 ) ) ;
#94187 = CARTESIAN_POINT ( 'NONE',  ( -0.3689425029237881626, 12.42874883491396609, 10.36894250292379027 ) ) ;
#94188 = CARTESIAN_POINT ( 'NONE',  ( -0.8801773607110991993, 67.85535201082151957, -2.915334737309923874 ) ) ;
#94189 = CARTESIAN_POINT ( 'NONE',  ( 7.361572987183170547, 52.05059781766745175, 9.846743663894590881 ) ) ;
#94190 = CARTESIAN_POINT ( 'NONE',  ( 19.42250999205614193, 25.14701867748817321, 5.440088680355555262 ) ) ;
#94191 = DIRECTION ( 'NONE',  ( 1.000000000000000000, 0.000000000000000000, 0.000000000000000000 ) ) ;
#94192 = CARTESIAN_POINT ( 'NONE',  ( 12.63842701281683922, 64.55059781766745175, -9.846743663894590881 ) ) ;
#94193 = AXIS2_PLACEMENT_3D ( 'NONE', #73817, #11354, #57342 ) ;
#94194 = ADVANCED_FACE ( 'NONE', ( #60223 ), #2287, .T. ) ;
#94195 = UNCERTAINTY_MEASURE_WITH_UNIT (LENGTH_MEASURE( 1.000000000000000082E-05 ), #43632, 'distance_accuracy_value', 'NONE');
#94196 = CARTESIAN_POINT ( 'NONE',  ( 6.579634127946608402, -87.99828267815712479, 2.500000000000000000 ) ) ;
#94197 = VERTEX_POINT ( 'NONE', #22735 ) ;
#94198 = ORIENTED_EDGE ( 'NONE', *, *, #46213, .T. ) ;
#94199 = DIRECTION ( 'NONE',  ( -0.000000000000000000, -0.000000000000000000, 1.000000000000000000 ) ) ;
#94200 = CARTESIAN_POINT ( 'NONE',  ( -2.266590686148945544, 6.387082168247300906, -7.082119434687050408 ) ) ;
#94201 = CARTESIAN_POINT ( 'NONE',  ( -4.164238869374098151, 1.595415501580634388, -3.795296366450310543 ) ) ;
#94202 = CARTESIAN_POINT ( 'NONE',  ( 13.79529636645030344, 48.26208216824728936, 14.16423886937410614 ) ) ;
#94203 = CARTESIAN_POINT ( 'NONE',  ( 2.791683348922237240, 60.38393115100078745, -7.208316651077763204 ) ) ;
#94204 = CARTESIAN_POINT ( 'NONE',  ( 14.92337183194729633, 27.67559781766745530, 8.527530157486181039 ) ) ;
#94205 = DIRECTION ( 'NONE',  ( -0.000000000000000000, 0.000000000000000000, 1.000000000000000000 ) ) ;
#94207 = CARTESIAN_POINT ( 'NONE',  ( 5.076628168052704559, 65.17559781766745175, -8.527530157486179263 ) ) ;
#94206 = CARTESIAN_POINT ( 'NONE',  ( 7.084665262690076126, 14.10535201082150358, 10.88017736071109987 ) ) ;
#94208 = FILL_AREA_STYLE ('',( #16261 ) ) ;
#94209 = CARTESIAN_POINT ( 'NONE',  ( 22.26659068614894466, 38.88708216824731068, 7.082119434687054849 ) ) ;
#94210 = CARTESIAN_POINT ( 'NONE',  ( -2.266590686148945544, 66.38708216824730357, -7.082119434687050408 ) ) ;
#94211 = DIRECTION ( 'NONE',  ( -1.000000000000000000, 0.000000000000000000, 0.000000000000000000 ) ) ;
#94212 = CARTESIAN_POINT ( 'NONE',  ( 17.97400638239465565, 77.67876782659364210, 4.131022355321460893 ) ) ;
#94213 = CARTESIAN_POINT ( 'NONE',  ( 4.559911319644449179, 63.89701867748817676, 9.422509992056141925 ) ) ;
#94214 = CARTESIAN_POINT ( 'NONE',  ( 1.472469842513823179, 16.42559781766745175, 4.923371831947296329 ) ) ;
#94215 = VECTOR ( 'NONE', #84227, 1000.000000000000000 ) ;
#94216 = CARTESIAN_POINT ( 'NONE',  ( -7.116171662378945051, -80.69120418497870162, 3.749999999999193534 ) ) ;
#94217 = ORIENTED_EDGE ( 'NONE', *, *, #60315, .T. ) ;
#94218 = CARTESIAN_POINT ( 'NONE',  ( 21.92686044187657401, 30.37045670184114599, -3.195792623639525765 ) ) ;
#94219 = EDGE_LOOP ( 'NONE', ( #26225, #19079, #31748, #84164 ) ) ;
#94220 = CARTESIAN_POINT ( 'NONE',  ( 19.84674366389459621, 23.50893115100078390, 7.409399052514197653E-17 ) ) ;
#94221 = EDGE_LOOP ( 'NONE', ( #82585, #90564, #42007, #97317 ) ) ;
#94222 = CARTESIAN_POINT ( 'NONE',  ( -4.164238869374099927, 37.01208216824731068, 3.795296366450308767 ) ) ;
#94223 = CARTESIAN_POINT ( 'NONE',  ( 7.361572987183169658, 29.96726448433411960, -9.846743663894592657 ) ) ;
#94224 = CARTESIAN_POINT ( 'NONE',  ( 20.88017736071110875, 45.77201867748816966, -2.915334737309920765 ) ) ;
#94225 = CARTESIAN_POINT ( 'NONE',  ( 19.42250999205614548, 45.98035201082150536, -5.440088680355545492 ) ) ;
#94226 = CARTESIAN_POINT ( 'NONE',  ( 0.1077916266722479394, 2.240628644642390643, -6.478736007405952790 ) ) ;
#94227 = CARTESIAN_POINT ( 'NONE',  ( -12.81628187352647252, -0.6680319967362452482, 3.434112377981066722 ) ) ;
#94228 = EDGE_LOOP ( 'NONE', ( #60648, #82250, #22561, #86626 ) ) ;
#94229 = CARTESIAN_POINT ( 'NONE',  ( -2.266590686148945544, 6.387082168247300906, -7.082119434687050408 ) ) ;
#94230 = VERTEX_POINT ( 'NONE', #76702 ) ;
#94231 = ORIENTED_EDGE ( 'NONE', *, *, #7735, .F. ) ;
#94232 = CARTESIAN_POINT ( 'NONE',  ( 2.791683348922240793, 1.633931151000784565, 7.208316651077764092 ) ) ;
#94233 = CARTESIAN_POINT ( 'NONE',  ( 13.43411237798106583, 37.66530133659708923, -12.81628187352647252 ) ) ;
#94234 = CARTESIAN_POINT ( 'NONE',  ( -42.70923076923077844, 104.8461538461538396, -9.500000000000000000 ) ) ;
#94235 = CARTESIAN_POINT ( 'NONE',  ( 2.791683348922240793, 21.63393115100078745, 7.208316651077764092 ) ) ;
#94236 = CARTESIAN_POINT ( 'NONE',  ( 14.40939250469966026, 4.578996266948430760E-16, -1.618458416365756714 ) ) ;
#94237 = LINE ( 'NONE', #25768, #87837 ) ;
#94238 = CARTESIAN_POINT ( 'NONE',  ( 1.472469842513823179, 36.42559781766745175, 4.923371831947296329 ) ) ;
#94239 = EDGE_CURVE ( 'NONE', #96487, #79084, #83720, .T. ) ;
#94241 = CIRCLE ( 'NONE', #6460, 14.49999999999999822 ) ;
#94240 = CARTESIAN_POINT ( 'NONE',  ( 15.44008868035555793, 61.39701867748817676, -9.422509992056140149 ) ) ;
#94242 =( LENGTH_UNIT ( ) NAMED_UNIT ( * ) SI_UNIT ( .MILLI., .METRE. ) );
#94243 = CARTESIAN_POINT ( 'NONE',  ( 4.559911319644449179, 63.89701867748817676, 9.422509992056141925 ) ) ;
#94244 = DIRECTION ( 'NONE',  ( -1.000000000000000000, 0.000000000000000000, -0.000000000000000000 ) ) ;
#94245 = FILL_AREA_STYLE ('',( #32758 ) ) ;
#94246 = CARTESIAN_POINT ( 'NONE',  ( 0.1532563361054083140, 11.00893115100078568, 1.131784320476157264E-15 ) ) ;
#94247 = CARTESIAN_POINT ( 'NONE',  ( 22.81628187352648496, 6.831968003263753531, -3.434112377981050290 ) ) ;
#94248 = TOROIDAL_SURFACE ( 'NONE', #68714, 14.49999999999999822, 0.5000000000000000000 ) ;
#94249 = CARTESIAN_POINT ( 'NONE',  ( 11.62006642627357778, -3.022637072276969577E-15, 8.881585844847220912 ) ) ;
#94250 = CIRCLE ( 'NONE', #54281, 10.90000000000026326 ) ;
#94251 = CARTESIAN_POINT ( 'NONE',  ( 7.361572987183169658, 44.96726448433412315, -9.846743663894592657 ) ) ;
#94252 = CARTESIAN_POINT ( 'NONE',  ( 0.6178305044545838731, 64.74863466993043914, 9.382169495545420901 ) ) ;
#94253 = CARTESIAN_POINT ( 'NONE',  ( 17.08211943468705840, 10.13708216824730179, -12.26659068614894466 ) ) ;
#94254 = CARTESIAN_POINT ( 'NONE',  ( 1.472469842513823179, 31.42559781766745530, 4.923371831947296329 ) ) ;
#94255 = CARTESIAN_POINT ( 'NONE',  ( 22.81628187352647785, 36.41530133659707502, 3.434112377981063169 ) ) ;
#94257 = CARTESIAN_POINT ( 'NONE',  ( 0.5774900079438590739, 22.64701867748817321, -5.440088680355550821 ) ) ;
#94256 = CARTESIAN_POINT ( 'NONE',  ( 38.04706783004212411, 44.99999999999999289, 7.000000000000000000 ) ) ;
#94258 = CARTESIAN_POINT ( 'NONE',  ( -0.8801773607111008646, 43.27201867748817676, 2.915334737309923430 ) ) ;
#94259 = AXIS2_PLACEMENT_3D ( 'NONE', #26243, #64708, #94738 ) ;
#94260 = CARTESIAN_POINT ( 'NONE',  ( 19.38216949554541202, 0.9986346699304200492, 9.382169495545424454 ) ) ;
#94261 = CARTESIAN_POINT ( 'NONE',  ( 4.850097797904172836, 14.95037102666663920, 13.93319274793806173 ) ) ;
#94262 = CARTESIAN_POINT ( 'NONE',  ( 12.63842701281683922, 19.55059781766745175, -9.846743663894590881 ) ) ;
#94263 = CARTESIAN_POINT ( 'NONE',  ( 7.084665262690076126, 29.10535201082150181, 10.88017736071109987 ) ) ;
#94264 = CARTESIAN_POINT ( 'NONE',  ( 19.38216949554541557, 32.24863466993041783, -9.382169495545420901 ) ) ;
#94265 = CARTESIAN_POINT ( 'NONE',  ( 7.361572987183169658, 19.96726448433411960, -9.846743663894592657 ) ) ;
#94266 =( NAMED_UNIT ( * ) PLANE_ANGLE_UNIT ( ) SI_UNIT ( $, .RADIAN. ) );
#94267 = CARTESIAN_POINT ( 'NONE',  ( -14.04391541078765826, 15.00000000000000000, 3.608107528142729503 ) ) ;
#94268 = ADVANCED_FACE ( 'NONE', ( #38716 ), #67739, .T. ) ;
#94269 = CARTESIAN_POINT ( 'NONE',  ( 0.5774900079438590739, 17.64701867748817321, -5.440088680355550821 ) ) ;
#94270 = CARTESIAN_POINT ( 'NONE',  ( 12.91533473730993009, 61.60535201082150536, -10.88017736071109987 ) ) ;
#94271 = CARTESIAN_POINT ( 'NONE',  ( 4.559911319644449179, 8.897018677488171434, 9.422509992056141925 ) ) ;
#94273 = CARTESIAN_POINT ( 'NONE',  ( 19.42250999205614193, 25.14701867748817321, 5.440088680355555262 ) ) ;
#94272 = CARTESIAN_POINT ( 'NONE',  ( 5.076628168052704559, 40.17559781766745175, -8.527530157486179263 ) ) ;
#94274 = DIRECTION ( 'NONE',  ( 0.000000000000000000, 0.000000000000000000, 1.000000000000000000 ) ) ;
#94275 = CARTESIAN_POINT ( 'NONE',  ( 15.44008868035555260, 39.73035201082150536, 9.422509992056143702 ) ) ;
#94277 = CARTESIAN_POINT ( 'NONE',  ( -0.3289641300568005855, 19.27164270246084499, -5.963430220938281678 ) ) ;
#94276 = CARTESIAN_POINT ( 'NONE',  ( 12.91533473730993009, 6.605352010821504471, -10.88017736071109987 ) ) ;
#94278 = CIRCLE ( 'NONE', #38421, 11.92686044187656513 ) ;
#94279 = DIRECTION ( 'NONE',  ( 1.000000000000000000, -5.782411586589362323E-17, 0.000000000000000000 ) ) ;
#94280 = CARTESIAN_POINT ( 'NONE',  ( 19.84674366389459266, 38.30059781766745175, 2.638427012816836559 ) ) ;
#94282 = CARTESIAN_POINT ( 'NONE',  ( 17.39651004071897589, 34.08210964143323451, -6.499999999999361400 ) ) ;
#94281 = CARTESIAN_POINT ( 'NONE',  ( 13.79529636645031943, 45.34541550158062506, -14.16423886937409904 ) ) ;
#94283 = CARTESIAN_POINT ( 'NONE',  ( 1.492507162822240385, 7.199555875704810148, -6.500000000000008882 ) ) ;
#94284 = CARTESIAN_POINT ( 'NONE',  ( 22.81628187352647785, 6.415301336597088344, 3.434112377981063169 ) ) ;
#94285 = CARTESIAN_POINT ( 'NONE',  ( 0.000000000000000000, 0.5000000000000004441, 0.000000000000000000 ) ) ;
#94286 = CARTESIAN_POINT ( 'NONE',  ( 22.26659068614895176, 29.72041550158063572, -7.082119434687042414 ) ) ;
#94288 = DIRECTION ( 'NONE',  ( 0.9426414910921783186, 0.000000000000000000, -0.3338068592337714025 ) ) ;
#94287 = AXIS2_PLACEMENT_3D ( 'NONE', #88603, #4145, #49138 ) ;
#94289 = VERTEX_POINT ( 'NONE', #90717 ) ;
#94290 = CARTESIAN_POINT ( 'NONE',  ( 17.08211943468705130, 63.47041550158063927, 12.26659068614894998 ) ) ;
#94291 = CARTESIAN_POINT ( 'NONE',  ( 17.20831665107776587, 24.13393115100078035, -7.208316651077762316 ) ) ;
#94292 = CARTESIAN_POINT ( 'NONE',  ( 2.393480905993150998, 0.5000000000000004441, -14.80781041047751323 ) ) ;
#94293 = CARTESIAN_POINT ( 'NONE',  ( 17.96484262340118221, 56.18868534415484817, -7.964842623401177768 ) ) ;
#94294 = CARTESIAN_POINT ( 'NONE',  ( -1.099225684535947600, 58.70696800326375353, -6.408140936763238038 ) ) ;
#94295 = CARTESIAN_POINT ( 'NONE',  ( 12.91533473730992121, 29.52201867748817321, 10.88017736071110164 ) ) ;
#94296 = DIRECTION ( 'NONE',  ( 0.000000000000000000, 0.000000000000000000, 1.000000000000000000 ) ) ;
#94297 = CARTESIAN_POINT ( 'NONE',  ( 19.38216949554541202, 10.99863466993042138, 9.382169495545424454 ) ) ;
#94298 = CARTESIAN_POINT ( 'NONE',  ( 12.63842701281683034, 17.46726448433411250, 9.846743663894596210 ) ) ;
#94299 = EDGE_LOOP ( 'NONE', ( #71411, #93189, #37734, #67253 ) ) ;
#94300 = CARTESIAN_POINT ( 'NONE',  ( 0.1532563361054100626, 0.8005978176674514168, -2.638427012816831230 ) ) ;
#94301 = FACE_OUTER_BOUND ( 'NONE', #84561, .T. ) ;
#94302 = CARTESIAN_POINT ( 'NONE',  ( 17.08211943468705130, 58.47041550158063927, 12.26659068614894998 ) ) ;
#94303 = CARTESIAN_POINT ( 'NONE',  ( 20.36894250292379738, 24.92874883491396787, -10.36894250292379027 ) ) ;
#94304 = CARTESIAN_POINT ( 'NONE',  ( 15.44008868035555260, 49.73035201082150536, 9.422509992056143702 ) ) ;
#94305 = CYLINDRICAL_SURFACE ( 'NONE', #67076, 11.92686044187656513 ) ;
#94306 = EDGE_CURVE ( 'NONE', #87326, #42998, #57223, .T. ) ;
#94307 = CARTESIAN_POINT ( 'NONE',  ( 8.650319761586390044, -1.048872767157960961, -3.999999999999999112 ) ) ;
#94308 = CARTESIAN_POINT ( 'NONE',  ( 2.791683348922240793, 6.633931151000785675, 7.208316651077764092 ) ) ;
#94309 = CARTESIAN_POINT ( 'NONE',  ( 18.52753015748618282, 23.92559781766745530, -4.923371831947291888 ) ) ;
#94310 =( NAMED_UNIT ( * ) SI_UNIT ( $, .STERADIAN. ) SOLID_ANGLE_UNIT ( ) );
#94311 = CARTESIAN_POINT ( 'NONE',  ( -12.00809552683971759, 14.49999999999999112, 8.989195838243478676 ) ) ;
#94312 = CARTESIAN_POINT ( 'NONE',  ( 19.84674366389459621, 28.50893115100078745, 7.409399052514197653E-17 ) ) ;
#94313 = CARTESIAN_POINT ( 'NONE',  ( 17.20831665107776587, 44.13393115100078745, -7.208316651077762316 ) ) ;
#94314 = AXIS2_PLACEMENT_3D ( 'NONE', #56754, #56279, #73225 ) ;
#94315 = EDGE_CURVE ( 'NONE', #20515, #87279, #21391, .T. ) ;
#94316 = UNCERTAINTY_MEASURE_WITH_UNIT (LENGTH_MEASURE( 1.000000000000000082E-05 ), #69164, 'distance_accuracy_value', 'NONE');
#94317 =( BOUNDED_SURFACE ( )  B_SPLINE_SURFACE ( 3, 2, ( 
 ( #97197, #19692, #73170 ),
 ( #65672, #44655, #50179 ),
 ( #14171, #58669, #96696 ),
 ( #13169, #36674, #96193 ),
 ( #58163, #82155, #51176 ),
 ( #50685, #81177, #36172 ),
 ( #66672, #59157, #21174 ),
 ( #13667, #44151, #74659 ),
 ( #61130, #30131, #91640 ),
 ( #46142, #68162, #69141 ),
 ( #68645, #669, #38159 ),
 ( #60637, #31119, #175 ),
 ( #14675, #84632, #23158 ),
 ( #15659, #6660, #8147 ),
 ( #53140, #61614, #16134 ),
 ( #76628, #38640, #54119 ),
 ( #91138, #29635, #83649 ),
 ( #22664, #77118, #54605 ),
 ( #15164, #45141, #92132 ),
 ( #75647, #23657, #46620 ),
 ( #30623, #85121, #31613 ),
 ( #53633, #8630, #39139 ),
 ( #45645, #7668, #76142 ),
 ( #1153, #7159, #90640 ),
 ( #67669, #37176, #84153 ),
 ( #69629, #62104, #37662 ),
 ( #16632, #92614, #75150 ),
 ( #98179, #52647, #24138 ),
 ( #60143, #98682, #22165 ),
 ( #83150, #49090, #48094 ) ),
 .UNSPECIFIED., .F., .F., .F. ) 
 B_SPLINE_SURFACE_WITH_KNOTS ( ( 4, 2, 2, 2, 2, 2, 2, 2, 2, 2, 2, 2, 2, 2, 4 ),
 ( 3, 3 ),
 ( 0.000000000000000000, 0.001557317058375510058, 0.003114634116751020115, 0.006229268233502040231, 0.01245853646700408046, 0.01868780470050612069, 0.02491707293400816092, 0.03737560940101224138, 0.04983414586801632185, 0.06229268233502040231, 0.07475121880202448277, 0.08720975526902856323, 0.09343902350253061040, 0.09655365761928162704, 0.09966829173603264369 ),
 ( 0.000000000000000000, 1.000000000000000000 ),
 .UNSPECIFIED. ) 
 GEOMETRIC_REPRESENTATION_ITEM ( )  RATIONAL_B_SPLINE_SURFACE ( (
 ( 1.000000000000000000, 0.7071067811865445751, 1.000000000000000000),
 ( 1.000000000000000000, 0.7071067811865445751, 1.000000000000000000),
 ( 1.000000000000000000, 0.7071067811865475727, 1.000000000000000000),
 ( 1.000000000000000000, 0.7071067811865475727, 1.000000000000000000),
 ( 1.000000000000000000, 0.7071067811865451302, 1.000000000000000000),
 ( 1.000000000000000000, 0.7071067811865451302, 1.000000000000000000),
 ( 1.000000000000000000, 0.7071067811865500152, 1.000000000000000000),
 ( 1.000000000000000000, 0.7071067811865500152, 1.000000000000000000),
 ( 1.000000000000000000, 0.7071067811865475727, 1.000000000000000000),
 ( 1.000000000000000000, 0.7071067811865475727, 1.000000000000000000),
 ( 1.000000000000000000, 0.7071067811865450192, 1.000000000000000000),
 ( 1.000000000000000000, 0.7071067811865450192, 1.000000000000000000),
 ( 1.000000000000000000, 0.7071067811865475727, 1.000000000000000000),
 ( 1.000000000000000000, 0.7071067811865475727, 1.000000000000000000),
 ( 1.000000000000000000, 0.7071067811865473507, 1.000000000000000000),
 ( 1.000000000000000000, 0.7071067811865473507, 1.000000000000000000),
 ( 1.000000000000000000, 0.7071067811865451302, 1.000000000000000000),
 ( 1.000000000000000000, 0.7071067811865451302, 1.000000000000000000),
 ( 1.000000000000000000, 0.7071067811865475727, 1.000000000000000000),
 ( 1.000000000000000000, 0.7071067811865475727, 1.000000000000000000),
 ( 1.000000000000000000, 0.7071067811865475727, 1.000000000000000000),
 ( 1.000000000000000000, 0.7071067811865475727, 1.000000000000000000),
 ( 1.000000000000000000, 0.7071067811865475727, 1.000000000000000000),
 ( 1.000000000000000000, 0.7071067811865475727, 1.000000000000000000),
 ( 1.000000000000000000, 0.7071067811865475727, 1.000000000000000000),
 ( 1.000000000000000000, 0.7071067811865475727, 1.000000000000000000),
 ( 1.000000000000000000, 0.7071067811865475727, 1.000000000000000000),
 ( 1.000000000000000000, 0.7071067811865475727, 1.000000000000000000),
 ( 1.000000000000000000, 0.7071067811865475727, 1.000000000000000000),
 ( 1.000000000000000000, 0.7071067811865475727, 1.000000000000000000) ) ) 
 REPRESENTATION_ITEM ( '' )  SURFACE ( )  );
#94318 = AXIS2_PLACEMENT_3D ( 'NONE', #32569, #71574, #77574 ) ;
#94319 = CARTESIAN_POINT ( 'NONE',  ( 19.38216949554541202, 50.99863466993042493, 9.382169495545424454 ) ) ;
#94320 = CARTESIAN_POINT ( 'NONE',  ( 4.559911319644449179, 47.23035201082150536, -9.422509992056141925 ) ) ;
#94321 = CARTESIAN_POINT ( 'NONE',  ( 5.076628168052703671, 31.84226448433412315, 8.527530157486179263 ) ) ;
#94323 = CARTESIAN_POINT ( 'NONE',  ( 0.1532563361054082862, 21.21726448433412315, 2.638427012816831674 ) ) ;
#94322 = CARTESIAN_POINT ( 'NONE',  ( 24.16423886937409904, 49.09541550158063217, 3.795296366450317205 ) ) ;
#94324 = DIRECTION ( 'NONE',  ( 0.000000000000000000, 0.000000000000000000, 1.000000000000000000 ) ) ;
#94325 = CARTESIAN_POINT ( 'NONE',  ( 7.361572987183170547, 57.05059781766744464, 9.846743663894590881 ) ) ;
#94327 = CARTESIAN_POINT ( 'NONE',  ( 17.08211943468705840, 10.13708216824730179, -12.26659068614894466 ) ) ;
#94326 = CARTESIAN_POINT ( 'NONE',  ( 17.20831665107776587, 42.88393115100077324, 7.208316651077764980 ) ) ;
#94328 =( BOUNDED_CURVE ( )  B_SPLINE_CURVE ( 2, ( #66057, #96584, #59054, #6550, #60036, #89061, #74048, #28559, #21066 ),
 .UNSPECIFIED., .F., .T. ) 
 B_SPLINE_CURVE_WITH_KNOTS ( ( 3, 2, 2, 2, 3 ),
 ( 0.04537130733198223298, 0.04761904761904761640, 0.05357142857142856845, 0.05952380952380952051, 0.06177154981087491087 ),
 .UNSPECIFIED. ) 
 CURVE ( )  GEOMETRIC_REPRESENTATION_ITEM ( )  RATIONAL_B_SPLINE_CURVE ( ( 0.9839835555609424134, 0.9871328979762477029, 1.000000000000000000, 0.9659258262890683122, 1.000000000000000000, 0.9659258262890683122, 1.000000000000000000, 0.9871328979762477029, 0.9839835555609424134 ) ) 
 REPRESENTATION_ITEM ( '' )  );
#94329 = CARTESIAN_POINT ( 'NONE',  ( 13.79529636645031943, 30.34541550158063927, -14.16423886937409904 ) ) ;
#94330 = CARTESIAN_POINT ( 'NONE',  ( 7.361572987183170547, 27.05059781766745175, 9.846743663894590881 ) ) ;
#94331 = VECTOR ( 'NONE', #7768, 1000.000000000000000 ) ;
#94332 = CARTESIAN_POINT ( 'NONE',  ( 20.88017736071110875, 25.77201867748816966, -2.915334737309920765 ) ) ;
#94333 = EDGE_CURVE ( 'NONE', #64921, #13800, #82733, .T. ) ;
#94334 = AXIS2_PLACEMENT_3D ( 'NONE', #16497, #77968, #69494 ) ;
#94335 = CARTESIAN_POINT ( 'NONE',  ( 19.42250999205614193, 50.14701867748817676, 5.440088680355555262 ) ) ;
#94336 = CARTESIAN_POINT ( 'NONE',  ( 20.88017736071110519, 40.56368534415484106, 2.639326808657452039E-16 ) ) ;
#94337 = ORIENTED_EDGE ( 'NONE', *, *, #77886, .T. ) ;
#94338 = CARTESIAN_POINT ( 'NONE',  ( -2.816281873526473856, 34.12363466993042493, 9.499525473075851096E-16 ) ) ;
#94339 = CARTESIAN_POINT ( 'NONE',  ( -0.8801773607111009756, 48.06368534415484817, 1.068504757029289695E-15 ) ) ;
#94340 = ORIENTED_EDGE ( 'NONE', *, *, #36949, .T. ) ;
#94341 = CARTESIAN_POINT ( 'NONE',  ( 5.076628168052704559, 0.1755978176674514724, -8.527530157486179263 ) ) ;
#94342 = CARTESIAN_POINT ( 'NONE',  ( 19.42250999205614548, 60.98035201082151247, -5.440088680355545492 ) ) ;
#94343 = EDGE_LOOP ( 'NONE', ( #45052, #10710, #24389, #91591 ) ) ;
#94344 = CARTESIAN_POINT ( 'NONE',  ( 0.5774900079438607392, 58.48035201082151247, 5.440088680355550821 ) ) ;
#94345 = CARTESIAN_POINT ( 'NONE',  ( 4.559911319644449179, 2.230352010821504471, -9.422509992056141925 ) ) ;
#94346 = CARTESIAN_POINT ( 'NONE',  ( 2.153642693323432944, 26.13791097397318808, -6.499999999999992006 ) ) ;
#94347 = LINE ( 'NONE', #48352, #18516 ) ;
#94348 = CARTESIAN_POINT ( 'NONE',  ( 7.084665262690076126, 7.022018677488170546, -10.88017736071110164 ) ) ;
#94349 = CARTESIAN_POINT ( 'NONE',  ( 10.00000000000000000, 9.758931151000785675, -9.846743663894594434 ) ) ;
#94350 = CARTESIAN_POINT ( 'NONE',  ( 24.16423886937410614, 4.512082168247300906, -3.795296366450302550 ) ) ;
#94351 = CARTESIAN_POINT ( 'NONE',  ( 12.63842701281683922, 9.550597817667449974, -9.846743663894590881 ) ) ;
#94352 = CARTESIAN_POINT ( 'NONE',  ( -0.8801773607110991993, 7.855352010821504471, -2.915334737309923874 ) ) ;
#94353 = CARTESIAN_POINT ( 'NONE',  ( 1.472469842513823179, 41.42559781766745886, 4.923371831947296329 ) ) ;
#94354 = ORIENTED_EDGE ( 'NONE', *, *, #39176, .F. ) ;
#94355 = CARTESIAN_POINT ( 'NONE',  ( 19.84674366389459266, 53.71726448433411605, -2.638427012816827677 ) ) ;
#94356 = EDGE_LOOP ( 'NONE', ( #89196, #22036 ) ) ;
#94357 = CARTESIAN_POINT ( 'NONE',  ( 7.084665262690076126, 57.02201867748817676, -10.88017736071110164 ) ) ;
#94358 = CARTESIAN_POINT ( 'NONE',  ( 0.1532563361054100626, 45.80059781766745886, -2.638427012816831230 ) ) ;
#94360 = CARTESIAN_POINT ( 'NONE',  ( 5.991992585808519678, 15.00000000000000000, 13.20401548210297271 ) ) ;
#94359 = FILL_AREA_STYLE ('',( #54879 ) ) ;
#94361 = CARTESIAN_POINT ( 'NONE',  ( 19.42250999205614193, 55.14701867748817676, 5.440088680355555262 ) ) ;
#94362 = CARTESIAN_POINT ( 'NONE',  ( -0.3689425029237898834, 66.17874883491396076, -10.36894250292378850 ) ) ;
#94363 = EDGE_CURVE ( 'NONE', #54280, #83059, #74107, .T. ) ;
#94364 = VECTOR ( 'NONE', #41453, 1000.000000000000000 ) ;
#94365 = CARTESIAN_POINT ( 'NONE',  ( 21.09922568453594849, 46.20696800326376064, 6.408140936763242479 ) ) ;
#94366 = CARTESIAN_POINT ( 'NONE',  ( 20.15039907845753930, 70.00000000000000000, 6.262539305110068177 ) ) ;
#94367 = EDGE_CURVE ( 'NONE', #84180, #38557, #31016, .T. ) ;
#94368 = ORIENTED_EDGE ( 'NONE', *, *, #61317, .T. ) ;
#94369 = CARTESIAN_POINT ( 'NONE',  ( 22.81628187352647785, 31.62363466993042138, 6.195893100308588602E-16 ) ) ;
#94370 = CARTESIAN_POINT ( 'NONE',  ( 17.96484262340118221, 31.18868534415483751, -7.964842623401177768 ) ) ;
#94371 = ORIENTED_EDGE ( 'NONE', *, *, #47675, .F. ) ;
#94372 = CARTESIAN_POINT ( 'NONE',  ( -1.983216688680738082, -0.03417435944610275333, -14.11131997956740491 ) ) ;
#94373 = CARTESIAN_POINT ( 'NONE',  ( 19.84674366389459266, 63.71726448433412315, -2.638427012816827677 ) ) ;
#94375 = CARTESIAN_POINT ( 'NONE',  ( 1.472469842513823179, 56.42559781766745886, 4.923371831947296329 ) ) ;
#94374 = CARTESIAN_POINT ( 'NONE',  ( 7.361572987183169658, 9.967264484334119601, -9.846743663894592657 ) ) ;
#94376 = CARTESIAN_POINT ( 'NONE',  ( -8.332083457818344030, -7.290751590027323203, 3.750000000000000888 ) ) ;
#94377 = FILL_AREA_STYLE_COLOUR ( '', #74664 ) ;
#94378 = CARTESIAN_POINT ( 'NONE',  ( 0.1532563361054083140, 36.00893115100078745, 1.131784320476157264E-15 ) ) ;
#94379 = DIRECTION ( 'NONE',  ( 1.000000000000000000, 0.000000000000000000, 1.214306433183763862E-14 ) ) ;
#94380 = CARTESIAN_POINT ( 'NONE',  ( 18.95386800104995473, 58.23810908735727310, -6.499999999999988454 ) ) ;
#94381 = CARTESIAN_POINT ( 'NONE',  ( 0.1532563361054083140, 21.00893115100078745, 1.131784320476157264E-15 ) ) ;
#94382 = CARTESIAN_POINT ( 'NONE',  ( 0.000000000000000000, 14.49999999999999822, 0.000000000000000000 ) ) ;
#94384 = ORIENTED_EDGE ( 'NONE', *, *, #30368, .F. ) ;
#94383 = CARTESIAN_POINT ( 'NONE',  ( 0.1532563361054100626, 55.80059781766745175, -2.638427012816831230 ) ) ;
#94385 = AXIS2_PLACEMENT_3D ( 'NONE', #36, #30978, #30482 ) ;
#94386 = CARTESIAN_POINT ( 'NONE',  ( 6.565887622018943937, 20.16530133659708213, 12.81628187352647430 ) ) ;
#94387 = EDGE_CURVE ( 'NONE', #63343, #57472, #7056, .T. ) ;
#94388 = CARTESIAN_POINT ( 'NONE',  ( 14.92337183194729988, 39.34226448433412315, -8.527530157486177487 ) ) ;
#94389 = CARTESIAN_POINT ( 'NONE',  ( -26.67076923076924189, 87.15384615384614619, -9.500000000000000000 ) ) ;
#94390 = CARTESIAN_POINT ( 'NONE',  ( 6.204703633549690345, 47.84541550158064638, 14.16423886937410082 ) ) ;
#94391 = CARTESIAN_POINT ( 'NONE',  ( 10.00000000000000000, 19.75893115100078390, -9.846743663894594434 ) ) ;
#94392 = CIRCLE ( 'NONE', #86502, 14.49999999999999822 ) ;
#94393 = CARTESIAN_POINT ( 'NONE',  ( -13.07751017358212131, 15.00000000000000000, 6.263284095430918796 ) ) ;
#94394 = EDGE_CURVE ( 'NONE', #48509, #27622, #78906, .T. ) ;
#94395 = CARTESIAN_POINT ( 'NONE',  ( 22.26659068614894466, 48.88708216824730357, 7.082119434687054849 ) ) ;
#94396 = CARTESIAN_POINT ( 'NONE',  ( 2.791683348922237240, 55.38393115100078745, -7.208316651077763204 ) ) ;
#94397 = CARTESIAN_POINT ( 'NONE',  ( 10.00000000000000000, 6.813685344154838397, -10.88017736071110342 ) ) ;
#94398 = CARTESIAN_POINT ( 'NONE',  ( 13.79529636645030344, 38.26208216824729647, 14.16423886937410614 ) ) ;
#94399 = CARTESIAN_POINT ( 'NONE',  ( -4.164238869374099927, 37.01208216824731068, 3.795296366450308767 ) ) ;
#94400 = SURFACE_STYLE_USAGE ( .BOTH. , #63888 ) ;
#94401 = B_SPLINE_CURVE_WITH_KNOTS ( 'NONE', 3,
 ( #28658, #5679, #66665, #36667, #97190, #6653 ),
 .UNSPECIFIED., .F., .F.,
 ( 4, 2, 4 ),
 ( 3.409110551495797298E-05, 0.0004400426677367831022, 0.0008459942299586082314 ),
 .UNSPECIFIED. ) ;
#94402 = COLOUR_RGB ( '', 0.09019608, 0.27058824, 0.51372549) ;
#94404 = CARTESIAN_POINT ( 'NONE',  ( 7.361572987183170547, 57.05059781766744464, 9.846743663894590881 ) ) ;
#94403 = CARTESIAN_POINT ( 'NONE',  ( -13.59972906620404487, 0.04962881387626322943, 5.718800721548481292 ) ) ;
#94405 = ORIENTED_EDGE ( 'NONE', *, *, #54300, .T. ) ;
#94406 = CARTESIAN_POINT ( 'NONE',  ( 12.91533473730992121, 34.52201867748817676, 10.88017736071110164 ) ) ;
#94407 = CARTESIAN_POINT ( 'NONE',  ( -12.21130863673195499, -2.649095542537823522E-15, -8.049375889233145287 ) ) ;
#94408 = CARTESIAN_POINT ( 'NONE',  ( 19.50000000000000355, 98.59912998021083297, -5.000000000000000000 ) ) ;
#94409 = DIRECTION ( 'NONE',  ( -1.000000000000000000, 0.000000000000000000, 0.000000000000000000 ) ) ;
#94410 = CARTESIAN_POINT ( 'NONE',  ( -7.082119434687058401, 5.970415501580637496, -12.26659068614894110 ) ) ;
#94411 = CARTESIAN_POINT ( 'NONE',  ( 19.84674366389459621, 53.50893115100078745, 7.409399052514197653E-17 ) ) ;
#94412 = CARTESIAN_POINT ( 'NONE',  ( 17.20831665107776587, 64.13393115100079456, -7.208316651077762316 ) ) ;
#94413 = ORIENTED_EDGE ( 'NONE', *, *, #22911, .F. ) ;
#94414 = CARTESIAN_POINT ( 'NONE',  ( -4.164238869374098151, 31.59541550158063927, -3.795296366450310543 ) ) ;
#94415 = PLANE ( 'NONE',  #19870 ) ;
#94416 = CARTESIAN_POINT ( 'NONE',  ( -6.606690058690507961, -50.93246948815529151, -2.750000000000000000 ) ) ;
#94417 = CARTESIAN_POINT ( 'NONE',  ( 15.44008868035555260, 9.730352010821505360, 9.422509992056143702 ) ) ;
#94418 = CARTESIAN_POINT ( 'NONE',  ( 22.81628187352648496, 21.83196800326374643, -3.434112377981050290 ) ) ;
#94419 = CARTESIAN_POINT ( 'NONE',  ( 11.10175276307597336, 14.95037105032437807, -9.716398248524681591 ) ) ;
#94420 = CARTESIAN_POINT ( 'NONE',  ( 17.20831665107776587, 17.88393115100078745, 7.208316651077764980 ) ) ;
#94421 = CARTESIAN_POINT ( 'NONE',  ( 10.27191093752563411, 9.181837148236613703E-16, -10.41278984915626360 ) ) ;
#94422 = CARTESIAN_POINT ( 'NONE',  ( -46.94000000000001194, 100.4344880109628093, -9.014049137172644777 ) ) ;
#94423 = CARTESIAN_POINT ( 'NONE',  ( 6.000000000000000000, 60.50000000000000000, -5.000000000000000000 ) ) ;
#94424 = CARTESIAN_POINT ( 'NONE',  ( 17.96484262340118221, 16.18868534415483396, -7.964842623401177768 ) ) ;
#94425 = CYLINDRICAL_SURFACE ( 'NONE', #60645, 0.5000000000000004441 ) ;
#94426 = CARTESIAN_POINT ( 'NONE',  ( 3.420591144908446957, 0.5000000000000004441, 14.60477854057958425 ) ) ;
#94427 = CARTESIAN_POINT ( 'NONE',  ( -0.8801773607110991993, 42.85535201082150536, -2.915334737309923874 ) ) ;
#94428 = CARTESIAN_POINT ( 'NONE',  ( 7.084665262690076126, 42.02201867748816966, -10.88017736071110164 ) ) ;
#94429 = CARTESIAN_POINT ( 'NONE',  ( 13.43411237798105340, 5.581968003263753531, 12.81628187352647963 ) ) ;
#94430 = CARTESIAN_POINT ( 'NONE',  ( 10.00000000000000178, 67.25893115100079456, 9.846743663894594434 ) ) ;
#94431 = CARTESIAN_POINT ( 'NONE',  ( -45.93038741018368398, 104.4960312484300999, -5.681613179053518259 ) ) ;
#94432 = CARTESIAN_POINT ( 'NONE',  ( 10.00000000000000000, 14.75893115100078568, -9.846743663894594434 ) ) ;
#94433 = VERTEX_POINT ( 'NONE', #1714 ) ;
#94434 = TOROIDAL_SURFACE ( 'NONE', #51327, 4.190000000000001279, 0.2500000000000000000 ) ;
#94435 = CARTESIAN_POINT ( 'NONE',  ( 12.91533473730992121, 34.52201867748817676, 10.88017736071110164 ) ) ;
#94436 = ADVANCED_FACE ( 'NONE', ( #62674 ), #72473, .T. ) ;
#94437 = CARTESIAN_POINT ( 'NONE',  ( -1.099225684535947600, 28.70696800326375353, -6.408140936763238038 ) ) ;
#94438 = B_SPLINE_CURVE_WITH_KNOTS ( 'NONE', 3,
 ( #35755, #65749, #66242, #28253, #20762, #51252, #43745, #5764, #21256, #54200 ),
 .UNSPECIFIED., .F., .F.,
 ( 4, 3, 3, 4 ),
 ( 0.000000000000000000, 0.0006253016069561002704, 0.001250604074564923892, 0.002501455912506560415 ),
 .UNSPECIFIED. ) ;
#94439 = CIRCLE ( 'NONE', #268, 0.2500000000000002220 ) ;
#94440 = CARTESIAN_POINT ( 'NONE',  ( 2.791683348922237240, 65.38393115100078035, -7.208316651077763204 ) ) ;
#94441 = CARTESIAN_POINT ( 'NONE',  ( 0.5774900079438607392, 68.48035201082150536, 5.440088680355550821 ) ) ;
#94442 = CARTESIAN_POINT ( 'NONE',  ( 7.361572987183169658, 14.96726448433411960, -9.846743663894592657 ) ) ;
#94443 = CARTESIAN_POINT ( 'NONE',  ( 13.43411237798105340, 35.58196800326375353, 12.81628187352647963 ) ) ;
#94444 = CARTESIAN_POINT ( 'NONE',  ( 5.076628168052703671, 11.84226448433411960, 8.527530157486179263 ) ) ;
#94445 = ORIENTED_EDGE ( 'NONE', *, *, #18998, .T. ) ;
#94446 = CARTESIAN_POINT ( 'NONE',  ( -4.000000000000000000, 10.00000000000000000, 3.750000000000000000 ) ) ;
#94447 =( NAMED_UNIT ( * ) SI_UNIT ( $, .STERADIAN. ) SOLID_ANGLE_UNIT ( ) );
#94448 = CARTESIAN_POINT ( 'NONE',  ( 4.559911319644449179, 7.230352010821504471, -9.422509992056141925 ) ) ;
#94449 = CARTESIAN_POINT ( 'NONE',  ( 10.00000000000000178, 55.37363466993042493, 12.81628187352647608 ) ) ;
#94450 = CARTESIAN_POINT ( 'NONE',  ( 0.1532563361054082862, 11.21726448433411605, 2.638427012816831674 ) ) ;
#94451 = CARTESIAN_POINT ( 'NONE',  ( 18.52753015748618282, 18.92559781766745175, -4.923371831947291888 ) ) ;
#94452 = CARTESIAN_POINT ( 'NONE',  ( 13.79529636645030344, 58.26208216824728936, 14.16423886937410614 ) ) ;
#94453 = VERTEX_POINT ( 'NONE', #25687 ) ;
#94454 = CARTESIAN_POINT ( 'NONE',  ( 12.91533473730992121, 19.52201867748816611, 10.88017736071110164 ) ) ;
#94455 = CARTESIAN_POINT ( 'NONE',  ( 12.91533473730992121, 24.52201867748816966, 10.88017736071110164 ) ) ;
#94456 = DIRECTION ( 'NONE',  ( -1.000000000000000000, 0.000000000000000000, 0.000000000000000000 ) ) ;
#94457 = AXIS2_PLACEMENT_3D ( 'NONE', #32568, #95033, #70091 ) ;
#94458 = VERTEX_POINT ( 'NONE', #39708 ) ;
#94459 = CARTESIAN_POINT ( 'NONE',  ( 6.898461952320324109, 15.00000000000000000, 12.75387089053312373 ) ) ;
#94460 = CARTESIAN_POINT ( 'NONE',  ( 10.00000000000000000, 26.81368534415484106, -10.88017736071110342 ) ) ;
#94462 = VECTOR ( 'NONE', #83818, 1000.000000000000000 ) ;
#94461 = CARTESIAN_POINT ( 'NONE',  ( 2.791683348922240793, 61.63393115100079456, 7.208316651077764092 ) ) ;
#94463 = LINE ( 'NONE', #34439, #63300 ) ;
#94464 = CARTESIAN_POINT ( 'NONE',  ( 21.09922568453594849, 46.20696800326376064, 6.408140936763242479 ) ) ;
#94465 = CARTESIAN_POINT ( 'NONE',  ( -0.3289641300568005855, 4.271642702460841434, -5.963430220938281678 ) ) ;
#94466 = CARTESIAN_POINT ( 'NONE',  ( 17.08211943468705840, 25.13708216824730357, -12.26659068614894466 ) ) ;
#94467 = CARTESIAN_POINT ( 'NONE',  ( 4.559911319644449179, 38.89701867748817676, 9.422509992056141925 ) ) ;
#94468 = CARTESIAN_POINT ( 'NONE',  ( 0.5774900079438590739, 17.64701867748817321, -5.440088680355550821 ) ) ;
#94469 = CARTESIAN_POINT ( 'NONE',  ( 17.20831665107776587, 49.13393115100078745, -7.208316651077762316 ) ) ;
#94470 = DIRECTION ( 'NONE',  ( 0.000000000000000000, 0.000000000000000000, -1.000000000000000000 ) ) ;
#94472 = EDGE_CURVE ( 'NONE', #33681, #87486, #49156, .T. ) ;
#94471 = CARTESIAN_POINT ( 'NONE',  ( 7.361572987183169658, 34.96726448433411605, -9.846743663894592657 ) ) ;
#94473 = DIRECTION ( 'NONE',  ( -0.000000000000000000, -1.000000000000000000, -0.000000000000000000 ) ) ;
#94474 = CARTESIAN_POINT ( 'NONE',  ( 12.63842701281683034, 12.46726448433411782, 9.846743663894596210 ) ) ;
#94475 = CARTESIAN_POINT ( 'NONE',  ( 12.81628187352647608, -38.37636533006957507, -2.602085213965210642E-15 ) ) ;
#94476 = ORIENTED_EDGE ( 'NONE', *, *, #75080, .T. ) ;
#94477 = VECTOR ( 'NONE', #46557, 1000.000000000000000 ) ;
#94478 = CARTESIAN_POINT ( 'NONE',  ( 7.084665262690076126, 9.105352010821503583, 10.88017736071109987 ) ) ;
#94479 = CARTESIAN_POINT ( 'NONE',  ( 0.1532563361054083140, 16.00893115100078390, 1.131784320476157264E-15 ) ) ;
#94480 = CARTESIAN_POINT ( 'NONE',  ( -0.8801773607110991993, 47.85535201082150536, -2.915334737309923874 ) ) ;
#94482 = CARTESIAN_POINT ( 'NONE',  ( 3.591859063236761518, 49.95696800326375353, 11.09922568453594849 ) ) ;
#94481 = CARTESIAN_POINT ( 'NONE',  ( 20.88017736071110519, 25.56368534415483751, 2.639326808657452039E-16 ) ) ;
#94483 = CARTESIAN_POINT ( 'NONE',  ( 6.204703633549690345, 35.76208216824729647, -14.16423886937410259 ) ) ;
#94484 = LINE ( 'NONE', #94974, #92189 ) ;
#94485 = EDGE_CURVE ( 'NONE', #25245, #38271, #32171, .T. ) ;
#94486 = CARTESIAN_POINT ( 'NONE',  ( 13.43411237798106583, 62.66530133659708923, -12.81628187352647252 ) ) ;
#94487 = EDGE_CURVE ( 'NONE', #7185, #20454, #24614, .T. ) ;
#94488 = VERTEX_POINT ( 'NONE', #79659 ) ;
#94489 = CARTESIAN_POINT ( 'NONE',  ( 5.076628168052704559, 55.17559781766745175, -8.527530157486179263 ) ) ;
#94490 = CARTESIAN_POINT ( 'NONE',  ( 20.88017736071110164, 40.35535201082150536, 2.915334737309930979 ) ) ;
#94491 = ORIENTED_EDGE ( 'NONE', *, *, #58344, .T. ) ;
#94493 = LINE ( 'NONE', #26013, #68729 ) ;
#94492 = CARTESIAN_POINT ( 'NONE',  ( 18.52753015748618282, 3.925597817667451306, -4.923371831947291888 ) ) ;
#94494 = CARTESIAN_POINT ( 'NONE',  ( 3.195792623639591490, 6.146642702460846763, 11.92686044187652961 ) ) ;
#94495 = CARTESIAN_POINT ( 'NONE',  ( 14.92337183194729988, 24.34226448433411960, -8.527530157486177487 ) ) ;
#94496 = CARTESIAN_POINT ( 'NONE',  ( 1.472469842513823179, 10.59226448433411782, -4.923371831947296329 ) ) ;
#94497 = CARTESIAN_POINT ( 'NONE',  ( 0.1532563361054082862, 6.217264484334118713, 2.638427012816831674 ) ) ;
#94499 = CARTESIAN_POINT ( 'NONE',  ( 5.302565485995492267, 0.000000000000000000, -1.273033341818833541 ) ) ;
#94498 = CARTESIAN_POINT ( 'NONE',  ( -0.8801773607110991993, 52.85535201082151247, -2.915334737309923874 ) ) ;
#94500 = CARTESIAN_POINT ( 'NONE',  ( 7.084665262690076126, 57.02201867748817676, -10.88017736071110164 ) ) ;
#94502 = ORIENTED_EDGE ( 'NONE', *, *, #14029, .F. ) ;
#94501 = CARTESIAN_POINT ( 'NONE',  ( 17.20831665107776587, 17.88393115100078745, 7.208316651077764980 ) ) ;
#94503 = AXIS2_PLACEMENT_3D ( 'NONE', #2760, #33213, #74158 ) ;
#94504 = CARTESIAN_POINT ( 'NONE',  ( 14.62617646268085281, 0.5000000000000004441, 3.327906561566980503 ) ) ;
#94505 = CARTESIAN_POINT ( 'NONE',  ( 1.472469842513823179, 51.42559781766745886, 4.923371831947296329 ) ) ;
#94506 = ORIENTED_EDGE ( 'NONE', *, *, #25455, .F. ) ;
#94507 = ORIENTED_EDGE ( 'NONE', *, *, #70442, .T. ) ;
#94508 = FACE_OUTER_BOUND ( 'NONE', #58884, .T. ) ;
#94509 = CARTESIAN_POINT ( 'NONE',  ( 24.16423886937409904, 4.095415501580634832, 3.795296366450317205 ) ) ;
#94510 = UNCERTAINTY_MEASURE_WITH_UNIT (LENGTH_MEASURE( 1.000000000000000082E-05 ), #13087, 'distance_accuracy_value', 'NONE');
#94511 = CARTESIAN_POINT ( 'NONE',  ( 22.81628187352648496, 61.83196800326376774, -3.434112377981050290 ) ) ;
#94512 = ADVANCED_FACE ( 'NONE', ( #11155 ), #86672, .F. ) ;
#94513 = CARTESIAN_POINT ( 'NONE',  ( -2.266590686148945544, 2.220415501580634388, 7.082119434687048631 ) ) ;
#94514 = CARTESIAN_POINT ( 'NONE',  ( 10.00000000000000178, 33.05374883491396787, 14.16423886937410082 ) ) ;
#94515 = DIRECTION ( 'NONE',  ( 0.000000000000000000, 0.000000000000000000, -1.000000000000000000 ) ) ;
#94516 = CARTESIAN_POINT ( 'NONE',  ( 6.204703633549690345, 0.7620821682473009062, -14.16423886937410259 ) ) ;
#94517 = CARTESIAN_POINT ( 'NONE',  ( 2.035157376598824452, 38.68868534415483396, 7.964842623401179544 ) ) ;
#94518 = SURFACE_STYLE_FILL_AREA ( #34000 ) ;
#94519 = ORIENTED_EDGE ( 'NONE', *, *, #65112, .F. ) ;
#94520 = CARTESIAN_POINT ( 'NONE',  ( 14.92337183194729988, 14.34226448433411782, -8.527530157486177487 ) ) ;
#94522 = CARTESIAN_POINT ( 'NONE',  ( 17.20831665107776587, 17.88393115100078745, 7.208316651077764980 ) ) ;
#94521 = CARTESIAN_POINT ( 'NONE',  ( 12.91533473730993009, 56.60535201082151247, -10.88017736071109987 ) ) ;
#94523 = CARTESIAN_POINT ( 'NONE',  ( 0.6178305044545838731, 44.74863466993042493, 9.382169495545420901 ) ) ;
#94524 = CARTESIAN_POINT ( 'NONE',  ( 5.076628168052703671, 36.84226448433412315, 8.527530157486179263 ) ) ;
#94525 = CARTESIAN_POINT ( 'NONE',  ( 8.439016546559892973, 15.00000000000000000, -11.79122553964970876 ) ) ;
#94526 = CARTESIAN_POINT ( 'NONE',  ( 17.96484262340118221, 59.93868534415484106, 7.964842623401181321 ) ) ;
#94527 = CARTESIAN_POINT ( 'NONE',  ( 13.43411237798105340, 25.58196800326374998, 12.81628187352647963 ) ) ;
#94528 = CARTESIAN_POINT ( 'NONE',  ( -7.082119434687044190, -37.36291783175269643, 12.26659068614894998 ) ) ;
#94529 = VECTOR ( 'NONE', #26247, 1000.000000000000000 ) ;
#94530 = CARTESIAN_POINT ( 'NONE',  ( 18.52753015748617571, 23.09226448433411960, 4.923371831947298993 ) ) ;
#94531 = CARTESIAN_POINT ( 'NONE',  ( 2.917880565312950480, 10.97041550158063572, -12.26659068614894821 ) ) ;
#94532 = ORIENTED_EDGE ( 'NONE', *, *, #85438, .T. ) ;
#94533 = CARTESIAN_POINT ( 'NONE',  ( 7.084665262690076126, 37.02201867748817676, -10.88017736071110164 ) ) ;
#94534 = CARTESIAN_POINT ( 'NONE',  ( 6.204703633549690345, 30.76208216824730357, -14.16423886937410259 ) ) ;
#94535 = CARTESIAN_POINT ( 'NONE',  ( 7.361572987183169658, 54.96726448433413026, -9.846743663894592657 ) ) ;
#94536 = CARTESIAN_POINT ( 'NONE',  ( 12.63842701281683034, 7.467264484334118713, 9.846743663894596210 ) ) ;
#94537 = AXIS2_PLACEMENT_3D ( 'NONE', #23593, #30068, #54057 ) ;
#94539 = PLANE ( 'NONE',  #12922 ) ;
#94538 = CARTESIAN_POINT ( 'NONE',  ( 0.6178305044545838731, 54.74863466993042493, 9.382169495545420901 ) ) ;
#94540 = CARTESIAN_POINT ( 'NONE',  ( 12.91533473730992121, 44.52201867748816966, 10.88017736071110164 ) ) ;
#94541 = SURFACE_SIDE_STYLE ('',( #70574 ) ) ;
#94542 = CARTESIAN_POINT ( 'NONE',  ( 10.00000000000000000, 17.87363466993041783, -12.81628187352647608 ) ) ;
#94543 = CARTESIAN_POINT ( 'NONE',  ( 19.84674366389459266, 48.30059781766745175, 2.638427012816836559 ) ) ;
#94544 = CARTESIAN_POINT ( 'NONE',  ( 9.422509992056141925, 10.98035201082150891, -5.440088680355554374 ) ) ;
#94545 = CARTESIAN_POINT ( 'NONE',  ( 2.035157376598822676, 2.438685344154837953, -7.964842623401177768 ) ) ;
#94546 = CIRCLE ( 'NONE', #37107, 2.899999999999999911 ) ;
#94548 = CARTESIAN_POINT ( 'NONE',  ( -8.000000000000000000, 75.73428692542562146, 2.900000000000000355 ) ) ;
#94547 = CARTESIAN_POINT ( 'NONE',  ( 0.1922240491738545221, 13.18878173731740766, 6.500000000000007105 ) ) ;
#94549 = CYLINDRICAL_SURFACE ( 'NONE', #91249, 15.00000000000000000 ) ;
#94550 = EDGE_CURVE ( 'NONE', #8774, #95706, #60059, .T. ) ;
#94551 = FACE_OUTER_BOUND ( 'NONE', #92406, .T. ) ;
#94552 = CARTESIAN_POINT ( 'NONE',  ( 17.96484262340118221, 56.18868534415484817, -7.964842623401177768 ) ) ;
#94553 = CARTESIAN_POINT ( 'NONE',  ( 17.96484262340118221, 51.18868534415483396, -7.964842623401177768 ) ) ;
#94554 = CARTESIAN_POINT ( 'NONE',  ( 15.61289147378509057, 15.00000000000000000, 3.480663193108788800 ) ) ;
#94555 = DIRECTION ( 'NONE',  ( 0.08715574274765151841, 0.9961946980917462113, 0.000000000000000000 ) ) ;
#94556 = CARTESIAN_POINT ( 'NONE',  ( 7.361572987183169658, 19.96726448433411960, -9.846743663894592657 ) ) ;
#94557 = CARTESIAN_POINT ( 'NONE',  ( 12.91533473730992121, 19.52201867748816611, 10.88017736071110164 ) ) ;
#94558 = CARTESIAN_POINT ( 'NONE',  ( -2.816281873526473856, -0.6680319967362464695, 3.434112377981055619 ) ) ;
#94560 = CARTESIAN_POINT ( 'NONE',  ( -7.037775641161837292, -86.26045154785950331, -3.750000000000000444 ) ) ;
#94559 = CARTESIAN_POINT ( 'NONE',  ( 10.00000000000000178, 19.31368534415484106, 10.88017736071110342 ) ) ;
#94561 = DIRECTION ( 'NONE',  ( -0.000000000000000000, 0.000000000000000000, 1.000000000000000000 ) ) ;
#94562 = CARTESIAN_POINT ( 'NONE',  ( 21.09922568453594849, 26.20696800326375353, 6.408140936763242479 ) ) ;
#94563 = VERTEX_POINT ( 'NONE', #10672 ) ;
#94564 = CARTESIAN_POINT ( 'NONE',  ( 7.084665262690076126, 54.10535201082151247, 10.88017736071109987 ) ) ;
#94565 = CARTESIAN_POINT ( 'NONE',  ( 5.076628168052703671, 46.84226448433412315, 8.527530157486179263 ) ) ;
#94566 = CARTESIAN_POINT ( 'NONE',  ( 21.09922568453594849, 26.20696800326375353, 6.408140936763242479 ) ) ;
#94567 = CARTESIAN_POINT ( 'NONE',  ( 19.42250999205614193, 25.14701867748817321, 5.440088680355555262 ) ) ;
#94568 = CARTESIAN_POINT ( 'NONE',  ( 20.36894250292379382, 48.67874883491396076, 10.36894250292379205 ) ) ;
#94569 = CARTESIAN_POINT ( 'NONE',  ( 18.52753015748617571, 43.09226448433412315, 4.923371831947298993 ) ) ;
#94570 = CARTESIAN_POINT ( 'NONE',  ( 10.00000000000000178, 69.31368534415484817, 10.88017736071110342 ) ) ;
#94571 = CARTESIAN_POINT ( 'NONE',  ( 20.88017736071110875, 50.77201867748817676, -2.915334737309920765 ) ) ;
#94572 = DIRECTION ( 'NONE',  ( 0.2334453638559156052, 0.000000000000000000, -0.9723699203976741146 ) ) ;
#94573 = CARTESIAN_POINT ( 'NONE',  ( 20.36894250292379738, 19.92874883491396787, -10.36894250292379027 ) ) ;
#94574 = ADVANCED_FACE ( 'NONE', ( #71667 ), #33642, .F. ) ;
#94575 = SURFACE_STYLE_FILL_AREA ( #41107 ) ;
#94576 = LINE ( 'NONE', #40108, #66319 ) ;
#94577 = ORIENTED_EDGE ( 'NONE', *, *, #88643, .F. ) ;
#94578 = ORIENTED_EDGE ( 'NONE', *, *, #1966, .F. ) ;
#94579 = AXIS2_PLACEMENT_3D ( 'NONE', #2907, #48373, #26853 ) ;
#94580 = CARTESIAN_POINT ( 'NONE',  ( 6.204703633549690345, 50.76208216824730357, -14.16423886937410259 ) ) ;
#94581 = CARTESIAN_POINT ( 'NONE',  ( 24.16423886937409904, 49.09541550158063217, 3.795296366450317205 ) ) ;
#94582 = CARTESIAN_POINT ( 'NONE',  ( 17.20831665107776587, 17.88393115100078745, 7.208316651077764980 ) ) ;
#94583 = CARTESIAN_POINT ( 'NONE',  ( 19.38216949554541557, 17.24863466993041783, -9.382169495545420901 ) ) ;
#94584 = CARTESIAN_POINT ( 'NONE',  ( -46.44000000000001194, 103.0000000000000000, 5.997726559847112782 ) ) ;
#94585 = CARTESIAN_POINT ( 'NONE',  ( 17.39651004071841456, 9.082109641433294911, -6.500000000000003553 ) ) ;
#94587 = CARTESIAN_POINT ( 'NONE',  ( 0.6178305044545838731, 29.74863466993042138, 9.382169495545420901 ) ) ;
#94586 = CARTESIAN_POINT ( 'NONE',  ( -0.8801773607111009756, 68.06368534415484817, 1.068504757029289695E-15 ) ) ;
#94588 = CARTESIAN_POINT ( 'NONE',  ( 6.204703633549690345, 47.84541550158064638, 14.16423886937410082 ) ) ;
#94589 = B_SPLINE_CURVE_WITH_KNOTS ( 'NONE', 3,
 ( #94126, #86640, #24666, #79125, #10637, #3146 ),
 .UNSPECIFIED., .F., .F.,
 ( 4, 2, 4 ),
 ( 0.000000000000000000, 0.0002605067024380841828, 0.0005210134048761683656 ),
 .UNSPECIFIED. ) ;
#94590 =( NAMED_UNIT ( * ) PLANE_ANGLE_UNIT ( ) SI_UNIT ( $, .RADIAN. ) );
#94591 = CARTESIAN_POINT ( 'NONE',  ( 19.42250999205614548, 65.98035201082151957, -5.440088680355545492 ) ) ;
#94592 = CARTESIAN_POINT ( 'NONE',  ( -8.527530157486182816, 5.592264484334121377, -4.923371831947288335 ) ) ;
#94593 = ORIENTED_EDGE ( 'NONE', *, *, #98248, .T. ) ;
#94594 = DIRECTION ( 'NONE',  ( -0.5547001962252290364, -0.8320502943378437211, 0.000000000000000000 ) ) ;
#94595 = CARTESIAN_POINT ( 'NONE',  ( 0.1532563361054100626, 15.80059781766745353, -2.638427012816831230 ) ) ;
#94597 = EDGE_CURVE ( 'NONE', #58863, #1208, #27713, .T. ) ;
#94596 = CARTESIAN_POINT ( 'NONE',  ( 20.15039907845753930, 70.00000000000000000, -6.262539305110068177 ) ) ;
#94598 = ORIENTED_EDGE ( 'NONE', *, *, #18765, .T. ) ;
#94600 = CARTESIAN_POINT ( 'NONE',  ( 15.44008868035555793, 16.39701867748817321, -9.422509992056140149 ) ) ;
#94599 = CARTESIAN_POINT ( 'NONE',  ( -0.3689425029237881626, 67.42874883491396076, 10.36894250292379027 ) ) ;
#94602 = CARTESIAN_POINT ( 'NONE',  ( 0.6178305044545818747, -1.501365330069579951, -9.382169495545419124 ) ) ;
#94601 = CARTESIAN_POINT ( 'NONE',  ( 0.1532563361054082862, 51.21726448433412315, 2.638427012816831674 ) ) ;
#94603 = CARTESIAN_POINT ( 'NONE',  ( -9.876730923139412255, 14.63606899087332636, 11.28938378619058547 ) ) ;
#94604 = AXIS2_PLACEMENT_3D ( 'NONE', #81596, #74596, #90579 ) ;
#94605 = EDGE_CURVE ( 'NONE', #27759, #56243, #85198, .T. ) ;
#94606 = CARTESIAN_POINT ( 'NONE',  ( 3.591859063236763294, 23.29030133659708568, -11.09922568453595026 ) ) ;
#94607 = EDGE_CURVE ( 'NONE', #48119, #79733, #15202, .T. ) ;
#94608 = ORIENTED_EDGE ( 'NONE', *, *, #84928, .T. ) ;
#94609 = STYLED_ITEM ( 'NONE', ( #95229 ), #24342 ) ;
#94610 = CARTESIAN_POINT ( 'NONE',  ( 2.917880565312950480, 60.97041550158063927, -12.26659068614894821 ) ) ;
#94611 = ORIENTED_EDGE ( 'NONE', *, *, #38673, .T. ) ;
#94612 = AXIS2_PLACEMENT_3D ( 'NONE', #16904, #54387, #84899 ) ;
#94613 = CARTESIAN_POINT ( 'NONE',  ( 22.26659068614895176, 59.72041550158063927, -7.082119434687042414 ) ) ;
#94614 = ORIENTED_EDGE ( 'NONE', *, *, #94239, .F. ) ;
#94615 = CARTESIAN_POINT ( 'NONE',  ( -0.8801773607110991993, 27.85535201082150181, -2.915334737309923874 ) ) ;
#94616 = CARTESIAN_POINT ( 'NONE',  ( 19.42250999205614193, 35.14701867748816966, 5.440088680355555262 ) ) ;
#94617 = B_SPLINE_CURVE_WITH_KNOTS ( 'NONE', 3,
 ( #7233, #740, #22734, #37740, #85197, #38715 ),
 .UNSPECIFIED., .F., .F.,
 ( 4, 2, 4 ),
 ( 1.608716371138911572E-17, 0.0002605067024381052163, 0.0005210134048761942780 ),
 .UNSPECIFIED. ) ;
#94618 = MECHANICAL_DESIGN_GEOMETRIC_PRESENTATION_REPRESENTATION (  '', ( #2081 ), #32371 ) ;
#94619 = CARTESIAN_POINT ( 'NONE',  ( 20.15039907845753930, 5.601585745166425490, -6.262539305110069954 ) ) ;
#94620 = CARTESIAN_POINT ( 'NONE',  ( 2.035157376598824452, 23.68868534415484461, 7.964842623401179544 ) ) ;
#94621 = PRESENTATION_LAYER_ASSIGNMENT (  '', '', ( #11545 ) ) ;
#94622 = DIRECTION ( 'NONE',  ( 0.000000000000000000, 0.000000000000000000, 1.000000000000000000 ) ) ;
#94623 = CARTESIAN_POINT ( 'NONE',  ( 0.1532563361054100626, 10.80059781766745175, -2.638427012816831230 ) ) ;
#94624 = CARTESIAN_POINT ( 'NONE',  ( -3.521047174887395048, -6.414748048906915301, 2.500000000000000888 ) ) ;
#94625 = ORIENTED_EDGE ( 'NONE', *, *, #37970, .T. ) ;
#94626 = CARTESIAN_POINT ( 'NONE',  ( 10.34946471139303092, -32.01331896743604233, 4.000000000000000000 ) ) ;
#94627 = CARTESIAN_POINT ( 'NONE',  ( 1.472469842513823179, 50.59226448433411605, -4.923371831947296329 ) ) ;
#94628 = CARTESIAN_POINT ( 'NONE',  ( 17.85158348494336522, 9.737265733804411738, -6.499999999999984901 ) ) ;
#94629 = EDGE_CURVE ( 'NONE', #91827, #80133, #34628, .T. ) ;
#94630 = CIRCLE ( 'NONE', #75440, 2.500000000000002220 ) ;
#94631 = CARTESIAN_POINT ( 'NONE',  ( 10.14667048435145169, 15.00000000000000000, -10.35833375027041292 ) ) ;
#94632 = ORIENTED_EDGE ( 'NONE', *, *, #98665, .F. ) ;
#94633 = DIRECTION ( 'NONE',  ( 0.000000000000000000, 1.000000000000000000, -0.000000000000000000 ) ) ;
#94634 = CARTESIAN_POINT ( 'NONE',  ( 8.157527544166429223, 0.2301507453079258969, 12.51706795611453593 ) ) ;
#94635 = CARTESIAN_POINT ( 'NONE',  ( 19.84674366389459266, 63.71726448433412315, -2.638427012816827677 ) ) ;
#94636 = CARTESIAN_POINT ( 'NONE',  ( 17.08211943468705840, 50.13708216824730357, -12.26659068614894466 ) ) ;
#94637 = DIRECTION ( 'NONE',  ( -0.5150380749100542666, 1.049727191138618572E-16, -0.8571673007021122226 ) ) ;
#94638 = ORIENTED_EDGE ( 'NONE', *, *, #59300, .F. ) ;
#94639 = LINE ( 'NONE', #19135, #19281 ) ;
#94640 = CARTESIAN_POINT ( 'NONE',  ( 17.20831665107776587, 39.13393115100079456, -7.208316651077762316 ) ) ;
#94641 = CARTESIAN_POINT ( 'NONE',  ( 21.09922568453594849, 61.20696800326376064, 6.408140936763242479 ) ) ;
#94642 = CARTESIAN_POINT ( 'NONE',  ( -1.099225684535947600, 9.540301336597087456, 6.408140936763237150 ) ) ;
#94643 = CARTESIAN_POINT ( 'NONE',  ( 10.00000000000000178, 64.31368534415483396, 10.88017736071110342 ) ) ;
#94644 = DIRECTION ( 'NONE',  ( 0.000000000000000000, -1.000000000000000000, 0.000000000000000000 ) ) ;
#94645 = CARTESIAN_POINT ( 'NONE',  ( 17.20831665107776587, 57.88393115100078745, 7.208316651077764980 ) ) ;
#94646 = EDGE_CURVE ( 'NONE', #57472, #295, #23051, .T. ) ;
#94647 = CARTESIAN_POINT ( 'NONE',  ( -45.94000000000000483, 92.00000000000000000, 9.000000000000000000 ) ) ;
#94648 = ORIENTED_EDGE ( 'NONE', *, *, #65647, .F. ) ;
#94649 =( BOUNDED_CURVE ( )  B_SPLINE_CURVE ( 2, ( #85554, #77541, #613, #83584, #84571, #69568, #9059, #23094, #31057 ),
 .UNSPECIFIED., .F., .F. ) 
 B_SPLINE_CURVE_WITH_KNOTS ( ( 3, 2, 2, 2, 3 ),
 ( 0.9382284501891250406, 0.9404761904761904656, 0.9464285714285713969, 0.9523809523809523281, 0.9546286926680177531 ),
 .UNSPECIFIED. ) 
 CURVE ( )  GEOMETRIC_REPRESENTATION_ITEM ( )  RATIONAL_B_SPLINE_CURVE ( ( 0.9839835555609424134, 0.9871328979762474809, 1.000000000000000000, 0.9659258262890683122, 1.000000000000000000, 0.9659258262890683122, 1.000000000000000000, 0.9871328979762477029, 0.9839835555609425244 ) ) 
 REPRESENTATION_ITEM ( '' )  );
#94650 = CARTESIAN_POINT ( 'NONE',  ( -2.266590686148945544, 62.22041550158063927, 7.082119434687048631 ) ) ;
#94651 = FACE_OUTER_BOUND ( 'NONE', #68191, .T. ) ;
#94652 = CARTESIAN_POINT ( 'NONE',  ( 15.44008868035555260, 44.73035201082151247, 9.422509992056143702 ) ) ;
#94654 = CARTESIAN_POINT ( 'NONE',  ( 2.035157376598824452, 68.68868534415484817, 7.964842623401179544 ) ) ;
#94653 = CARTESIAN_POINT ( 'NONE',  ( -2.816281873526471635, 18.91530133659708213, -3.434112377981056508 ) ) ;
#94655 = CARTESIAN_POINT ( 'NONE',  ( 4.559911319644449179, 7.230352010821504471, -9.422509992056141925 ) ) ;
#94656 = CARTESIAN_POINT ( 'NONE',  ( 13.61464873478162829, 14.49999999999999822, 6.296136897217933459 ) ) ;
#94657 = CARTESIAN_POINT ( 'NONE',  ( 17.39651004071897589, 34.08210964143323451, -6.499999999999361400 ) ) ;
#94658 = CARTESIAN_POINT ( 'NONE',  ( 14.92337183194729633, 57.67559781766745886, 8.527530157486181039 ) ) ;
#94659 = CARTESIAN_POINT ( 'NONE',  ( 15.64039516285221154, 89.00000000000000000, -9.500000000000000000 ) ) ;
#94660 = CARTESIAN_POINT ( 'NONE',  ( -2.915334737309934532, -37.97798132251182324, -10.88017736071109987 ) ) ;
#94661 = CARTESIAN_POINT ( 'NONE',  ( -1.099225684535947600, 24.54030133659708923, 6.408140936763237150 ) ) ;
#94662 = CARTESIAN_POINT ( 'NONE',  ( -8.000000000000000000, 1.019547802438466100, -4.000000000000000000 ) ) ;
#94664 = CARTESIAN_POINT ( 'NONE',  ( 8.564643372776536978, 0.5000000000000004441, 12.31449893000746343 ) ) ;
#94663 = CARTESIAN_POINT ( 'NONE',  ( 7.084665262690076126, 22.02201867748817321, -10.88017736071110164 ) ) ;
#94665 = DIRECTION ( 'NONE',  ( 0.3173046564051031360, 0.000000000000000000, -0.9483236552061955482 ) ) ;
#94666 = CARTESIAN_POINT ( 'NONE',  ( 24.16423886937410614, 39.30374883491396787, 8.672049930838204340E-16 ) ) ;
#94667 = CARTESIAN_POINT ( 'NONE',  ( 17.08211943468705840, 25.13708216824730357, -12.26659068614894466 ) ) ;
#94668 = CARTESIAN_POINT ( 'NONE',  ( 19.42250999205614548, 10.98035201082150536, -5.440088680355545492 ) ) ;
#94669 = MECHANICAL_DESIGN_GEOMETRIC_PRESENTATION_REPRESENTATION (  '', ( #24461 ), #80328 ) ;
#94670 = CARTESIAN_POINT ( 'NONE',  ( 19.84674366389459266, 38.71726448433412315, -2.638427012816827677 ) ) ;
#94671 = CARTESIAN_POINT ( 'NONE',  ( 3.591859063236763294, 38.29030133659708923, -11.09922568453595026 ) ) ;
#94672 = CARTESIAN_POINT ( 'NONE',  ( 7.084665262690076126, 17.02201867748817676, -10.88017736071110164 ) ) ;
#94673 = CARTESIAN_POINT ( 'NONE',  ( 12.63842701281683034, 42.46726448433412315, 9.846743663894596210 ) ) ;
#94674 = CARTESIAN_POINT ( 'NONE',  ( -0.8801773607111009756, 38.06368534415484106, 1.068504757029289695E-15 ) ) ;
#94675 = CARTESIAN_POINT ( 'NONE',  ( 19.38216949554541557, 7.248634669930421381, -9.382169495545420901 ) ) ;
#94676 = CARTESIAN_POINT ( 'NONE',  ( -0.3689425029237898834, 26.17874883491396432, -10.36894250292378850 ) ) ;
#94677 = DIRECTION ( 'NONE',  ( -0.1822355254921381451, 0.000000000000000000, -0.9832549075639562819 ) ) ;
#94678 = PRESENTATION_LAYER_ASSIGNMENT (  '', '', ( #43568 ) ) ;
#94679 = COLOUR_RGB ( '', 0.72549020, 0.75294118, 0.79215686) ;
#94680 = CARTESIAN_POINT ( 'NONE',  ( 10.00000000000000000, 19.75893115100078390, -9.846743663894594434 ) ) ;
#94681 = CARTESIAN_POINT ( 'NONE',  ( 13.43411237798106583, 52.66530133659708213, -12.81628187352647252 ) ) ;
#94682 = CARTESIAN_POINT ( 'NONE',  ( 0.1532563361054083140, 61.00893115100078745, 1.131784320476157264E-15 ) ) ;
#94683 = VERTEX_POINT ( 'NONE', #27630 ) ;
#94684 = STYLED_ITEM ( 'NONE', ( #7633 ), #92799 ) ;
#94685 = CARTESIAN_POINT ( 'NONE',  ( -14.71525861348285957, 15.00000000000000000, -2.908807992686776700 ) ) ;
#94686 = PRESENTATION_STYLE_ASSIGNMENT (( #41217 ) ) ;
#94687 = CARTESIAN_POINT ( 'NONE',  ( -2.266590686148945544, 67.22041550158063217, 7.082119434687048631 ) ) ;
#94688 = CARTESIAN_POINT ( 'NONE',  ( 17.96484262340118221, 59.93868534415484106, 7.964842623401181321 ) ) ;
#94689 = CARTESIAN_POINT ( 'NONE',  ( -2.266590686148945544, 12.22041550158063394, 7.082119434687048631 ) ) ;
#94690 = EDGE_CURVE ( 'NONE', #27652, #97731, #98069, .T. ) ;
#94691 = CARTESIAN_POINT ( 'NONE',  ( 1.472469842513823179, 5.592264484334118713, -4.923371831947296329 ) ) ;
#94692 = CARTESIAN_POINT ( 'NONE',  ( 5.076628168052703671, 46.84226448433412315, 8.527530157486179263 ) ) ;
#94693 = CARTESIAN_POINT ( 'NONE',  ( 15.44008868035555793, 21.39701867748817321, -9.422509992056140149 ) ) ;
#94694 = AXIS2_PLACEMENT_3D ( 'NONE', #81041, #29016, #59526 ) ;
#94695 = FACE_OUTER_BOUND ( 'NONE', #9219, .T. ) ;
#94696 = LINE ( 'NONE', #9723, #2602 ) ;
#94697 = EDGE_CURVE ( 'NONE', #89452, #46043, #37391, .T. ) ;
#94698 = VERTEX_POINT ( 'NONE', #35632 ) ;
#94699 = DIRECTION ( 'NONE',  ( -0.000000000000000000, 0.000000000000000000, 1.000000000000000000 ) ) ;
#94700 = ORIENTED_EDGE ( 'NONE', *, *, #94485, .T. ) ;
#94701 = VERTEX_POINT ( 'NONE', #57143 ) ;
#94702 = CARTESIAN_POINT ( 'NONE',  ( -5.204170427930421283E-15, 11.67180217785154817, -11.25000000000000178 ) ) ;
#94703 = CARTESIAN_POINT ( 'NONE',  ( 2.917880565312948704, 2.637082168247300906, 12.26659068614894643 ) ) ;
#94704 = CARTESIAN_POINT ( 'NONE',  ( 13.79529636645031943, 5.345415501580634832, -14.16423886937409904 ) ) ;
#94705 = CARTESIAN_POINT ( 'NONE',  ( 19.84674366389459621, 58.50893115100078745, 7.409399052514197653E-17 ) ) ;
#94706 = CARTESIAN_POINT ( 'NONE',  ( 2.791683348922237240, 40.38393115100078035, -7.208316651077763204 ) ) ;
#94707 = CARTESIAN_POINT ( 'NONE',  ( -6.000000000000000000, 78.07179676972447169, -4.250000000000000000 ) ) ;
#94709 = CARTESIAN_POINT ( 'NONE',  ( 7.361572987183169658, 64.96726448433412315, -9.846743663894592657 ) ) ;
#94708 = CARTESIAN_POINT ( 'NONE',  ( 20.88017736071110519, 35.56368534415484106, 2.639326808657452039E-16 ) ) ;
#94710 = CARTESIAN_POINT ( 'NONE',  ( 24.16423886937410614, 44.30374883491397497, 8.672049930838204340E-16 ) ) ;
#94711 = CARTESIAN_POINT ( 'NONE',  ( 12.91533473730992121, 4.522018677488170546, 10.88017736071110164 ) ) ;
#94712 = DIRECTION ( 'NONE',  ( 0.000000000000000000, 0.000000000000000000, 1.000000000000000000 ) ) ;
#94713 = CARTESIAN_POINT ( 'NONE',  ( 10.00000000000000178, 59.31368534415484106, 10.88017736071110342 ) ) ;
#94714 = CARTESIAN_POINT ( 'NONE',  ( 7.361572987183169658, 29.96726448433411960, -9.846743663894592657 ) ) ;
#94715 = DIRECTION ( 'NONE',  ( 6.608470384673550777E-17, 1.000000000000000000, -0.000000000000000000 ) ) ;
#94716 = ORIENTED_EDGE ( 'NONE', *, *, #56594, .F. ) ;
#94717 = DIRECTION ( 'NONE',  ( -1.000000000000000000, 0.000000000000000000, 0.000000000000000000 ) ) ;
#94718 = VERTEX_POINT ( 'NONE', #50135 ) ;
#94719 = CARTESIAN_POINT ( 'NONE',  ( 12.63842701281683034, 22.46726448433411605, 9.846743663894596210 ) ) ;
#94720 = ORIENTED_EDGE ( 'NONE', *, *, #54069, .F. ) ;
#94721 = CARTESIAN_POINT ( 'NONE',  ( 20.36894250292379382, 33.67874883491396076, 10.36894250292379205 ) ) ;
#94722 = CARTESIAN_POINT ( 'NONE',  ( 14.92337183194729988, 34.34226448433411605, -8.527530157486177487 ) ) ;
#94723 = CARTESIAN_POINT ( 'NONE',  ( 2.035157376598824452, 53.68868534415484817, 7.964842623401179544 ) ) ;
#94724 = CARTESIAN_POINT ( 'NONE',  ( 20.88017736071110519, 35.56368534415484106, 2.639326808657452039E-16 ) ) ;
#94725 = CIRCLE ( 'NONE', #58019, 0.5000000000000004441 ) ;
#94726 = EDGE_CURVE ( 'NONE', #21166, #69569, #50380, .T. ) ;
#94727 = CARTESIAN_POINT ( 'NONE',  ( 0.1532563361054083140, 51.00893115100078745, 1.131784320476157264E-15 ) ) ;
#94728 = CARTESIAN_POINT ( 'NONE',  ( -12.81628187352647963, -11.08469866340290899, -3.434112377981046293 ) ) ;
#94729 = ADVANCED_FACE ( 'NONE', ( #66117 ), #64626, .F. ) ;
#94730 = ORIENTED_EDGE ( 'NONE', *, *, #68637, .F. ) ;
#94731 = CARTESIAN_POINT ( 'NONE',  ( -0.3689425029237881626, 12.42874883491396609, 10.36894250292379027 ) ) ;
#94732 = ORIENTED_EDGE ( 'NONE', *, *, #8057, .F. ) ;
#94733 = ORIENTED_EDGE ( 'NONE', *, *, #89584, .T. ) ;
#94734 = CARTESIAN_POINT ( 'NONE',  ( 5.076628168052704559, 0.1755978176674514724, -8.527530157486179263 ) ) ;
#94735 = CARTESIAN_POINT ( 'NONE',  ( 16.40814093676323893, 25.79030133659708923, 11.09922568453595026 ) ) ;
#94736 = CARTESIAN_POINT ( 'NONE',  ( 5.076628168052703671, 16.84226448433411960, 8.527530157486179263 ) ) ;
#94737 = CARTESIAN_POINT ( 'NONE',  ( 19.38216949554541557, 47.24863466993041783, -9.382169495545420901 ) ) ;
#94738 = DIRECTION ( 'NONE',  ( 1.000000000000000000, 0.000000000000000000, 0.000000000000000000 ) ) ;
#94739 = CARTESIAN_POINT ( 'NONE',  ( 10.00000000000000178, 32.25893115100078745, 9.846743663894594434 ) ) ;
#94740 = CARTESIAN_POINT ( 'NONE',  ( 12.91533473730992121, 59.52201867748816966, 10.88017736071110164 ) ) ;
#94741 = DIRECTION ( 'NONE',  ( -0.9588197348681908316, 0.000000000000000000, -0.2840153447039300283 ) ) ;
#94742 = CARTESIAN_POINT ( 'NONE',  ( -14.94699059465106572, 14.63606911935818289, 1.259949270174702818 ) ) ;
#94743 = ADVANCED_FACE ( 'NONE', ( #19154 ), #26646, .T. ) ;
#94744 = CARTESIAN_POINT ( 'NONE',  ( 2.148416515056630782, 2.237265733804437495, 6.499999999999993783 ) ) ;
#94745 = CARTESIAN_POINT ( 'NONE',  ( 0.5774900079438607392, 68.48035201082150536, 5.440088680355550821 ) ) ;
#94746 = AXIS2_PLACEMENT_3D ( 'NONE', #77651, #24183, #90689 ) ;
#94747 = CARTESIAN_POINT ( 'NONE',  ( 3.591859063236761518, 14.95696800326375531, 11.09922568453594849 ) ) ;
#94749 =( NAMED_UNIT ( * ) SI_UNIT ( $, .STERADIAN. ) SOLID_ANGLE_UNIT ( ) );
#94748 = AXIS2_PLACEMENT_3D ( 'NONE', #44132, #42673, #46010 ) ;
#94750 = CARTESIAN_POINT ( 'NONE',  ( 10.00000000000000000, 49.75893115100078745, -9.846743663894594434 ) ) ;
#94751 = CARTESIAN_POINT ( 'NONE',  ( 13.43411237798106583, 62.66530133659708923, -12.81628187352647252 ) ) ;
#94752 = CARTESIAN_POINT ( 'NONE',  ( -4.164238869374098151, 11.59541550158063217, -3.795296366450310543 ) ) ;
#94753 = CARTESIAN_POINT ( 'NONE',  ( 2.791683348922240793, 36.63393115100078035, 7.208316651077764092 ) ) ;
#94754 = VECTOR ( 'NONE', #73224, 1000.000000000000000 ) ;
#94755 = CARTESIAN_POINT ( 'NONE',  ( 16.40814093676323893, 30.79030133659708923, 11.09922568453595026 ) ) ;
#94757 = CARTESIAN_POINT ( 'NONE',  ( 20.10421743870887212, 15.60736173766201951, -6.337391062633417782 ) ) ;
#94756 = CARTESIAN_POINT ( 'NONE',  ( 14.56372689393328734, 0.04962896412619403896, 2.356940382833113024 ) ) ;
#94758 = CARTESIAN_POINT ( 'NONE',  ( 10.00000000000000000, 66.81368534415484817, -10.88017736071110342 ) ) ;
#94759 = CARTESIAN_POINT ( 'NONE',  ( -2.816281873526473856, 4.123634669930420493, 9.499525473075851096E-16 ) ) ;
#94760 = CARTESIAN_POINT ( 'NONE',  ( 9.520529577030492518, 2.507217523872729004E-16, -11.10395710204420716 ) ) ;
#94761 = CARTESIAN_POINT ( 'NONE',  ( 19.84674366389459266, 38.30059781766745175, 2.638427012816836559 ) ) ;
#94762 = CARTESIAN_POINT ( 'NONE',  ( 10.00000000000000178, 29.31368534415483751, 10.88017736071110342 ) ) ;
#94763 = CARTESIAN_POINT ( 'NONE',  ( -2.816281873526473856, 24.33196800326375353, 3.434112377981055619 ) ) ;
#94764 = CARTESIAN_POINT ( 'NONE',  ( 17.20831665107776587, 17.88393115100078745, 7.208316651077764980 ) ) ;
#94765 = CARTESIAN_POINT ( 'NONE',  ( -9.343156623282764528, 88.41679554545861208, 5.273290232418111678 ) ) ;
#94766 = CARTESIAN_POINT ( 'NONE',  ( 2.035157376598824452, 38.68868534415483396, 7.964842623401179544 ) ) ;
#94767 = ORIENTED_EDGE ( 'NONE', *, *, #389, .F. ) ;
#94768 = CARTESIAN_POINT ( 'NONE',  ( 0.5774900079438607392, 58.48035201082151247, 5.440088680355550821 ) ) ;
#94769 = SURFACE_STYLE_FILL_AREA ( #10788 ) ;
#94771 = CARTESIAN_POINT ( 'NONE',  ( -0.8801773607110991993, 27.85535201082150181, -2.915334737309923874 ) ) ;
#94770 = CARTESIAN_POINT ( 'NONE',  ( 14.92337183194729633, 47.67559781766745175, 8.527530157486181039 ) ) ;
#94772 = CARTESIAN_POINT ( 'NONE',  ( 2.035157376598822676, 47.43868534415484817, -7.964842623401177768 ) ) ;
#94773 = CARTESIAN_POINT ( 'NONE',  ( 12.91533473730993009, 11.60535201082150714, -10.88017736071109987 ) ) ;
#94774 = CARTESIAN_POINT ( 'NONE',  ( 8.879999999999991900, 76.07179676972447169, -6.500000000000000888 ) ) ;
#94775 = CARTESIAN_POINT ( 'NONE',  ( 14.92337183194729633, 42.67559781766745886, 8.527530157486181039 ) ) ;
#94777 = CARTESIAN_POINT ( 'NONE',  ( 6.757757868617466634, -58.31753767725378879, 3.750000000000000888 ) ) ;
#94776 = CARTESIAN_POINT ( 'NONE',  ( 6.204703633549690345, 47.84541550158064638, 14.16423886937410082 ) ) ;
#94778 = CARTESIAN_POINT ( 'NONE',  ( 66.56412365047464164, 26.99999999999998224, 10.00000000000000000 ) ) ;
#94779 = COLOUR_RGB ( '', 0.72549020, 0.75294118, 0.79215686) ;
#94780 = DIRECTION ( 'NONE',  ( 1.000000000000000000, 0.000000000000000000, 0.000000000000000000 ) ) ;
#94781 = CARTESIAN_POINT ( 'NONE',  ( 20.36894250292379382, 43.67874883491397497, 10.36894250292379205 ) ) ;
#94782 = CARTESIAN_POINT ( 'NONE',  ( -6.982525766850298687, -88.11956318484570261, 2.750000000000000444 ) ) ;
#94783 = VERTEX_POINT ( 'NONE', #95135 ) ;
#94784 = CARTESIAN_POINT ( 'NONE',  ( 4.559911319644449179, 3.897018677488171434, 9.422509992056141925 ) ) ;
#94785 = CARTESIAN_POINT ( 'NONE',  ( 18.52753015748618282, 38.92559781766745175, -4.923371831947291888 ) ) ;
#94787 = CARTESIAN_POINT ( 'NONE',  ( -8.004790597918161055, 84.51838969325523010, -3.750000002001242283 ) ) ;
#94786 = CARTESIAN_POINT ( 'NONE',  ( -6.741983435833607707, 14.95077488074853456, 13.12218577464082614 ) ) ;
#94788 = CARTESIAN_POINT ( 'NONE',  ( 0.5774900079438607392, 63.48035201082149825, 5.440088680355550821 ) ) ;
#94789 = CARTESIAN_POINT ( 'NONE',  ( -1.099225684535947600, 59.54030133659708923, 6.408140936763237150 ) ) ;
#94790 = CARTESIAN_POINT ( 'NONE',  ( 12.91533473730993009, 36.60535201082151247, -10.88017736071109987 ) ) ;
#94791 = CARTESIAN_POINT ( 'NONE',  ( 10.00000000000000178, 60.37363466993041783, 12.81628187352647608 ) ) ;
#94792 = CARTESIAN_POINT ( 'NONE',  ( 13.43411237798105340, 10.58196800326375353, 12.81628187352647963 ) ) ;
#94793 = CARTESIAN_POINT ( 'NONE',  ( 0.1532563361054082862, 16.21726448433411960, 2.638427012816831674 ) ) ;
#94794 = ORIENTED_EDGE ( 'NONE', *, *, #78519, .F. ) ;
#94795 =( LENGTH_UNIT ( ) NAMED_UNIT ( * ) SI_UNIT ( .MILLI., .METRE. ) );
#94796 = DIRECTION ( 'NONE',  ( -0.000000000000000000, -1.000000000000000000, -0.000000000000000000 ) ) ;
#94797 = CARTESIAN_POINT ( 'NONE',  ( 2.035157376598822676, 7.438685344154837509, -7.964842623401177768 ) ) ;
#94798 = CARTESIAN_POINT ( 'NONE',  ( -0.3689425029237898834, 21.17874883491396432, -10.36894250292378850 ) ) ;
#94799 = CARTESIAN_POINT ( 'NONE',  ( 17.96484262340118221, 29.93868534415484106, 7.964842623401181321 ) ) ;
#94800 = CARTESIAN_POINT ( 'NONE',  ( 19.42250999205614548, 50.98035201082151247, -5.440088680355545492 ) ) ;
#94801 = CARTESIAN_POINT ( 'NONE',  ( -38.69000000000001194, 93.50000000000000000, -10.09898361729590199 ) ) ;
#94802 = CARTESIAN_POINT ( 'NONE',  ( -13.07751017357375112, 4.831904710033835254E-16, -6.263284095430687870 ) ) ;
#94803 = CARTESIAN_POINT ( 'NONE',  ( 1.472469842513823179, 6.425597817667451750, 4.923371831947296329 ) ) ;
#94804 = DIRECTION ( 'NONE',  ( -1.000000000000000000, -1.257402221000611116E-16, 0.000000000000000000 ) ) ;
#94805 = CARTESIAN_POINT ( 'NONE',  ( 7.361572987183170547, 27.05059781766745175, 9.846743663894590881 ) ) ;
#94806 = CARTESIAN_POINT ( 'NONE',  ( 6.579634127946655475, -87.99828267815715321, -3.750000000000000000 ) ) ;
#94807 = CARTESIAN_POINT ( 'NONE',  ( 19.84674366389459621, 23.50893115100078390, 7.409399052514197653E-17 ) ) ;
#94808 = CARTESIAN_POINT ( 'NONE',  ( 1.472469842513823179, 46.42559781766745175, 4.923371831947296329 ) ) ;
#94809 = EDGE_CURVE ( 'NONE', #87334, #62932, #62913, .T. ) ;
#94810 = CARTESIAN_POINT ( 'NONE',  ( 2.035157376598822676, 22.43868534415483396, -7.964842623401177768 ) ) ;
#94811 = CARTESIAN_POINT ( 'NONE',  ( 10.00000000000000000, 42.87363466993042493, -12.81628187352647608 ) ) ;
#94812 =( GEOMETRIC_REPRESENTATION_CONTEXT ( 3 ) GLOBAL_UNCERTAINTY_ASSIGNED_CONTEXT ( ( #43473 ) ) GLOBAL_UNIT_ASSIGNED_CONTEXT ( ( #33300, #87292, #95287 ) ) REPRESENTATION_CONTEXT ( 'NONE', 'WORKASPACE' ) );
#94813 = CARTESIAN_POINT ( 'NONE',  ( 0.1532563361054100626, 0.8005978176674514168, -2.638427012816831230 ) ) ;
#94814 = CARTESIAN_POINT ( 'NONE',  ( 14.92337183194729633, 32.67559781766745175, 8.527530157486181039 ) ) ;
#94816 = CARTESIAN_POINT ( 'NONE',  ( 18.52753015748617571, 18.09226448433411960, 4.923371831947298993 ) ) ;
#94815 = CARTESIAN_POINT ( 'NONE',  ( 13.79529636645031943, 60.34541550158063927, -14.16423886937409904 ) ) ;
#94817 = DIRECTION ( 'NONE',  ( 0.000000000000000000, 1.000000000000000000, 0.000000000000000000 ) ) ;
#94818 = CARTESIAN_POINT ( 'NONE',  ( -42.80192881254231452, 92.20710678118653902, -9.499999999999998224 ) ) ;
#94819 = CARTESIAN_POINT ( 'NONE',  ( -4.164238869374099039, 6.803748834913967869, 8.674139862899312516E-16 ) ) ;
#94820 = CARTESIAN_POINT ( 'NONE',  ( -2.266590686148945544, 32.22041550158063927, 7.082119434687048631 ) ) ;
#94821 = CARTESIAN_POINT ( 'NONE',  ( 2.791683348922237240, 25.38393115100078390, -7.208316651077763204 ) ) ;
#94822 = CARTESIAN_POINT ( 'NONE',  ( 4.130000000000002558, 1.019547802438464545, -2.500000000000000000 ) ) ;
#94823 = CARTESIAN_POINT ( 'NONE',  ( 15.44008868035555260, 19.73035201082150536, 9.422509992056143702 ) ) ;
#94824 = AXIS2_PLACEMENT_3D ( 'NONE', #13621, #22123, #76584 ) ;
#94825 = CARTESIAN_POINT ( 'NONE',  ( 10.00000000000000000, 56.81368534415484106, -10.88017736071110342 ) ) ;
#94826 = CARTESIAN_POINT ( 'NONE',  ( 0.5774900079438607392, 38.48035201082150536, 5.440088680355550821 ) ) ;
#94827 = EDGE_LOOP ( 'NONE', ( #75064, #84188, #53460, #79400 ) ) ;
#94828 = CARTESIAN_POINT ( 'NONE',  ( 3.591859063236761518, 44.95696800326376064, 11.09922568453594849 ) ) ;
#94829 = CARTESIAN_POINT ( 'NONE',  ( 12.91533473730992121, 49.52201867748817676, 10.88017736071110164 ) ) ;
#94830 = ORIENTED_EDGE ( 'NONE', *, *, #71236, .T. ) ;
#94831 = CARTESIAN_POINT ( 'NONE',  ( 3.243710765982298128, 0.000000000000000000, 4.383623511354910463 ) ) ;
#94832 = DIRECTION ( 'NONE',  ( 0.000000000000000000, 0.000000000000000000, -1.000000000000000000 ) ) ;
#94833 = ORIENTED_EDGE ( 'NONE', *, *, #934, .T. ) ;
#94834 = CARTESIAN_POINT ( 'NONE',  ( 15.44008868035555793, 61.39701867748817676, -9.422509992056140149 ) ) ;
#94835 = CARTESIAN_POINT ( 'NONE',  ( 19.42250999205614548, 5.980352010821504471, -5.440088680355545492 ) ) ;
#94836 = EDGE_CURVE ( 'NONE', #52439, #65339, #86897, .T. ) ;
#94837 = CARTESIAN_POINT ( 'NONE',  ( 20.88017736071110164, 40.35535201082150536, 2.915334737309930979 ) ) ;
#94838 = DIRECTION ( 'NONE',  ( -0.000000000000000000, -1.000000000000000000, 0.000000000000000000 ) ) ;
#94839 = CARTESIAN_POINT ( 'NONE',  ( 10.00000000000000000, 1.813685344154838175, -10.88017736071110342 ) ) ;
#94840 = CARTESIAN_POINT ( 'NONE',  ( 14.92337183194729988, 4.342264484334117824, -8.527530157486177487 ) ) ;
#94841 = CARTESIAN_POINT ( 'NONE',  ( 22.26659068614894466, 8.887082168247300018, 7.082119434687054849 ) ) ;
#94842 = CARTESIAN_POINT ( 'NONE',  ( 5.076628168052704559, 5.175597817667451750, -8.527530157486179263 ) ) ;
#94843 = ADVANCED_FACE ( 'NONE', ( #35123 ), #13124, .T. ) ;
#94844 = CARTESIAN_POINT ( 'NONE',  ( -0.8801773607111008646, 13.27201867748817143, 2.915334737309923430 ) ) ;
#94845 = CARTESIAN_POINT ( 'NONE',  ( 1.472469842513823179, 46.42559781766745175, 4.923371831947296329 ) ) ;
#94846 = VERTEX_POINT ( 'NONE', #11650 ) ;
#94847 = CARTESIAN_POINT ( 'NONE',  ( 19.84674366389459621, 48.50893115100078745, 7.409399052514197653E-17 ) ) ;
#94848 = ORIENTED_EDGE ( 'NONE', *, *, #13478, .T. ) ;
#94849 = CARTESIAN_POINT ( 'NONE',  ( 0.000000000000000000, 15.00000000000000000, 0.000000000000000000 ) ) ;
#94850 = CARTESIAN_POINT ( 'NONE',  ( 12.91533473730993009, 56.60535201082151247, -10.88017736071109987 ) ) ;
#94851 = CARTESIAN_POINT ( 'NONE',  ( 5.076628168052703671, 51.84226448433412315, 8.527530157486179263 ) ) ;
#94853 = CARTESIAN_POINT ( 'NONE',  ( 24.35999999999999233, 37.99999999999997868, 9.500000000000000000 ) ) ;
#94852 = CARTESIAN_POINT ( 'NONE',  ( 0.5774900079438607392, 3.480352010821504027, 5.440088680355550821 ) ) ;
#94854 = CARTESIAN_POINT ( 'NONE',  ( 15.44008868035555260, 54.73035201082150536, 9.422509992056143702 ) ) ;
#94855 = CARTESIAN_POINT ( 'NONE',  ( 4.559911319644449179, 7.230352010821505360, -9.422509992056141925 ) ) ;
#94856 = CARTESIAN_POINT ( 'NONE',  ( 10.00000000000000000, 37.87363466993041783, -12.81628187352647608 ) ) ;
#94857 = CARTESIAN_POINT ( 'NONE',  ( 12.91533473730992121, 34.52201867748817676, 10.88017736071110164 ) ) ;
#94858 = CARTESIAN_POINT ( 'NONE',  ( 0.000000000000000000, 69.50000000000000000, 6.000000000000000000 ) ) ;
#94859 = EDGE_LOOP ( 'NONE', ( #3313, #7688, #19001, #57577 ) ) ;
#94860 = CARTESIAN_POINT ( 'NONE',  ( 16.40814093676323893, 45.79030133659708923, 11.09922568453595026 ) ) ;
#94861 = CARTESIAN_POINT ( 'NONE',  ( 0.5774900079438607392, 38.48035201082150536, 5.440088680355550821 ) ) ;
#94862 = EDGE_LOOP ( 'NONE', ( #12587, #30769, #38368, #76953 ) ) ;
#94863 = CARTESIAN_POINT ( 'NONE',  ( 1.983216688680843109, -0.03417435944610275333, 14.11131997956739070 ) ) ;
#94864 = EDGE_CURVE ( 'NONE', #73802, #67464, #5640, .T. ) ;
#94865 = CARTESIAN_POINT ( 'NONE',  ( 18.52753015748617571, 8.092264484334117824, 4.923371831947298993 ) ) ;
#94866 = CARTESIAN_POINT ( 'NONE',  ( 10.00000000000000178, 62.25893115100078745, 9.846743663894594434 ) ) ;
#94868 = CARTESIAN_POINT ( 'NONE',  ( 14.92337183194729633, 57.67559781766745886, 8.527530157486181039 ) ) ;
#94867 = CARTESIAN_POINT ( 'NONE',  ( 1.472469842513823179, 6.425597817667451750, 4.923371831947296329 ) ) ;
#94869 = LINE ( 'NONE', #71875, #40905 ) ;
#94870 = CARTESIAN_POINT ( 'NONE',  ( 12.63842701281683922, 39.55059781766744464, -9.846743663894590881 ) ) ;
#94871 = CARTESIAN_POINT ( 'NONE',  ( 14.29541133317244217, 0.2306972965111902807, -4.345028136609535352 ) ) ;
#94872 = DIRECTION ( 'NONE',  ( -0.000000000000000000, -0.000000000000000000, -1.000000000000000000 ) ) ;
#94873 = EDGE_CURVE ( 'NONE', #72785, #38297, #42165, .T. ) ;
#94875 = CARTESIAN_POINT ( 'NONE',  ( 10.00000000000000000, -0.2410688489992152128, -9.846743663894594434 ) ) ;
#94874 = CARTESIAN_POINT ( 'NONE',  ( 17.20831665107776587, 34.13393115100078745, -7.208316651077762316 ) ) ;
#94876 = PLANE ( 'NONE',  #40967 ) ;
#94878 = EDGE_LOOP ( 'NONE', ( #87768, #39760, #71252, #9144 ) ) ;
#94877 = CARTESIAN_POINT ( 'NONE',  ( 12.63842701281683922, 59.55059781766744464, -9.846743663894590881 ) ) ;
#94879 =( NAMED_UNIT ( * ) PLANE_ANGLE_UNIT ( ) SI_UNIT ( $, .RADIAN. ) );
#94880 = CARTESIAN_POINT ( 'NONE',  ( -2.816281873526473856, 29.12363466993041783, 9.499525473075851096E-16 ) ) ;
#94881 = CARTESIAN_POINT ( 'NONE',  ( 12.63842701281683922, 44.55059781766745175, -9.846743663894590881 ) ) ;
#94882 = VECTOR ( 'NONE', #8922, 1000.000000000000000 ) ;
#94883 = CARTESIAN_POINT ( 'NONE',  ( 3.469446951953614189E-15, 6.368033628982654903, 11.25000000000000178 ) ) ;
#94884 = CARTESIAN_POINT ( 'NONE',  ( 20.36894250292379382, 58.67874883491396076, 10.36894250292379205 ) ) ;
#94885 = CARTESIAN_POINT ( 'NONE',  ( 1.472469842513823179, 21.42559781766745175, 4.923371831947296329 ) ) ;
#94886 = CARTESIAN_POINT ( 'NONE',  ( 20.00000000000000355, 82.53121788603681352, 5.047406989012417355 ) ) ;
#94887 = CIRCLE ( 'NONE', #51794, 3.000000000000002665 ) ;
#94888 = CARTESIAN_POINT ( 'NONE',  ( -4.164238869374098151, 61.59541550158063217, -3.795296366450310543 ) ) ;
#94889 = CARTESIAN_POINT ( 'NONE',  ( 12.63842701281683922, 54.55059781766745175, -9.846743663894590881 ) ) ;
#94890 = CARTESIAN_POINT ( 'NONE',  ( 7.084665262690076126, 9.105352010821503583, 10.88017736071109987 ) ) ;
#94891 = CARTESIAN_POINT ( 'NONE',  ( 24.16423886937410614, 34.30374883491396787, 8.672049930838204340E-16 ) ) ;
#94892 = CARTESIAN_POINT ( 'NONE',  ( -4.164238869374099927, 42.01208216824728936, 3.795296366450308767 ) ) ;
#94893 = DIRECTION ( 'NONE',  ( -1.000000000000000000, 0.000000000000000000, 0.000000000000000000 ) ) ;
#94895 = CARTESIAN_POINT ( 'NONE',  ( 12.63842701281683034, 52.46726448433413026, 9.846743663894596210 ) ) ;
#94894 = DIRECTION ( 'NONE',  ( 0.000000000000000000, -1.000000000000000000, 0.000000000000000000 ) ) ;
#94896 = ORIENTED_EDGE ( 'NONE', *, *, #22288, .T. ) ;
#94897 = CARTESIAN_POINT ( 'NONE',  ( 4.559911319644449179, 32.23035201082150536, -9.422509992056141925 ) ) ;
#94898 = CARTESIAN_POINT ( 'NONE',  ( 11.44532481276809577, -77.50732122612269848, 3.750000000000000444 ) ) ;
#94899 = CARTESIAN_POINT ( 'NONE',  ( 19.84674366389459621, 53.50893115100078745, 7.409399052514197653E-17 ) ) ;
#94900 = CARTESIAN_POINT ( 'NONE',  ( 1.379999999999981908, 20.99999999999999645, 1.249999999999987121 ) ) ;
#94901 = CARTESIAN_POINT ( 'NONE',  ( -10.36894250292379205, 1.178748834913966315, -10.36894250292378672 ) ) ;
#94902 = CARTESIAN_POINT ( 'NONE',  ( 12.63842701281683034, 52.46726448433413026, 9.846743663894596210 ) ) ;
#94904 = CARTESIAN_POINT ( 'NONE',  ( 17.20831665107776587, 62.88393115100078745, 7.208316651077764980 ) ) ;
#94903 =( BOUNDED_CURVE ( )  B_SPLINE_CURVE ( 2, ( #65708, #82195, #87723, #72710, #34718, #27215, #80226, #28700, #5233 ),
 .UNSPECIFIED., .F., .F. ) 
 B_SPLINE_CURVE_WITH_KNOTS ( ( 3, 2, 2, 2, 3 ),
 ( 0.6187123655116599785, 0.6190476190476190688, 0.6250000000000000000, 0.6309523809523809312, 0.6312876344883400215 ),
 .UNSPECIFIED. ) 
 CURVE ( )  GEOMETRIC_REPRESENTATION_ITEM ( )  RATIONAL_B_SPLINE_CURVE ( ( 0.9963778908391764944, 0.9980808541467923733, 1.000000000000000000, 0.9659258262890683122, 1.000000000000000000, 0.9659258262890683122, 1.000000000000000000, 0.9980808541467922623, 0.9963778908391764944 ) ) 
 REPRESENTATION_ITEM ( '' )  );
#94905 = CARTESIAN_POINT ( 'NONE',  ( 13.79529636645031943, 25.34541550158063572, -14.16423886937409904 ) ) ;
#94906 = CARTESIAN_POINT ( 'NONE',  ( -14.91937968691865990, 14.76930270348881535, 0.8063277559917156889 ) ) ;
#94908 = CARTESIAN_POINT ( 'NONE',  ( -46.68456736488007408, 103.6675473310227034, 5.775421524742653467 ) ) ;
#94907 = CARTESIAN_POINT ( 'NONE',  ( -3.627483523208788530, -3.617667194775422423, -2.499999999999798383 ) ) ;
#94909 = CARTESIAN_POINT ( 'NONE',  ( 19.42250999205614193, 15.14701867748817143, 5.440088680355555262 ) ) ;
#94910 = CARTESIAN_POINT ( 'NONE',  ( 10.00000000000000178, 20.37363466993042138, 12.81628187352647608 ) ) ;
#94911 = CARTESIAN_POINT ( 'NONE',  ( -7.313705784284425526, 14.63595249122788999, -13.09617149020754034 ) ) ;
#94912 = CARTESIAN_POINT ( 'NONE',  ( 1.472469842513823179, 10.59226448433411782, -4.923371831947296329 ) ) ;
#94913 = CARTESIAN_POINT ( 'NONE',  ( 4.573751236700658751, -6.413519960483383464, -3.750000000000000000 ) ) ;
#94914 = CARTESIAN_POINT ( 'NONE',  ( 6.204703633549690345, 30.76208216824730357, -14.16423886937410259 ) ) ;
#94915 = FACE_OUTER_BOUND ( 'NONE', #26587, .T. ) ;
#94916 = SURFACE_STYLE_FILL_AREA ( #64410 ) ;
#94917 = CARTESIAN_POINT ( 'NONE',  ( 2.035157376598824452, 8.688685344154839285, 7.964842623401179544 ) ) ;
#94918 = DIRECTION ( 'NONE',  ( -0.000000000000000000, -1.000000000000000000, -0.000000000000000000 ) ) ;
#94919 = CARTESIAN_POINT ( 'NONE',  ( 7.084665262690076126, 42.02201867748816966, -10.88017736071110164 ) ) ;
#94920 = CARTESIAN_POINT ( 'NONE',  ( 7.084665262690076126, 37.02201867748817676, -10.88017736071110164 ) ) ;
#94921 = CARTESIAN_POINT ( 'NONE',  ( 19.84674366389459266, 63.71726448433412315, -2.638427012816827677 ) ) ;
#94922 = LINE ( 'NONE', #41462, #26617 ) ;
#94923 = DIRECTION ( 'NONE',  ( 0.000000000000000000, 0.000000000000000000, -1.000000000000000000 ) ) ;
#94924 = CARTESIAN_POINT ( 'NONE',  ( 19.84674366389459266, 8.717264484334116048, -2.638427012816827677 ) ) ;
#94925 = EDGE_LOOP ( 'NONE', ( #62591, #95710, #86427, #92065 ) ) ;
#94926 = AXIS2_PLACEMENT_3D ( 'NONE', #91760, #51292, #81777 ) ;
#94927 = CARTESIAN_POINT ( 'NONE',  ( 20.88017736071110875, 40.77201867748818387, -2.915334737309920765 ) ) ;
#94928 = EDGE_CURVE ( 'NONE', #36109, #88333, #66624, .T. ) ;
#94929 = CARTESIAN_POINT ( 'NONE',  ( -2.816281873526473856, 4.331968003263754419, 3.434112377981055619 ) ) ;
#94930 = CARTESIAN_POINT ( 'NONE',  ( 4.559911319644449179, 58.89701867748817676, 9.422509992056141925 ) ) ;
#94931 = CARTESIAN_POINT ( 'NONE',  ( 14.92337183194729633, 22.67559781766745175, 8.527530157486181039 ) ) ;
#94932 = CARTESIAN_POINT ( 'NONE',  ( 0.6178305044545838731, 29.74863466993042138, 9.382169495545420901 ) ) ;
#94934 = DIRECTION ( 'NONE',  ( -0.08715574274765129636, -0.9961946980917462113, 0.000000000000000000 ) ) ;
#94933 = CARTESIAN_POINT ( 'NONE',  ( 0.1532563361054082862, 6.217264484334118713, 2.638427012816831674 ) ) ;
#94935 = VERTEX_POINT ( 'NONE', #51631 ) ;
#94936 = LINE ( 'NONE', #94446, #96414 ) ;
#94937 = CARTESIAN_POINT ( 'NONE',  ( 0.000000000000000000, 0.5000000000000004441, 0.000000000000000000 ) ) ;
#94938 = CARTESIAN_POINT ( 'NONE',  ( 12.91533473730992121, 9.522018677488171434, 10.88017736071110164 ) ) ;
#94940 = CARTESIAN_POINT ( 'NONE',  ( 10.00000000000000000, 20.55374883491396787, -14.16423886937410082 ) ) ;
#94939 = CARTESIAN_POINT ( 'NONE',  ( 6.565887622018943937, 55.16530133659709634, 12.81628187352647430 ) ) ;
#94941 = CARTESIAN_POINT ( 'NONE',  ( 19.84674366389459266, 33.71726448433410894, -2.638427012816827677 ) ) ;
#94942 = CARTESIAN_POINT ( 'NONE',  ( 15.44008868035555793, 6.397018677488170546, -9.422509992056140149 ) ) ;
#94943 = CARTESIAN_POINT ( 'NONE',  ( 13.79529636645031943, 65.34541550158063217, -14.16423886937409904 ) ) ;
#94944 = ORIENTED_EDGE ( 'NONE', *, *, #63163, .F. ) ;
#94945 = CARTESIAN_POINT ( 'NONE',  ( 17.96484262340118221, 11.18868534415483929, -7.964842623401177768 ) ) ;
#94946 = CARTESIAN_POINT ( 'NONE',  ( -0.8801773607111008646, 23.27201867748817676, 2.915334737309923430 ) ) ;
#94947 = CARTESIAN_POINT ( 'NONE',  ( -5.419894505350392855, 14.49999999999999822, -13.98659156302466045 ) ) ;
#94948 = ORIENTED_EDGE ( 'NONE', *, *, #65210, .F. ) ;
#94949 = CARTESIAN_POINT ( 'NONE',  ( 7.361572987183169658, 64.96726448433412315, -9.846743663894592657 ) ) ;
#94950 = CARTESIAN_POINT ( 'NONE',  ( 20.88017736071110875, 20.77201867748816611, -2.915334737309920765 ) ) ;
#94951 = CARTESIAN_POINT ( 'NONE',  ( 5.076628168052703671, 51.84226448433412315, 8.527530157486179263 ) ) ;
#94952 = EDGE_CURVE ( 'NONE', #64082, #15746, #38948, .T. ) ;
#94953 = CARTESIAN_POINT ( 'NONE',  ( 22.81628187352647785, 51.41530133659708923, 3.434112377981063169 ) ) ;
#94954 = DIRECTION ( 'NONE',  ( -0.000000000000000000, -1.000000000000000000, -0.000000000000000000 ) ) ;
#94955 = CARTESIAN_POINT ( 'NONE',  ( 17.08211943468705840, 40.13708216824731068, -12.26659068614894466 ) ) ;
#94956 = CARTESIAN_POINT ( 'NONE',  ( 20.88017736071110519, 40.56368534415484106, 2.639326808657452039E-16 ) ) ;
#94957 = CARTESIAN_POINT ( 'NONE',  ( -0.8801773607110991993, 17.85535201082150536, -2.915334737309923874 ) ) ;
#94958 = CARTESIAN_POINT ( 'NONE',  ( 2.791683348922237240, 50.38393115100078035, -7.208316651077763204 ) ) ;
#94959 = CIRCLE ( 'NONE', #32645, 0.5000000000000004441 ) ;
#94960 = CARTESIAN_POINT ( 'NONE',  ( 7.361572987183169658, 54.96726448433413026, -9.846743663894592657 ) ) ;
#94961 = EDGE_CURVE ( 'NONE', #39745, #95826, #61576, .T. ) ;
#94962 =( GEOMETRIC_REPRESENTATION_CONTEXT ( 3 ) GLOBAL_UNCERTAINTY_ASSIGNED_CONTEXT ( ( #52459 ) ) GLOBAL_UNIT_ASSIGNED_CONTEXT ( ( #25346, #76360, #23374 ) ) REPRESENTATION_CONTEXT ( 'NONE', 'WORKASPACE' ) );
#94963 = CARTESIAN_POINT ( 'NONE',  ( 18.52753015748618282, 3.925597817667451306, -4.923371831947291888 ) ) ;
#94964 = CARTESIAN_POINT ( 'NONE',  ( 11.09922568453594671, -37.95969866340291077, -6.408140936763241591 ) ) ;
#94965 = ORIENTED_EDGE ( 'NONE', *, *, #58588, .T. ) ;
#94966 = CARTESIAN_POINT ( 'NONE',  ( 2.035157376598824452, 18.68868534415484106, 7.964842623401179544 ) ) ;
#94967 = CARTESIAN_POINT ( 'NONE',  ( 0.1532563361054100626, 15.80059781766745353, -2.638427012816831230 ) ) ;
#94968 = CARTESIAN_POINT ( 'NONE',  ( 13.43411237798106583, 2.665301336597086568, -12.81628187352647252 ) ) ;
#94970 = CARTESIAN_POINT ( 'NONE',  ( 0.5774900079438590739, 52.64701867748817676, -5.440088680355550821 ) ) ;
#94969 = CARTESIAN_POINT ( 'NONE',  ( 19.42250999205614548, 45.98035201082150536, -5.440088680355545492 ) ) ;
#94972 = CARTESIAN_POINT ( 'NONE',  ( 13.43411237798105340, 45.58196800326374643, 12.81628187352647963 ) ) ;
#94971 = CARTESIAN_POINT ( 'NONE',  ( 12.91533473730992121, 14.52201867748817143, 10.88017736071110164 ) ) ;
#94973 = CARTESIAN_POINT ( 'NONE',  ( 24.16423886937410614, 29.30374883491396787, 8.672049930838204340E-16 ) ) ;
#94974 = CARTESIAN_POINT ( 'NONE',  ( 0.000000000000000000, 69.99999999999998579, 6.250000000000000000 ) ) ;
#94975 = VECTOR ( 'NONE', #392, 1000.000000000000114 ) ;
#94976 = CARTESIAN_POINT ( 'NONE',  ( 16.40814093676323893, 55.79030133659708923, 11.09922568453595026 ) ) ;
#94977 = VERTEX_POINT ( 'NONE', #83608 ) ;
#94978 = CARTESIAN_POINT ( 'NONE',  ( 10.00000000000000000, 59.75893115100078745, -9.846743663894594434 ) ) ;
#94979 = CARTESIAN_POINT ( 'NONE',  ( 15.44008868035555260, 29.73035201082150891, 9.422509992056143702 ) ) ;
#94980 = ORIENTED_EDGE ( 'NONE', *, *, #63217, .F. ) ;
#94982 = CARTESIAN_POINT ( 'NONE',  ( 10.14667048435135577, 15.00000000000000000, 10.35833375027046976 ) ) ;
#94981 = CARTESIAN_POINT ( 'NONE',  ( 5.076628168052703671, 6.842264484334118713, 8.527530157486179263 ) ) ;
#94983 = CARTESIAN_POINT ( 'NONE',  ( 2.791683348922240793, 6.633931151000785675, 7.208316651077764092 ) ) ;
#94984 = CARTESIAN_POINT ( 'NONE',  ( 7.361572987183169658, 19.96726448433411960, -9.846743663894592657 ) ) ;
#94985 = CARTESIAN_POINT ( 'NONE',  ( 14.92337183194729633, 7.675597817667451750, 8.527530157486181039 ) ) ;
#94986 = CARTESIAN_POINT ( 'NONE',  ( 17.20831665107776587, 2.883931151000785231, 7.208316651077764980 ) ) ;
#94987 = AXIS2_PLACEMENT_3D ( 'NONE', #85144, #4110, #35576 ) ;
#94988 = EDGE_CURVE ( 'NONE', #70649, #33114, #75604, .T. ) ;
#94989 = CARTESIAN_POINT ( 'NONE',  ( 2.035157376598824452, 63.68868534415484106, 7.964842623401179544 ) ) ;
#94990 = CARTESIAN_POINT ( 'NONE',  ( 4.559911319644449179, 62.23035201082150536, -9.422509992056141925 ) ) ;
#94992 = VERTEX_POINT ( 'NONE', #38600 ) ;
#94991 = CARTESIAN_POINT ( 'NONE',  ( 2.791683348922237240, 20.38393115100078745, -7.208316651077763204 ) ) ;
#94993 = B_SPLINE_CURVE_WITH_KNOTS ( 'NONE', 3,
 ( #84564, #6717, #96748, #36731 ),
 .UNSPECIFIED., .F., .F.,
 ( 4, 4 ),
 ( 1.321126039445492370E-17, 0.002562518741975311660 ),
 .UNSPECIFIED. ) ;
#94994 = CARTESIAN_POINT ( 'NONE',  ( -5.999999999999994671, 43.00000000000000000, 6.250000000000000000 ) ) ;
#94995 = CARTESIAN_POINT ( 'NONE',  ( 12.63842701281683922, 59.55059781766744464, -9.846743663894590881 ) ) ;
#94996 = ORIENTED_EDGE ( 'NONE', *, *, #34653, .T. ) ;
#94997 = CARTESIAN_POINT ( 'NONE',  ( -42.94000000000001194, 92.00000000000000000, -10.09898361729590199 ) ) ;
#94998 = CARTESIAN_POINT ( 'NONE',  ( 20.36894250292379382, 3.678748834913967869, 10.36894250292379205 ) ) ;
#94999 = CARTESIAN_POINT ( 'NONE',  ( 0.000000000000000000, 0.5000000000000004441, 0.000000000000000000 ) ) ;
#95000 = CARTESIAN_POINT ( 'NONE',  ( -4.164238869374099927, 12.01208216824730357, 3.795296366450308767 ) ) ;
#95001 = CARTESIAN_POINT ( 'NONE',  ( 13.79529636645030344, 28.26208216824729647, 14.16423886937410614 ) ) ;
#95002 =( LENGTH_UNIT ( ) NAMED_UNIT ( * ) SI_UNIT ( .MILLI., .METRE. ) );
#95003 = CARTESIAN_POINT ( 'NONE',  ( 6.204703633549690345, 2.845415501580634388, 14.16423886937410082 ) ) ;
#95004 = CARTESIAN_POINT ( 'NONE',  ( 20.88017736071110164, 35.35535201082150536, 2.915334737309930979 ) ) ;
#95005 = ORIENTED_EDGE ( 'NONE', *, *, #69909, .F. ) ;
#95006 = CARTESIAN_POINT ( 'NONE',  ( 18.52753015748618282, 18.92559781766745175, -4.923371831947291888 ) ) ;
#95008 = CARTESIAN_POINT ( 'NONE',  ( 19.84674366389459266, 13.71726448433411782, -2.638427012816827677 ) ) ;
#95007 = CARTESIAN_POINT ( 'NONE',  ( 4.559911319644449179, 52.23035201082151247, -9.422509992056141925 ) ) ;
#95009 = CARTESIAN_POINT ( 'NONE',  ( 19.38216949554541202, 40.99863466993042493, 9.382169495545424454 ) ) ;
#95010 = CARTESIAN_POINT ( 'NONE',  ( 14.92337183194729988, 39.34226448433412315, -8.527530157486177487 ) ) ;
#95011 = DIRECTION ( 'NONE',  ( 1.000000000000000000, -0.000000000000000000, -0.000000000000000000 ) ) ;
#95012 = CARTESIAN_POINT ( 'NONE',  ( 21.09922568453594849, 26.20696800326375353, 6.408140936763242479 ) ) ;
#95013 = CARTESIAN_POINT ( 'NONE',  ( 3.795296366450314540, -36.73791783175269643, 14.16423886937410082 ) ) ;
#95014 = CARTESIAN_POINT ( 'NONE',  ( 2.791683348922237240, 30.38393115100078390, -7.208316651077763204 ) ) ;
#95015 = CARTESIAN_POINT ( 'NONE',  ( -2.266590686148945544, 17.22041550158063572, 7.082119434687048631 ) ) ;
#95016 =( GEOMETRIC_REPRESENTATION_CONTEXT ( 3 ) GLOBAL_UNCERTAINTY_ASSIGNED_CONTEXT ( ( #67471 ) ) GLOBAL_UNIT_ASSIGNED_CONTEXT ( ( #27736, #4269, #87745 ) ) REPRESENTATION_CONTEXT ( 'NONE', 'WORKASPACE' ) );
#95017 = ORIENTED_EDGE ( 'NONE', *, *, #86978, .T. ) ;
#95018 = COLOUR_RGB ( '', 0.72549020, 0.75294118, 0.79215686) ;
#95019 = CARTESIAN_POINT ( 'NONE',  ( 20.88017736071110519, 35.56368534415484106, 2.639326808657452039E-16 ) ) ;
#95020 = CARTESIAN_POINT ( 'NONE',  ( -0.8801773607110991993, 52.85535201082151247, -2.915334737309923874 ) ) ;
#95021 = CARTESIAN_POINT ( 'NONE',  ( -4.164238869374099039, 46.80374883491397497, 8.674139862899312516E-16 ) ) ;
#95022 = CARTESIAN_POINT ( 'NONE',  ( 14.92337183194729633, 57.67559781766745886, 8.527530157486181039 ) ) ;
#95023 = CARTESIAN_POINT ( 'NONE',  ( 0.1532563361054083140, 6.008931151000784787, 1.131784320476157264E-15 ) ) ;
#95025 = CARTESIAN_POINT ( 'NONE',  ( -12.16982443903230759, 90.48687232357862342, 7.214476785723132224 ) ) ;
#95024 = CARTESIAN_POINT ( 'NONE',  ( -14.52844422123737012, 14.99999999999803713, -1.683098224411851307 ) ) ;
#95026 = CARTESIAN_POINT ( 'NONE',  ( 12.91533473730993009, 46.60535201082150536, -10.88017736071109987 ) ) ;
#95027 = DIRECTION ( 'NONE',  ( -0.000000000000000000, -0.000000000000000000, -1.000000000000000000 ) ) ;
#95028 = CARTESIAN_POINT ( 'NONE',  ( 21.09922568453594849, 26.20696800326375353, 6.408140936763242479 ) ) ;
#95029 = CARTESIAN_POINT ( 'NONE',  ( 19.84674366389459621, 53.50893115100078745, 7.409399052514197653E-17 ) ) ;
#95030 = CARTESIAN_POINT ( 'NONE',  ( 9.422509992056141925, 10.14701867748817676, 5.440088680355547268 ) ) ;
#95031 = CARTESIAN_POINT ( 'NONE',  ( 10.00000000000000178, 4.313685344154837509, 10.88017736071110342 ) ) ;
#95032 = CARTESIAN_POINT ( 'NONE',  ( 0.5774900079438607392, 63.48035201082149825, 5.440088680355550821 ) ) ;
#95033 = DIRECTION ( 'NONE',  ( 0.000000000000000000, 1.000000000000000000, 0.000000000000000000 ) ) ;
#95034 = ADVANCED_FACE ( 'NONE', ( #67116 ), #75107, .T. ) ;
#95035 = FACE_OUTER_BOUND ( 'NONE', #72585, .T. ) ;
#95036 = CARTESIAN_POINT ( 'NONE',  ( 20.88017736071110875, 65.77201867748817676, -2.915334737309920765 ) ) ;
#95037 = CARTESIAN_POINT ( 'NONE',  ( 10.00000000000000000, 66.81368534415484817, -10.88017736071110342 ) ) ;
#95038 = CARTESIAN_POINT ( 'NONE',  ( 17.99999999999999645, 78.80384757729335377, -3.999999999999996891 ) ) ;
#95039 = CIRCLE ( 'NONE', #29580, 15.00000000000000000 ) ;
#95040 = CARTESIAN_POINT ( 'NONE',  ( 17.20831665107776587, 37.88393115100078745, 7.208316651077764980 ) ) ;
#95041 = EDGE_CURVE ( 'NONE', #48119, #80255, #30585, .T. ) ;
#95042 = CARTESIAN_POINT ( 'NONE',  ( 4.559911319644449179, 22.23035201082150536, -9.422509992056141925 ) ) ;
#95043 = CARTESIAN_POINT ( 'NONE',  ( 6.565887622018943937, 0.1653013365970866511, 12.81628187352647430 ) ) ;
#95045 = CARTESIAN_POINT ( 'NONE',  ( -4.536162299966319367, -17.54167381550513838, -3.750000000000000000 ) ) ;
#95044 = CARTESIAN_POINT ( 'NONE',  ( 19.42250999205614548, 35.98035201082151247, -5.440088680355545492 ) ) ;
#95046 = FACE_OUTER_BOUND ( 'NONE', #29347, .T. ) ;
#95047 = CARTESIAN_POINT ( 'NONE',  ( 16.40814093676324603, 32.45696800326375353, -11.09922568453594671 ) ) ;
#95048 = ORIENTED_EDGE ( 'NONE', *, *, #85248, .T. ) ;
#95049 = CARTESIAN_POINT ( 'NONE',  ( 15.44008868035555793, 51.39701867748816966, -9.422509992056140149 ) ) ;
#95050 = CARTESIAN_POINT ( 'NONE',  ( 16.40814093676324603, 22.45696800326375353, -11.09922568453594671 ) ) ;
#95051 = CARTESIAN_POINT ( 'NONE',  ( 12.91533473730992121, 24.52201867748816966, 10.88017736071110164 ) ) ;
#95052 = CARTESIAN_POINT ( 'NONE',  ( 2.917880565312950480, 65.97041550158063217, -12.26659068614894821 ) ) ;
#95053 = CARTESIAN_POINT ( 'NONE',  ( 0.1532563361054100626, 45.80059781766745886, -2.638427012816831230 ) ) ;
#95054 = CARTESIAN_POINT ( 'NONE',  ( 19.84674366389459266, 3.300597817667451750, 2.638427012816836559 ) ) ;
#95055 = CARTESIAN_POINT ( 'NONE',  ( 15.44008868035555793, 56.39701867748817676, -9.422509992056140149 ) ) ;
#95056 = CARTESIAN_POINT ( 'NONE',  ( -8.502721643905040594, 14.95037103750416563, -12.05657636697581658 ) ) ;
#95057 = CARTESIAN_POINT ( 'NONE',  ( 20.36894250292379382, 33.67874883491396076, 10.36894250292379205 ) ) ;
#95058 = EDGE_CURVE ( 'NONE', #37334, #5292, #6613, .T. ) ;
#95059 = AXIS2_PLACEMENT_3D ( 'NONE', #7356, #46810, #60338 ) ;
#95060 = FACE_OUTER_BOUND ( 'NONE', #38021, .T. ) ;
#95061 = CARTESIAN_POINT ( 'NONE',  ( -10.88853822400146854, 46.97908644289115898, -3.000000000000000000 ) ) ;
#95062 = ORIENTED_EDGE ( 'NONE', *, *, #43644, .F. ) ;
#95063 = ORIENTED_EDGE ( 'NONE', *, *, #3061, .F. ) ;
#95064 = CARTESIAN_POINT ( 'NONE',  ( 22.26659068614894466, 53.88708216824731068, 7.082119434687054849 ) ) ;
#95065 = CARTESIAN_POINT ( 'NONE',  ( -0.3689425029237881626, 52.42874883491396076, 10.36894250292379027 ) ) ;
#95066 = CARTESIAN_POINT ( 'NONE',  ( 2.791683348922237240, 15.38393115100078212, -7.208316651077763204 ) ) ;
#95067 = EDGE_CURVE ( 'NONE', #12737, #325, #95847, .T. ) ;
#95069 = CARTESIAN_POINT ( 'NONE',  ( 10.00000000000000178, 15.37363466993042138, 12.81628187352647608 ) ) ;
#95068 = AXIS2_PLACEMENT_3D ( 'NONE', #70861, #85856, #86837 ) ;
#95070 = CARTESIAN_POINT ( 'NONE',  ( 10.58521204051726627, -0.03417435944610275333, 11.99294302885416563 ) ) ;
#95071 = CARTESIAN_POINT ( 'NONE',  ( 4.999999999999999112, 11.50000000000000000, 6.500000000000000888 ) ) ;
#95072 = CARTESIAN_POINT ( 'NONE',  ( 0.6178305044545818747, 28.49863466993041783, -9.382169495545419124 ) ) ;
#95073 = CARTESIAN_POINT ( 'NONE',  ( 22.26659068614894466, 43.88708216824729647, 7.082119434687054849 ) ) ;
#95074 = DIRECTION ( 'NONE',  ( 0.000000000000000000, 1.000000000000000000, -0.000000000000000000 ) ) ;
#95075 =( NAMED_UNIT ( * ) SI_UNIT ( $, .STERADIAN. ) SOLID_ANGLE_UNIT ( ) );
#95076 = EDGE_CURVE ( 'NONE', #40011, #74673, #45598, .T. ) ;
#95077 = CARTESIAN_POINT ( 'NONE',  ( 4.923371831947301658, 2.675597817667456191, 8.527530157486175710 ) ) ;
#95078 = ORIENTED_EDGE ( 'NONE', *, *, #69598, .T. ) ;
#95079 = AXIS2_PLACEMENT_3D ( 'NONE', #72005, #11505, #12490 ) ;
#95080 = FACE_OUTER_BOUND ( 'NONE', #46028, .T. ) ;
#95081 = CARTESIAN_POINT ( 'NONE',  ( 5.076628168052703671, 16.84226448433411960, 8.527530157486179263 ) ) ;
#95082 = ORIENTED_EDGE ( 'NONE', *, *, #69435, .F. ) ;
#95084 = CARTESIAN_POINT ( 'NONE',  ( 0.5774900079438607392, 8.480352010821505360, 5.440088680355550821 ) ) ;
#95083 = CARTESIAN_POINT ( 'NONE',  ( 17.96484262340118221, 11.18868534415484106, -7.964842623401177768 ) ) ;
#95086 = CARTESIAN_POINT ( 'NONE',  ( -1.099225684535947600, 3.706968003263753531, -6.408140936763238038 ) ) ;
#95085 = CARTESIAN_POINT ( 'NONE',  ( 17.20831665107776587, 54.13393115100079456, -7.208316651077762316 ) ) ;
#95087 = CIRCLE ( 'NONE', #40864, 15.00000000000000000 ) ;
#95088 = VECTOR ( 'NONE', #75457, 1000.000000000000000 ) ;
#95090 = CARTESIAN_POINT ( 'NONE',  ( 6.565887622018943937, 15.16530133659708568, 12.81628187352647430 ) ) ;
#95089 =( GEOMETRIC_REPRESENTATION_CONTEXT ( 3 ) GLOBAL_UNCERTAINTY_ASSIGNED_CONTEXT ( ( #33501 ) ) GLOBAL_UNIT_ASSIGNED_CONTEXT ( ( #22022, #66516, #90980 ) ) REPRESENTATION_CONTEXT ( 'NONE', 'WORKASPACE' ) );
#95091 = EDGE_LOOP ( 'NONE', ( #35475, #32236, #83559, #21084, #93012, #29098 ) ) ;
#95092 = CARTESIAN_POINT ( 'NONE',  ( 22.26659068614894466, 58.88708216824729647, 7.082119434687054849 ) ) ;
#95093 = ORIENTED_EDGE ( 'NONE', *, *, #7658, .F. ) ;
#95094 = CARTESIAN_POINT ( 'NONE',  ( -4.164238869374098151, 61.59541550158063217, -3.795296366450310543 ) ) ;
#95095 = ORIENTED_EDGE ( 'NONE', *, *, #74804, .F. ) ;
#95096 = CARTESIAN_POINT ( 'NONE',  ( 4.559911319644449179, 28.89701867748817321, 9.422509992056141925 ) ) ;
#95097 = CARTESIAN_POINT ( 'NONE',  ( 17.96484262340118221, 41.18868534415484106, -7.964842623401177768 ) ) ;
#95098 = CARTESIAN_POINT ( 'NONE',  ( 19.42250999205614548, 55.98035201082150536, -5.440088680355545492 ) ) ;
#95099 = SURFACE_SIDE_STYLE ('',( #73084 ) ) ;
#95100 = CARTESIAN_POINT ( 'NONE',  ( 7.084665262690076126, 47.02201867748818387, -10.88017736071110164 ) ) ;
#95101 = EDGE_CURVE ( 'NONE', #44442, #50694, #30090, .T. ) ;
#95102 = CARTESIAN_POINT ( 'NONE',  ( -5.991992585808714189, 4.061121054423934144E-16, 13.20401548210291054 ) ) ;
#95103 = VECTOR ( 'NONE', #83106, 1000.000000000000000 ) ;
#95104 = CARTESIAN_POINT ( 'NONE',  ( 12.63842701281683034, 12.46726448433411782, 9.846743663894596210 ) ) ;
#95105 = ORIENTED_EDGE ( 'NONE', *, *, #18604, .T. ) ;
#95106 = CARTESIAN_POINT ( 'NONE',  ( 11.43665280317779676, -81.62088987012548102, 3.750000000000000000 ) ) ;
#95107 = CARTESIAN_POINT ( 'NONE',  ( 1.472469842513823179, 41.42559781766745886, 4.923371831947296329 ) ) ;
#95108 = DIRECTION ( 'NONE',  ( 0.000000000000000000, -0.000000000000000000, -1.000000000000000000 ) ) ;
#95109 = CARTESIAN_POINT ( 'NONE',  ( 10.00000000000000178, 50.37363466993042493, 12.81628187352647608 ) ) ;
#95110 = CARTESIAN_POINT ( 'NONE',  ( -5.204170427930421283E-15, 11.41212336850781739, -11.92686044187656513 ) ) ;
#95111 = ORIENTED_EDGE ( 'NONE', *, *, #57106, .T. ) ;
#95112 = DIRECTION ( 'NONE',  ( 0.000000000000000000, -1.000000000000000000, 0.000000000000000000 ) ) ;
#95113 = FACE_OUTER_BOUND ( 'NONE', #5465, .T. ) ;
#95114 = FACE_OUTER_BOUND ( 'NONE', #16955, .T. ) ;
#95115 = CARTESIAN_POINT ( 'NONE',  ( 6.204703633549690345, 65.76208216824731778, -14.16423886937410259 ) ) ;
#95116 = CARTESIAN_POINT ( 'NONE',  ( 1.472469842513823179, 66.42559781766745175, 4.923371831947296329 ) ) ;
#95117 = ORIENTED_EDGE ( 'NONE', *, *, #65020, .F. ) ;
#95118 = CYLINDRICAL_SURFACE ( 'NONE', #41644, 0.5000000000000000000 ) ;
#95119 = CARTESIAN_POINT ( 'NONE',  ( 10.00000000000000000, 34.75893115100078745, -9.846743663894594434 ) ) ;
#95120 = CARTESIAN_POINT ( 'NONE',  ( 22.81628187352647785, 61.62363466993041783, 6.195893100308588602E-16 ) ) ;
#95121 = CIRCLE ( 'NONE', #32823, 14.49999999999999822 ) ;
#95122 = CARTESIAN_POINT ( 'NONE',  ( -1.099225684535947600, 3.706968003263753531, -6.408140936763238038 ) ) ;
#95123 = CARTESIAN_POINT ( 'NONE',  ( 19.84674366389459266, 3.300597817667451750, 2.638427012816836559 ) ) ;
#95124 = CARTESIAN_POINT ( 'NONE',  ( -6.000000000000000000, 78.07179676972447169, -6.250000000000000000 ) ) ;
#95125 = CARTESIAN_POINT ( 'NONE',  ( 2.791683348922237240, 15.38393115100078212, -7.208316651077763204 ) ) ;
#95126 = CARTESIAN_POINT ( 'NONE',  ( 12.63842701281683034, 52.46726448433413026, 9.846743663894596210 ) ) ;
#95127 = CARTESIAN_POINT ( 'NONE',  ( 0.7166339456633684657, 0.000000000000000000, -15.98010739087745868 ) ) ;
#95128 = ORIENTED_EDGE ( 'NONE', *, *, #54940, .F. ) ;
#95129 = CARTESIAN_POINT ( 'NONE',  ( 2.917880565312948704, 62.63708216824730357, 12.26659068614894643 ) ) ;
#95130 = CARTESIAN_POINT ( 'NONE',  ( 20.36894250292379382, 8.678748834913967869, 10.36894250292379205 ) ) ;
#95131 = CARTESIAN_POINT ( 'NONE',  ( 15.44008868035555793, 41.39701867748817676, -9.422509992056140149 ) ) ;
#95133 = CARTESIAN_POINT ( 'NONE',  ( 4.559911319644449179, 67.23035201082150536, -9.422509992056141925 ) ) ;
#95132 = CARTESIAN_POINT ( 'NONE',  ( 6.565887622018943937, 28.08196800326375353, -12.81628187352647608 ) ) ;
#95134 = SURFACE_STYLE_FILL_AREA ( #19642 ) ;
#95135 = CARTESIAN_POINT ( 'NONE',  ( -42.50369195530269195, 107.9060299417078426, -4.500000000000001776 ) ) ;
#95136 = CARTESIAN_POINT ( 'NONE',  ( 9.011287250621787592, 0.2306972965111906138, -11.91783356064788535 ) ) ;
#95137 = CARTESIAN_POINT ( 'NONE',  ( 12.63842701281683922, 54.55059781766745175, -9.846743663894590881 ) ) ;
#95138 = CARTESIAN_POINT ( 'NONE',  ( 0.1532563361054100626, 10.80059781766745175, -2.638427012816831230 ) ) ;
#95139 = CARTESIAN_POINT ( 'NONE',  ( -2.915334737309934532, -22.97798132251182324, -10.88017736071109987 ) ) ;
#95140 = CARTESIAN_POINT ( 'NONE',  ( 21.09922568453594849, 21.20696800326375353, 6.408140936763242479 ) ) ;
#95141 = CARTESIAN_POINT ( 'NONE',  ( -14.16722289976693894, 14.49999999999999112, 4.928467845925465163 ) ) ;
#95142 = EDGE_CURVE ( 'NONE', #54039, #4498, #88637, .T. ) ;
#95144 = CARTESIAN_POINT ( 'NONE',  ( 8.549892366338765370, 0.2306972965111890594, 12.25305656628361106 ) ) ;
#95143 = CARTESIAN_POINT ( 'NONE',  ( 17.96484262340118221, 31.18868534415483751, -7.964842623401177768 ) ) ;
#95145 = CARTESIAN_POINT ( 'NONE',  ( -10.17177286909455525, 14.76984972048479783, -10.94336654633696604 ) ) ;
#95146 = CARTESIAN_POINT ( 'NONE',  ( 22.26659068614895176, 54.72041550158063217, -7.082119434687042414 ) ) ;
#95147 = CARTESIAN_POINT ( 'NONE',  ( 2.917880565312950480, 35.97041550158063217, -12.26659068614894821 ) ) ;
#95148 = COLOUR_RGB ( '', 0.09019608, 0.27058824, 0.51372549) ;
#95149 = CARTESIAN_POINT ( 'NONE',  ( 2.791683348922240793, 41.63393115100078745, 7.208316651077764092 ) ) ;
#95150 = ADVANCED_FACE ( 'NONE', ( #91092 ), #69098, .T. ) ;
#95151 = CARTESIAN_POINT ( 'NONE',  ( 21.09922568453594849, 31.20696800326375353, 6.408140936763242479 ) ) ;
#95152 = CARTESIAN_POINT ( 'NONE',  ( 20.88017736071110875, 25.77201867748816966, -2.915334737309920765 ) ) ;
#95153 = ADVANCED_FACE ( 'NONE', ( #68607 ), #84594, .F. ) ;
#95154 = CARTESIAN_POINT ( 'NONE',  ( 7.361572987183169658, 54.96726448433413026, -9.846743663894592657 ) ) ;
#95155 = CARTESIAN_POINT ( 'NONE',  ( 7.084665262690076126, 37.02201867748817676, -10.88017736071110164 ) ) ;
#95156 = CARTESIAN_POINT ( 'NONE',  ( -2.816281873526473856, 4.123634669930420493, 9.499525473075851096E-16 ) ) ;
#95157 = CARTESIAN_POINT ( 'NONE',  ( 2.917880565312950480, 15.97041550158063217, -12.26659068614894821 ) ) ;
#95158 = PLANE ( 'NONE',  #82292 ) ;
#95159 = TOROIDAL_SURFACE ( 'NONE', #74389, 14.49999999999999822, 0.5000000000000000000 ) ;
#95160 = EDGE_CURVE ( 'NONE', #55238, #33937, #22620, .T. ) ;
#95161 = CARTESIAN_POINT ( 'NONE',  ( 7.361572987183169658, 19.96726448433411960, -9.846743663894592657 ) ) ;
#95162 = FILL_AREA_STYLE_COLOUR ( '', #7319 ) ;
#95163 = CARTESIAN_POINT ( 'NONE',  ( 10.00000000000000178, 62.25893115100078745, 9.846743663894594434 ) ) ;
#95164 = VERTEX_POINT ( 'NONE', #36632 ) ;
#95165 = CARTESIAN_POINT ( 'NONE',  ( -9.000000000000003553, 80.99999999999994316, 0.000000000000000000 ) ) ;
#95166 = CARTESIAN_POINT ( 'NONE',  ( 6.452519493965914954, -47.68837976023561964, 3.750000000000001776 ) ) ;
#95167 = CARTESIAN_POINT ( 'NONE',  ( 20.36894250292379382, 63.67874883491396787, 10.36894250292379205 ) ) ;
#95168 = CARTESIAN_POINT ( 'NONE',  ( 17.08211943468705840, 15.13708216824730179, -12.26659068614894466 ) ) ;
#95169 = CARTESIAN_POINT ( 'NONE',  ( 20.88017736071110875, 65.77201867748817676, -2.915334737309920765 ) ) ;
#95170 = CARTESIAN_POINT ( 'NONE',  ( 2.791683348922237240, 50.38393115100078035, -7.208316651077763204 ) ) ;
#95171 = CARTESIAN_POINT ( 'NONE',  ( 0.5774900079438607392, 33.48035201082150536, 5.440088680355550821 ) ) ;
#95172 = CARTESIAN_POINT ( 'NONE',  ( -6.982525766850298687, -88.11956318484570261, 3.750000000000000000 ) ) ;
#95173 = CARTESIAN_POINT ( 'NONE',  ( 14.92337183194729633, 57.67559781766745886, 8.527530157486181039 ) ) ;
#95174 = ADVANCED_FACE ( 'NONE', ( #97641 ), #15123, .F. ) ;
#95175 = ORIENTED_EDGE ( 'NONE', *, *, #63531, .F. ) ;
#95176 = CARTESIAN_POINT ( 'NONE',  ( 12.34086200392826882, 15.00000000000000000, -7.124999999999971578 ) ) ;
#95177 = ORIENTED_EDGE ( 'NONE', *, *, #51630, .F. ) ;
#95178 = ORIENTED_EDGE ( 'NONE', *, *, #13361, .T. ) ;
#95179 = CARTESIAN_POINT ( 'NONE',  ( 24.16423886937410614, 9.512082168247301794, -3.795296366450302550 ) ) ;
#95180 = CARTESIAN_POINT ( 'NONE',  ( 17.08211943468705840, 10.13708216824730179, -12.26659068614894466 ) ) ;
#95181 = CARTESIAN_POINT ( 'NONE',  ( 24.16423886937409904, 59.09541550158063217, 3.795296366450317205 ) ) ;
#95182 = CARTESIAN_POINT ( 'NONE',  ( 17.20831665107776587, 62.88393115100078745, 7.208316651077764980 ) ) ;
#95183 = CARTESIAN_POINT ( 'NONE',  ( 0.1532563361054083140, 41.00893115100078745, 1.131784320476157264E-15 ) ) ;
#95184 = CARTESIAN_POINT ( 'NONE',  ( 14.49999999999999822, 60.50000000000000000, 5.000000000000000000 ) ) ;
#95186 = CARTESIAN_POINT ( 'NONE',  ( 10.00000000000000000, 59.75893115100078745, -9.846743663894594434 ) ) ;
#95185 = CARTESIAN_POINT ( 'NONE',  ( 20.88017736071110875, 35.77201867748816966, -2.915334737309920765 ) ) ;
#95187 = CARTESIAN_POINT ( 'NONE',  ( 22.26659068614894466, 8.887082168247300018, 7.082119434687054849 ) ) ;
#95188 = CARTESIAN_POINT ( 'NONE',  ( 10.00000000000000178, 58.05374883491397497, 14.16423886937410082 ) ) ;
#95189 = CARTESIAN_POINT ( 'NONE',  ( 20.88017736071110164, 10.35535201082150714, 2.915334737309930979 ) ) ;
#95190 = CARTESIAN_POINT ( 'NONE',  ( -0.2418659066527709955, 68.09014588040356841, 6.114288769123044531 ) ) ;
#95191 = DIRECTION ( 'NONE',  ( 0.1305261922200583458, 0.000000000000000000, -0.9914448613738096050 ) ) ;
#95192 = CARTESIAN_POINT ( 'NONE',  ( -0.8801773607111009756, 63.06368534415484106, 1.068504757029289695E-15 ) ) ;
#95193 = EDGE_CURVE ( 'NONE', #74944, #67813, #65972, .T. ) ;
#95194 = CARTESIAN_POINT ( 'NONE',  ( 18.52753015748618282, 23.92559781766745530, -4.923371831947291888 ) ) ;
#95195 = CARTESIAN_POINT ( 'NONE',  ( 14.03351048042397231, -0.03417435944610275333, -2.474486531753715024 ) ) ;
#95196 = ORIENTED_EDGE ( 'NONE', *, *, #33169, .F. ) ;
#95197 = DIRECTION ( 'NONE',  ( 0.000000000000000000, 0.000000000000000000, 1.000000000000000000 ) ) ;
#95198 = ORIENTED_EDGE ( 'NONE', *, *, #89735, .T. ) ;
#95199 = CARTESIAN_POINT ( 'NONE',  ( 18.52753015748618282, 18.92559781766745175, -4.923371831947291888 ) ) ;
#95200 = EDGE_LOOP ( 'NONE', ( #48958, #49670, #39048, #50340 ) ) ;
#95201 = VECTOR ( 'NONE', #77397, 1000.000000000000000 ) ;
#95202 = CARTESIAN_POINT ( 'NONE',  ( -4.164238869374098151, 31.59541550158063927, -3.795296366450310543 ) ) ;
#95203 = CARTESIAN_POINT ( 'NONE',  ( 0.1532563361054083140, 31.00893115100078390, 1.131784320476157264E-15 ) ) ;
#95204 = CARTESIAN_POINT ( 'NONE',  ( 7.084665262690076126, 57.02201867748817676, -10.88017736071110164 ) ) ;
#95205 = EDGE_CURVE ( 'NONE', #53280, #73183, #72539, .T. ) ;
#95206 = CARTESIAN_POINT ( 'NONE',  ( 20.88017736071110519, 50.56368534415484106, 2.639326808657452039E-16 ) ) ;
#95207 = CARTESIAN_POINT ( 'NONE',  ( 12.63842701281683922, 49.55059781766744464, -9.846743663894590881 ) ) ;
#95208 = CARTESIAN_POINT ( 'NONE',  ( 21.09922568453595559, 62.04030133659709634, -6.408140936763230044 ) ) ;
#95209 = CARTESIAN_POINT ( 'NONE',  ( 11.09922568453594671, 7.040301336597089232, -6.408140936763241591 ) ) ;
#95210 = MECHANICAL_DESIGN_GEOMETRIC_PRESENTATION_REPRESENTATION (  '', ( #25018 ), #34528 ) ;
#95211 = ORIENTED_EDGE ( 'NONE', *, *, #19747, .T. ) ;
#95212 = CARTESIAN_POINT ( 'NONE',  ( 13.79529636645030344, 18.26208216824730002, 14.16423886937410614 ) ) ;
#95213 = VERTEX_POINT ( 'NONE', #17582 ) ;
#95214 = EDGE_LOOP ( 'NONE', ( #63946, #3160, #58716, #10580 ) ) ;
#95215 = CARTESIAN_POINT ( 'NONE',  ( 21.09922568453595559, 27.04030133659708568, -6.408140936763230044 ) ) ;
#95216 = CARTESIAN_POINT ( 'NONE',  ( 18.52753015748617571, 18.09226448433411960, 4.923371831947298993 ) ) ;
#95217 = CARTESIAN_POINT ( 'NONE',  ( 20.88017736071110164, 5.355352010821502695, 2.915334737309930979 ) ) ;
#95218 = CARTESIAN_POINT ( 'NONE',  ( 0.6178305044545838731, 54.74863466993042493, 9.382169495545420901 ) ) ;
#95219 = CARTESIAN_POINT ( 'NONE',  ( 12.83294900548062678, 14.49999999999999112, 7.766300266068507874 ) ) ;
#95220 = CARTESIAN_POINT ( 'NONE',  ( 12.63842701281683922, 24.55059781766745175, -9.846743663894590881 ) ) ;
#95222 = MECHANICAL_DESIGN_GEOMETRIC_PRESENTATION_REPRESENTATION (  '', ( #31353 ), #93662 ) ;
#95221 = CARTESIAN_POINT ( 'NONE',  ( 10.00000000000000178, 69.31368534415484817, 10.88017736071110342 ) ) ;
#95223 = DIRECTION ( 'NONE',  ( 0.000000000000000000, -1.000000000000000000, 0.000000000000000000 ) ) ;
#95224 = DIRECTION ( 'NONE',  ( 0.000000000000000000, 0.000000000000000000, 1.000000000000000000 ) ) ;
#95225 = CARTESIAN_POINT ( 'NONE',  ( 20.05723567505239302, 69.83236346210667023, 6.413539670616450472 ) ) ;
#95226 = CARTESIAN_POINT ( 'NONE',  ( 13.48255862861923937, 4.031870098369226268E-16, 5.335786055104250636 ) ) ;
#95227 = CARTESIAN_POINT ( 'NONE',  ( 7.361572987183169658, 4.967264484334119601, -9.846743663894592657 ) ) ;
#95228 = CARTESIAN_POINT ( 'NONE',  ( -2.816281873526473856, 29.12363466993041783, 9.499525473075851096E-16 ) ) ;
#95229 = PRESENTATION_STYLE_ASSIGNMENT (( #3769 ) ) ;
#95230 = ADVANCED_FACE ( 'NONE', ( #78068 ), #74179, .T. ) ;
#95231 = CARTESIAN_POINT ( 'NONE',  ( 14.92337183194729988, 49.34226448433411605, -8.527530157486177487 ) ) ;
#95232 = DIRECTION ( 'NONE',  ( -0.000000000000000000, -1.000000000000000000, -0.000000000000000000 ) ) ;
#95233 = CARTESIAN_POINT ( 'NONE',  ( -4.164238869374099039, 21.80374883491396787, 8.674139862899312516E-16 ) ) ;
#95234 = CARTESIAN_POINT ( 'NONE',  ( 12.63842701281683922, 34.55059781766745886, -9.846743663894590881 ) ) ;
#95235 = CARTESIAN_POINT ( 'NONE',  ( 16.40814093676324603, 37.45696800326376064, -11.09922568453594671 ) ) ;
#95237 = FACE_OUTER_BOUND ( 'NONE', #44820, .T. ) ;
#95236 = DIRECTION ( 'NONE',  ( -0.5664062369248369366, 0.000000000000000000, 0.8241261886220128119 ) ) ;
#95238 = CARTESIAN_POINT ( 'NONE',  ( 0.5774900079438607392, 63.48035201082149825, 5.440088680355550821 ) ) ;
#95239 = CARTESIAN_POINT ( 'NONE',  ( -2.816281873526473856, 9.331968003263753531, 3.434112377981055619 ) ) ;
#95240 = AXIS2_PLACEMENT_3D ( 'NONE', #63776, #39823, #94780 ) ;
#95241 = CARTESIAN_POINT ( 'NONE',  ( 0.1532563361054100626, 40.80059781766745886, -2.638427012816831230 ) ) ;
#95242 = EDGE_CURVE ( 'NONE', #25004, #38304, #10072, .T. ) ;
#95243 = CARTESIAN_POINT ( 'NONE',  ( 18.52753015748618282, 28.92559781766745175, -4.923371831947291888 ) ) ;
#95244 = CARTESIAN_POINT ( 'NONE',  ( 2.035157376598824452, 28.68868534415484106, 7.964842623401179544 ) ) ;
#95245 = CARTESIAN_POINT ( 'NONE',  ( 16.40814093676323893, 30.79030133659708923, 11.09922568453595026 ) ) ;
#95246 = VECTOR ( 'NONE', #64960, 1000.000000000000227 ) ;
#95247 = CARTESIAN_POINT ( 'NONE',  ( 19.84674366389459621, 23.50893115100078390, 7.409399052514197653E-17 ) ) ;
#95248 = STYLED_ITEM ( 'NONE', ( #11873 ), #72940 ) ;
#95249 = CARTESIAN_POINT ( 'NONE',  ( 0.000000000000000000, 0.000000000000000000, 0.000000000000000000 ) ) ;
#95250 = CARTESIAN_POINT ( 'NONE',  ( -12.24686443627862964, 90.44926614966664147, 7.163467944141830301 ) ) ;
#95251 = AXIS2_PLACEMENT_3D ( 'NONE', #50622, #81113, #66610 ) ;
#95252 = CARTESIAN_POINT ( 'NONE',  ( 19.42250999205614548, 35.98035201082151247, -5.440088680355545492 ) ) ;
#95253 = ORIENTED_EDGE ( 'NONE', *, *, #81629, .F. ) ;
#95254 = CARTESIAN_POINT ( 'NONE',  ( 4.559911319644449179, 62.23035201082150536, -9.422509992056141925 ) ) ;
#95255 = CARTESIAN_POINT ( 'NONE',  ( 12.91533473730992121, 4.522018677488169658, 10.88017736071110164 ) ) ;
#95257 = CARTESIAN_POINT ( 'NONE',  ( 17.96484262340118221, 29.93868534415484106, 7.964842623401181321 ) ) ;
#95256 = CARTESIAN_POINT ( 'NONE',  ( 10.00000000000000000, 59.75893115100078745, -9.846743663894594434 ) ) ;
#95258 = DIRECTION ( 'NONE',  ( 0.000000000000000000, 0.000000000000000000, -1.000000000000000000 ) ) ;
#95259 = CARTESIAN_POINT ( 'NONE',  ( 20.88017736071110164, 50.35535201082151247, 2.915334737309930979 ) ) ;
#95261 = CARTESIAN_POINT ( 'NONE',  ( 20.00000000000000711, 85.79222437201613616, -4.885465336098351763 ) ) ;
#95260 = CARTESIAN_POINT ( 'NONE',  ( 4.559911319644449179, 12.23035201082150714, -9.422509992056141925 ) ) ;
#95262 = CARTESIAN_POINT ( 'NONE',  ( 0.000000000000000000, 81.99999999999992895, -5.000000000000000000 ) ) ;
#95263 = CARTESIAN_POINT ( 'NONE',  ( 5.500000000000000000, 11.50000000000000000, -5.000000000000000000 ) ) ;
#95264 = CARTESIAN_POINT ( 'NONE',  ( 19.84674366389459266, 58.30059781766745886, 2.638427012816836559 ) ) ;
#95265 = CARTESIAN_POINT ( 'NONE',  ( -0.3689425029237881626, 57.42874883491397497, 10.36894250292379027 ) ) ;
#95266 = CIRCLE ( 'NONE', #56945, 11.99999999999999645 ) ;
#95267 = CARTESIAN_POINT ( 'NONE',  ( 12.50534872682727539, 3.894361491432412218E-16, 7.339363270777609749 ) ) ;
#95268 = CARTESIAN_POINT ( 'NONE',  ( -12.21238578215998771, 15.00000000000000888, -8.049595036947295057 ) ) ;
#95269 = CARTESIAN_POINT ( 'NONE',  ( -4.164238869374099039, 31.80374883491396432, 8.674139862899312516E-16 ) ) ;
#95270 = STYLED_ITEM ( 'NONE', ( #58583 ), #41174 ) ;
#95271 = EDGE_CURVE ( 'NONE', #50559, #69353, #40572, .T. ) ;
#95272 = DIRECTION ( 'NONE',  ( -1.000000000000000000, -0.000000000000000000, -0.000000000000000000 ) ) ;
#95273 = ORIENTED_EDGE ( 'NONE', *, *, #22580, .T. ) ;
#95274 = CARTESIAN_POINT ( 'NONE',  ( 2.917880565312948704, 67.63708216824730357, 12.26659068614894643 ) ) ;
#95275 = CARTESIAN_POINT ( 'NONE',  ( 18.52753015748618282, 33.92559781766745886, -4.923371831947291888 ) ) ;
#95277 = CARTESIAN_POINT ( 'NONE',  ( -8.352412229647901754, 86.23350694210130030, -4.048761466749791538 ) ) ;
#95276 = CARTESIAN_POINT ( 'NONE',  ( -6.732636091893172470, -88.11213685669366669, -3.250000000000000000 ) ) ;
#95278 = CARTESIAN_POINT ( 'NONE',  ( 10.00000000000000178, 54.31368534415484106, 10.88017736071110342 ) ) ;
#95279 = FACE_OUTER_BOUND ( 'NONE', #39721, .T. ) ;
#95280 = EDGE_CURVE ( 'NONE', #875, #95488, #17090, .T. ) ;
#95281 = CIRCLE ( 'NONE', #15522, 0.5000000000000004441 ) ;
#95282 = CARTESIAN_POINT ( 'NONE',  ( 15.44008868035555793, 26.39701867748817321, -9.422509992056140149 ) ) ;
#95283 = FACE_OUTER_BOUND ( 'NONE', #90550, .T. ) ;
#95284 = CARTESIAN_POINT ( 'NONE',  ( 19.38216949554541557, 17.24863466993041783, -9.382169495545420901 ) ) ;
#95285 = CARTESIAN_POINT ( 'NONE',  ( 17.20831665107776587, 17.88393115100078745, 7.208316651077764980 ) ) ;
#95286 = VERTEX_POINT ( 'NONE', #71069 ) ;
#95287 =( NAMED_UNIT ( * ) SI_UNIT ( $, .STERADIAN. ) SOLID_ANGLE_UNIT ( ) );
#95288 =( NAMED_UNIT ( * ) PLANE_ANGLE_UNIT ( ) SI_UNIT ( $, .RADIAN. ) );
#95289 = CARTESIAN_POINT ( 'NONE',  ( -4.164238869374099039, 66.80374883491396076, 8.674139862899312516E-16 ) ) ;
#95290 = CARTESIAN_POINT ( 'NONE',  ( -2.266590686148945544, 31.38708216824730002, -7.082119434687050408 ) ) ;
#95291 = CARTESIAN_POINT ( 'NONE',  ( -0.8801773607111009756, 28.06368534415484106, 1.068504757029289695E-15 ) ) ;
#95292 = CARTESIAN_POINT ( 'NONE',  ( 4.559911319644449179, 47.23035201082150536, -9.422509992056141925 ) ) ;
#95293 = CARTESIAN_POINT ( 'NONE',  ( -1.983216688681034068, -0.03417435944610275333, 14.11131997956736406 ) ) ;
#95294 = FILL_AREA_STYLE ('',( #18820 ) ) ;
#95295 = CARTESIAN_POINT ( 'NONE',  ( 14.92337183194729988, 9.342264484334119601, -8.527530157486177487 ) ) ;
#95296 = CARTESIAN_POINT ( 'NONE',  ( 6.000000000000000000, 10.49999999999999822, -6.500000000000000888 ) ) ;
#95297 = DIRECTION ( 'NONE',  ( 0.000000000000000000, 0.000000000000000000, -1.000000000000000000 ) ) ;
#95298 = CARTESIAN_POINT ( 'NONE',  ( -4.547378612396732578, 0.000000000000000000, -3.009844244835570670 ) ) ;
#95299 = CARTESIAN_POINT ( 'NONE',  ( 18.52753015748618282, 23.92559781766745530, -4.923371831947291888 ) ) ;
#95300 = CARTESIAN_POINT ( 'NONE',  ( 12.63842701281683922, 49.55059781766744464, -9.846743663894590881 ) ) ;
#95301 = CARTESIAN_POINT ( 'NONE',  ( -0.8801773607110991993, 27.85535201082150181, -2.915334737309923874 ) ) ;
#95302 = UNCERTAINTY_MEASURE_WITH_UNIT (LENGTH_MEASURE( 1.000000000000000082E-05 ), #16146, 'distance_accuracy_value', 'NONE');
#95303 = CARTESIAN_POINT ( 'NONE',  ( -2.816281873526471635, 48.91530133659708213, -3.434112377981056508 ) ) ;
#95304 = DIRECTION ( 'NONE',  ( 0.000000000000000000, 0.000000000000000000, 1.000000000000000000 ) ) ;
#95305 = CARTESIAN_POINT ( 'NONE',  ( 10.00000000000000178, 64.31368534415483396, 10.88017736071110342 ) ) ;
#95306 = CARTESIAN_POINT ( 'NONE',  ( 12.63842701281683034, 32.46726448433412315, 9.846743663894596210 ) ) ;
#95309 = EDGE_CURVE ( 'NONE', #80996, #42048, #31078, .T. ) ;
#95308 = CARTESIAN_POINT ( 'NONE',  ( 0.1532563361054082862, 26.21726448433411605, 2.638427012816831674 ) ) ;
#95307 = CARTESIAN_POINT ( 'NONE',  ( -4.164238869374098151, 56.59541550158063927, -3.795296366450310543 ) ) ;
#95310 = DIRECTION ( 'NONE',  ( 0.000000000000000000, 1.000000000000000000, 0.000000000000000000 ) ) ;
#95311 = AXIS2_PLACEMENT_3D ( 'NONE', #4634, #81589, #43105 ) ;
#95312 = CARTESIAN_POINT ( 'NONE',  ( 2.791683348922240793, 66.63393115100079456, 7.208316651077764092 ) ) ;
#95313 = CARTESIAN_POINT ( 'NONE',  ( -0.3689425029237881626, 7.428748834913967869, 10.36894250292379027 ) ) ;
#95314 = CARTESIAN_POINT ( 'NONE',  ( 24.16423886937410614, 29.30374883491396787, 8.672049930838204340E-16 ) ) ;
#95315 = CARTESIAN_POINT ( 'NONE',  ( 1.472469842513823179, 31.42559781766745530, 4.923371831947296329 ) ) ;
#95316 = CARTESIAN_POINT ( 'NONE',  ( 1.457314710996481688, 0.000000000000000000, 5.254907083456974881 ) ) ;
#95317 = CARTESIAN_POINT ( 'NONE',  ( 4.559911319644449179, 28.89701867748817321, 9.422509992056141925 ) ) ;
#95318 = EDGE_CURVE ( 'NONE', #57591, #9146, #2594, .T. ) ;
#95319 = CARTESIAN_POINT ( 'NONE',  ( -0.8801773607111009756, 53.06368534415484106, 1.068504757029289695E-15 ) ) ;
#95320 = CARTESIAN_POINT ( 'NONE',  ( 19.42250999205614193, 50.14701867748817676, 5.440088680355555262 ) ) ;
#95321 = VERTEX_POINT ( 'NONE', #93556 ) ;
#95322 = CARTESIAN_POINT ( 'NONE',  ( 10.00000000000000000, 42.87363466993042493, -12.81628187352647608 ) ) ;
#95323 = CARTESIAN_POINT ( 'NONE',  ( 10.00000000000000000, 46.81368534415484106, -10.88017736071110342 ) ) ;
#95324 = ORIENTED_EDGE ( 'NONE', *, *, #43284, .T. ) ;
#95325 = CARTESIAN_POINT ( 'NONE',  ( 1.379999999999981908, 20.99999999999999645, -1.249999999999987121 ) ) ;
#95326 = AXIS2_PLACEMENT_3D ( 'NONE', #18034, #41038, #47036 ) ;
#95327 = CARTESIAN_POINT ( 'NONE',  ( 7.084665262690076126, 69.10535201082151957, 10.88017736071109987 ) ) ;
#95328 = ORIENTED_EDGE ( 'NONE', *, *, #78614, .T. ) ;
#95329 = STYLED_ITEM ( 'NONE', ( #63087 ), #67519 ) ;
#95330 = CARTESIAN_POINT ( 'NONE',  ( 19.42250999205614548, 60.98035201082151247, -5.440088680355545492 ) ) ;
#95331 = CARTESIAN_POINT ( 'NONE',  ( 20.88017736071110519, 20.56368534415484106, 2.639326808657452039E-16 ) ) ;
#95332 = CARTESIAN_POINT ( 'NONE',  ( -9.000000000000001776, 80.99999999999994316, 1.249999999999987121 ) ) ;
#95333 = DIRECTION ( 'NONE',  ( 0.000000000000000000, 0.000000000000000000, 1.000000000000000000 ) ) ;
#95334 = CARTESIAN_POINT ( 'NONE',  ( 15.44008868035555793, 6.397018677488171434, -9.422509992056140149 ) ) ;
#95335 = CARTESIAN_POINT ( 'NONE',  ( 5.076628168052704559, 15.17559781766745175, -8.527530157486179263 ) ) ;
#95336 = CARTESIAN_POINT ( 'NONE',  ( 13.79529636645030344, 18.26208216824730002, 14.16423886937410614 ) ) ;
#95337 = CARTESIAN_POINT ( 'NONE',  ( 7.084665262690076126, 29.10535201082150181, 10.88017736071109987 ) ) ;
#95338 = CARTESIAN_POINT ( 'NONE',  ( 0.1532563361054083140, 61.00893115100078745, 1.131784320476157264E-15 ) ) ;
#95339 = ORIENTED_EDGE ( 'NONE', *, *, #60871, .T. ) ;
#95340 = CARTESIAN_POINT ( 'NONE',  ( 7.361572987183170547, 67.05059781766746596, 9.846743663894590881 ) ) ;
#95341 = EDGE_LOOP ( 'NONE', ( #57671, #56767, #65545, #66060 ) ) ;
#95342 = FACE_OUTER_BOUND ( 'NONE', #41142, .T. ) ;
#95343 = CARTESIAN_POINT ( 'NONE',  ( 7.084665262690076126, 49.10535201082149825, 10.88017736071109987 ) ) ;
#95344 = CARTESIAN_POINT ( 'NONE',  ( 14.92337183194729633, 57.67559781766745886, 8.527530157486181039 ) ) ;
#95345 = STYLED_ITEM ( 'NONE', ( #86218 ), #144 ) ;
#95346 = CARTESIAN_POINT ( 'NONE',  ( 16.40814093676324603, 32.45696800326375353, -11.09922568453594671 ) ) ;
#95348 = CARTESIAN_POINT ( 'NONE',  ( -14.02068044289372395, 14.63595249122790598, -5.331089937175856441 ) ) ;
#95347 = CARTESIAN_POINT ( 'NONE',  ( -0.8801773607111009756, 3.063685344154837509, 1.068504757029289695E-15 ) ) ;
#95349 = CARTESIAN_POINT ( 'NONE',  ( 15.44008868035555260, 59.73035201082151247, 9.422509992056143702 ) ) ;
#95350 = CARTESIAN_POINT ( 'NONE',  ( 6.204703633549690345, 67.84541550158060375, 14.16423886937410082 ) ) ;
#95351 = ORIENTED_EDGE ( 'NONE', *, *, #37719, .T. ) ;
#95352 = CARTESIAN_POINT ( 'NONE',  ( -2.816281873526471635, 38.91530133659708213, -3.434112377981056508 ) ) ;
#95353 = CARTESIAN_POINT ( 'NONE',  ( 20.88017736071110875, 35.77201867748816966, -2.915334737309920765 ) ) ;
#95354 = CARTESIAN_POINT ( 'NONE',  ( 0.000000000000000000, 0.5000000000000004441, 0.000000000000000000 ) ) ;
#95355 = ORIENTED_EDGE ( 'NONE', *, *, #63270, .F. ) ;
#95356 = CARTESIAN_POINT ( 'NONE',  ( 22.81628187352647785, 41.41530133659708923, 3.434112377981063169 ) ) ;
#95357 = CARTESIAN_POINT ( 'NONE',  ( 4.559911319644449179, 33.89701867748817676, 9.422509992056141925 ) ) ;
#95358 = CARTESIAN_POINT ( 'NONE',  ( 0.1532563361054082862, 51.21726448433412315, 2.638427012816831674 ) ) ;
#95359 = ORIENTED_EDGE ( 'NONE', *, *, #97466, .F. ) ;
#95360 = CARTESIAN_POINT ( 'NONE',  ( 1.472469842513823179, 56.42559781766745886, 4.923371831947296329 ) ) ;
#95362 = CARTESIAN_POINT ( 'NONE',  ( 10.00000000000000178, 52.25893115100078745, 9.846743663894594434 ) ) ;
#95361 = CARTESIAN_POINT ( 'NONE',  ( -0.4427729075171641382, 14.61885305295417048, 10.00000000000000000 ) ) ;
#95363 = CARTESIAN_POINT ( 'NONE',  ( 19.42250999205614548, 20.98035201082150891, -5.440088680355545492 ) ) ;
#95364 = SURFACE_STYLE_USAGE ( .BOTH. , #3388 ) ;
#95365 = CARTESIAN_POINT ( 'NONE',  ( 19.84674366389459621, 38.50893115100078745, 7.409399052514197653E-17 ) ) ;
#95366 = DIRECTION ( 'NONE',  ( 0.000000000000000000, 1.000000000000000000, 0.000000000000000000 ) ) ;
#95367 = CARTESIAN_POINT ( 'NONE',  ( 0.9082943533637201083, 4.650128654361622927E-16, -14.47152380945585115 ) ) ;
#95368 = EDGE_CURVE ( 'NONE', #76544, #87452, #24096, .T. ) ;
#95370 = CARTESIAN_POINT ( 'NONE',  ( 12.63842701281683922, 14.55059781766744997, -9.846743663894590881 ) ) ;
#95369 = CARTESIAN_POINT ( 'NONE',  ( 0.1532563361054100626, 30.80059781766744820, -2.638427012816831230 ) ) ;
#95371 = CARTESIAN_POINT ( 'NONE',  ( 5.076628168052704559, 0.1755978176674514724, -8.527530157486179263 ) ) ;
#95373 = ORIENTED_EDGE ( 'NONE', *, *, #22531, .F. ) ;
#95372 = CARTESIAN_POINT ( 'NONE',  ( 17.20831665107776587, 59.13393115100078745, -7.208316651077762316 ) ) ;
#95374 = CARTESIAN_POINT ( 'NONE',  ( -1.099225684535947600, 63.70696800326376774, -6.408140936763238038 ) ) ;
#95375 = CARTESIAN_POINT ( 'NONE',  ( -0.3093388210927633941, 14.49999999999999822, -14.99680997725065978 ) ) ;
#95376 = CARTESIAN_POINT ( 'NONE',  ( 3.591859063236761518, 44.95696800326376064, 11.09922568453594849 ) ) ;
#95377 = CARTESIAN_POINT ( 'NONE',  ( 17.20831665107776587, 47.88393115100078745, 7.208316651077764980 ) ) ;
#95378 = CARTESIAN_POINT ( 'NONE',  ( 0.2751277870542978565, 12.28217586085238011, -6.500000000000002665 ) ) ;
#95379 = CARTESIAN_POINT ( 'NONE',  ( 13.79529636645031943, 65.34541550158063217, -14.16423886937409904 ) ) ;
#95380 = CARTESIAN_POINT ( 'NONE',  ( 0.1532563361054100626, 20.80059781766744464, -2.638427012816831230 ) ) ;
#95381 = LINE ( 'NONE', #3411, #4111 ) ;
#95382 = CARTESIAN_POINT ( 'NONE',  ( 20.36894250292379382, 53.67874883491397497, 10.36894250292379205 ) ) ;
#95383 = CARTESIAN_POINT ( 'NONE',  ( -6.689969769699040114, 0.000000000000000000, 12.58200319823965785 ) ) ;
#95384 = CARTESIAN_POINT ( 'NONE',  ( -0.3689425029237898834, 66.17874883491396076, -10.36894250292378850 ) ) ;
#95385 = CARTESIAN_POINT ( 'NONE',  ( 20.36894250292379382, 38.67874883491396076, 10.36894250292379205 ) ) ;
#95387 = CARTESIAN_POINT ( 'NONE',  ( -43.84531931158922191, 106.6415101899049915, -4.576679558232020995 ) ) ;
#95386 = CARTESIAN_POINT ( 'NONE',  ( 22.26659068614894466, 38.88708216824731068, 7.082119434687054849 ) ) ;
#95388 = CARTESIAN_POINT ( 'NONE',  ( 12.21130863673206157, 15.00000000000000533, -8.049375889232978309 ) ) ;
#95389 = CARTESIAN_POINT ( 'NONE',  ( 1.472469842513823179, 16.42559781766745175, 4.923371831947296329 ) ) ;
#95391 = CARTESIAN_POINT ( 'NONE',  ( 2.791683348922240793, 56.63393115100078035, 7.208316651077764092 ) ) ;
#95390 = CARTESIAN_POINT ( 'NONE',  ( -13.40508947812170781, 4.272460637706398645E-16, 5.527528931046010285 ) ) ;
#95392 = VECTOR ( 'NONE', #89857, 1000.000000000000000 ) ;
#95393 = ORIENTED_EDGE ( 'NONE', *, *, #39772, .F. ) ;
#95394 = CARTESIAN_POINT ( 'NONE',  ( 19.42250999205614548, 50.98035201082151247, -5.440088680355545492 ) ) ;
#95395 = CARTESIAN_POINT ( 'NONE',  ( 11.13571380284232326, -94.04086316623734376, 3.750000000000001332 ) ) ;
#95396 = CARTESIAN_POINT ( 'NONE',  ( 10.00000000000000178, 47.25893115100078745, 9.846743663894594434 ) ) ;
#95398 = CARTESIAN_POINT ( 'NONE',  ( 19.72487221294570858, 0.000000000000000000, -6.500000000000000888 ) ) ;
#95397 = AXIS2_PLACEMENT_3D ( 'NONE', #39457, #10427, #63893 ) ;
#95399 = AXIS2_PLACEMENT_3D ( 'NONE', #12796, #43297, #56823 ) ;
#95400 = CARTESIAN_POINT ( 'NONE',  ( 1.472469842513823179, 50.59226448433411605, -4.923371831947296329 ) ) ;
#95401 = FILL_AREA_STYLE_COLOUR ( '', #75305 ) ;
#95402 = EDGE_CURVE ( 'NONE', #11994, #12652, #24674, .T. ) ;
#95403 = ORIENTED_EDGE ( 'NONE', *, *, #11493, .F. ) ;
#95404 = CARTESIAN_POINT ( 'NONE',  ( -0.3689425029237898834, 21.17874883491396432, -10.36894250292378850 ) ) ;
#95405 = CARTESIAN_POINT ( 'NONE',  ( -14.97687855664609913, 14.63595249122789177, 0.8325315005899581733 ) ) ;
#95407 = DIRECTION ( 'NONE',  ( -0.000000000000000000, -1.000000000000000000, -0.000000000000000000 ) ) ;
#95406 = CARTESIAN_POINT ( 'NONE',  ( -3.638343494402133782, -8.270261767329072811, -2.500000000000000888 ) ) ;
#95408 = CARTESIAN_POINT ( 'NONE',  ( 10.00000000000000178, 24.31368534415484106, 10.88017736071110342 ) ) ;
#95409 = CARTESIAN_POINT ( 'NONE',  ( 16.40814093676324603, 22.45696800326375353, -11.09922568453594671 ) ) ;
#95410 = EDGE_CURVE ( 'NONE', #23460, #81310, #39592, .T. ) ;
#95411 = CARTESIAN_POINT ( 'NONE',  ( -14.35840480524195861, 14.63595249122789177, -4.340070442839036424 ) ) ;
#95412 = CARTESIAN_POINT ( 'NONE',  ( 1.472469842513823179, 6.425597817667451750, 4.923371831947296329 ) ) ;
#95413 = CARTESIAN_POINT ( 'NONE',  ( 10.00000000000000178, 50.37363466993042493, 12.81628187352647608 ) ) ;
#95414 = ORIENTED_EDGE ( 'NONE', *, *, #12112, .F. ) ;
#95415 = CARTESIAN_POINT ( 'NONE',  ( 7.185087194272973932, -80.58596676771932721, -4.000000000000000000 ) ) ;
#95416 = CARTESIAN_POINT ( 'NONE',  ( -19.00000000000000000, 75.76920769491739804, 2.900000000000000355 ) ) ;
#95417 = CARTESIAN_POINT ( 'NONE',  ( 19.80448550324509682, 61.82703681773343618, 6.500000000002703615 ) ) ;
#95418 = CARTESIAN_POINT ( 'NONE',  ( 19.42250999205614548, 5.980352010821504471, -5.440088680355545492 ) ) ;
#95419 = CARTESIAN_POINT ( 'NONE',  ( 0.000000000000000000, 15.00000000000000000, 0.000000000000000000 ) ) ;
#95420 = DIRECTION ( 'NONE',  ( 0.000000000000000000, 0.000000000000000000, 1.000000000000000000 ) ) ;
#95421 = CARTESIAN_POINT ( 'NONE',  ( 12.91533473730992121, 39.52201867748817676, 10.88017736071110164 ) ) ;
#95422 = CARTESIAN_POINT ( 'NONE',  ( 12.91533473730993009, 41.60535201082149825, -10.88017736071109987 ) ) ;
#95423 = CARTESIAN_POINT ( 'NONE',  ( -1.099225684535947600, 19.54030133659708568, 6.408140936763237150 ) ) ;
#95424 = PLANE ( 'NONE',  #53762 ) ;
#95425 = CARTESIAN_POINT ( 'NONE',  ( -12.80781515976318907, -0.03417435944610275333, 6.246788841744232990 ) ) ;
#95426 = CARTESIAN_POINT ( 'NONE',  ( 0.1532563361054100626, 15.80059781766745353, -2.638427012816831230 ) ) ;
#95427 = DIRECTION ( 'NONE',  ( 0.000000000000000000, 0.000000000000000000, -1.000000000000000000 ) ) ;
#95428 = CARTESIAN_POINT ( 'NONE',  ( 12.91533473730993009, 46.60535201082150536, -10.88017736071109987 ) ) ;
#95429 = B_SPLINE_CURVE_WITH_KNOTS ( 'NONE', 3,
 ( #17793, #10288, #2810, #40787, #41776, #57244 ),
 .UNSPECIFIED., .F., .F.,
 ( 4, 2, 4 ),
 ( 0.0002800001171771102754, 0.0006862053477396429148, 0.001092410578302175500 ),
 .UNSPECIFIED. ) ;
#95430 = UNCERTAINTY_MEASURE_WITH_UNIT (LENGTH_MEASURE( 1.000000000000000082E-05 ), #37427, 'distance_accuracy_value', 'NONE');
#95431 =( BOUNDED_SURFACE ( )  B_SPLINE_SURFACE ( 1, 2, ( 
 ( #70281, #2293, #63736, #16782, #79241, #49235, #79737, #25284, #2787, #72224, #11234, #33241, #41272, #71747, #93258, #34214, #64707, #95217, #85277, #47258, #1798, #32253, #62754, #12710, #5229, #80222, #95726, #36203, #65702, #74694, #82189, #35199, #27708, #50717, #35707, #5715, #81690, #96229, #13204, #44184, #74184, #36707, #66193, #58191, #73694, #66701, #19719, #88703, #20213, #81210, #97229, #96727, #42723, #28696, #28203, #59188, #4736, #43204, #58699, #89203, #20716, #51207, #43697, #67197, #49711, #89693, #21208, #51706, #11726, #19231, #27210, #88211, #80719, #42239, #57711, #50208, #13699, #6204, #97722, #72705, #12215, #57219, #87716, #4241, #34711, #65206, #73204, #22696, #7697, #76661, #53667, #68194, #84183, #16170, #46177, #8659, #38193, #7193, #45678, #8180, #90676, #37696, #60670, #53175, #38676, #68680, #14706, #700, #76176, #69177, #75679, #83681, #98715, #61165, #15196, #23192, #208, #39172, #21708, #30166, #15692, #91168, #82688, #90178, #98212, #60179, #52681, #14205, #29670, #22202, #84662, #54152, #31153, #30658, #91673, #61643, #92164, #69661, #83182, #59684, #52193, #46654, #67700, #23689, #45180, #77150, #29186, #44686, #37212, #75181, #6693, #85647, #55644, #63615, #78642, #77636, #40149, #9153, #92644, #54639, #39671, #86144, #24169, #93136, #10149, #25168, #17657, #17166, #16665, #33121, #70162, #24663, #31646, #48127, #62136, #85157, #2176, #40644, #1187, #55133, #71142, #1679, #32132, #47647, #2670, #47139, #56141, #62631, #78142, #94122, #25648, #9652, #70653, #32634, #63132, #93634, #98548, #46, #8984, #16002, #61487, #91992, #69500, #39501, #23523, #46012, #38512, #30988, #83019, #45006, #30000, #69010, #22037, #84502, #39005, #84986, #22528, #68517, #46979, #92479, #53000, #53995, #15531, #60507, #30495, #69990, #46490, #76989, #8502, #1016, #1518, #31476, #76501, #541, #14536, #90997, #61979, #60994, #31964, #16502, #91506, #23025, #84007, #24004, #54476, #77473, #53497, #90503, #52512, #75512, #7026, #37532, #8015, #68022, #83514, #15032, #45505, #76005, #7532, #38023, #9476, #63990, #42017, #33979, #72482, #94500, #33492, #41528, #63022, #26494, #86526, #48507, #87004, #40537, #63512, #49002, #25050, #41029, #79993, #24560, #64482, #3521, #19010, #17050, #4016, #26019, #71531, #33013, #56514, #55021, #94990, #18512, #17545, #94016, #55536, #78032, #34477, #25538, #64971, #85537, #93522, #10514, #56029, #56992, #47530, #86032, #87495, #18026, #79509, #79010, #3040, #49486, #11011, #48013, #71996, #9534, #40038, #78522, #11496, #2556, #10034, #71035, #70539, #2061, #32523 ),
 ( #83320, #27969, #49987, #57487, #65469, #27479, #19980, #80494, #95996, #57972, #53307, #22831, #7336, #65969, #66464, #20484, #96496, #7829, #50477, #26988, #19492, #83815, #34973, #29811, #80981, #88478, #98848, #12481, #4507, #37837, #73965, #58461, #14845, #15341, #68328, #42984, #5494, #73465, #11992, #42493, #4992, #45317, #72978, #35473, #30302, #52813, #75814, #88977, #50972, #45824, #81465, #12970, #87981, #22339, #43463, #35966, #98353, #60804, #60320, #90811, #91304, #76311, #38325, #95497, #47276, #352, #62778, #17300, #63261, #830, #46791, #25296, #70794, #31289, #39799, #92781, #76796, #77284, #86278, #93277, #70299, #1814, #47775, #17787, #32269, #24312, #16800, #91808, #8312, #78273, #8795, #48262, #93770, #39312, #69805, #62275, #77777, #9787, #24800, #1328, #55277, #55783, #85787, #78775, #9290, #31780, #85293, #40286, #61788, #54777, #2311, #32766, #10281, #68819, #54285, #30799, #61299, #23330, #92298, #53810, #84321, #15822, #46309, #38815, #69308, #23822, #84800, #16309, #64724, #4258, #56752, #79753, #65220, #41287, #57237, #96246, #40781, #80737, #19738, #35220, #33258, #88723, #42254, #87735, #49253, #11746, #71281, #12232, #72724, #33735, #11251, #71761, #94254, #58206, #41769, #81227, #2803, #79261, #26742, #72240, #42741, #63749, #10772, #4750, #34227, #80238, #3773, #95234, #65720, #34729, #3271, #19247, #20234, #25782, #64236, #95747, #18771, #94753, #26255, #49731, #56276, #87245, #27231, #57726, #86771, #88229, #50223, #73222, #27726, #50738, #18274, #48753, #90697, #60691, #60202, #91191, #44704, #67719, #73715, #75204, #89224, #6224, #89710, #74714, #20733, #66723, #45205, #81708, #51224, #52702, #36728, #97247, #90201, #22226, #67219, #53200, #97742, #30190, #29205, #5248, #14225, #59207, #68218, #22716, #21731, #13222, #83207, #36222, #43718, #74202, #12726, #5736, #28716, #14729, #52213, #21224, #43221, #75704, #6714, #96745, #59704, #37231, #98232, #82707, #35726, #7215, #29693, #66214, #37716, #28221, #98739, #58719, #51728, #82210, #13720, #44204, #23712, #16687, #39194, #77660, #31668, #63149, #76200, #31176, #70180, #16194, #38216, #45700, #53687, #15713, #8203, #68701, #84205, #46199, #40168, #9671, #93158, #54173, #54661, #8682, #84684, #93651, #38698, #15221, #7719, #70673, #23214, #47157, #69197, #76683, #85667, #722, #91695, #24682, #62158, #46676, #1696, #2193, #55153, #61667, #92664, #92186, #233, #30681, #77174, #32152, #61189, #69682, #17187, #39692, #62654, #1213, #24192, #32655, #85177, #9174, #47667, #78161, #25185, #83704, #95116, #34608, #86164, #25668, #26624 ) ),
 .UNSPECIFIED., .F., .F., .F. ) 
 B_SPLINE_SURFACE_WITH_KNOTS ( ( 2, 2 ),
 ( 3, 2, 2, 2, 2, 2, 2, 2, 2, 2, 2, 2, 2, 2, 2, 2, 2, 2, 2, 2, 2, 2, 2, 2, 2, 2, 2, 2, 2, 2, 2, 2, 2, 2, 2, 2, 2, 2, 2, 2, 2, 2, 2, 2, 2, 2, 2, 2, 2, 2, 2, 2, 2, 2, 2, 2, 2, 2, 2, 2, 2, 2, 2, 2, 2, 2, 2, 2, 2, 2, 2, 2, 2, 2, 2, 2, 2, 2, 2, 2, 2, 2, 2, 2, 2, 2, 2, 2, 2, 2, 2, 2, 2, 2, 2, 2, 2, 2, 2, 2, 2, 2, 2, 2, 2, 2, 2, 2, 2, 2, 2, 2, 2, 2, 2, 2, 2, 2, 2, 2, 2, 2, 2, 2, 2, 2, 2, 2, 2, 2, 2, 2, 2, 2, 2, 2, 2, 2, 2, 2, 2, 2, 2, 2, 2, 2, 2, 2, 2, 2, 2, 2, 2, 2, 2, 2, 2, 2, 2, 2, 2, 2, 3 ),
 ( 0.000000000000000000, 1.000000000000000000 ),
 ( 0.000000000000000000, 0.005952380952380952051, 0.01190476190476190410, 0.01785714285714285615, 0.02380952380952380820, 0.02976190476190476025, 0.03571428571428571230, 0.04166666666666666435, 0.04761904761904761640, 0.05357142857142856845, 0.05952380952380952051, 0.06547619047619047949, 0.07142857142857142461, 0.07738095238095238360, 0.08333333333333332871, 0.08928571428571428770, 0.09523809523809523281, 0.1011904761904761918, 0.1071428571428571369, 0.1130952380952380959, 0.1190476190476190410, 0.1250000000000000000, 0.1309523809523809590, 0.1369047619047619180, 0.1428571428571428492, 0.1488095238095238082, 0.1547619047619047672, 0.1607142857142857262, 0.1666666666666666574, 0.1726190476190476164, 0.1785714285714285754, 0.1845238095238095344, 0.1904761904761904656, 0.1964285714285714246, 0.2023809523809523836, 0.2083333333333333426, 0.2142857142857142738, 0.2202380952380952328, 0.2261904761904761918, 0.2321428571428571508, 0.2380952380952380820, 0.2440476190476190410, 0.2500000000000000000, 0.2559523809523809312, 0.2619047619047619180, 0.2678571428571428492, 0.2738095238095238360, 0.2797619047619047672, 0.2857142857142856984, 0.2916666666666666852, 0.2976190476190476164, 0.3035714285714285476, 0.3095238095238095344, 0.3154761904761904656, 0.3214285714285714524, 0.3273809523809523836, 0.3333333333333333148, 0.3392857142857143016, 0.3452380952380952328, 0.3511904761904761640, 0.3571428571428571508, 0.3630952380952380820, 0.3690476190476190688, 0.3750000000000000000, 0.3809523809523809312, 0.3869047619047619180, 0.3928571428571428492, 0.3988095238095238360, 0.4047619047619047672, 0.4107142857142856984, 0.4166666666666666852, 0.4226190476190476164, 0.4285714285714285476, 0.4345238095238095344, 0.4404761904761904656, 0.4464285714285714524, 0.4523809523809523836, 0.4583333333333333148, 0.4642857142857143016, 0.4702380952380952328, 0.4761904761904761640, 0.4821428571428571508, 0.4880952380952380820, 0.4940476190476190688, 0.5000000000000000000, 0.5059523809523809312, 0.5119047619047618625, 0.5178571428571429047, 0.5238095238095238360, 0.5297619047619047672, 0.5357142857142856984, 0.5416666666666666297, 0.5476190476190476719, 0.5535714285714286031, 0.5595238095238095344, 0.5654761904761904656, 0.5714285714285713969, 0.5773809523809523281, 0.5833333333333333703, 0.5892857142857143016, 0.5952380952380952328, 0.6011904761904761640, 0.6071428571428570953, 0.6130952380952381375, 0.6190476190476190688, 0.6250000000000000000, 0.6309523809523809312, 0.6369047619047618625, 0.6428571428571429047, 0.6488095238095238360, 0.6547619047619047672, 0.6607142857142856984, 0.6666666666666666297, 0.6726190476190476719, 0.6785714285714286031, 0.6845238095238095344, 0.6904761904761904656, 0.6964285714285713969, 0.7023809523809523281, 0.7083333333333333703, 0.7142857142857143016, 0.7202380952380952328, 0.7261904761904761640, 0.7321428571428570953, 0.7380952380952381375, 0.7440476190476190688, 0.7500000000000000000, 0.7559523809523809312, 0.7619047619047618625, 0.7678571428571429047, 0.7738095238095238360, 0.7797619047619047672, 0.7857142857142856984, 0.7916666666666666297, 0.7976190476190476719, 0.8035714285714286031, 0.8095238095238095344, 0.8154761904761904656, 0.8214285714285713969, 0.8273809523809523281, 0.8333333333333333703, 0.8392857142857143016, 0.8452380952380952328, 0.8511904761904761640, 0.8571428571428570953, 0.8630952380952381375, 0.8690476190476190688, 0.8750000000000000000, 0.8809523809523809312, 0.8869047619047618625, 0.8928571428571429047, 0.8988095238095238360, 0.9047619047619047672, 0.9107142857142856984, 0.9166666666666666297, 0.9226190476190476719, 0.9285714285714286031, 0.9345238095238095344, 0.9404761904761904656, 0.9464285714285713969, 0.9523809523809523281, 0.9583333333333333703, 0.9642857142857143016 ),
 .UNSPECIFIED. ) 
 GEOMETRIC_REPRESENTATION_ITEM ( )  RATIONAL_B_SPLINE_SURFACE ( (
 ( 1.000000000000000000, 0.9659258262890683122, 1.000000000000000000, 0.9659258262890683122, 1.000000000000000000, 0.9659258262890683122, 1.000000000000000000, 0.9659258262890683122, 1.000000000000000000, 0.9659258262890683122, 1.000000000000000000, 0.9659258262890683122, 1.000000000000000000, 0.9659258262890683122, 1.000000000000000000, 0.9659258262890683122, 1.000000000000000000, 0.9659258262890683122, 1.000000000000000000, 0.9659258262890683122, 1.000000000000000000, 0.9659258262890683122, 1.000000000000000000, 0.9659258262890683122, 1.000000000000000000, 0.9659258262890683122, 1.000000000000000000, 0.9659258262890683122, 1.000000000000000000, 0.9659258262890683122, 1.000000000000000000, 0.9659258262890683122, 1.000000000000000000, 0.9659258262890683122, 1.000000000000000000, 0.9659258262890683122, 1.000000000000000000, 0.9659258262890683122, 1.000000000000000000, 0.9659258262890683122, 1.000000000000000000, 0.9659258262890683122, 1.000000000000000000, 0.9659258262890683122, 1.000000000000000000, 0.9659258262890683122, 1.000000000000000000, 0.9659258262890683122, 1.000000000000000000, 0.9659258262890683122, 1.000000000000000000, 0.9659258262890683122, 1.000000000000000000, 0.9659258262890683122, 1.000000000000000000, 0.9659258262890683122, 1.000000000000000000, 0.9659258262890683122, 1.000000000000000000, 0.9659258262890683122, 1.000000000000000000, 0.9659258262890683122, 1.000000000000000000, 0.9659258262890683122, 1.000000000000000000, 0.9659258262890683122, 1.000000000000000000, 0.9659258262890683122, 1.000000000000000000, 0.9659258262890683122, 1.000000000000000000, 0.9659258262890683122, 1.000000000000000000, 0.9659258262890683122, 1.000000000000000000, 0.9659258262890683122, 1.000000000000000000, 0.9659258262890683122, 1.000000000000000000, 0.9659258262890683122, 1.000000000000000000, 0.9659258262890683122, 1.000000000000000000, 0.9659258262890683122, 1.000000000000000000, 0.9659258262890683122, 1.000000000000000000, 0.9659258262890683122, 1.000000000000000000, 0.9659258262890683122, 1.000000000000000000, 0.9659258262890683122, 1.000000000000000000, 0.9659258262890683122, 1.000000000000000000, 0.9659258262890683122, 1.000000000000000000, 0.9659258262890683122, 1.000000000000000000, 0.9659258262890683122, 1.000000000000000000, 0.9659258262890683122, 1.000000000000000000, 0.9659258262890683122, 1.000000000000000000, 0.9659258262890683122, 1.000000000000000000, 0.9659258262890683122, 1.000000000000000000, 0.9659258262890683122, 1.000000000000000000, 0.9659258262890683122, 1.000000000000000000, 0.9659258262890683122, 1.000000000000000000, 0.9659258262890683122, 1.000000000000000000, 0.9659258262890683122, 1.000000000000000000, 0.9659258262890683122, 1.000000000000000000, 0.9659258262890683122, 1.000000000000000000, 0.9659258262890683122, 1.000000000000000000, 0.9659258262890683122, 1.000000000000000000, 0.9659258262890683122, 1.000000000000000000, 0.9659258262890683122, 1.000000000000000000, 0.9659258262890683122, 1.000000000000000000, 0.9659258262890683122, 1.000000000000000000, 0.9659258262890683122, 1.000000000000000000, 0.9659258262890683122, 1.000000000000000000, 0.9659258262890683122, 1.000000000000000000, 0.9659258262890683122, 1.000000000000000000, 0.9659258262890683122, 1.000000000000000000, 0.9659258262890683122, 1.000000000000000000, 0.9659258262890683122, 1.000000000000000000, 0.9659258262890683122, 1.000000000000000000, 0.9659258262890683122, 1.000000000000000000, 0.9659258262890683122, 1.000000000000000000, 0.9659258262890683122, 1.000000000000000000, 0.9659258262890683122, 1.000000000000000000, 0.9659258262890683122, 1.000000000000000000, 0.9659258262890683122, 1.000000000000000000, 0.9659258262890683122, 1.000000000000000000, 0.9659258262890683122, 1.000000000000000000, 0.9659258262890683122, 1.000000000000000000, 0.9659258262890683122, 1.000000000000000000, 0.9659258262890683122, 1.000000000000000000, 0.9659258262890683122, 1.000000000000000000, 0.9659258262890683122, 1.000000000000000000, 0.9659258262890683122, 1.000000000000000000, 0.9659258262890683122, 1.000000000000000000, 0.9659258262890683122, 1.000000000000000000, 0.9659258262890683122, 1.000000000000000000, 0.9659258262890683122, 1.000000000000000000, 0.9659258262890683122, 1.000000000000000000, 0.9659258262890683122, 1.000000000000000000, 0.9659258262890683122, 1.000000000000000000, 0.9659258262890683122, 1.000000000000000000, 0.9659258262890683122, 1.000000000000000000, 0.9659258262890683122, 1.000000000000000000, 0.9659258262890683122, 1.000000000000000000, 0.9659258262890683122, 1.000000000000000000, 0.9659258262890683122, 1.000000000000000000, 0.9659258262890683122, 1.000000000000000000, 0.9659258262890683122, 1.000000000000000000, 0.9659258262890683122, 1.000000000000000000, 0.9659258262890683122, 1.000000000000000000, 0.9659258262890683122, 1.000000000000000000, 0.9659258262890683122, 1.000000000000000000, 0.9659258262890683122, 1.000000000000000000, 0.9659258262890683122, 1.000000000000000000, 0.9659258262890683122, 1.000000000000000000, 0.9659258262890683122, 1.000000000000000000, 0.9659258262890683122, 1.000000000000000000, 0.9659258262890683122, 1.000000000000000000, 0.9659258262890683122, 1.000000000000000000, 0.9659258262890683122, 1.000000000000000000, 0.9659258262890683122, 1.000000000000000000, 0.9659258262890683122, 1.000000000000000000, 0.9659258262890683122, 1.000000000000000000, 0.9659258262890683122, 1.000000000000000000, 0.9659258262890683122, 1.000000000000000000, 0.9659258262890683122, 1.000000000000000000, 0.9659258262890683122, 1.000000000000000000, 0.9659258262890683122, 1.000000000000000000, 0.9659258262890683122, 1.000000000000000000, 0.9659258262890683122, 1.000000000000000000, 0.9659258262890683122, 1.000000000000000000, 0.9659258262890683122, 1.000000000000000000, 0.9659258262890683122, 1.000000000000000000, 0.9659258262890683122, 1.000000000000000000, 0.9659258262890683122, 1.000000000000000000, 0.9659258262890683122, 1.000000000000000000, 0.9659258262890683122, 1.000000000000000000, 0.9659258262890683122, 1.000000000000000000, 0.9659258262890683122, 1.000000000000000000, 0.9659258262890683122, 1.000000000000000000, 0.9659258262890683122, 1.000000000000000000, 0.9659258262890683122, 1.000000000000000000, 0.9659258262890683122, 1.000000000000000000, 0.9659258262890683122, 1.000000000000000000, 0.9659258262890683122, 1.000000000000000000, 0.9659258262890683122, 1.000000000000000000, 0.9659258262890683122, 1.000000000000000000, 0.9659258262890683122, 1.000000000000000000, 0.9659258262890683122, 1.000000000000000000, 0.9659258262890683122, 1.000000000000000000, 0.9659258262890683122, 1.000000000000000000, 0.9659258262890683122, 1.000000000000000000, 0.9659258262890683122, 1.000000000000000000, 0.9659258262890683122, 1.000000000000000000, 0.9659258262890683122, 1.000000000000000000, 0.9659258262890683122, 1.000000000000000000, 0.9659258262890683122, 1.000000000000000000, 0.9659258262890683122, 1.000000000000000000, 0.9659258262890683122, 1.000000000000000000, 0.9659258262890683122, 1.000000000000000000, 0.9659258262890683122, 1.000000000000000000, 0.9659258262890683122, 1.000000000000000000, 0.9659258262890683122, 1.000000000000000000, 0.9659258262890683122, 1.000000000000000000, 0.9659258262890683122, 1.000000000000000000, 0.9659258262890683122, 1.000000000000000000),
 ( 1.000000000000000000, 0.9659258262890683122, 1.000000000000000000, 0.9659258262890683122, 1.000000000000000000, 0.9659258262890683122, 1.000000000000000000, 0.9659258262890683122, 1.000000000000000000, 0.9659258262890683122, 1.000000000000000000, 0.9659258262890683122, 1.000000000000000000, 0.9659258262890683122, 1.000000000000000000, 0.9659258262890683122, 1.000000000000000000, 0.9659258262890683122, 1.000000000000000000, 0.9659258262890683122, 1.000000000000000000, 0.9659258262890683122, 1.000000000000000000, 0.9659258262890683122, 1.000000000000000000, 0.9659258262890683122, 1.000000000000000000, 0.9659258262890683122, 1.000000000000000000, 0.9659258262890683122, 1.000000000000000000, 0.9659258262890683122, 1.000000000000000000, 0.9659258262890683122, 1.000000000000000000, 0.9659258262890683122, 1.000000000000000000, 0.9659258262890683122, 1.000000000000000000, 0.9659258262890683122, 1.000000000000000000, 0.9659258262890683122, 1.000000000000000000, 0.9659258262890683122, 1.000000000000000000, 0.9659258262890683122, 1.000000000000000000, 0.9659258262890683122, 1.000000000000000000, 0.9659258262890683122, 1.000000000000000000, 0.9659258262890683122, 1.000000000000000000, 0.9659258262890683122, 1.000000000000000000, 0.9659258262890683122, 1.000000000000000000, 0.9659258262890683122, 1.000000000000000000, 0.9659258262890683122, 1.000000000000000000, 0.9659258262890683122, 1.000000000000000000, 0.9659258262890683122, 1.000000000000000000, 0.9659258262890683122, 1.000000000000000000, 0.9659258262890683122, 1.000000000000000000, 0.9659258262890683122, 1.000000000000000000, 0.9659258262890683122, 1.000000000000000000, 0.9659258262890683122, 1.000000000000000000, 0.9659258262890683122, 1.000000000000000000, 0.9659258262890683122, 1.000000000000000000, 0.9659258262890683122, 1.000000000000000000, 0.9659258262890683122, 1.000000000000000000, 0.9659258262890683122, 1.000000000000000000, 0.9659258262890683122, 1.000000000000000000, 0.9659258262890683122, 1.000000000000000000, 0.9659258262890683122, 1.000000000000000000, 0.9659258262890683122, 1.000000000000000000, 0.9659258262890683122, 1.000000000000000000, 0.9659258262890683122, 1.000000000000000000, 0.9659258262890683122, 1.000000000000000000, 0.9659258262890683122, 1.000000000000000000, 0.9659258262890683122, 1.000000000000000000, 0.9659258262890683122, 1.000000000000000000, 0.9659258262890683122, 1.000000000000000000, 0.9659258262890683122, 1.000000000000000000, 0.9659258262890683122, 1.000000000000000000, 0.9659258262890683122, 1.000000000000000000, 0.9659258262890683122, 1.000000000000000000, 0.9659258262890683122, 1.000000000000000000, 0.9659258262890683122, 1.000000000000000000, 0.9659258262890683122, 1.000000000000000000, 0.9659258262890683122, 1.000000000000000000, 0.9659258262890683122, 1.000000000000000000, 0.9659258262890683122, 1.000000000000000000, 0.9659258262890683122, 1.000000000000000000, 0.9659258262890683122, 1.000000000000000000, 0.9659258262890683122, 1.000000000000000000, 0.9659258262890683122, 1.000000000000000000, 0.9659258262890683122, 1.000000000000000000, 0.9659258262890683122, 1.000000000000000000, 0.9659258262890683122, 1.000000000000000000, 0.9659258262890683122, 1.000000000000000000, 0.9659258262890683122, 1.000000000000000000, 0.9659258262890683122, 1.000000000000000000, 0.9659258262890683122, 1.000000000000000000, 0.9659258262890683122, 1.000000000000000000, 0.9659258262890683122, 1.000000000000000000, 0.9659258262890683122, 1.000000000000000000, 0.9659258262890683122, 1.000000000000000000, 0.9659258262890683122, 1.000000000000000000, 0.9659258262890683122, 1.000000000000000000, 0.9659258262890683122, 1.000000000000000000, 0.9659258262890683122, 1.000000000000000000, 0.9659258262890683122, 1.000000000000000000, 0.9659258262890683122, 1.000000000000000000, 0.9659258262890683122, 1.000000000000000000, 0.9659258262890683122, 1.000000000000000000, 0.9659258262890683122, 1.000000000000000000, 0.9659258262890683122, 1.000000000000000000, 0.9659258262890683122, 1.000000000000000000, 0.9659258262890683122, 1.000000000000000000, 0.9659258262890683122, 1.000000000000000000, 0.9659258262890683122, 1.000000000000000000, 0.9659258262890683122, 1.000000000000000000, 0.9659258262890683122, 1.000000000000000000, 0.9659258262890683122, 1.000000000000000000, 0.9659258262890683122, 1.000000000000000000, 0.9659258262890683122, 1.000000000000000000, 0.9659258262890683122, 1.000000000000000000, 0.9659258262890683122, 1.000000000000000000, 0.9659258262890683122, 1.000000000000000000, 0.9659258262890683122, 1.000000000000000000, 0.9659258262890683122, 1.000000000000000000, 0.9659258262890683122, 1.000000000000000000, 0.9659258262890683122, 1.000000000000000000, 0.9659258262890683122, 1.000000000000000000, 0.9659258262890683122, 1.000000000000000000, 0.9659258262890683122, 1.000000000000000000, 0.9659258262890683122, 1.000000000000000000, 0.9659258262890683122, 1.000000000000000000, 0.9659258262890683122, 1.000000000000000000, 0.9659258262890683122, 1.000000000000000000, 0.9659258262890683122, 1.000000000000000000, 0.9659258262890683122, 1.000000000000000000, 0.9659258262890683122, 1.000000000000000000, 0.9659258262890683122, 1.000000000000000000, 0.9659258262890683122, 1.000000000000000000, 0.9659258262890683122, 1.000000000000000000, 0.9659258262890683122, 1.000000000000000000, 0.9659258262890683122, 1.000000000000000000, 0.9659258262890683122, 1.000000000000000000, 0.9659258262890683122, 1.000000000000000000, 0.9659258262890683122, 1.000000000000000000, 0.9659258262890683122, 1.000000000000000000, 0.9659258262890683122, 1.000000000000000000, 0.9659258262890683122, 1.000000000000000000, 0.9659258262890683122, 1.000000000000000000, 0.9659258262890683122, 1.000000000000000000, 0.9659258262890683122, 1.000000000000000000, 0.9659258262890683122, 1.000000000000000000, 0.9659258262890683122, 1.000000000000000000, 0.9659258262890683122, 1.000000000000000000, 0.9659258262890683122, 1.000000000000000000, 0.9659258262890683122, 1.000000000000000000, 0.9659258262890683122, 1.000000000000000000, 0.9659258262890683122, 1.000000000000000000, 0.9659258262890683122, 1.000000000000000000, 0.9659258262890683122, 1.000000000000000000, 0.9659258262890683122, 1.000000000000000000, 0.9659258262890683122, 1.000000000000000000, 0.9659258262890683122, 1.000000000000000000, 0.9659258262890683122, 1.000000000000000000, 0.9659258262890683122, 1.000000000000000000, 0.9659258262890683122, 1.000000000000000000, 0.9659258262890683122, 1.000000000000000000, 0.9659258262890683122, 1.000000000000000000, 0.9659258262890683122, 1.000000000000000000, 0.9659258262890683122, 1.000000000000000000, 0.9659258262890683122, 1.000000000000000000, 0.9659258262890683122, 1.000000000000000000, 0.9659258262890683122, 1.000000000000000000, 0.9659258262890683122, 1.000000000000000000, 0.9659258262890683122, 1.000000000000000000, 0.9659258262890683122, 1.000000000000000000, 0.9659258262890683122, 1.000000000000000000, 0.9659258262890683122, 1.000000000000000000, 0.9659258262890683122, 1.000000000000000000, 0.9659258262890683122, 1.000000000000000000, 0.9659258262890683122, 1.000000000000000000, 0.9659258262890683122, 1.000000000000000000, 0.9659258262890683122, 1.000000000000000000, 0.9659258262890683122, 1.000000000000000000, 0.9659258262890683122, 1.000000000000000000) ) ) 
 REPRESENTATION_ITEM ( '' )  SURFACE ( )  );
#95432 = CARTESIAN_POINT ( 'NONE',  ( 21.09922568453594849, 1.206968003263753531, 6.408140936763242479 ) ) ;
#95433 = CARTESIAN_POINT ( 'NONE',  ( 15.44008868035555260, 64.73035201082151957, 9.422509992056143702 ) ) ;
#95434 = CARTESIAN_POINT ( 'NONE',  ( 19.84674366389459266, 28.71726448433411960, -2.638427012816827677 ) ) ;
#95435 = CARTESIAN_POINT ( 'NONE',  ( 22.81628187352647785, 46.41530133659708213, 3.434112377981063169 ) ) ;
#95437 = DIRECTION ( 'NONE',  ( -1.000000000000000000, -0.000000000000000000, -0.000000000000000000 ) ) ;
#95436 = CARTESIAN_POINT ( 'NONE',  ( 10.00000000000000178, 2.258931151000784787, 9.846743663894594434 ) ) ;
#95438 = ORIENTED_EDGE ( 'NONE', *, *, #84161, .F. ) ;
#95439 = B_SPLINE_CURVE_WITH_KNOTS ( 'NONE', 3,
 ( #45761, #98794, #76255, #97297 ),
 .UNSPECIFIED., .F., .F.,
 ( 4, 4 ),
 ( 7.269816092100958512E-18, 0.002562518741975552787 ),
 .UNSPECIFIED. ) ;
#95440 = LINE ( 'NONE', #95940, #53287 ) ;
#95441 = CARTESIAN_POINT ( 'NONE',  ( 0.2751277870542980231, 9.366073187301308778, -6.500000000000002665 ) ) ;
#95442 = CARTESIAN_POINT ( 'NONE',  ( 10.00000000000000178, 19.31368534415484106, 10.88017736071110342 ) ) ;
#95444 = CARTESIAN_POINT ( 'NONE',  ( 20.36894250292379382, 23.67874883491397142, 10.36894250292379205 ) ) ;
#95443 = CARTESIAN_POINT ( 'NONE',  ( 6.565887622018943937, 58.08196800326376064, -12.81628187352647608 ) ) ;
#95445 = CARTESIAN_POINT ( 'NONE',  ( 10.00000000000000000, 29.75893115100078745, -9.846743663894594434 ) ) ;
#95446 = CARTESIAN_POINT ( 'NONE',  ( -0.8801773607110991993, 22.85535201082150181, -2.915334737309923874 ) ) ;
#95447 = AXIS2_PLACEMENT_3D ( 'NONE', #12735, #43232, #74214 ) ;
#95448 = CARTESIAN_POINT ( 'NONE',  ( 6.204703633549690345, 65.76208216824731778, -14.16423886937410259 ) ) ;
#95449 = VERTEX_POINT ( 'NONE', #39096 ) ;
#95450 = CARTESIAN_POINT ( 'NONE',  ( 4.559911319644449179, 8.897018677488171434, 9.422509992056141925 ) ) ;
#95451 = ADVANCED_FACE ( 'NONE', ( #85080 ), #69588, .F. ) ;
#95452 = CARTESIAN_POINT ( 'NONE',  ( 10.00000000000000000, 21.81368534415484106, -10.88017736071110342 ) ) ;
#95454 = CARTESIAN_POINT ( 'NONE',  ( 2.035157376598824452, 23.68868534415484461, 7.964842623401179544 ) ) ;
#95453 = CARTESIAN_POINT ( 'NONE',  ( 6.091055032734395525, 3.591419696358233438E-16, -13.29802223412757911 ) ) ;
#95455 = VERTEX_POINT ( 'NONE', #62558 ) ;
#95456 = CARTESIAN_POINT ( 'NONE',  ( 20.32896413005680003, 26.77164270246084499, 5.963430220938287007 ) ) ;
#95457 = CARTESIAN_POINT ( 'NONE',  ( -0.8801773607110991993, 17.85535201082150536, -2.915334737309923874 ) ) ;
#95458 = CARTESIAN_POINT ( 'NONE',  ( 0.1532563361054082862, 56.21726448433411605, 2.638427012816831674 ) ) ;
#95459 = CARTESIAN_POINT ( 'NONE',  ( -8.564643372776718167, 14.49999999999999112, 12.31449893000741369 ) ) ;
#95460 = SURFACE_STYLE_FILL_AREA ( #13428 ) ;
#95461 = CARTESIAN_POINT ( 'NONE',  ( -20.19000000000000838, 92.00000000000000000, 9.500000000000000000 ) ) ;
#95462 = CARTESIAN_POINT ( 'NONE',  ( 17.08211943468705840, 35.13708216824730357, -12.26659068614894466 ) ) ;
#95463 = CARTESIAN_POINT ( 'NONE',  ( 4.559911319644449179, 42.23035201082151247, -9.422509992056141925 ) ) ;
#95464 = CARTESIAN_POINT ( 'NONE',  ( 15.44008868035555260, 19.73035201082150536, 9.422509992056143702 ) ) ;
#95465 = CARTESIAN_POINT ( 'NONE',  ( 19.84674366389459266, 63.71726448433412315, -2.638427012816827677 ) ) ;
#95466 = CARTESIAN_POINT ( 'NONE',  ( 18.95785429995053306, 32.24216108172007011, 6.499999999999848121 ) ) ;
#95467 = CARTESIAN_POINT ( 'NONE',  ( 19.84674366389459621, 53.50893115100078745, 7.409399052514197653E-17 ) ) ;
#95468 = LINE ( 'NONE', #57944, #15990 ) ;
#95469 = CARTESIAN_POINT ( 'NONE',  ( 5.076628168052704559, 10.17559781766745175, -8.527530157486179263 ) ) ;
#95470 = CARTESIAN_POINT ( 'NONE',  ( 3.469446951953614189E-15, -34.62636533006957507, 12.81628187352647608 ) ) ;
#95471 = ADVANCED_BREP_SHAPE_REPRESENTATION ( '', ( #9364, #74641, #40953, #27931 ), #34259 ) ;
#95472 = CARTESIAN_POINT ( 'NONE',  ( 7.084665262690076126, 14.10535201082150358, 10.88017736071109987 ) ) ;
#95473 = CARTESIAN_POINT ( 'NONE',  ( 1.472469842513823179, 10.59226448433411782, -4.923371831947296329 ) ) ;
#95475 = CARTESIAN_POINT ( 'NONE',  ( 0.1532563361054100626, 65.80059781766745175, -2.638427012816831230 ) ) ;
#95474 = AXIS2_PLACEMENT_3D ( 'NONE', #31808, #29841, #37374 ) ;
#95476 = CARTESIAN_POINT ( 'NONE',  ( 17.96484262340118221, 64.93868534415483396, 7.964842623401181321 ) ) ;
#95478 = CARTESIAN_POINT ( 'NONE',  ( 21.09922568453594849, 51.20696800326375353, 6.408140936763242479 ) ) ;
#95477 = CARTESIAN_POINT ( 'NONE',  ( 0.5774900079438607392, 23.48035201082150536, 5.440088680355550821 ) ) ;
#95479 = CARTESIAN_POINT ( 'NONE',  ( 17.08211943468705840, 30.13708216824730357, -12.26659068614894466 ) ) ;
#95480 = CARTESIAN_POINT ( 'NONE',  ( 0.000000000000000000, 14.49999999999999822, 0.000000000000000000 ) ) ;
#95481 = CIRCLE ( 'NONE', #26806, 1.000000000000000000 ) ;
#95482 = CARTESIAN_POINT ( 'NONE',  ( -1.099225684535947600, 58.70696800326375353, -6.408140936763238038 ) ) ;
#95483 = ORIENTED_EDGE ( 'NONE', *, *, #37611, .F. ) ;
#95484 = CARTESIAN_POINT ( 'NONE',  ( 6.565887622018943937, 0.1653013365970866511, 12.81628187352647430 ) ) ;
#95485 = LINE ( 'NONE', #95984, #50528 ) ;
#95486 = CARTESIAN_POINT ( 'NONE',  ( 7.084665262690076126, 37.02201867748817676, -10.88017736071110164 ) ) ;
#95487 = CARTESIAN_POINT ( 'NONE',  ( 0.1532563361054082862, 61.21726448433412315, 2.638427012816831674 ) ) ;
#95488 = VERTEX_POINT ( 'NONE', #55572 ) ;
#95489 = CARTESIAN_POINT ( 'NONE',  ( 14.92337183194729988, 9.342264484334119601, -8.527530157486177487 ) ) ;
#95490 = CARTESIAN_POINT ( 'NONE',  ( 0.1532563361054082862, 11.21726448433411605, 2.638427012816831674 ) ) ;
#95491 = CARTESIAN_POINT ( 'NONE',  ( 2.791683348922240793, 21.63393115100078745, 7.208316651077764092 ) ) ;
#95492 = CARTESIAN_POINT ( 'NONE',  ( 5.076628168052703671, 6.842264484334118713, 8.527530157486179263 ) ) ;
#95493 = CARTESIAN_POINT ( 'NONE',  ( 19.84674366389459266, 3.300597817667451750, 2.638427012816836559 ) ) ;
#95494 = EDGE_CURVE ( 'NONE', #20560, #91650, #47006, .T. ) ;
#95496 = DIRECTION ( 'NONE',  ( 0.000000000000000000, 1.000000000000000000, 0.000000000000000000 ) ) ;
#95495 = CARTESIAN_POINT ( 'NONE',  ( 12.91533473730993009, 51.60535201082149825, -10.88017736071109987 ) ) ;
#95497 = CARTESIAN_POINT ( 'NONE',  ( 17.20831665107776587, 12.88393115100078390, 7.208316651077764980 ) ) ;
#95499 = ORIENTED_EDGE ( 'NONE', *, *, #54687, .T. ) ;
#95498 = CARTESIAN_POINT ( 'NONE',  ( 1.472469842513823179, 15.59226448433411960, -4.923371831947296329 ) ) ;
#95500 = CARTESIAN_POINT ( 'NONE',  ( -8.722765153436430552, 1.609362599783170644E-16, 11.74102699209679912 ) ) ;
#95501 = CARTESIAN_POINT ( 'NONE',  ( 1.472469842513823179, 55.59226448433412315, -4.923371831947296329 ) ) ;
#95502 = VERTEX_POINT ( 'NONE', #10557 ) ;
#95503 = CARTESIAN_POINT ( 'NONE',  ( 0.2751277870542967463, 70.00000000000000000, -6.500000000000000888 ) ) ;
#95504 = CARTESIAN_POINT ( 'NONE',  ( 10.00000000000000000, 15.55374883491396787, -14.16423886937410082 ) ) ;
#95505 = UNCERTAINTY_MEASURE_WITH_UNIT (LENGTH_MEASURE( 1.000000000000000082E-05 ), #47072, 'distance_accuracy_value', 'NONE');
#95506 = FACE_OUTER_BOUND ( 'NONE', #49343, .T. ) ;
#95507 = CARTESIAN_POINT ( 'NONE',  ( 22.26659068614895176, 14.72041550158063572, -7.082119434687042414 ) ) ;
#95508 = CARTESIAN_POINT ( 'NONE',  ( 20.36894250292379738, 34.92874883491396076, -10.36894250292379027 ) ) ;
#95509 = CARTESIAN_POINT ( 'NONE',  ( 13.79529636645030344, 3.262082168247301350, 14.16423886937410614 ) ) ;
#95510 = CARTESIAN_POINT ( 'NONE',  ( 20.88017736071110875, 40.77201867748818387, -2.915334737309920765 ) ) ;
#95511 = CARTESIAN_POINT ( 'NONE',  ( 14.71525861348287734, 15.00000000000000000, 2.908807992686682109 ) ) ;
#95512 = VERTEX_POINT ( 'NONE', #41068 ) ;
#95513 = CARTESIAN_POINT ( 'NONE',  ( 2.791683348922240793, 16.63393115100078745, 7.208316651077764092 ) ) ;
#95515 = CARTESIAN_POINT ( 'NONE',  ( 5.076628168052704559, 15.17559781766745175, -8.527530157486179263 ) ) ;
#95514 = CARTESIAN_POINT ( 'NONE',  ( 10.00000000000000000, 56.81368534415484106, -10.88017736071110342 ) ) ;
#95516 = CARTESIAN_POINT ( 'NONE',  ( 10.00000000000000000, 16.81368534415483751, -10.88017736071110342 ) ) ;
#95517 = CARTESIAN_POINT ( 'NONE',  ( 19.38216949554541202, 50.99863466993042493, 9.382169495545424454 ) ) ;
#95518 = CARTESIAN_POINT ( 'NONE',  ( 14.92337183194729988, 49.34226448433411605, -8.527530157486177487 ) ) ;
#95519 = CARTESIAN_POINT ( 'NONE',  ( 12.00809552683959502, 0.3640475087720981828, -8.989195838243551506 ) ) ;
#95520 = CARTESIAN_POINT ( 'NONE',  ( 0.6178305044545838731, 24.74863466993042493, 9.382169495545420901 ) ) ;
#95521 = CARTESIAN_POINT ( 'NONE',  ( 7.082119434687047743, -29.86291783175269643, -12.26659068614894821 ) ) ;
#95522 = AXIS2_PLACEMENT_3D ( 'NONE', #72942, #94954, #49451 ) ;
#95523 = CARTESIAN_POINT ( 'NONE',  ( 0.1532563361054083140, 46.00893115100079456, 1.131784320476157264E-15 ) ) ;
#95524 = CARTESIAN_POINT ( 'NONE',  ( 22.26659068614894466, 18.88708216824730002, 7.082119434687054849 ) ) ;
#95525 = EDGE_CURVE ( 'NONE', #97969, #51220, #62992, .T. ) ;
#95526 = VERTEX_POINT ( 'NONE', #20021 ) ;
#95527 = ORIENTED_EDGE ( 'NONE', *, *, #14935, .T. ) ;
#95528 =( NAMED_UNIT ( * ) PLANE_ANGLE_UNIT ( ) SI_UNIT ( $, .RADIAN. ) );
#95529 = CARTESIAN_POINT ( 'NONE',  ( 17.96484262340118221, 51.18868534415483396, -7.964842623401177768 ) ) ;
#95530 = CARTESIAN_POINT ( 'NONE',  ( 10.00000000000000000, 56.81368534415484106, -10.88017736071110342 ) ) ;
#95531 = CARTESIAN_POINT ( 'NONE',  ( 22.26659068614895176, 39.72041550158063217, -7.082119434687042414 ) ) ;
#95532 = CARTESIAN_POINT ( 'NONE',  ( 1.472469842513823179, 60.59226448433412315, -4.923371831947296329 ) ) ;
#95533 = CARTESIAN_POINT ( 'NONE',  ( 18.52753015748618282, 8.925597817667451750, -4.923371831947291888 ) ) ;
#95534 = CYLINDRICAL_SURFACE ( 'NONE', #73583, 0.5000000000000004441 ) ;
#95535 = CARTESIAN_POINT ( 'NONE',  ( 19.42250999205614193, 45.14701867748817676, 5.440088680355555262 ) ) ;
#95536 = EDGE_CURVE ( 'NONE', #14505, #28596, #21826, .T. ) ;
#95537 = CARTESIAN_POINT ( 'NONE',  ( -6.787878914541004782, -86.25326249609902618, -2.499999999999999556 ) ) ;
#95538 = CARTESIAN_POINT ( 'NONE',  ( 14.92337183194729988, 49.34226448433411605, -8.527530157486177487 ) ) ;
#95539 = CARTESIAN_POINT ( 'NONE',  ( 2.915334737309928315, 9.522018677488167882, 10.88017736071109987 ) ) ;
#95540 = CARTESIAN_POINT ( 'NONE',  ( -0.8801773607110991993, 2.855352010821504471, -2.915334737309923874 ) ) ;
#95541 = CARTESIAN_POINT ( 'NONE',  ( -11.75249112336545387, 0.04962895880866165232, -8.918310463590589876 ) ) ;
#95542 = CIRCLE ( 'NONE', #18891, 2.899999999999999023 ) ;
#95543 = CARTESIAN_POINT ( 'NONE',  ( 4.559911319644449179, 2.230352010821504471, -9.422509992056141925 ) ) ;
#95544 = DIRECTION ( 'NONE',  ( -0.000000000000000000, 1.000000000000000000, -0.000000000000000000 ) ) ;
#95545 = AXIS2_PLACEMENT_3D ( 'NONE', #88066, #34561, #86610 ) ;
#95546 = CARTESIAN_POINT ( 'NONE',  ( -0.8801773607111008646, 63.27201867748817676, 2.915334737309923430 ) ) ;
#95547 = CARTESIAN_POINT ( 'NONE',  ( 5.076628168052703671, 1.842264484334118047, 8.527530157486179263 ) ) ;
#95548 = CARTESIAN_POINT ( 'NONE',  ( 18.00000000000000000, 78.80384757729335377, -3.750000000000000444 ) ) ;
#95549 = CARTESIAN_POINT ( 'NONE',  ( 19.84674366389459266, 33.71726448433410894, -2.638427012816827677 ) ) ;
#95550 = CARTESIAN_POINT ( 'NONE',  ( 19.42250999205614193, 25.14701867748817321, 5.440088680355555262 ) ) ;
#95551 = CARTESIAN_POINT ( 'NONE',  ( 19.84674366389459266, 63.71726448433412315, -2.638427012816827677 ) ) ;
#95553 = CARTESIAN_POINT ( 'NONE',  ( -6.607077646681807082, -50.94230861868440741, -3.750000000000000444 ) ) ;
#95552 = CARTESIAN_POINT ( 'NONE',  ( -0.8801773607111008646, 38.27201867748816255, 2.915334737309923430 ) ) ;
#95554 = CARTESIAN_POINT ( 'NONE',  ( -1.099225684535947600, 44.54030133659708923, 6.408140936763237150 ) ) ;
#95555 = ORIENTED_EDGE ( 'NONE', *, *, #18082, .T. ) ;
#95556 = CARTESIAN_POINT ( 'NONE',  ( 17.96484262340118221, 56.18868534415484817, -7.964842623401177768 ) ) ;
#95558 = CARTESIAN_POINT ( 'NONE',  ( 18.52753015748618282, 18.92559781766745175, -4.923371831947291888 ) ) ;
#95557 = CARTESIAN_POINT ( 'NONE',  ( 21.09922568453594849, 16.20696800326375353, 6.408140936763242479 ) ) ;
#95559 = CARTESIAN_POINT ( 'NONE',  ( 17.20831665107776587, 2.883931151000785231, 7.208316651077764980 ) ) ;
#95560 = CARTESIAN_POINT ( 'NONE',  ( 15.44008868035555793, 31.39701867748817676, -9.422509992056140149 ) ) ;
#95561 = CARTESIAN_POINT ( 'NONE',  ( 17.08211943468705130, 63.47041550158063927, 12.26659068614894998 ) ) ;
#95562 = CARTESIAN_POINT ( 'NONE',  ( 0.1532563361054082862, 51.21726448433412315, 2.638427012816831674 ) ) ;
#95563 = CARTESIAN_POINT ( 'NONE',  ( 18.52753015748618282, 8.925597817667451750, -4.923371831947291888 ) ) ;
#95564 = CARTESIAN_POINT ( 'NONE',  ( 2.035157376598824452, 63.68868534415484106, 7.964842623401179544 ) ) ;
#95565 = CARTESIAN_POINT ( 'NONE',  ( -3.927832320392339316, 15.00000000000000000, 13.69797916712101404 ) ) ;
#95566 = CARTESIAN_POINT ( 'NONE',  ( -0.3689425029237881626, 32.42874883491395366, 10.36894250292379027 ) ) ;
#95567 = B_SPLINE_CURVE_WITH_KNOTS ( 'NONE', 3,
 ( #74079, #13095, #51097, #59083, #80617, #44076 ),
 .UNSPECIFIED., .F., .F.,
 ( 4, 2, 4 ),
 ( 3.409110551377157120E-05, 0.0004400426677356206748, 0.0008459942299574697106 ),
 .UNSPECIFIED. ) ;
#95568 = EDGE_CURVE ( 'NONE', #44437, #90212, #57575, .T. ) ;
#95569 = DIRECTION ( 'NONE',  ( -1.000000000000000000, 0.000000000000000000, 0.000000000000000000 ) ) ;
#95570 = DIRECTION ( 'NONE',  ( 0.9848077530122084644, 0.1736481776669281663, 0.000000000000000000 ) ) ;
#95571 = ORIENTED_EDGE ( 'NONE', *, *, #47534, .T. ) ;
#95572 = ORIENTED_EDGE ( 'NONE', *, *, #68637, .T. ) ;
#95573 = CARTESIAN_POINT ( 'NONE',  ( -0.3689425029237898834, 51.17874883491397497, -10.36894250292378850 ) ) ;
#95574 = CARTESIAN_POINT ( 'NONE',  ( 2.917880565312948704, 52.63708216824730357, 12.26659068614894643 ) ) ;
#95575 = CARTESIAN_POINT ( 'NONE',  ( 7.361572987183170547, 12.05059781766744997, 9.846743663894590881 ) ) ;
#95576 = CARTESIAN_POINT ( 'NONE',  ( 3.591859063236763294, 18.29030133659708568, -11.09922568453595026 ) ) ;
#95577 = DIRECTION ( 'NONE',  ( -1.000000000000000000, 0.000000000000000000, 0.000000000000000000 ) ) ;
#95578 = CARTESIAN_POINT ( 'NONE',  ( -3.897244926436313150, 4.087811286569849197E-16, 13.96644127841328142 ) ) ;
#95580 = CARTESIAN_POINT ( 'NONE',  ( -2.816281873526471635, 43.91530133659708923, -3.434112377981056508 ) ) ;
#95579 = DIRECTION ( 'NONE',  ( 4.683753385137374737E-14, -1.000000000000000000, 0.000000000000000000 ) ) ;
#95581 = CARTESIAN_POINT ( 'NONE',  ( 24.16423886937409904, 49.09541550158063217, 3.795296366450317205 ) ) ;
#95582 = B_SPLINE_CURVE_WITH_KNOTS ( 'NONE', 3,
 ( #3800, #18301, #9819, #33283, #95268, #9317 ),
 .UNSPECIFIED., .F., .F.,
 ( 4, 2, 4 ),
 ( 3.409110551494648044E-05, 0.0004400426677367923179, 0.0008459942299586381553 ),
 .UNSPECIFIED. ) ;
#95583 = CARTESIAN_POINT ( 'NONE',  ( -4.862001128006231632, 15.00000000000000000, -13.66056166603291189 ) ) ;
#95584 = CARTESIAN_POINT ( 'NONE',  ( 7.361572987183170547, 12.05059781766744997, 9.846743663894590881 ) ) ;
#95585 = CARTESIAN_POINT ( 'NONE',  ( -2.638427012816824124, 2.050597817667449974, 9.846743663894596210 ) ) ;
#95586 = ORIENTED_EDGE ( 'NONE', *, *, #34725, .F. ) ;
#95587 = DIRECTION ( 'NONE',  ( -0.000000000000000000, 1.000000000000000000, 0.000000000000000000 ) ) ;
#95588 = CARTESIAN_POINT ( 'NONE',  ( 2.791683348922240793, 21.63393115100078745, 7.208316651077764092 ) ) ;
#95589 = ORIENTED_EDGE ( 'NONE', *, *, #47875, .F. ) ;
#95590 = CARTESIAN_POINT ( 'NONE',  ( -19.19000000000001194, 93.50000000000000000, 9.500000000000000000 ) ) ;
#95591 = EDGE_LOOP ( 'NONE', ( #805, #83293 ) ) ;
#95593 = CARTESIAN_POINT ( 'NONE',  ( 12.91533473730993009, 31.60535201082150891, -10.88017736071109987 ) ) ;
#95592 = CARTESIAN_POINT ( 'NONE',  ( 20.88017736071110164, 20.35535201082150891, 2.915334737309930979 ) ) ;
#95595 = CARTESIAN_POINT ( 'NONE',  ( 22.81628187352647785, 1.623634669930420271, 6.195893100308588602E-16 ) ) ;
#95594 = CARTESIAN_POINT ( 'NONE',  ( 14.92337183194729988, 49.34226448433411605, -8.527530157486177487 ) ) ;
#95596 = SURFACE_STYLE_USAGE ( .BOTH. , #88078 ) ;
#95597 = CARTESIAN_POINT ( 'NONE',  ( 16.40814093676324603, 22.45696800326375353, -11.09922568453594671 ) ) ;
#95598 = ORIENTED_EDGE ( 'NONE', *, *, #71722, .T. ) ;
#95599 = CARTESIAN_POINT ( 'NONE',  ( 14.92337183194729988, 29.34226448433411960, -8.527530157486177487 ) ) ;
#95600 = CARTESIAN_POINT ( 'NONE',  ( 6.204703633549690345, 55.76208216824730357, -14.16423886937410259 ) ) ;
#95601 = CARTESIAN_POINT ( 'NONE',  ( 15.44008868035555260, 9.730352010821505360, 9.422509992056143702 ) ) ;
#95602 = ORIENTED_EDGE ( 'NONE', *, *, #45830, .F. ) ;
#95603 = CARTESIAN_POINT ( 'NONE',  ( 0.5774900079438607392, 38.48035201082150536, 5.440088680355550821 ) ) ;
#95604 = CARTESIAN_POINT ( 'NONE',  ( 20.88017736071110519, 40.56368534415484106, 2.639326808657452039E-16 ) ) ;
#95605 = CARTESIAN_POINT ( 'NONE',  ( 20.88017736071110519, 50.56368534415484106, 2.639326808657452039E-16 ) ) ;
#95606 = CARTESIAN_POINT ( 'NONE',  ( 19.42250999205614193, 35.14701867748816966, 5.440088680355555262 ) ) ;
#95607 = CARTESIAN_POINT ( 'NONE',  ( 2.603489959281613420, 45.43575266056827644, -6.500000000000031086 ) ) ;
#95608 = CIRCLE ( 'NONE', #98855, 14.49999999999999822 ) ;
#95609 = ADVANCED_FACE ( 'NONE', ( #18554 ), #35009, .T. ) ;
#95610 = B_SPLINE_CURVE_WITH_KNOTS ( 'NONE', 3,
 ( #14932, #85377, #45399, #54375, #22923, #914 ),
 .UNSPECIFIED., .F., .F.,
 ( 4, 2, 4 ),
 ( 0.000000000000000000, 0.0002565770811490922947, 0.0005131541622981845895 ),
 .UNSPECIFIED. ) ;
#95612 = EDGE_LOOP ( 'NONE', ( #13357, #32232, #45360, #95177 ) ) ;
#95611 = CARTESIAN_POINT ( 'NONE',  ( -9.722841580490317881, 15.00000000000000000, -12.70211588817950066 ) ) ;
#95613 = CARTESIAN_POINT ( 'NONE',  ( 5.076628168052704559, 20.17559781766745175, -8.527530157486179263 ) ) ;
#95614 = VERTEX_POINT ( 'NONE', #41570 ) ;
#95615 = CARTESIAN_POINT ( 'NONE',  ( 10.79852199278004754, -95.56374241347876364, 4.000000000000000000 ) ) ;
#95616 = CARTESIAN_POINT ( 'NONE',  ( 7.361572987183170547, 52.05059781766745175, 9.846743663894590881 ) ) ;
#95617 = EDGE_CURVE ( 'NONE', #52000, #87579, #43844, .T. ) ;
#95618 = CARTESIAN_POINT ( 'NONE',  ( 4.838527690343521925, 0.5000000000000004441, 14.19819177887730177 ) ) ;
#95619 = VERTEX_POINT ( 'NONE', #5029 ) ;
#95620 = CARTESIAN_POINT ( 'NONE',  ( -46.56032334906372938, 103.8061263278359689, 5.692785474546972146 ) ) ;
#95621 = CARTESIAN_POINT ( 'NONE',  ( -1.354709868695416208, 14.63595249122790598, -14.93870011653153895 ) ) ;
#95623 = CARTESIAN_POINT ( 'NONE',  ( 0.1532563361054100626, 30.80059781766744820, -2.638427012816831230 ) ) ;
#95622 = CARTESIAN_POINT ( 'NONE',  ( 1.354709868695618935, 0.5000000000000004441, -14.93870011653151586 ) ) ;
#95624 = CARTESIAN_POINT ( 'NONE',  ( -4.164238869374098151, 66.59541550158060375, -3.795296366450310543 ) ) ;
#95625 = CARTESIAN_POINT ( 'NONE',  ( 0.000000000000000000, 15.00000000000000000, 0.000000000000000000 ) ) ;
#95626 = ORIENTED_EDGE ( 'NONE', *, *, #22946, .T. ) ;
#95627 = CARTESIAN_POINT ( 'NONE',  ( 0.2751277870542967463, 70.00000000000000000, -6.500000000000000888 ) ) ;
#95628 = CARTESIAN_POINT ( 'NONE',  ( 0.1532563361054083140, 31.00893115100078390, 1.131784320476157264E-15 ) ) ;
#95629 = ADVANCED_FACE ( 'NONE', ( #87533 ), #88021, .T. ) ;
#95630 = CARTESIAN_POINT ( 'NONE',  ( 11.57153612472183646, -43.60599867514397943, 3.750000000000000000 ) ) ;
#95631 = CARTESIAN_POINT ( 'NONE',  ( -2.816281873526473856, -0.6680319967362464695, 3.434112377981055619 ) ) ;
#95632 = CARTESIAN_POINT ( 'NONE',  ( 2.791683348922237240, 0.3839311510007847872, -7.208316651077763204 ) ) ;
#95633 = CIRCLE ( 'NONE', #98880, 2.999999999999999112 ) ;
#95634 = CARTESIAN_POINT ( 'NONE',  ( 0.1532563361054082862, 16.21726448433411960, 2.638427012816831674 ) ) ;
#95635 = CARTESIAN_POINT ( 'NONE',  ( 17.20831665107776587, 62.88393115100078745, 7.208316651077764980 ) ) ;
#95636 = CYLINDRICAL_SURFACE ( 'NONE', #36101, 11.92686044187656513 ) ;
#95637 = EDGE_CURVE ( 'NONE', #25751, #12094, #83774, .T. ) ;
#95638 = ORIENTED_EDGE ( 'NONE', *, *, #51915, .T. ) ;
#95639 = CARTESIAN_POINT ( 'NONE',  ( -0.8801773607111009756, 13.06368534415483929, 1.068504757029289695E-15 ) ) ;
#95640 = CARTESIAN_POINT ( 'NONE',  ( 24.16423886937410614, 4.303748834913967869, 8.672049930838204340E-16 ) ) ;
#95641 = CARTESIAN_POINT ( 'NONE',  ( 19.84674366389459266, 8.300597817667451750, 2.638427012816836559 ) ) ;
#95642 = CARTESIAN_POINT ( 'NONE',  ( 12.91533473730992121, 39.52201867748817676, 10.88017736071110164 ) ) ;
#95644 = CARTESIAN_POINT ( 'NONE',  ( 17.96484262340118221, 64.93868534415483396, 7.964842623401181321 ) ) ;
#95643 = CARTESIAN_POINT ( 'NONE',  ( 22.81628187352648496, 31.83196800326375353, -3.434112377981050290 ) ) ;
#95645 = SURFACE_STYLE_USAGE ( .BOTH. , #11154 ) ;
#95646 = ADVANCED_FACE ( 'NONE', ( #96033 ), #65511, .T. ) ;
#95647 = DIRECTION ( 'NONE',  ( 0.000000000000000000, 0.000000000000000000, 1.000000000000000000 ) ) ;
#95648 = SURFACE_STYLE_FILL_AREA ( #42643 ) ;
#95649 = AXIS2_PLACEMENT_3D ( 'NONE', #26192, #56684, #11679 ) ;
#95650 = CARTESIAN_POINT ( 'NONE',  ( 0.1532563361054083140, 51.00893115100078745, 1.131784320476157264E-15 ) ) ;
#95651 = CARTESIAN_POINT ( 'NONE',  ( 10.00000000000000000, 14.75893115100078568, -9.846743663894594434 ) ) ;
#95652 = CARTESIAN_POINT ( 'NONE',  ( -5.440088680355558814, -22.76964798917849109, -9.422509992056136596 ) ) ;
#95653 = CARTESIAN_POINT ( 'NONE',  ( 0.6178305044545818747, 28.49863466993041783, -9.382169495545419124 ) ) ;
#95654 = CARTESIAN_POINT ( 'NONE',  ( -11.26382985214544696, -93.42670896122723434, -3.999999999999098943 ) ) ;
#95656 = DIRECTION ( 'NONE',  ( -0.000000000000000000, 1.000000000000000000, -0.000000000000000000 ) ) ;
#95655 = CARTESIAN_POINT ( 'NONE',  ( 20.88017736071110875, 30.77201867748816966, -2.915334737309920765 ) ) ;
#95657 = DIRECTION ( 'NONE',  ( -0.000000000000000000, -1.000000000000000000, -0.000000000000000000 ) ) ;
#95658 = CARTESIAN_POINT ( 'NONE',  ( 24.16423886937410614, 44.30374883491397497, 8.672049930838204340E-16 ) ) ;
#95659 = CARTESIAN_POINT ( 'NONE',  ( 1.780824192092386404, 14.49999999999999112, 14.89391369643520946 ) ) ;
#95660 = CARTESIAN_POINT ( 'NONE',  ( 5.076628168052704559, 45.17559781766745175, -8.527530157486179263 ) ) ;
#95661 = CARTESIAN_POINT ( 'NONE',  ( -1.099225684535947600, 33.70696800326375353, -6.408140936763238038 ) ) ;
#95662 = CARTESIAN_POINT ( 'NONE',  ( 7.084665262690076126, 24.10535201082150181, 10.88017736071109987 ) ) ;
#95663 = CARTESIAN_POINT ( 'NONE',  ( 17.20831665107776587, 57.88393115100078745, 7.208316651077764980 ) ) ;
#95664 = CARTESIAN_POINT ( 'NONE',  ( 2.035157376598824452, 48.68868534415483396, 7.964842623401179544 ) ) ;
#95665 = CARTESIAN_POINT ( 'NONE',  ( 3.591859063236761518, 9.956968003263753531, 11.09922568453594849 ) ) ;
#95666 = CARTESIAN_POINT ( 'NONE',  ( 20.36894250292379382, 38.67874883491396076, 10.36894250292379205 ) ) ;
#95667 = CARTESIAN_POINT ( 'NONE',  ( -14.88640444357865711, 14.76930270348885088, -1.277895705730453413 ) ) ;
#95668 = CARTESIAN_POINT ( 'NONE',  ( 1.472469842513823179, 31.42559781766745530, 4.923371831947296329 ) ) ;
#95669 = CARTESIAN_POINT ( 'NONE',  ( 21.09922568453594849, 61.20696800326376064, 6.408140936763242479 ) ) ;
#95670 = CARTESIAN_POINT ( 'NONE',  ( 22.81628187352647785, 1.415301336597087012, 3.434112377981063169 ) ) ;
#95671 = VERTEX_POINT ( 'NONE', #74003 ) ;
#95672 = CARTESIAN_POINT ( 'NONE',  ( 6.878063601867475008, -66.29791949882819324, 2.750000000000000000 ) ) ;
#95673 = CARTESIAN_POINT ( 'NONE',  ( 20.88017736071110875, 10.77201867748817143, -2.915334737309920765 ) ) ;
#95674 = PRESENTATION_LAYER_ASSIGNMENT (  '', '', ( #9454 ) ) ;
#95676 = CARTESIAN_POINT ( 'NONE',  ( 12.25993886608599581, 15.00000000000000000, 8.642563219313704082 ) ) ;
#95675 = CARTESIAN_POINT ( 'NONE',  ( -4.164238869374099039, 26.80374883491397142, 8.674139862899312516E-16 ) ) ;
#95677 = CARTESIAN_POINT ( 'NONE',  ( 12.91533473730993009, 66.60535201082150536, -10.88017736071109987 ) ) ;
#95678 = CARTESIAN_POINT ( 'NONE',  ( 2.791683348922237240, 45.38393115100079456, -7.208316651077763204 ) ) ;
#95679 = CARTESIAN_POINT ( 'NONE',  ( 0.5774900079438607392, 28.48035201082150891, 5.440088680355550821 ) ) ;
#95680 = DIRECTION ( 'NONE',  ( 0.000000000000000000, 0.000000000000000000, 1.000000000000000000 ) ) ;
#95681 = CARTESIAN_POINT ( 'NONE',  ( 2.550000000000003819, 99.99999999999998579, -8.525133428036873795 ) ) ;
#95682 = VECTOR ( 'NONE', #7061, 1000.000000000000114 ) ;
#95683 = ADVANCED_FACE ( 'NONE', ( #4054 ), #72037, .T. ) ;
#95684 = ORIENTED_EDGE ( 'NONE', *, *, #75311, .T. ) ;
#95685 = B_SPLINE_CURVE_WITH_KNOTS ( 'NONE', 3,
 ( #45464, #61446, #54923, #67981, #16946, #7975 ),
 .UNSPECIFIED., .F., .F.,
 ( 4, 2, 4 ),
 ( 0.0002800086601672329388, 0.0006862139742886589440, 0.001092419288410084949 ),
 .UNSPECIFIED. ) ;
#95686 = CARTESIAN_POINT ( 'NONE',  ( 8.209432707284774366, 14.49999999999999822, 12.55409154915492032 ) ) ;
#95687 = ORIENTED_EDGE ( 'NONE', *, *, #87068, .F. ) ;
#95688 = ORIENTED_EDGE ( 'NONE', *, *, #39123, .T. ) ;
#95689 = CARTESIAN_POINT ( 'NONE',  ( 2.603489959281592991, 11.58210964143329313, 6.500000000000006217 ) ) ;
#95690 = CARTESIAN_POINT ( 'NONE',  ( 24.16423886937410614, 4.303748834913967869, 8.672049930838204340E-16 ) ) ;
#95691 = CARTESIAN_POINT ( 'NONE',  ( 6.204703633549690345, 5.762082168247301794, -14.16423886937410259 ) ) ;
#95692 = CARTESIAN_POINT ( 'NONE',  ( 7.084665262690076126, 49.10535201082149825, 10.88017736071109987 ) ) ;
#95693 = CARTESIAN_POINT ( 'NONE',  ( -0.3689425029237898834, 61.17874883491396076, -10.36894250292378850 ) ) ;
#95694 = CARTESIAN_POINT ( 'NONE',  ( 14.92337183194729633, 57.67559781766745886, 8.527530157486181039 ) ) ;
#95695 = CARTESIAN_POINT ( 'NONE',  ( 7.361572987183170547, 37.05059781766744464, 9.846743663894590881 ) ) ;
#95696 = CARTESIAN_POINT ( 'NONE',  ( -14.54804176595373555, 15.00000000000000000, -6.650705016170777917 ) ) ;
#95698 = CARTESIAN_POINT ( 'NONE',  ( 1.472469842513823179, 61.42559781766745175, 4.923371831947296329 ) ) ;
#95697 = CARTESIAN_POINT ( 'NONE',  ( 7.084665262690076126, 34.10535201082151247, 10.88017736071109987 ) ) ;
#95699 = CARTESIAN_POINT ( 'NONE',  ( 13.79529636645030344, 8.262082168247300018, 14.16423886937410614 ) ) ;
#95700 = B_SPLINE_CURVE_WITH_KNOTS ( 'NONE', 3,
 ( #28393, #50894, #11056, #88899, #56074, #79052, #10564, #65887, #13390, #20408, #41576, #36391, #89388, #72044, #20902, #51391, #74369, #97403, #7388, #37886, #92344, #61349, #400, #7876, #22883, #14392, #30350, #23870 ),
 .UNSPECIFIED., .F., .F.,
 ( 4, 2, 2, 2, 2, 2, 2, 2, 2, 2, 2, 2, 2, 4 ),
 ( 0.000000000000000000, 0.001557342785199824619, 0.003114685570399649238, 0.006229371140799340109, 0.01245874228159868022, 0.02491748456319740554, 0.03737622684479612045, 0.04983496912639484577, 0.06229371140799356416, 0.07475245368959228254, 0.08721119597119100786, 0.09344056711199036358, 0.09655525268239005532, 0.09966993825278973318 ),
 .UNSPECIFIED. ) ;
#95701 = CARTESIAN_POINT ( 'NONE',  ( 2.917880565312950480, 50.97041550158064638, -12.26659068614894821 ) ) ;
#95702 = CARTESIAN_POINT ( 'NONE',  ( 4.559911319644449179, 3.897018677488171434, 9.422509992056141925 ) ) ;
#95703 = CARTESIAN_POINT ( 'NONE',  ( 5.500000000000000000, 60.50000000000000711, 6.000000000000000000 ) ) ;
#95704 = LINE ( 'NONE', #50186, #15629 ) ;
#95705 = CARTESIAN_POINT ( 'NONE',  ( 8.527530157486179263, -36.90773551566588395, 4.923371831947292776 ) ) ;
#95706 = VERTEX_POINT ( 'NONE', #50030 ) ;
#95707 =( NAMED_UNIT ( * ) PLANE_ANGLE_UNIT ( ) SI_UNIT ( $, .RADIAN. ) );
#95708 = ORIENTED_EDGE ( 'NONE', *, *, #68527, .F. ) ;
#95709 = CARTESIAN_POINT ( 'NONE',  ( 19.84674366389459621, 28.50893115100078745, 7.409399052514197653E-17 ) ) ;
#95710 = ORIENTED_EDGE ( 'NONE', *, *, #64564, .F. ) ;
#95711 = CARTESIAN_POINT ( 'NONE',  ( 22.26659068614894466, 33.88708216824730357, 7.082119434687054849 ) ) ;
#95712 = CARTESIAN_POINT ( 'NONE',  ( 14.92337183194729633, 37.67559781766745175, 8.527530157486181039 ) ) ;
#95713 = CARTESIAN_POINT ( 'NONE',  ( 15.44008868035555793, 51.39701867748816966, -9.422509992056140149 ) ) ;
#95714 = AXIS2_PLACEMENT_3D ( 'NONE', #5919, #97425, #26934 ) ;
#95715 = DIRECTION ( 'NONE',  ( 0.000000000000000000, 0.000000000000000000, -1.000000000000000000 ) ) ;
#95716 = CARTESIAN_POINT ( 'NONE',  ( 7.084665262690076126, 57.02201867748817676, -10.88017736071110164 ) ) ;
#95717 = CARTESIAN_POINT ( 'NONE',  ( 3.591859063236761518, 59.95696800326375353, 11.09922568453594849 ) ) ;
#95718 = CARTESIAN_POINT ( 'NONE',  ( -6.408140936763246032, 13.29030133659709456, -11.09922568453594316 ) ) ;
#95719 = ORIENTED_EDGE ( 'NONE', *, *, #31633, .F. ) ;
#95720 = CARTESIAN_POINT ( 'NONE',  ( 10.00000000000000000, 25.55374883491396787, -14.16423886937410082 ) ) ;
#95721 = ORIENTED_EDGE ( 'NONE', *, *, #33098, .F. ) ;
#95722 = CARTESIAN_POINT ( 'NONE',  ( 3.591859063236763294, 38.29030133659708923, -11.09922568453595026 ) ) ;
#95723 = AXIS2_PLACEMENT_3D ( 'NONE', #73036, #88044, #88541 ) ;
#95724 = CARTESIAN_POINT ( 'NONE',  ( 20.88017736071110875, 20.77201867748816611, -2.915334737309920765 ) ) ;
#95725 = CARTESIAN_POINT ( 'NONE',  ( 17.20831665107776587, 29.13393115100078390, -7.208316651077762316 ) ) ;
#95726 = CARTESIAN_POINT ( 'NONE',  ( 4.559911319644449179, 7.230352010821504471, -9.422509992056141925 ) ) ;
#95727 = CARTESIAN_POINT ( 'NONE',  ( 3.591859063236761518, 59.95696800326375353, 11.09922568453594849 ) ) ;
#95728 = PLANE ( 'NONE',  #73485 ) ;
#95729 = CARTESIAN_POINT ( 'NONE',  ( 10.00000000000000000, 24.75893115100078745, -9.846743663894594434 ) ) ;
#95730 = TOROIDAL_SURFACE ( 'NONE', #22311, 14.49999999999999822, 0.5000000000000000000 ) ;
#95731 = CARTESIAN_POINT ( 'NONE',  ( 19.42250999205614548, 50.98035201082151247, -5.440088680355545492 ) ) ;
#95733 = ORIENTED_EDGE ( 'NONE', *, *, #25776, .F. ) ;
#95732 = CARTESIAN_POINT ( 'NONE',  ( 7.084665262690076126, 69.10535201082151957, 10.88017736071109987 ) ) ;
#95734 = EDGE_CURVE ( 'NONE', #22423, #73925, #80240, .T. ) ;
#95735 = CARTESIAN_POINT ( 'NONE',  ( 14.71525861348295727, 14.49999999999999112, -2.908807992686619048 ) ) ;
#95736 = LINE ( 'NONE', #19728, #49842 ) ;
#95737 = DIRECTION ( 'NONE',  ( 0.000000000000000000, 0.000000000000000000, 1.000000000000000000 ) ) ;
#95738 = ADVANCED_FACE ( 'NONE', ( #59498 ), #38001, .T. ) ;
#95739 = DIRECTION ( 'NONE',  ( 3.375077994860475883E-14, 0.000000000000000000, 1.000000000000000000 ) ) ;
#95740 = CARTESIAN_POINT ( 'NONE',  ( 19.84674366389459266, 8.300597817667451750, 2.638427012816836559 ) ) ;
#95741 = EDGE_CURVE ( 'NONE', #96981, #73925, #86148, .T. ) ;
#95742 = CARTESIAN_POINT ( 'NONE',  ( 16.40814093676323893, 30.79030133659708923, 11.09922568453595026 ) ) ;
#95743 = SPHERICAL_SURFACE ( 'NONE', #77051, 0.2500000000000000000 ) ;
#95744 = CARTESIAN_POINT ( 'NONE',  ( 2.791683348922237240, 40.38393115100078035, -7.208316651077763204 ) ) ;
#95745 = DIRECTION ( 'NONE',  ( 1.000000000000000000, 0.000000000000000000, 0.000000000000000000 ) ) ;
#95746 = CARTESIAN_POINT ( 'NONE',  ( -0.3689425029237898834, 16.17874883491396076, -10.36894250292378850 ) ) ;
#95747 = CARTESIAN_POINT ( 'NONE',  ( 0.1532563361054082862, 36.21726448433410894, 2.638427012816831674 ) ) ;
#95748 = CARTESIAN_POINT ( 'NONE',  ( 0.6178305044545838731, 34.74863466993042493, 9.382169495545420901 ) ) ;
#95750 = DIRECTION ( 'NONE',  ( 6.608470384673550777E-17, 1.000000000000000000, -0.000000000000000000 ) ) ;
#95749 = CARTESIAN_POINT ( 'NONE',  ( 18.72515096720570327, 16.07228050351031712, -6.499999999999992006 ) ) ;
#95751 = CARTESIAN_POINT ( 'NONE',  ( 4.559911319644449179, 62.23035201082150536, -9.422509992056141925 ) ) ;
#95752 = CARTESIAN_POINT ( 'NONE',  ( 22.81628187352647785, 11.41530133659708390, 3.434112377981063169 ) ) ;
#95753 = DIRECTION ( 'NONE',  ( 0.000000000000000000, 0.000000000000000000, 1.000000000000000000 ) ) ;
#95754 = CARTESIAN_POINT ( 'NONE',  ( 14.92337183194729988, 34.34226448433411605, -8.527530157486177487 ) ) ;
#95755 = CARTESIAN_POINT ( 'NONE',  ( 20.88017736071110875, 20.77201867748816611, -2.915334737309920765 ) ) ;
#95756 = CARTESIAN_POINT ( 'NONE',  ( 13.43411237798106583, 32.66530133659708213, -12.81628187352647252 ) ) ;
#95757 = CARTESIAN_POINT ( 'NONE',  ( 10.00000000000000000, 29.75893115100078745, -9.846743663894594434 ) ) ;
#95758 = CARTESIAN_POINT ( 'NONE',  ( 14.99847009497945649, 14.63595249122788999, 0.2142307401081327833 ) ) ;
#95759 = CARTESIAN_POINT ( 'NONE',  ( 7.084665262690076126, 32.02201867748816966, -10.88017736071110164 ) ) ;
#95760 = ORIENTED_EDGE ( 'NONE', *, *, #69832, .F. ) ;
#95761 = CARTESIAN_POINT ( 'NONE',  ( -8.235571585149864760, 3.546802177851540172, 8.235571585149875418 ) ) ;
#95762 = CARTESIAN_POINT ( 'NONE',  ( 15.44008868035555260, 4.730352010821504471, 9.422509992056143702 ) ) ;
#95764 = CARTESIAN_POINT ( 'NONE',  ( 4.559911319644449179, 33.89701867748817676, 9.422509992056141925 ) ) ;
#95763 = CARTESIAN_POINT ( 'NONE',  ( 0.1532563361054082862, 51.21726448433412315, 2.638427012816831674 ) ) ;
#95765 = DIRECTION ( 'NONE',  ( 0.000000000000000000, 0.000000000000000000, 1.000000000000000000 ) ) ;
#95766 = EDGE_CURVE ( 'NONE', #71601, #79717, #71008, .T. ) ;
#95767 = CARTESIAN_POINT ( 'NONE',  ( 10.00000000000000178, 64.31368534415483396, 10.88017736071110342 ) ) ;
#95768 = CIRCLE ( 'NONE', #9544, 15.00000000000000000 ) ;
#95770 = CARTESIAN_POINT ( 'NONE',  ( 0.000000000000000000, 75.66482536767503575, -6.574273087692857231 ) ) ;
#95769 = CARTESIAN_POINT ( 'NONE',  ( 7.084665262690076126, 29.10535201082150181, 10.88017736071109987 ) ) ;
#95771 =( NAMED_UNIT ( * ) SI_UNIT ( $, .STERADIAN. ) SOLID_ANGLE_UNIT ( ) );
#95772 = LINE ( 'NONE', #36248, #96900 ) ;
#95773 = CARTESIAN_POINT ( 'NONE',  ( 18.52753015748617571, 53.09226448433412315, 4.923371831947298993 ) ) ;
#95774 = TOROIDAL_SURFACE ( 'NONE', #73418, 6.499999999999995559, 0.5000000000000000000 ) ;
#95776 = CARTESIAN_POINT ( 'NONE',  ( 21.92686044187656691, 19.95379003517448169, 3.195792623639537755 ) ) ;
#95775 = CARTESIAN_POINT ( 'NONE',  ( -4.164238869374099927, 52.01208216824729647, 3.795296366450308767 ) ) ;
#95777 = CARTESIAN_POINT ( 'NONE',  ( -13.78891971893212443, 15.00000000000000000, 5.904717858191433244 ) ) ;
#95778 =( GEOMETRIC_REPRESENTATION_CONTEXT ( 3 ) GLOBAL_UNCERTAINTY_ASSIGNED_CONTEXT ( ( #76114 ) ) GLOBAL_UNIT_ASSIGNED_CONTEXT ( ( #94242, #18263, #56741 ) ) REPRESENTATION_CONTEXT ( 'NONE', 'WORKASPACE' ) );
#95779 = CARTESIAN_POINT ( 'NONE',  ( 17.08211943468705840, 15.13708216824730179, -12.26659068614894466 ) ) ;
#95780 = CARTESIAN_POINT ( 'NONE',  ( 24.16423886937409904, 44.09541550158063927, 3.795296366450317205 ) ) ;
#95781 = CARTESIAN_POINT ( 'NONE',  ( 16.40814093676323893, 5.790301336597087456, 11.09922568453595026 ) ) ;
#95782 = CARTESIAN_POINT ( 'NONE',  ( 11.10000000000000142, 98.49999999999998579, -8.000000000000000000 ) ) ;
#95783 = ORIENTED_EDGE ( 'NONE', *, *, #23470, .F. ) ;
#95784 = CARTESIAN_POINT ( 'NONE',  ( 10.00000000000000000, 65.55374883491396076, -14.16423886937410082 ) ) ;
#95785 = CARTESIAN_POINT ( 'NONE',  ( 12.63842701281683922, 39.55059781766744464, -9.846743663894590881 ) ) ;
#95787 = CARTESIAN_POINT ( 'NONE',  ( -4.431036607602373500, 15.00000000000000000, -14.33059365769916838 ) ) ;
#95786 = DIRECTION ( 'NONE',  ( 0.000000000000000000, 0.000000000000000000, -1.000000000000000000 ) ) ;
#95788 = CARTESIAN_POINT ( 'NONE',  ( 10.00000000000000000, 56.81368534415484106, -10.88017736071110342 ) ) ;
#95789 = DIRECTION ( 'NONE',  ( -0.000000000000000000, -0.000000000000000000, -1.000000000000000000 ) ) ;
#95790 = CARTESIAN_POINT ( 'NONE',  ( 19.38216949554541202, 55.99863466993041072, 9.382169495545424454 ) ) ;
#95791 = CARTESIAN_POINT ( 'NONE',  ( 16.40814093676323893, 30.79030133659708923, 11.09922568453595026 ) ) ;
#95792 = CARTESIAN_POINT ( 'NONE',  ( 18.52753015748617571, 28.09226448433411960, 4.923371831947298993 ) ) ;
#95793 = VERTEX_POINT ( 'NONE', #36513 ) ;
#95794 = CYLINDRICAL_SURFACE ( 'NONE', #3831, 0.2500000000000002220 ) ;
#95795 = CARTESIAN_POINT ( 'NONE',  ( -9.000000000000001776, 83.99999999999994316, 3.000000000000000000 ) ) ;
#95796 = CARTESIAN_POINT ( 'NONE',  ( -2.266590686148945544, 61.38708216824730357, -7.082119434687050408 ) ) ;
#95797 = CARTESIAN_POINT ( 'NONE',  ( -0.8801773607111009756, 18.06368534415484106, 1.068504757029289695E-15 ) ) ;
#95798 = CARTESIAN_POINT ( 'NONE',  ( 20.36894250292379382, 43.67874883491397497, 10.36894250292379205 ) ) ;
#95799 = CARTESIAN_POINT ( 'NONE',  ( -0.8801773607110991993, 32.85535201082151247, -2.915334737309923874 ) ) ;
#95800 = CARTESIAN_POINT ( 'NONE',  ( 0.5774900079438607392, 63.48035201082149825, 5.440088680355550821 ) ) ;
#95801 = FACE_OUTER_BOUND ( 'NONE', #67204, .T. ) ;
#95802 = AXIS2_PLACEMENT_3D ( 'NONE', #62299, #70818, #10794 ) ;
#95803 = CARTESIAN_POINT ( 'NONE',  ( 5.803070148808231465, 15.00000000000000000, 13.28812917035392260 ) ) ;
#95804 = CARTESIAN_POINT ( 'NONE',  ( 14.92337183194729633, 12.67559781766745353, 8.527530157486181039 ) ) ;
#95805 = CARTESIAN_POINT ( 'NONE',  ( 0.2751277870542967463, 0.000000000000000000, 6.500000000000000888 ) ) ;
#95806 = CARTESIAN_POINT ( 'NONE',  ( -14.40939250469964783, 15.00000000000000000, 1.618458416365647023 ) ) ;
#95807 = FILL_AREA_STYLE ('',( #80300 ) ) ;
#95808 = CARTESIAN_POINT ( 'NONE',  ( 1.472469842513823179, 40.59226448433411605, -4.923371831947296329 ) ) ;
#95809 = CARTESIAN_POINT ( 'NONE',  ( 18.52753015748617571, 58.09226448433411605, 4.923371831947298993 ) ) ;
#95810 = CARTESIAN_POINT ( 'NONE',  ( 10.00000000000000178, 29.31368534415483751, 10.88017736071110342 ) ) ;
#95811 = EDGE_LOOP ( 'NONE', ( #80022, #73196, #69623, #1274, #40052, #46353 ) ) ;
#95812 = CARTESIAN_POINT ( 'NONE',  ( 10.00000000000000178, 50.37363466993042493, 12.81628187352647608 ) ) ;
#95813 = PRESENTATION_STYLE_ASSIGNMENT (( #11315 ) ) ;
#95814 = CARTESIAN_POINT ( 'NONE',  ( 15.44008868035555260, 59.73035201082151247, 9.422509992056143702 ) ) ;
#95815 = CARTESIAN_POINT ( 'NONE',  ( 0.1532563361054083140, 26.00893115100078745, 1.131784320476157264E-15 ) ) ;
#95817 = CARTESIAN_POINT ( 'NONE',  ( 5.076628168052704559, 20.17559781766745175, -8.527530157486179263 ) ) ;
#95816 = CARTESIAN_POINT ( 'NONE',  ( -2.266590686148945544, 56.38708216824731068, -7.082119434687050408 ) ) ;
#95818 = CARTESIAN_POINT ( 'NONE',  ( -0.04068437667222160603, 47.21974360917721469, -6.396802510829771471 ) ) ;
#95819 = CARTESIAN_POINT ( 'NONE',  ( 0.1532563361054082862, 61.21726448433412315, 2.638427012816831674 ) ) ;
#95820 = CARTESIAN_POINT ( 'NONE',  ( 6.204703633549690345, 30.76208216824730357, -14.16423886937410259 ) ) ;
#95821 = CARTESIAN_POINT ( 'NONE',  ( 18.52753015748617571, 38.09226448433412315, 4.923371831947298993 ) ) ;
#95822 = CARTESIAN_POINT ( 'NONE',  ( 14.47650479471822216, 15.00000000000000000, -3.928206833722012625 ) ) ;
#95823 = CARTESIAN_POINT ( 'NONE',  ( 0.5774900079438590739, 27.64701867748817676, -5.440088680355550821 ) ) ;
#95824 = CARTESIAN_POINT ( 'NONE',  ( 17.96484262340118221, 64.93868534415483396, 7.964842623401181321 ) ) ;
#95825 = FACE_OUTER_BOUND ( 'NONE', #63610, .T. ) ;
#95826 = VERTEX_POINT ( 'NONE', #91480 ) ;
#95827 = CARTESIAN_POINT ( 'NONE',  ( 21.09922568453594849, 41.20696800326375353, 6.408140936763242479 ) ) ;
#95828 = CARTESIAN_POINT ( 'NONE',  ( 10.00000000000000178, 54.31368534415484106, 10.88017736071110342 ) ) ;
#95829 = ORIENTED_EDGE ( 'NONE', *, *, #28330, .F. ) ;
#95830 = EDGE_CURVE ( 'NONE', #94433, #46057, #52487, .T. ) ;
#95831 = PLANE ( 'NONE',  #33847 ) ;
#95832 = CARTESIAN_POINT ( 'NONE',  ( 0.000000000000000000, 14.49999999999999822, 0.000000000000000000 ) ) ;
#95833 = ORIENTED_EDGE ( 'NONE', *, *, #65959, .F. ) ;
#95834 = CARTESIAN_POINT ( 'NONE',  ( 4.559911319644449179, 63.89701867748817676, 9.422509992056141925 ) ) ;
#95835 = CARTESIAN_POINT ( 'NONE',  ( 4.559911319644449179, 13.89701867748817143, 9.422509992056141925 ) ) ;
#95836 = CARTESIAN_POINT ( 'NONE',  ( 0.1532563361054083140, 1.008931151000784787, 1.131784320476157264E-15 ) ) ;
#95837 = LINE ( 'NONE', #82670, #98418 ) ;
#95838 = CARTESIAN_POINT ( 'NONE',  ( -0.8801773607111009756, 3.063685344154838397, 1.068504757029289695E-15 ) ) ;
#95839 = CARTESIAN_POINT ( 'NONE',  ( 17.20831665107776587, 4.133931151000785675, -7.208316651077762316 ) ) ;
#95840 = CARTESIAN_POINT ( 'NONE',  ( -2.266590686148945544, 16.38708216824730357, -7.082119434687050408 ) ) ;
#95841 = CARTESIAN_POINT ( 'NONE',  ( 17.96484262340118221, 21.18868534415483396, -7.964842623401177768 ) ) ;
#95842 = CARTESIAN_POINT ( 'NONE',  ( 12.63842701281683034, 62.46726448433410894, 9.846743663894596210 ) ) ;
#95843 = ORIENTED_EDGE ( 'NONE', *, *, #59434, .T. ) ;
#95844 = CARTESIAN_POINT ( 'NONE',  ( 2.791683348922237240, 65.38393115100078035, -7.208316651077763204 ) ) ;
#95845 = ORIENTED_EDGE ( 'NONE', *, *, #78802, .F. ) ;
#95846 = CARTESIAN_POINT ( 'NONE',  ( 17.96484262340118221, 54.93868534415484106, 7.964842623401181321 ) ) ;
#95848 = CARTESIAN_POINT ( 'NONE',  ( 14.92337183194729633, 62.67559781766745886, 8.527530157486181039 ) ) ;
#95847 = B_SPLINE_CURVE_WITH_KNOTS ( 'NONE', 3,
 ( #61089, #68115, #7627, #84101, #46101, #98131 ),
 .UNSPECIFIED., .F., .F.,
 ( 4, 2, 4 ),
 ( 0.0002800008091676943586, 0.0006862060465022846306, 0.001092411283836874957 ),
 .UNSPECIFIED. ) ;
#95849 = EDGE_CURVE ( 'NONE', #40524, #24045, #36156, .T. ) ;
#95850 = CARTESIAN_POINT ( 'NONE',  ( 22.81628187352648496, 41.83196800326375353, -3.434112377981050290 ) ) ;
#95852 = CARTESIAN_POINT ( 'NONE',  ( 5.000000000000002665, 44.99999999999999289, 7.000000000000000000 ) ) ;
#95851 = CARTESIAN_POINT ( 'NONE',  ( 10.00000000000000178, 4.313685344154837509, 10.88017736071110342 ) ) ;
#95853 = CARTESIAN_POINT ( 'NONE',  ( 17.96484262340118221, 64.93868534415483396, 7.964842623401181321 ) ) ;
#95854 = AXIS2_PLACEMENT_3D ( 'NONE', #84307, #46292, #8296 ) ;
#95855 = CARTESIAN_POINT ( 'NONE',  ( 15.44008868035555260, 9.730352010821505360, 9.422509992056143702 ) ) ;
#95856 = EDGE_CURVE ( 'NONE', #70759, #66028, #13457, .T. ) ;
#95857 = VERTEX_POINT ( 'NONE', #14514 ) ;
#95858 = CARTESIAN_POINT ( 'NONE',  ( 6.565887622018943937, 35.16530133659708923, 12.81628187352647430 ) ) ;
#95859 = CARTESIAN_POINT ( 'NONE',  ( 12.91533473730992121, 24.52201867748816966, 10.88017736071110164 ) ) ;
#95860 = CARTESIAN_POINT ( 'NONE',  ( 0.9408516040111476464, 47.46693863883976405, -6.499999999999953815 ) ) ;
#95861 = ORIENTED_EDGE ( 'NONE', *, *, #23633, .T. ) ;
#95862 = CARTESIAN_POINT ( 'NONE',  ( 3.591859063236761518, 39.95696800326375353, 11.09922568453594849 ) ) ;
#95863 = CARTESIAN_POINT ( 'NONE',  ( 10.00000000000000000, 31.81368534415483751, -10.88017736071110342 ) ) ;
#95864 = EDGE_CURVE ( 'NONE', #93697, #39498, #79004, .T. ) ;
#95865 = CARTESIAN_POINT ( 'NONE',  ( 10.00000000000000178, 52.25893115100078745, 9.846743663894594434 ) ) ;
#95866 = ORIENTED_EDGE ( 'NONE', *, *, #54420, .T. ) ;
#95867 = CARTESIAN_POINT ( 'NONE',  ( -7.618485323809357723, 15.00000000000000711, 12.48587314215754773 ) ) ;
#95868 = B_SPLINE_CURVE_WITH_KNOTS ( 'NONE', 3,
 ( #12357, #227, #65843, #43344, #42864, #12844 ),
 .UNSPECIFIED., .F., .F.,
 ( 4, 2, 4 ),
 ( 0.0002800553958269955037, 0.0006862611673083459643, 0.001092466938789696425 ),
 .UNSPECIFIED. ) ;
#95869 = CARTESIAN_POINT ( 'NONE',  ( 2.791683348922240793, 61.63393115100079456, 7.208316651077764092 ) ) ;
#95871 = CARTESIAN_POINT ( 'NONE',  ( 1.472469842513823179, 51.42559781766745886, 4.923371831947296329 ) ) ;
#95870 = CARTESIAN_POINT ( 'NONE',  ( 0.2751277870542967463, 70.00000000000000000, -6.000000000000000000 ) ) ;
#95872 = CARTESIAN_POINT ( 'NONE',  ( 15.44008868035555793, 21.39701867748817321, -9.422509992056140149 ) ) ;
#95873 =( NAMED_UNIT ( * ) PLANE_ANGLE_UNIT ( ) SI_UNIT ( $, .RADIAN. ) );
#95874 = CARTESIAN_POINT ( 'NONE',  ( 14.92337183194729988, 39.34226448433412315, -8.527530157486177487 ) ) ;
#95875 = CARTESIAN_POINT ( 'NONE',  ( -46.82017113615791004, 100.6079546444643569, -9.324761308090124601 ) ) ;
#95876 = DIRECTION ( 'NONE',  ( -0.000000000000000000, -0.000000000000000000, 1.000000000000000000 ) ) ;
#95878 = CARTESIAN_POINT ( 'NONE',  ( 19.84674366389459621, 13.50893115100078568, 7.409399052514197653E-17 ) ) ;
#95877 = CARTESIAN_POINT ( 'NONE',  ( 5.076628168052704559, 40.17559781766745175, -8.527530157486179263 ) ) ;
#95879 = CARTESIAN_POINT ( 'NONE',  ( 0.1532563361054100626, 0.8005978176674514168, -2.638427012816831230 ) ) ;
#95881 = ORIENTED_EDGE ( 'NONE', *, *, #42334, .F. ) ;
#95880 = CARTESIAN_POINT ( 'NONE',  ( 5.076628168052703671, 61.84226448433412315, 8.527530157486179263 ) ) ;
#95882 = CARTESIAN_POINT ( 'NONE',  ( 10.00000000000000178, 65.37363466993042493, 12.81628187352647608 ) ) ;
#95883 = FILL_AREA_STYLE ('',( #44333 ) ) ;
#95884 = CIRCLE ( 'NONE', #32042, 7.250000000000002665 ) ;
#95885 = CARTESIAN_POINT ( 'NONE',  ( 19.38216949554541557, 42.24863466993041783, -9.382169495545420901 ) ) ;
#95886 = CARTESIAN_POINT ( 'NONE',  ( 10.00000000000000178, 42.25893115100078745, 9.846743663894594434 ) ) ;
#95887 = CARTESIAN_POINT ( 'NONE',  ( 15.86177583122252344, 15.00000000000000000, -2.069169861586653170 ) ) ;
#95888 = CARTESIAN_POINT ( 'NONE',  ( 10.00000000000000178, 58.05374883491397497, 14.16423886937410082 ) ) ;
#95889 = CARTESIAN_POINT ( 'NONE',  ( 7.361572987183170547, 27.05059781766745175, 9.846743663894590881 ) ) ;
#95890 = CARTESIAN_POINT ( 'NONE',  ( 0.1532563361054082862, 6.217264484334118713, 2.638427012816831674 ) ) ;
#95891 = DIRECTION ( 'NONE',  ( 0.9681476403781049678, 0.000000000000000000, 0.2503800040544527095 ) ) ;
#95892 = CARTESIAN_POINT ( 'NONE',  ( 24.16423886937409904, 59.09541550158063217, 3.795296366450317205 ) ) ;
#95893 = CARTESIAN_POINT ( 'NONE',  ( 10.00000000000000178, 67.25893115100079456, 9.846743663894594434 ) ) ;
#95894 = EDGE_CURVE ( 'NONE', #87579, #79151, #15805, .T. ) ;
#95895 = CARTESIAN_POINT ( 'NONE',  ( 7.084665262690076126, 7.022018677488170546, -10.88017736071110164 ) ) ;
#95896 = CARTESIAN_POINT ( 'NONE',  ( -2.266590686148945544, 37.22041550158063217, 7.082119434687048631 ) ) ;
#95898 = FACE_OUTER_BOUND ( 'NONE', #53058, .T. ) ;
#95897 = CARTESIAN_POINT ( 'NONE',  ( -0.3689425029237898834, 51.17874883491397497, -10.36894250292378850 ) ) ;
#95899 = DIRECTION ( 'NONE',  ( 0.000000000000000000, 1.000000000000000000, 0.000000000000000000 ) ) ;
#95900 = CARTESIAN_POINT ( 'NONE',  ( 7.361572987183169658, 9.967264484334119601, -9.846743663894592657 ) ) ;
#95902 = CARTESIAN_POINT ( 'NONE',  ( 12.63842701281683922, 64.55059781766745175, -9.846743663894590881 ) ) ;
#95901 = CYLINDRICAL_SURFACE ( 'NONE', #75696, 0.5000000000000004441 ) ;
#95903 = CARTESIAN_POINT ( 'NONE',  ( 2.035157376598824452, 48.68868534415483396, 7.964842623401179544 ) ) ;
#95904 = CARTESIAN_POINT ( 'NONE',  ( 14.92337183194729633, 47.67559781766745175, 8.527530157486181039 ) ) ;
#95905 = CARTESIAN_POINT ( 'NONE',  ( -18.89999999999999147, 91.25000000000000000, 7.750000000000000000 ) ) ;
#95906 = CARTESIAN_POINT ( 'NONE',  ( 12.63842701281683922, 59.55059781766744464, -9.846743663894590881 ) ) ;
#95907 = PRESENTATION_STYLE_ASSIGNMENT (( #64875 ) ) ;
#95908 = CIRCLE ( 'NONE', #24042, 15.00000000000000000 ) ;
#95909 = ORIENTED_EDGE ( 'NONE', *, *, #34474, .F. ) ;
#95910 = CARTESIAN_POINT ( 'NONE',  ( 20.36894250292379382, 23.67874883491397142, 10.36894250292379205 ) ) ;
#95911 = DIRECTION ( 'NONE',  ( 0.000000000000000000, 1.000000000000000000, 0.000000000000000000 ) ) ;
#95912 = CARTESIAN_POINT ( 'NONE',  ( -3.250000001579299802, 0.08818787376460503202, -2.500000000000000000 ) ) ;
#95913 = CARTESIAN_POINT ( 'NONE',  ( -0.8801773607111008646, 18.27201867748817321, 2.915334737309923430 ) ) ;
#95914 = CARTESIAN_POINT ( 'NONE',  ( 19.38216949554541202, 35.99863466993041072, 9.382169495545424454 ) ) ;
#95915 = CARTESIAN_POINT ( 'NONE',  ( -13.55255535720589322, 15.00000000000000000, -4.403492169843143067 ) ) ;
#95916 = CARTESIAN_POINT ( 'NONE',  ( 18.52753015748618282, 8.925597817667451750, -4.923371831947291888 ) ) ;
#95917 = CARTESIAN_POINT ( 'NONE',  ( 19.38216949554541557, 57.24863466993042493, -9.382169495545420901 ) ) ;
#95918 = ORIENTED_EDGE ( 'NONE', *, *, #35562, .T. ) ;
#95919 = DIRECTION ( 'NONE',  ( 0.000000000000000000, 0.000000000000000000, 1.000000000000000000 ) ) ;
#95920 = CARTESIAN_POINT ( 'NONE',  ( 20.36894250292379738, 24.92874883491396787, -10.36894250292379027 ) ) ;
#95921 = PRESENTATION_STYLE_ASSIGNMENT (( #65888 ) ) ;
#95922 = CARTESIAN_POINT ( 'NONE',  ( -7.366188783701793419, -80.69039970148938323, 3.999999999999999112 ) ) ;
#95923 = CARTESIAN_POINT ( 'NONE',  ( 20.88017736071110875, 10.77201867748817143, -2.915334737309920765 ) ) ;
#95924 = DIRECTION ( 'NONE',  ( 0.000000000000000000, 0.000000000000000000, -1.000000000000000000 ) ) ;
#95925 = CARTESIAN_POINT ( 'NONE',  ( 4.265659168453312944, 0.04922511925147125822, -14.12268572233451991 ) ) ;
#95926 = CARTESIAN_POINT ( 'NONE',  ( 10.00000000000000178, 39.31368534415484106, 10.88017736071110342 ) ) ;
#95927 = CARTESIAN_POINT ( 'NONE',  ( 20.88017736071110519, 45.56368534415484106, 2.639326808657452039E-16 ) ) ;
#95928 = CARTESIAN_POINT ( 'NONE',  ( 6.565887622018943937, 18.08196800326375708, -12.81628187352647608 ) ) ;
#95929 = CARTESIAN_POINT ( 'NONE',  ( 7.361572987183170547, 67.05059781766746596, 9.846743663894590881 ) ) ;
#95930 = DIRECTION ( 'NONE',  ( 0.000000000000000000, -1.000000000000000000, 0.000000000000000000 ) ) ;
#95931 = CARTESIAN_POINT ( 'NONE',  ( 5.076628168052704559, 10.17559781766745175, -8.527530157486179263 ) ) ;
#95932 = CARTESIAN_POINT ( 'NONE',  ( 8.879999999999999005, 20.99999999999999645, -1.249999999999987121 ) ) ;
#95933 = CARTESIAN_POINT ( 'NONE',  ( 12.91533473730992121, 44.52201867748816966, 10.88017736071110164 ) ) ;
#95934 = CARTESIAN_POINT ( 'NONE',  ( 19.38216949554541202, 5.998634669930420493, 9.382169495545424454 ) ) ;
#95935 = CARTESIAN_POINT ( 'NONE',  ( 4.559911319644449179, 57.23035201082150536, -9.422509992056141925 ) ) ;
#95936 = CARTESIAN_POINT ( 'NONE',  ( 10.00000000000000000, 19.75893115100078390, -9.846743663894594434 ) ) ;
#95937 = CARTESIAN_POINT ( 'NONE',  ( 6.565887622018943937, 43.08196800326374643, -12.81628187352647608 ) ) ;
#95938 = CARTESIAN_POINT ( 'NONE',  ( 17.20831665107776587, 9.133931151000787452, -7.208316651077762316 ) ) ;
#95939 = ORIENTED_EDGE ( 'NONE', *, *, #73384, .F. ) ;
#95940 = CARTESIAN_POINT ( 'NONE',  ( -8.000000000000000000, 80.07179676972448590, 4.250000000000000000 ) ) ;
#95941 = CARTESIAN_POINT ( 'NONE',  ( 19.72487221294570858, 0.000000000000000000, -6.500000000000000888 ) ) ;
#95942 = CARTESIAN_POINT ( 'NONE',  ( 19.42250999205614193, 20.14701867748817321, 5.440088680355555262 ) ) ;
#95943 = CARTESIAN_POINT ( 'NONE',  ( -2.816281873526471635, 53.91530133659709634, -3.434112377981056508 ) ) ;
#95944 = CARTESIAN_POINT ( 'NONE',  ( 7.361572987183170547, 37.05059781766744464, 9.846743663894590881 ) ) ;
#95945 = CARTESIAN_POINT ( 'NONE',  ( 2.035157376598822676, 12.43868534415483751, -7.964842623401177768 ) ) ;
#95946 = CARTESIAN_POINT ( 'NONE',  ( 6.204703633549690345, 67.84541550158060375, 14.16423886937410082 ) ) ;
#95947 = EDGE_LOOP ( 'NONE', ( #5109, #15329 ) ) ;
#95948 = AXIS2_PLACEMENT_3D ( 'NONE', #64026, #41066, #13375 ) ;
#95949 = CARTESIAN_POINT ( 'NONE',  ( 12.91533473730993009, 16.60535201082150891, -10.88017736071109987 ) ) ;
#95950 = EDGE_CURVE ( 'NONE', #76280, #18387, #22505, .T. ) ;
#95951 = CARTESIAN_POINT ( 'NONE',  ( 4.559911319644449179, 37.23035201082150536, -9.422509992056141925 ) ) ;
#95953 = CARTESIAN_POINT ( 'NONE',  ( 12.91533473730993009, 21.60535201082150536, -10.88017736071109987 ) ) ;
#95952 = DIRECTION ( 'NONE',  ( 1.000000000000000000, 0.000000000000000000, 0.000000000000000000 ) ) ;
#95954 = ORIENTED_EDGE ( 'NONE', *, *, #87719, .F. ) ;
#95955 = CARTESIAN_POINT ( 'NONE',  ( 20.32896413005680714, 10.57879003517447281, -5.963430220938276349 ) ) ;
#95956 = CARTESIAN_POINT ( 'NONE',  ( 7.084665262690076126, 19.10535201082150181, 10.88017736071109987 ) ) ;
#95957 = CARTESIAN_POINT ( 'NONE',  ( 4.630000001262032150, 0.09071174558778491437, 4.000000000000000000 ) ) ;
#95958 = DIRECTION ( 'NONE',  ( 0.000000000000000000, 0.000000000000000000, -1.000000000000000000 ) ) ;
#95959 = CARTESIAN_POINT ( 'NONE',  ( 6.565887622018943937, 63.08196800326376064, -12.81628187352647608 ) ) ;
#95960 = DIRECTION ( 'NONE',  ( -0.5547001962252290364, -0.8320502943378437211, 0.000000000000000000 ) ) ;
#95961 = CARTESIAN_POINT ( 'NONE',  ( 10.00000000000000178, 28.05374883491396787, 14.16423886937410082 ) ) ;
#95962 = CARTESIAN_POINT ( 'NONE',  ( 10.00000000000000178, 39.31368534415484106, 10.88017736071110342 ) ) ;
#95963 = CARTESIAN_POINT ( 'NONE',  ( 17.96484262340118221, 36.18868534415484106, -7.964842623401177768 ) ) ;
#95964 = DIRECTION ( 'NONE',  ( -0.1132032137679106348, 0.000000000000000000, 0.9935718556765871234 ) ) ;
#95965 = CARTESIAN_POINT ( 'NONE',  ( 19.72487221294571569, 60.71833443783937412, -6.499999999999990230 ) ) ;
#95966 = CARTESIAN_POINT ( 'NONE',  ( 5.076628168052704559, 45.17559781766745175, -8.527530157486179263 ) ) ;
#95967 = PLANE ( 'NONE',  #70237 ) ;
#95968 = CARTESIAN_POINT ( 'NONE',  ( 10.00000000000000178, 22.25893115100078745, 9.846743663894594434 ) ) ;
#95969 = CARTESIAN_POINT ( 'NONE',  ( 6.408140936763243367, -29.20969866340290721, 11.09922568453594494 ) ) ;
#95970 = CARTESIAN_POINT ( 'NONE',  ( 2.035157376598822676, 7.438685344154837509, -7.964842623401177768 ) ) ;
#95971 = CARTESIAN_POINT ( 'NONE',  ( 5.076628168052703671, 11.84226448433411960, 8.527530157486179263 ) ) ;
#95973 = CARTESIAN_POINT ( 'NONE',  ( -2.816281873526471635, 13.91530133659708746, -3.434112377981056508 ) ) ;
#95972 = STYLED_ITEM ( 'NONE', ( #13723 ), #33401 ) ;
#95974 = CARTESIAN_POINT ( 'NONE',  ( 20.88017736071110519, 55.56368534415484817, 2.639326808657452039E-16 ) ) ;
#95976 = CARTESIAN_POINT ( 'NONE',  ( 13.43411237798105340, 60.58196800326376064, 12.81628187352647963 ) ) ;
#95975 = CARTESIAN_POINT ( 'NONE',  ( 0.5774900079438590739, 22.64701867748817321, -5.440088680355550821 ) ) ;
#95977 = CARTESIAN_POINT ( 'NONE',  ( 22.26659068614894466, 33.88708216824730357, 7.082119434687054849 ) ) ;
#95978 = CARTESIAN_POINT ( 'NONE',  ( -14.61146088927472064, 2.507217523872729004E-16, -0.6660010753336522704 ) ) ;
#95979 = AXIS2_PLACEMENT_3D ( 'NONE', #72139, #33153, #24693 ) ;
#95980 = EDGE_CURVE ( 'NONE', #49746, #30157, #15009, .T. ) ;
#95981 = CARTESIAN_POINT ( 'NONE',  ( 8.375939845167682307, -0.03417435944610275333, 11.52849216984304448 ) ) ;
#95982 = ORIENTED_EDGE ( 'NONE', *, *, #46564, .F. ) ;
#95983 = CARTESIAN_POINT ( 'NONE',  ( 6.565887622018943937, 8.081968003263751754, -12.81628187352647608 ) ) ;
#95984 = CARTESIAN_POINT ( 'NONE',  ( 0.9940297508537879745, 15.00000000000000000, -14.21528771620249820 ) ) ;
#95985 = EDGE_CURVE ( 'NONE', #90632, #6306, #9961, .T. ) ;
#95986 = CARTESIAN_POINT ( 'NONE',  ( 7.084665262690076126, 39.10535201082150536, 10.88017736071109987 ) ) ;
#95987 = CIRCLE ( 'NONE', #89556, 15.00000000000000000 ) ;
#95988 = CARTESIAN_POINT ( 'NONE',  ( 7.361572987183169658, 59.96726448433410894, -9.846743663894592657 ) ) ;
#95989 = ORIENTED_EDGE ( 'NONE', *, *, #50459, .T. ) ;
#95990 = CARTESIAN_POINT ( 'NONE',  ( 2.791683348922240793, 21.63393115100078745, 7.208316651077764092 ) ) ;
#95991 = CARTESIAN_POINT ( 'NONE',  ( 17.20831665107776587, 22.88393115100078745, 7.208316651077764980 ) ) ;
#95992 = CARTESIAN_POINT ( 'NONE',  ( 0.1532563361054083140, 16.00893115100078390, 1.131784320476157264E-15 ) ) ;
#95993 = CARTESIAN_POINT ( 'NONE',  ( 2.791683348922240793, 6.633931151000785675, 7.208316651077764092 ) ) ;
#95995 = CARTESIAN_POINT ( 'NONE',  ( -45.94000000000000483, 92.50000000000000000, -9.500000000000000000 ) ) ;
#95994 = CARTESIAN_POINT ( 'NONE',  ( 7.361572987183169658, 4.967264484334119601, -9.846743663894592657 ) ) ;
#95996 = CARTESIAN_POINT ( 'NONE',  ( 1.472469842513823179, 1.425597817667451528, 4.923371831947296329 ) ) ;
#95998 = ORIENTED_EDGE ( 'NONE', *, *, #71933, .F. ) ;
#95997 = CARTESIAN_POINT ( 'NONE',  ( 1.472469842513823179, 16.42559781766745175, 4.923371831947296329 ) ) ;
#95999 = DIRECTION ( 'NONE',  ( 0.000000000000000000, 1.000000000000000000, -0.000000000000000000 ) ) ;
#96000 = CARTESIAN_POINT ( 'NONE',  ( 0.6178305044545818747, -1.501365330069579951, -9.382169495545419124 ) ) ;
#96001 = ORIENTED_EDGE ( 'NONE', *, *, #13059, .T. ) ;
#96002 = SURFACE_SIDE_STYLE ('',( #4514 ) ) ;
#96003 = EDGE_CURVE ( 'NONE', #77971, #56319, #82001, .T. ) ;
#96004 = CARTESIAN_POINT ( 'NONE',  ( 20.36894250292379382, 23.67874883491397142, 10.36894250292379205 ) ) ;
#96005 = DIRECTION ( 'NONE',  ( -0.000000000000000000, -1.000000000000000000, 0.000000000000000000 ) ) ;
#96006 = CARTESIAN_POINT ( 'NONE',  ( 20.36894250292379382, 18.67874883491397142, 10.36894250292379205 ) ) ;
#96007 = CARTESIAN_POINT ( 'NONE',  ( 24.16423886937409904, 34.09541550158064638, 3.795296366450317205 ) ) ;
#96008 = DIRECTION ( 'NONE',  ( -0.000000000000000000, 0.000000000000000000, 1.000000000000000000 ) ) ;
#96009 = CARTESIAN_POINT ( 'NONE',  ( 2.035157376598824452, 28.68868534415484106, 7.964842623401179544 ) ) ;
#96010 = DIRECTION ( 'NONE',  ( 1.000000000000000000, 0.000000000000000000, 0.000000000000000000 ) ) ;
#96011 = CARTESIAN_POINT ( 'NONE',  ( 10.00000000000000000, 19.75893115100078390, -9.846743663894594434 ) ) ;
#96013 = CARTESIAN_POINT ( 'NONE',  ( 7.361572987183170547, 32.05059781766745175, 9.846743663894590881 ) ) ;
#96012 = CARTESIAN_POINT ( 'NONE',  ( 19.42250999205614548, 60.98035201082151247, -5.440088680355545492 ) ) ;
#96014 = AXIS2_PLACEMENT_3D ( 'NONE', #33287, #24346, #86311 ) ;
#96015 = VECTOR ( 'NONE', #69334, 1000.000000000000000 ) ;
#96016 = CARTESIAN_POINT ( 'NONE',  ( 2.035157376598824452, 13.68868534415483751, 7.964842623401179544 ) ) ;
#96017 = CARTESIAN_POINT ( 'NONE',  ( 22.81628187352648496, 46.83196800326376064, -3.434112377981050290 ) ) ;
#96018 = CARTESIAN_POINT ( 'NONE',  ( 1.472469842513823179, 45.59226448433412315, -4.923371831947296329 ) ) ;
#96019 = FILL_AREA_STYLE_COLOUR ( '', #37826 ) ;
#96020 = CARTESIAN_POINT ( 'NONE',  ( 7.361572987183170547, 22.05059781766745530, 9.846743663894590881 ) ) ;
#96021 = CARTESIAN_POINT ( 'NONE',  ( 13.43411237798106583, 22.66530133659708923, -12.81628187352647252 ) ) ;
#96022 = CARTESIAN_POINT ( 'NONE',  ( -3.795296366450300773, -37.15458449841936783, 14.16423886937410437 ) ) ;
#96023 = CARTESIAN_POINT ( 'NONE',  ( 19.84674366389459621, 38.50893115100078745, 7.409399052514197653E-17 ) ) ;
#96024 = AXIS2_PLACEMENT_3D ( 'NONE', #91580, #76074, #7604 ) ;
#96025 = CARTESIAN_POINT ( 'NONE',  ( 13.79529636645031943, 15.34541550158063750, -14.16423886937409904 ) ) ;
#96026 = ORIENTED_EDGE ( 'NONE', *, *, #5462, .F. ) ;
#96027 = CARTESIAN_POINT ( 'NONE',  ( 2.035157376598822676, 47.43868534415484817, -7.964842623401177768 ) ) ;
#96028 = CARTESIAN_POINT ( 'NONE',  ( -0.8801773607111008646, 53.27201867748816966, 2.915334737309923430 ) ) ;
#96029 = CARTESIAN_POINT ( 'NONE',  ( -2.266590686148945544, 41.38708216824729647, -7.082119434687050408 ) ) ;
#96030 = CARTESIAN_POINT ( 'NONE',  ( 19.84674366389459266, 53.30059781766744464, 2.638427012816836559 ) ) ;
#96031 = CARTESIAN_POINT ( 'NONE',  ( 14.62617646268086524, 14.63595249122788999, 3.327906561566979615 ) ) ;
#96032 = CARTESIAN_POINT ( 'NONE',  ( 2.035157376598822676, 42.43868534415483396, -7.964842623401177768 ) ) ;
#96033 = FACE_OUTER_BOUND ( 'NONE', #94173, .T. ) ;
#96034 = CARTESIAN_POINT ( 'NONE',  ( -2.816281873526473856, 24.33196800326375353, 3.434112377981055619 ) ) ;
#96035 = CARTESIAN_POINT ( 'NONE',  ( 18.52753015748618282, 58.92559781766745886, -4.923371831947291888 ) ) ;
#96036 = CARTESIAN_POINT ( 'NONE',  ( -9.422509992056136596, 13.48035201082151069, 5.440088680355559703 ) ) ;
#96037 = CARTESIAN_POINT ( 'NONE',  ( 15.44008868035555793, 6.397018677488170546, -9.422509992056140149 ) ) ;
#96038 = CARTESIAN_POINT ( 'NONE',  ( 2.035157376598822676, 62.43868534415483396, -7.964842623401177768 ) ) ;
#96039 = AXIS2_PLACEMENT_3D ( 'NONE', #71179, #33156, #63650 ) ;
#96040 = EDGE_LOOP ( 'NONE', ( #7172, #77513, #28031, #79443 ) ) ;
#96041 = CARTESIAN_POINT ( 'NONE',  ( 0.5774900079438607392, 8.480352010821505360, 5.440088680355550821 ) ) ;
#96042 = DIRECTION ( 'NONE',  ( -0.000000000000000000, -1.000000000000000000, -0.000000000000000000 ) ) ;
#96043 = CARTESIAN_POINT ( 'NONE',  ( 10.00000000000000178, 64.31368534415483396, 10.88017736071110342 ) ) ;
#96044 = VECTOR ( 'NONE', #53306, 1000.000000000000000 ) ;
#96045 = CARTESIAN_POINT ( 'NONE',  ( 7.084665262690076126, 69.10535201082151957, 10.88017736071109987 ) ) ;
#96046 = CARTESIAN_POINT ( 'NONE',  ( 18.00000000000000000, 78.53751499213353782, -3.955843470927832950 ) ) ;
#96047 = CARTESIAN_POINT ( 'NONE',  ( 17.20831665107776587, 32.88393115100078745, 7.208316651077764980 ) ) ;
#96048 = CARTESIAN_POINT ( 'NONE',  ( 0.5774900079438607392, 28.48035201082150891, 5.440088680355550821 ) ) ;
#96049 = CARTESIAN_POINT ( 'NONE',  ( 0.6178305044545838731, 9.748634669930416052, 9.382169495545420901 ) ) ;
#96051 = CARTESIAN_POINT ( 'NONE',  ( -7.124966299160218952, -78.82422258446059971, -3.750000000000000000 ) ) ;
#96050 = CARTESIAN_POINT ( 'NONE',  ( 15.44008868035555260, 39.73035201082150536, 9.422509992056143702 ) ) ;
#96052 = DIRECTION ( 'NONE',  ( -0.000000000000000000, -1.000000000000000000, -0.000000000000000000 ) ) ;
#96053 = CARTESIAN_POINT ( 'NONE',  ( -1.099225684535947600, 39.54030133659708923, 6.408140936763237150 ) ) ;
#96054 = ORIENTED_EDGE ( 'NONE', *, *, #16788, .F. ) ;
#96055 = CARTESIAN_POINT ( 'NONE',  ( 0.5774900079438607392, 63.48035201082149825, 5.440088680355550821 ) ) ;
#96057 = CARTESIAN_POINT ( 'NONE',  ( 19.88701968852526036, 51.79427333184086990, 6.480634945678620973 ) ) ;
#96056 = CARTESIAN_POINT ( 'NONE',  ( -2.816281873526473856, 19.33196800326375708, 3.434112377981055619 ) ) ;
#96058 = CARTESIAN_POINT ( 'NONE',  ( 19.84674366389459266, 3.300597817667451750, 2.638427012816836559 ) ) ;
#96059 = CARTESIAN_POINT ( 'NONE',  ( 2.035157376598824452, 23.68868534415484461, 7.964842623401179544 ) ) ;
#96060 = CARTESIAN_POINT ( 'NONE',  ( 20.36894250292379738, 59.92874883491397497, -10.36894250292379027 ) ) ;
#96061 = CARTESIAN_POINT ( 'NONE',  ( 19.84674366389459266, 48.71726448433413026, -2.638427012816827677 ) ) ;
#96062 = CARTESIAN_POINT ( 'NONE',  ( 7.361572987183169658, 4.967264484334119601, -9.846743663894592657 ) ) ;
#96063 = CARTESIAN_POINT ( 'NONE',  ( 10.00000000000000178, 59.31368534415484106, 10.88017736071110342 ) ) ;
#96064 = B_SPLINE_CURVE_WITH_KNOTS ( 'NONE', 3,
 ( #78947, #1005, #8973, #17480 ),
 .UNSPECIFIED., .F., .F.,
 ( 4, 4 ),
 ( 0.000000000000000000, 0.001036303429213342089 ),
 .UNSPECIFIED. ) ;
#96065 = CARTESIAN_POINT ( 'NONE',  ( 0.2751277870542981341, 8.218334437839383000, 6.500000000000002665 ) ) ;
#96066 = CARTESIAN_POINT ( 'NONE',  ( 22.26659068614895176, 24.72041550158063572, -7.082119434687042414 ) ) ;
#96067 = MECHANICAL_DESIGN_GEOMETRIC_PRESENTATION_REPRESENTATION (  '', ( #9849 ), #6621 ) ;
#96068 = EDGE_CURVE ( 'NONE', #81670, #93612, #10802, .T. ) ;
#96069 = DIRECTION ( 'NONE',  ( -0.9999619230641711987, 0.000000000000000000, -0.008726535498381204903 ) ) ;
#96070 =( NAMED_UNIT ( * ) PLANE_ANGLE_UNIT ( ) SI_UNIT ( $, .RADIAN. ) );
#96071 = EDGE_LOOP ( 'NONE', ( #43028, #55189, #74310, #92518, #13822, #81471 ) ) ;
#96072 = ORIENTED_EDGE ( 'NONE', *, *, #9639, .T. ) ;
#96073 = CARTESIAN_POINT ( 'NONE',  ( -0.3689425029237881626, 67.42874883491396076, 10.36894250292379027 ) ) ;
#96074 = CARTESIAN_POINT ( 'NONE',  ( 24.16423886937410614, 44.30374883491397497, 8.672049930838204340E-16 ) ) ;
#96075 = CARTESIAN_POINT ( 'NONE',  ( 14.92337183194729988, 24.34226448433411960, -8.527530157486177487 ) ) ;
#96076 = CARTESIAN_POINT ( 'NONE',  ( 22.81628187352647785, 26.62363466993042138, 6.195893100308588602E-16 ) ) ;
#96077 = DIRECTION ( 'NONE',  ( 0.000000000000000000, 0.000000000000000000, 1.000000000000000000 ) ) ;
#96078 = FACE_OUTER_BOUND ( 'NONE', #7531, .T. ) ;
#96079 = LINE ( 'NONE', #11581, #61144 ) ;
#96080 = CARTESIAN_POINT ( 'NONE',  ( 10.00000000000000000, 45.55374883491397497, -14.16423886937410082 ) ) ;
#96081 = LINE ( 'NONE', #81065, #22111 ) ;
#96082 = CARTESIAN_POINT ( 'NONE',  ( 2.791683348922237240, 15.38393115100078212, -7.208316651077763204 ) ) ;
#96083 = CARTESIAN_POINT ( 'NONE',  ( 18.28836319691943757, 59.34492782695770074, 6.500000000000035527 ) ) ;
#96084 = CARTESIAN_POINT ( 'NONE',  ( 4.923371831947295441, 4.342264484334126706, -8.527530157486179263 ) ) ;
#96085 = ORIENTED_EDGE ( 'NONE', *, *, #19153, .F. ) ;
#96086 = CARTESIAN_POINT ( 'NONE',  ( 14.17193700899790265, -0.03417435944610275333, -1.489530601564018175 ) ) ;
#96087 = ORIENTED_EDGE ( 'NONE', *, *, #76771, .F. ) ;
#96088 = EDGE_LOOP ( 'NONE', ( #8871, #55007, #72074, #51079 ) ) ;
#96089 = CARTESIAN_POINT ( 'NONE',  ( 13.79529636645030344, 13.26208216824729824, 14.16423886937410614 ) ) ;
#96091 = CARTESIAN_POINT ( 'NONE',  ( -0.8801773607110991993, 22.85535201082150181, -2.915334737309923874 ) ) ;
#96090 = CARTESIAN_POINT ( 'NONE',  ( -0.8801773607110991993, 17.85535201082150536, -2.915334737309923874 ) ) ;
#96093 = CARTESIAN_POINT ( 'NONE',  ( -2.816281873526473856, 24.12363466993042138, 9.499525473075851096E-16 ) ) ;
#96092 = CARTESIAN_POINT ( 'NONE',  ( 17.20831665107776587, 47.88393115100078745, 7.208316651077764980 ) ) ;
#96094 = SURFACE_STYLE_USAGE ( .BOTH. , #65568 ) ;
#96095 = CARTESIAN_POINT ( 'NONE',  ( 18.04007052943771683, 43.01528370094807485, 5.767676674365856293 ) ) ;
#96096 = AXIS2_PLACEMENT_3D ( 'NONE', #55335, #56806, #54830 ) ;
#96097 = EDGE_CURVE ( 'NONE', #96723, #18240, #94887, .T. ) ;
#96098 = CARTESIAN_POINT ( 'NONE',  ( 3.591859063236761518, 24.95696800326375353, 11.09922568453594849 ) ) ;
#96099 = ORIENTED_EDGE ( 'NONE', *, *, #22498, .T. ) ;
#96100 = CARTESIAN_POINT ( 'NONE',  ( 2.791683348922240793, 36.63393115100078035, 7.208316651077764092 ) ) ;
#96101 = CARTESIAN_POINT ( 'NONE',  ( -4.164238869374098151, 61.59541550158063217, -3.795296366450310543 ) ) ;
#96102 = VERTEX_POINT ( 'NONE', #86446 ) ;
#96103 = CARTESIAN_POINT ( 'NONE',  ( 13.79529636645031943, 65.34541550158063217, -14.16423886937409904 ) ) ;
#96104 = VERTEX_POINT ( 'NONE', #1977 ) ;
#96105 = CARTESIAN_POINT ( 'NONE',  ( 7.084665262690076126, 52.02201867748816255, -10.88017736071110164 ) ) ;
#96106 = CARTESIAN_POINT ( 'NONE',  ( 0.5774900079438607392, 43.48035201082151247, 5.440088680355550821 ) ) ;
#96107 = CARTESIAN_POINT ( 'NONE',  ( 4.559911319644449179, 47.23035201082150536, -9.422509992056141925 ) ) ;
#96108 = CYLINDRICAL_SURFACE ( 'NONE', #40990, 10.00000000000000178 ) ;
#96109 = CARTESIAN_POINT ( 'NONE',  ( -0.8801773607111008646, 43.27201867748817676, 2.915334737309923430 ) ) ;
#96110 = DIRECTION ( 'NONE',  ( 0.000000000000000000, 1.000000000000000000, 0.000000000000000000 ) ) ;
#96111 = CARTESIAN_POINT ( 'NONE',  ( 3.591859063236761518, 29.95696800326375708, 11.09922568453594849 ) ) ;
#96114 = ORIENTED_EDGE ( 'NONE', *, *, #95637, .F. ) ;
#96113 = AXIS2_PLACEMENT_3D ( 'NONE', #24104, #45609, #1117 ) ;
#96112 = DIRECTION ( 'NONE',  ( 0.000000000000000000, 1.000000000000000000, 0.000000000000000000 ) ) ;
#96115 = CARTESIAN_POINT ( 'NONE',  ( 17.20831665107776587, 29.13393115100078390, -7.208316651077762316 ) ) ;
#96116 = ORIENTED_EDGE ( 'NONE', *, *, #27402, .T. ) ;
#96117 = CARTESIAN_POINT ( 'NONE',  ( 2.791683348922237240, 60.38393115100078745, -7.208316651077763204 ) ) ;
#96118 = FACE_OUTER_BOUND ( 'NONE', #66153, .T. ) ;
#96119 =( GEOMETRIC_REPRESENTATION_CONTEXT ( 3 ) GLOBAL_UNCERTAINTY_ASSIGNED_CONTEXT ( ( #71344 ) ) GLOBAL_UNIT_ASSIGNED_CONTEXT ( ( #38409, #33337, #40868 ) ) REPRESENTATION_CONTEXT ( 'NONE', 'WORKASPACE' ) );
#96120 = B_SPLINE_CURVE_WITH_KNOTS ( 'NONE', 3,
 ( #49265, #51234, #26755, #58219, #11757, #57250 ),
 .UNSPECIFIED., .F., .F.,
 ( 4, 2, 4 ),
 ( 0.0002800020636817301435, 0.0006862073132860486719, 0.001092412562890367200 ),
 .UNSPECIFIED. ) ;
#96121 = CARTESIAN_POINT ( 'NONE',  ( -5.812563760649267941, -35.09659463721938977, 3.750000000000000444 ) ) ;
#96122 = ORIENTED_EDGE ( 'NONE', *, *, #83073, .T. ) ;
#96123 = ADVANCED_FACE ( 'NONE', ( #40950 ), #91969, .F. ) ;
#96124 = CARTESIAN_POINT ( 'NONE',  ( 32.06412365047463453, 26.99999999999997868, 9.500000000000000000 ) ) ;
#96126 = CARTESIAN_POINT ( 'NONE',  ( 17.20831665107776587, 37.88393115100078745, 7.208316651077764980 ) ) ;
#96125 = CARTESIAN_POINT ( 'NONE',  ( 7.361572987183170547, 67.05059781766746596, 9.846743663894590881 ) ) ;
#96127 = CARTESIAN_POINT ( 'NONE',  ( -4.164238869374099927, 57.01208216824731068, 3.795296366450308767 ) ) ;
#96128 = DIRECTION ( 'NONE',  ( -1.000000000000000000, -0.000000000000000000, -0.000000000000000000 ) ) ;
#96129 = EDGE_LOOP ( 'NONE', ( #84285, #84657, #28801, #50201 ) ) ;
#96130 = LINE ( 'NONE', #26149, #91082 ) ;
#96131 = CARTESIAN_POINT ( 'NONE',  ( 12.63842701281683922, 34.55059781766745886, -9.846743663894590881 ) ) ;
#96132 = CARTESIAN_POINT ( 'NONE',  ( 10.00000000000000000, 62.87363466993042493, -12.81628187352647608 ) ) ;
#96133 = CARTESIAN_POINT ( 'NONE',  ( 0.6178305044545838731, 4.748634669930420493, 9.382169495545420901 ) ) ;
#96135 = EDGE_CURVE ( 'NONE', #86711, #21427, #92453, .T. ) ;
#96134 = CARTESIAN_POINT ( 'NONE',  ( 14.92337183194729988, 4.342264484334117824, -8.527530157486177487 ) ) ;
#96136 = CARTESIAN_POINT ( 'NONE',  ( 1.472469842513823179, 5.592264484334118713, -4.923371831947296329 ) ) ;
#96137 = CARTESIAN_POINT ( 'NONE',  ( 19.84674366389459621, 53.50893115100078745, 7.409399052514197653E-17 ) ) ;
#96138 = CARTESIAN_POINT ( 'NONE',  ( 19.42250999205614548, 20.98035201082150891, -5.440088680355545492 ) ) ;
#96139 = ORIENTED_EDGE ( 'NONE', *, *, #57620, .T. ) ;
#96140 = CARTESIAN_POINT ( 'NONE',  ( 15.44008868035555260, 14.73035201082150536, 9.422509992056143702 ) ) ;
#96141 = CARTESIAN_POINT ( 'NONE',  ( 6.204703633549690345, 0.7620821682473009062, -14.16423886937410259 ) ) ;
#96142 = CARTESIAN_POINT ( 'NONE',  ( 19.84674366389459266, 8.717264484334116048, -2.638427012816827677 ) ) ;
#96143 = CARTESIAN_POINT ( 'NONE',  ( 17.96484262340118221, 59.93868534415484106, 7.964842623401181321 ) ) ;
#96145 = CARTESIAN_POINT ( 'NONE',  ( 11.33568117652998986, 12.60026003655735849, -0.6654292126732216373 ) ) ;
#96144 = CARTESIAN_POINT ( 'NONE',  ( 22.81628187352647785, 21.62363466993041783, 6.195893100308588602E-16 ) ) ;
#96146 = PLANE ( 'NONE',  #37628 ) ;
#96147 = B_SPLINE_CURVE_WITH_KNOTS ( 'NONE', 3,
 ( #89293, #79330, #80807, #95818, #10840, #73296 ),
 .UNSPECIFIED., .F., .F.,
 ( 4, 2, 4 ),
 ( 0.000000000000000000, 0.0002565770811490924574, 0.0005131541622981849148 ),
 .UNSPECIFIED. ) ;
#96148 = CARTESIAN_POINT ( 'NONE',  ( -1.926860441876562247, 57.45379003517447813, -3.195792623639530650 ) ) ;
#96149 = CARTESIAN_POINT ( 'NONE',  ( 18.72515096720578853, 60.05509018479938277, 6.499999999999877431 ) ) ;
#96150 = CARTESIAN_POINT ( 'NONE',  ( 1.472469842513823179, 66.42559781766745175, 4.923371831947296329 ) ) ;
#96151 = CARTESIAN_POINT ( 'NONE',  ( 0.1532563361054082862, 11.21726448433411605, 2.638427012816831674 ) ) ;
#96152 = CARTESIAN_POINT ( 'NONE',  ( 9.422509992056141925, -29.85298132251182324, 5.440088680355547268 ) ) ;
#96153 = CARTESIAN_POINT ( 'NONE',  ( -2.816281873526471635, 23.91530133659708568, -3.434112377981056508 ) ) ;
#96154 = PLANE ( 'NONE',  #35654 ) ;
#96155 = CARTESIAN_POINT ( 'NONE',  ( 20.88017736071110519, 30.56368534415484106, 2.639326808657452039E-16 ) ) ;
#96156 = CYLINDRICAL_SURFACE ( 'NONE', #62741, 2.000000000000001776 ) ;
#96157 = CARTESIAN_POINT ( 'NONE',  ( 10.00000000000000000, 45.55374883491397497, -14.16423886937410082 ) ) ;
#96158 = SURFACE_STYLE_FILL_AREA ( #73630 ) ;
#96159 = CARTESIAN_POINT ( 'NONE',  ( 10.00000000000000178, 45.37363466993041783, 12.81628187352647608 ) ) ;
#96160 = CARTESIAN_POINT ( 'NONE',  ( -0.8801773607111008646, 33.27201867748817676, 2.915334737309923430 ) ) ;
#96161 = CIRCLE ( 'NONE', #70612, 15.00000000000000000 ) ;
#96162 = CARTESIAN_POINT ( 'NONE',  ( 1.472469842513823179, 56.42559781766745886, 4.923371831947296329 ) ) ;
#96163 = CARTESIAN_POINT ( 'NONE',  ( 15.44008868035555260, 59.73035201082151247, 9.422509992056143702 ) ) ;
#96164 = CARTESIAN_POINT ( 'NONE',  ( -0.3689425029237898834, 31.17874883491396787, -10.36894250292378850 ) ) ;
#96165 = DIRECTION ( 'NONE',  ( -0.5807029557109515405, -0.000000000000000000, 0.8141155183563107967 ) ) ;
#96166 = CARTESIAN_POINT ( 'NONE',  ( 14.92337183194729633, 32.67559781766745175, 8.527530157486181039 ) ) ;
#96167 = CARTESIAN_POINT ( 'NONE',  ( 10.00000000000000178, 60.37363466993041783, 12.81628187352647608 ) ) ;
#96168 = CARTESIAN_POINT ( 'NONE',  ( 3.591859063236761518, -0.04303199673624671928, 11.09922568453594849 ) ) ;
#96169 = ORIENTED_EDGE ( 'NONE', *, *, #42353, .T. ) ;
#96170 = CARTESIAN_POINT ( 'NONE',  ( 15.44008868035555793, 21.39701867748817321, -9.422509992056140149 ) ) ;
#96171 = CARTESIAN_POINT ( 'NONE',  ( 18.00000000000000000, 91.21610151837452918, -8.000000000000000000 ) ) ;
#96172 = CARTESIAN_POINT ( 'NONE',  ( 6.452519493965914954, -47.68837976023561964, 2.750000000000000000 ) ) ;
#96173 = CARTESIAN_POINT ( 'NONE',  ( 20.88017736071110164, 20.35535201082150891, 2.915334737309930979 ) ) ;
#96174 = CARTESIAN_POINT ( 'NONE',  ( -0.3689425029237881626, 27.42874883491397142, 10.36894250292379027 ) ) ;
#96175 = CARTESIAN_POINT ( 'NONE',  ( 12.63842701281683034, 12.46726448433411782, 9.846743663894596210 ) ) ;
#96176 = CARTESIAN_POINT ( 'NONE',  ( 19.84674366389459266, 58.71726448433411605, -2.638427012816827677 ) ) ;
#96177 = CARTESIAN_POINT ( 'NONE',  ( 7.084665262690076126, 27.02201867748817676, -10.88017736071110164 ) ) ;
#96178 = DIRECTION ( 'NONE',  ( 0.000000000000000000, 0.000000000000000000, -1.000000000000000000 ) ) ;
#96179 = CARTESIAN_POINT ( 'NONE',  ( -3.468686501387143295, 0.000000000000000000, -4.207853202970329498 ) ) ;
#96180 = ADVANCED_FACE ( 'NONE', ( #31451 ), #89960, .T. ) ;
#96181 = ORIENTED_EDGE ( 'NONE', *, *, #43235, .T. ) ;
#96182 = CIRCLE ( 'NONE', #53057, 14.49999999999999822 ) ;
#96183 = LINE ( 'NONE', #27666, #65851 ) ;
#96184 = CARTESIAN_POINT ( 'NONE',  ( 0.1532563361054100626, 50.80059781766745175, -2.638427012816831230 ) ) ;
#96185 = VERTEX_POINT ( 'NONE', #10443 ) ;
#96186 = ORIENTED_EDGE ( 'NONE', *, *, #97896, .T. ) ;
#96187 = LINE ( 'NONE', #40721, #24606 ) ;
#96188 = CARTESIAN_POINT ( 'NONE',  ( 2.917880565312948704, 12.63708216824730179, 12.26659068614894643 ) ) ;
#96189 = CARTESIAN_POINT ( 'NONE',  ( 13.79529636645030344, 8.262082168247300018, 14.16423886937410614 ) ) ;
#96190 = CARTESIAN_POINT ( 'NONE',  ( 12.91533473730993009, 51.60535201082149825, -10.88017736071109987 ) ) ;
#96191 = CARTESIAN_POINT ( 'NONE',  ( -4.164238869374099039, 56.80374883491397497, 8.674139862899312516E-16 ) ) ;
#96192 = CARTESIAN_POINT ( 'NONE',  ( 7.361572987183170547, 32.05059781766745175, 9.846743663894590881 ) ) ;
#96193 = CARTESIAN_POINT ( 'NONE',  ( -11.02874191836853512, -96.54482102863701698, 3.750000000000000000 ) ) ;
#96195 = CARTESIAN_POINT ( 'NONE',  ( 6.565887622018943937, 8.081968003263751754, -12.81628187352647608 ) ) ;
#96194 = CARTESIAN_POINT ( 'NONE',  ( 2.035157376598824452, 33.68868534415484106, 7.964842623401179544 ) ) ;
#96196 = SURFACE_STYLE_USAGE ( .BOTH. , #33692 ) ;
#96197 = EDGE_CURVE ( 'NONE', #79151, #47550, #77445, .T. ) ;
#96198 = CARTESIAN_POINT ( 'NONE',  ( -2.266590686148945544, 52.22041550158064638, 7.082119434687048631 ) ) ;
#96199 = VECTOR ( 'NONE', #71277, 1000.000000000000114 ) ;
#96200 = CARTESIAN_POINT ( 'NONE',  ( 10.00000000000000178, 24.31368534415484106, 10.88017736071110342 ) ) ;
#96201 = DIRECTION ( 'NONE',  ( 0.000000000000000000, 0.000000000000000000, -1.000000000000000000 ) ) ;
#96202 = LINE ( 'NONE', #27685, #2862 ) ;
#96203 = MECHANICAL_DESIGN_GEOMETRIC_PRESENTATION_REPRESENTATION (  '', ( #56237 ), #81755 ) ;
#96204 = CARTESIAN_POINT ( 'NONE',  ( 2.638427012816835227, -32.53273551566588395, 9.846743663894590881 ) ) ;
#96205 = ORIENTED_EDGE ( 'NONE', *, *, #59826, .T. ) ;
#96206 = CARTESIAN_POINT ( 'NONE',  ( 10.83696084481538691, -98.17058944465519232, 3.750000000000000000 ) ) ;
#96207 = CIRCLE ( 'NONE', #97802, 11.15000000000026326 ) ;
#96208 = ORIENTED_EDGE ( 'NONE', *, *, #53411, .F. ) ;
#96209 = ORIENTED_EDGE ( 'NONE', *, *, #3440, .T. ) ;
#96210 = CARTESIAN_POINT ( 'NONE',  ( -0.3689425029237881626, 52.42874883491396076, 10.36894250292379027 ) ) ;
#96211 = CARTESIAN_POINT ( 'NONE',  ( 19.84674366389459621, 43.50893115100078745, 7.409399052514197653E-17 ) ) ;
#96212 = CARTESIAN_POINT ( 'NONE',  ( 15.44008868035555260, 59.73035201082151247, 9.422509992056143702 ) ) ;
#96213 = CARTESIAN_POINT ( 'NONE',  ( 14.71525861348295727, 14.49999999999999112, -2.908807992686619048 ) ) ;
#96214 = AXIS2_PLACEMENT_3D ( 'NONE', #80678, #72183, #65166 ) ;
#96215 = CARTESIAN_POINT ( 'NONE',  ( 20.88017736071110164, 50.35535201082151247, 2.915334737309930979 ) ) ;
#96216 = ADVANCED_FACE ( 'NONE', ( #24476 ), #82935, .T. ) ;
#96217 = CARTESIAN_POINT ( 'NONE',  ( 21.09922568453595559, 57.04030133659708923, -6.408140936763230044 ) ) ;
#96218 = CARTESIAN_POINT ( 'NONE',  ( -11.09922568453595382, 3.706968003263755307, -6.408140936763226492 ) ) ;
#96219 = VERTEX_POINT ( 'NONE', #86925 ) ;
#96220 = CARTESIAN_POINT ( 'NONE',  ( 12.91533473730992121, 49.52201867748817676, 10.88017736071110164 ) ) ;
#96221 = CARTESIAN_POINT ( 'NONE',  ( -4.164238869374099927, 17.01208216824730357, 3.795296366450308767 ) ) ;
#96222 = EDGE_CURVE ( 'NONE', #7152, #55464, #4914, .T. ) ;
#96223 = CARTESIAN_POINT ( 'NONE',  ( -2.816281873526473856, 19.12363466993042138, 9.499525473075851096E-16 ) ) ;
#96224 = EDGE_LOOP ( 'NONE', ( #31760, #55938, #4399, #12959, #68917 ) ) ;
#96225 = VECTOR ( 'NONE', #14467, 1000.000000000000000 ) ;
#96226 = CARTESIAN_POINT ( 'NONE',  ( 0.6178305044545838731, 44.74863466993042493, 9.382169495545420901 ) ) ;
#96227 = CARTESIAN_POINT ( 'NONE',  ( 15.44008868035555793, 21.39701867748817321, -9.422509992056140149 ) ) ;
#96228 = CARTESIAN_POINT ( 'NONE',  ( 10.00000000000000178, 42.25893115100078745, 9.846743663894594434 ) ) ;
#96229 = CARTESIAN_POINT ( 'NONE',  ( 12.91533473730992121, 9.522018677488171434, 10.88017736071110164 ) ) ;
#96230 = CARTESIAN_POINT ( 'NONE',  ( 3.591859063236763294, 48.29030133659708923, -11.09922568453595026 ) ) ;
#96231 = CARTESIAN_POINT ( 'NONE',  ( 26.00000000000000355, 35.99999999999997158, -10.00000000000000000 ) ) ;
#96232 = CARTESIAN_POINT ( 'NONE',  ( 19.84674366389459266, 48.30059781766745175, 2.638427012816836559 ) ) ;
#96234 = VERTEX_POINT ( 'NONE', #72897 ) ;
#96233 = CARTESIAN_POINT ( 'NONE',  ( -0.8801773607111009756, 68.06368534415484817, 1.068504757029289695E-15 ) ) ;
#96235 = AXIS2_PLACEMENT_3D ( 'NONE', #32381, #93383, #17410 ) ;
#96236 = LINE ( 'NONE', #71751, #19522 ) ;
#96237 = CARTESIAN_POINT ( 'NONE',  ( 20.15039907845753930, 69.92552686551195507, 6.262539305110068177 ) ) ;
#96238 = CARTESIAN_POINT ( 'NONE',  ( 0.000000000000000000, 14.49999999999999822, 0.000000000000000000 ) ) ;
#96239 = CARTESIAN_POINT ( 'NONE',  ( 10.00000000000000178, 12.25893115100078568, 9.846743663894594434 ) ) ;
#96240 = CARTESIAN_POINT ( 'NONE',  ( 19.38216949554541202, 20.99863466993042138, 9.382169495545424454 ) ) ;
#96241 = LINE ( 'NONE', #5243, #6824 ) ;
#96242 = ORIENTED_EDGE ( 'NONE', *, *, #49412, .T. ) ;
#96243 = CARTESIAN_POINT ( 'NONE',  ( 12.63842701281683034, 52.46726448433413026, 9.846743663894596210 ) ) ;
#96244 = CARTESIAN_POINT ( 'NONE',  ( -13.16740645155962852, 0.04922511925147048800, -6.653232860246741431 ) ) ;
#96245 = CARTESIAN_POINT ( 'NONE',  ( 17.08211943468705840, 20.13708216824730357, -12.26659068614894466 ) ) ;
#96246 = CARTESIAN_POINT ( 'NONE',  ( 17.20831665107776587, 27.88393115100078390, 7.208316651077764980 ) ) ;
#96247 = CARTESIAN_POINT ( 'NONE',  ( 22.81628187352647785, 41.41530133659708923, 3.434112377981063169 ) ) ;
#96249 = CARTESIAN_POINT ( 'NONE',  ( 8.839000071697000749, 0.04962890530003118833, 11.81225584161647113 ) ) ;
#96248 = CYLINDRICAL_SURFACE ( 'NONE', #59178, 2.000000000000000000 ) ;
#96250 = CARTESIAN_POINT ( 'NONE',  ( -0.8801773607111009756, 58.06368534415484106, 1.068504757029289695E-15 ) ) ;
#96251 = CARTESIAN_POINT ( 'NONE',  ( 0.6178305044545838731, 14.74863466993041783, 9.382169495545420901 ) ) ;
#96252 = DIRECTION ( 'NONE',  ( -0.000000000000000000, -1.000000000000000000, -0.000000000000000000 ) ) ;
#96253 = CARTESIAN_POINT ( 'NONE',  ( 19.84674366389459621, 28.50893115100078745, 7.409399052514197653E-17 ) ) ;
#96255 = EDGE_CURVE ( 'NONE', #40043, #6847, #81388, .T. ) ;
#96254 = CARTESIAN_POINT ( 'NONE',  ( 2.035157376598822676, 37.43868534415484106, -7.964842623401177768 ) ) ;
#96256 = CARTESIAN_POINT ( 'NONE',  ( 13.43411237798105340, 40.58196800326375353, 12.81628187352647963 ) ) ;
#96257 = AXIS2_PLACEMENT_3D ( 'NONE', #13606, #81110, #75090 ) ;
#96258 = CARTESIAN_POINT ( 'NONE',  ( 7.361572987183170547, 37.05059781766744464, 9.846743663894590881 ) ) ;
#96259 = CARTESIAN_POINT ( 'NONE',  ( -12.29167862326001348, 90.46743899975659531, 7.079701151216531763 ) ) ;
#96260 = CARTESIAN_POINT ( 'NONE',  ( -0.8801773607111009756, 38.06368534415484106, 1.068504757029289695E-15 ) ) ;
#96261 = AXIS2_PLACEMENT_3D ( 'NONE', #5630, #59596, #98629 ) ;
#96262 = AXIS2_PLACEMENT_3D ( 'NONE', #71756, #3266, #18767 ) ;
#96263 = ORIENTED_EDGE ( 'NONE', *, *, #79818, .T. ) ;
#96264 = VECTOR ( 'NONE', #31426, 1000.000000000000000 ) ;
#96265 = DIRECTION ( 'NONE',  ( -1.000000000000000000, 0.000000000000000000, 0.000000000000000000 ) ) ;
#96266 = CARTESIAN_POINT ( 'NONE',  ( 20.88017736071110519, 5.563685344154837509, 2.639326808657452039E-16 ) ) ;
#96268 = CARTESIAN_POINT ( 'NONE',  ( 20.88017736071110164, 35.35535201082150536, 2.915334737309930979 ) ) ;
#96267 = CARTESIAN_POINT ( 'NONE',  ( 17.20831665107776587, 57.88393115100078745, 7.208316651077764980 ) ) ;
#96269 = CARTESIAN_POINT ( 'NONE',  ( 5.795997163830165277, 15.00000000000000000, -13.01802277140705932 ) ) ;
#96270 = STYLED_ITEM ( 'NONE', ( #64342 ), #92159 ) ;
#96271 = CARTESIAN_POINT ( 'NONE',  ( -0.8801773607111008646, 63.27201867748817676, 2.915334737309923430 ) ) ;
#96272 = CARTESIAN_POINT ( 'NONE',  ( 12.91533473730993009, 21.60535201082150536, -10.88017736071109987 ) ) ;
#96273 = CARTESIAN_POINT ( 'NONE',  ( 1.472469842513823179, 21.42559781766745175, 4.923371831947296329 ) ) ;
#96274 = CARTESIAN_POINT ( 'NONE',  ( 2.962741594153077251, -0.03417435944610275333, -13.93860331045673107 ) ) ;
#96275 = VECTOR ( 'NONE', #74240, 1000.000000000000000 ) ;
#96276 = CARTESIAN_POINT ( 'NONE',  ( 2.791683348922237240, 50.38393115100078035, -7.208316651077763204 ) ) ;
#96277 = CARTESIAN_POINT ( 'NONE',  ( 2.917880565312948704, 47.63708216824730357, 12.26659068614894643 ) ) ;
#96278 = CARTESIAN_POINT ( 'NONE',  ( 10.00000000000000178, 3.053748834913967425, 14.16423886937410082 ) ) ;
#96279 = CARTESIAN_POINT ( 'NONE',  ( -2.266590686148945544, 32.22041550158063927, 7.082119434687048631 ) ) ;
#96280 = CARTESIAN_POINT ( 'NONE',  ( 6.565887622018943937, 3.081968003263753531, -12.81628187352647608 ) ) ;
#96281 = CARTESIAN_POINT ( 'NONE',  ( 11.59580422753452922, 14.76984949557379245, 9.421229451859275628 ) ) ;
#96282 = CARTESIAN_POINT ( 'NONE',  ( 17.96484262340118221, 9.938685344154839285, 7.964842623401181321 ) ) ;
#96283 = CARTESIAN_POINT ( 'NONE',  ( 10.00000000000000000, 39.75893115100078745, -9.846743663894594434 ) ) ;
#96285 = CARTESIAN_POINT ( 'NONE',  ( -10.89045396206015504, 89.68015320059716089, -6.284968870999087187 ) ) ;
#96284 = PRESENTATION_STYLE_ASSIGNMENT (( #89745 ) ) ;
#96286 = CARTESIAN_POINT ( 'NONE',  ( -0.8801773607111009756, 58.06368534415484106, 1.068504757029289695E-15 ) ) ;
#96287 = FACE_OUTER_BOUND ( 'NONE', #63718, .T. ) ;
#96288 = UNCERTAINTY_MEASURE_WITH_UNIT (LENGTH_MEASURE( 1.000000000000000082E-05 ), #43868, 'distance_accuracy_value', 'NONE');
#96289 = ADVANCED_FACE ( 'NONE', ( #50395 ), #3760, .T. ) ;
#96290 = CARTESIAN_POINT ( 'NONE',  ( 6.565887622018943937, 65.16530133659709634, 12.81628187352647430 ) ) ;
#96291 = CARTESIAN_POINT ( 'NONE',  ( -2.816281873526473856, 24.33196800326375353, 3.434112377981055619 ) ) ;
#96292 = CARTESIAN_POINT ( 'NONE',  ( 19.84674366389459266, 33.71726448433410894, -2.638427012816827677 ) ) ;
#96293 = ORIENTED_EDGE ( 'NONE', *, *, #31738, .F. ) ;
#96294 = LINE ( 'NONE', #12281, #77391 ) ;
#96295 = LINE ( 'NONE', #57774, #76388 ) ;
#96296 = CARTESIAN_POINT ( 'NONE',  ( 20.88017736071110875, 5.772018677488170546, -2.915334737309920765 ) ) ;
#96297 = CARTESIAN_POINT ( 'NONE',  ( -0.8801773607111008646, 8.272018677488171434, 2.915334737309923430 ) ) ;
#96298 = VECTOR ( 'NONE', #71846, 1000.000000000000000 ) ;
#96299 = CARTESIAN_POINT ( 'NONE',  ( 13.79529636645031943, 40.34541550158063217, -14.16423886937409904 ) ) ;
#96300 = CARTESIAN_POINT ( 'NONE',  ( 7.084665262690076126, 37.02201867748817676, -10.88017736071110164 ) ) ;
#96301 = CARTESIAN_POINT ( 'NONE',  ( 4.559911319644449179, 57.23035201082150536, -9.422509992056141925 ) ) ;
#96302 = CARTESIAN_POINT ( 'NONE',  ( -13.55101055326594839, 14.76984994142488361, 6.292244619294627306 ) ) ;
#96303 = DIRECTION ( 'NONE',  ( -1.000000000000000000, 0.000000000000000000, 0.000000000000000000 ) ) ;
#96304 = CARTESIAN_POINT ( 'NONE',  ( 19.84674366389459266, 18.30059781766745175, 2.638427012816836559 ) ) ;
#96305 = CARTESIAN_POINT ( 'NONE',  ( 1.472469842513823179, 0.5922644843341181575, -4.923371831947296329 ) ) ;
#96306 = DIRECTION ( 'NONE',  ( 0.000000000000000000, 1.000000000000000000, 0.000000000000000000 ) ) ;
#96307 = CARTESIAN_POINT ( 'NONE',  ( 14.92337183194729633, 37.67559781766745175, 8.527530157486181039 ) ) ;
#96308 = CARTESIAN_POINT ( 'NONE',  ( 0.6178305044545838731, -0.2513653300695798953, 9.382169495545420901 ) ) ;
#96309 = AXIS2_PLACEMENT_3D ( 'NONE', #79167, #41196, #40193 ) ;
#96310 = CARTESIAN_POINT ( 'NONE',  ( 7.084665262690076126, 39.10535201082150536, 10.88017736071109987 ) ) ;
#96311 = EDGE_CURVE ( 'NONE', #83450, #53280, #89805, .T. ) ;
#96312 = UNCERTAINTY_MEASURE_WITH_UNIT (LENGTH_MEASURE( 1.000000000000000082E-05 ), #47990, 'distance_accuracy_value', 'NONE');
#96313 = ORIENTED_EDGE ( 'NONE', *, *, #42600, .T. ) ;
#96314 = CARTESIAN_POINT ( 'NONE',  ( -1.099225684535947600, 43.70696800326375353, -6.408140936763238038 ) ) ;
#96315 = CARTESIAN_POINT ( 'NONE',  ( 1.983216688680843109, -0.03417435944610275333, 14.11131997956739070 ) ) ;
#96316 = CARTESIAN_POINT ( 'NONE',  ( 10.00000000000000000, 61.81368534415484106, -10.88017736071110342 ) ) ;
#96317 = CARTESIAN_POINT ( 'NONE',  ( -2.816281873526473856, 49.33196800326374643, 3.434112377981055619 ) ) ;
#96319 = CARTESIAN_POINT ( 'NONE',  ( 14.92337183194729988, 34.34226448433411605, -8.527530157486177487 ) ) ;
#96318 = CARTESIAN_POINT ( 'NONE',  ( 20.36894250292379738, 54.92874883491396076, -10.36894250292379027 ) ) ;
#96320 = CARTESIAN_POINT ( 'NONE',  ( 0.000000000000000000, 14.49999999999999822, 0.000000000000000000 ) ) ;
#96321 = ADVANCED_FACE ( 'NONE', ( #56439 ), #38882, .T. ) ;
#96322 = CARTESIAN_POINT ( 'NONE',  ( 0.8801356535991349261, 124.4373638429518962, -4.500000000000001776 ) ) ;
#96323 = CARTESIAN_POINT ( 'NONE',  ( -4.164238869374098151, 16.59541550158063927, -3.795296366450310543 ) ) ;
#96324 = CARTESIAN_POINT ( 'NONE',  ( 17.08211943468705840, 35.13708216824730357, -12.26659068614894466 ) ) ;
#96325 = CARTESIAN_POINT ( 'NONE',  ( 12.63842701281683922, 44.55059781766745175, -9.846743663894590881 ) ) ;
#96326 = DIRECTION ( 'NONE',  ( -0.000000000000000000, -1.000000000000000000, -0.000000000000000000 ) ) ;
#96327 = CARTESIAN_POINT ( 'NONE',  ( 4.559911319644449179, 43.89701867748816966, 9.422509992056141925 ) ) ;
#96328 = CARTESIAN_POINT ( 'NONE',  ( 15.44008868035555793, 61.39701867748817676, -9.422509992056140149 ) ) ;
#96329 = FACE_OUTER_BOUND ( 'NONE', #15095, .T. ) ;
#96330 = ORIENTED_EDGE ( 'NONE', *, *, #17682, .F. ) ;
#96331 = CARTESIAN_POINT ( 'NONE',  ( 16.40814093676323893, 40.79030133659708923, 11.09922568453595026 ) ) ;
#96332 = ORIENTED_EDGE ( 'NONE', *, *, #97672, .T. ) ;
#96333 = CARTESIAN_POINT ( 'NONE',  ( -0.8801773607111008646, 63.27201867748817676, 2.915334737309923430 ) ) ;
#96334 = ORIENTED_EDGE ( 'NONE', *, *, #66898, .T. ) ;
#96335 = CARTESIAN_POINT ( 'NONE',  ( -0.3689425029237881626, 7.428748834913967869, 10.36894250292379027 ) ) ;
#96336 = DIRECTION ( 'NONE',  ( -0.8038568606172203923, 0.000000000000000000, 0.5948227867513371514 ) ) ;
#96337 = DIRECTION ( 'NONE',  ( 0.3826834323650877834, -0.000000000000000000, 0.9238795325112876267 ) ) ;
#96338 = VERTEX_POINT ( 'NONE', #48920 ) ;
#96339 =( NAMED_UNIT ( * ) PLANE_ANGLE_UNIT ( ) SI_UNIT ( $, .RADIAN. ) );
#96340 = CARTESIAN_POINT ( 'NONE',  ( 0.5774900079438590739, 17.64701867748817321, -5.440088680355550821 ) ) ;
#96341 = CARTESIAN_POINT ( 'NONE',  ( 19.42250999205614193, 60.14701867748817676, 5.440088680355555262 ) ) ;
#96342 = EDGE_CURVE ( 'NONE', #76829, #44664, #14975, .T. ) ;
#96343 = CARTESIAN_POINT ( 'NONE',  ( -4.164238869374098151, 21.59541550158063217, -3.795296366450310543 ) ) ;
#96344 = CIRCLE ( 'NONE', #42027, 2.000000000000000888 ) ;
#96345 = CARTESIAN_POINT ( 'NONE',  ( 19.42250999205614193, 20.14701867748817321, 5.440088680355555262 ) ) ;
#96346 = CARTESIAN_POINT ( 'NONE',  ( 17.20831665107776587, 57.88393115100078745, 7.208316651077764980 ) ) ;
#96347 = ORIENTED_EDGE ( 'NONE', *, *, #10295, .T. ) ;
#96348 = ADVANCED_FACE ( 'NONE', ( #75365 ), #28870, .F. ) ;
#96349 = CIRCLE ( 'NONE', #93111, 2.999999999999997335 ) ;
#96350 = CARTESIAN_POINT ( 'NONE',  ( 18.52753015748617571, 58.09226448433411605, 4.923371831947298993 ) ) ;
#96351 = ORIENTED_EDGE ( 'NONE', *, *, #50335, .F. ) ;
#96352 = COLOUR_RGB ( '', 0.09019608, 0.27058824, 0.51372549) ;
#96353 = CARTESIAN_POINT ( 'NONE',  ( 4.559911319644449179, 53.89701867748817676, 9.422509992056141925 ) ) ;
#96354 = CARTESIAN_POINT ( 'NONE',  ( 7.361572987183170547, 67.05059781766746596, 9.846743663894590881 ) ) ;
#96356 = CARTESIAN_POINT ( 'NONE',  ( -7.443082168244859353, 2.043284506775928211, -9.050130897022322429 ) ) ;
#96355 = CARTESIAN_POINT ( 'NONE',  ( 20.88017736071110164, 10.35535201082150714, 2.915334737309930979 ) ) ;
#96357 = CARTESIAN_POINT ( 'NONE',  ( 10.00000000000000000, 66.81368534415484817, -10.88017736071110342 ) ) ;
#96358 = CARTESIAN_POINT ( 'NONE',  ( 7.084665262690076126, 12.02201867748817321, -10.88017736071110164 ) ) ;
#96359 = ORIENTED_EDGE ( 'NONE', *, *, #41929, .F. ) ;
#96360 = CARTESIAN_POINT ( 'NONE',  ( 3.591859063236761518, 59.95696800326375353, 11.09922568453594849 ) ) ;
#96361 = CARTESIAN_POINT ( 'NONE',  ( 20.88017736071110519, 25.56368534415483751, 2.639326808657452039E-16 ) ) ;
#96362 = DIRECTION ( 'NONE',  ( 0.000000000000000000, 0.000000000000000000, 1.000000000000000000 ) ) ;
#96363 = CARTESIAN_POINT ( 'NONE',  ( 19.38216949554541202, 40.99863466993042493, 9.382169495545424454 ) ) ;
#96364 = CARTESIAN_POINT ( 'NONE',  ( -0.8801773607110991993, 52.85535201082151247, -2.915334737309923874 ) ) ;
#96365 = CARTESIAN_POINT ( 'NONE',  ( 5.076628168052704559, 55.17559781766745175, -8.527530157486179263 ) ) ;
#96366 = ORIENTED_EDGE ( 'NONE', *, *, #82692, .T. ) ;
#96367 = DIRECTION ( 'NONE',  ( -0.1650476058606676344, 0.000000000000000000, -0.9862856015372331031 ) ) ;
#96368 = CARTESIAN_POINT ( 'NONE',  ( 21.09922568453594849, 11.20696800326375531, 6.408140936763242479 ) ) ;
#96370 = CARTESIAN_POINT ( 'NONE',  ( 1.472469842513823179, 46.42559781766745175, 4.923371831947296329 ) ) ;
#96369 = CARTESIAN_POINT ( 'NONE',  ( -13.80022967267210987, 90.89648642031431791, -7.755896862406649106 ) ) ;
#96371 = CARTESIAN_POINT ( 'NONE',  ( 0.5774900079438607392, 23.48035201082150536, 5.440088680355550821 ) ) ;
#96372 = CARTESIAN_POINT ( 'NONE',  ( 12.63842701281683922, 49.55059781766744464, -9.846743663894590881 ) ) ;
#96373 = LINE ( 'NONE', #75698, #77840 ) ;
#96374 = PRESENTATION_LAYER_ASSIGNMENT (  '', '', ( #40494 ) ) ;
#96376 = CARTESIAN_POINT ( 'NONE',  ( 5.076628168052704559, 5.175597817667451750, -8.527530157486179263 ) ) ;
#96375 = CARTESIAN_POINT ( 'NONE',  ( 1.472469842513823179, 41.42559781766745886, 4.923371831947296329 ) ) ;
#96377 = SURFACE_SIDE_STYLE ('',( #42868 ) ) ;
#96379 = VERTEX_POINT ( 'NONE', #13892 ) ;
#96378 = CARTESIAN_POINT ( 'NONE',  ( 19.84674366389459621, 53.50893115100078745, 7.409399052514197653E-17 ) ) ;
#96380 = DIRECTION ( 'NONE',  ( 1.000000000000000000, -1.257568779154408485E-17, 0.000000000000000000 ) ) ;
#96381 = CARTESIAN_POINT ( 'NONE',  ( 16.40814093676323893, 40.79030133659708923, 11.09922568453595026 ) ) ;
#96382 = CARTESIAN_POINT ( 'NONE',  ( 12.63842701281683034, 32.46726448433412315, 9.846743663894596210 ) ) ;
#96383 = CARTESIAN_POINT ( 'NONE',  ( -0.04068437667225312249, 12.21974360917720581, -6.396802510829700417 ) ) ;
#96384 = CARTESIAN_POINT ( 'NONE',  ( -4.164238869374099039, 61.80374883491397497, 8.674139862899312516E-16 ) ) ;
#96385 = CARTESIAN_POINT ( 'NONE',  ( 0.1532563361054100626, 35.80059781766745175, -2.638427012816831230 ) ) ;
#96386 = ORIENTED_EDGE ( 'NONE', *, *, #24734, .F. ) ;
#96387 = CARTESIAN_POINT ( 'NONE',  ( 20.00000000000000711, 79.40087001978916703, 4.500000000000000000 ) ) ;
#96388 = CARTESIAN_POINT ( 'NONE',  ( -0.3689425029237898834, 51.17874883491397497, -10.36894250292378850 ) ) ;
#96389 = CARTESIAN_POINT ( 'NONE',  ( 1.472469842513823179, 66.42559781766745175, 4.923371831947296329 ) ) ;
#96390 = CARTESIAN_POINT ( 'NONE',  ( 10.00000000000000178, 19.31368534415484106, 10.88017736071110342 ) ) ;
#96391 = CARTESIAN_POINT ( 'NONE',  ( 22.26659068614894466, 38.88708216824731068, 7.082119434687054849 ) ) ;
#96393 = CARTESIAN_POINT ( 'NONE',  ( -4.873787042390612001, -0.03417435944610275333, -13.39061984619925916 ) ) ;
#96392 = CARTESIAN_POINT ( 'NONE',  ( 24.16423886937410614, 49.30374883491396787, 8.672049930838204340E-16 ) ) ;
#96394 = CARTESIAN_POINT ( 'NONE',  ( 18.52753015748618282, 8.925597817667451750, -4.923371831947291888 ) ) ;
#96395 = CARTESIAN_POINT ( 'NONE',  ( 16.40814093676324603, 2.456968003263753531, -11.09922568453594671 ) ) ;
#96396 = ORIENTED_EDGE ( 'NONE', *, *, #45490, .T. ) ;
#96397 = CARTESIAN_POINT ( 'NONE',  ( 4.559911319644449179, 47.23035201082150536, -9.422509992056141925 ) ) ;
#96398 = DIRECTION ( 'NONE',  ( 0.000000000000000000, -1.000000000000000000, 0.000000000000000000 ) ) ;
#96399 = DIRECTION ( 'NONE',  ( -0.000000000000000000, -1.000000000000000000, -0.000000000000000000 ) ) ;
#96400 = CARTESIAN_POINT ( 'NONE',  ( 8.879999999999991900, 76.07179676972447169, -6.500000000000000888 ) ) ;
#96401 = DIRECTION ( 'NONE',  ( 0.000000000000000000, 0.000000000000000000, 1.000000000000000000 ) ) ;
#96402 = ORIENTED_EDGE ( 'NONE', *, *, #3014, .T. ) ;
#96403 = STYLED_ITEM ( 'NONE', ( #88771 ), #96915 ) ;
#96404 = CARTESIAN_POINT ( 'NONE',  ( -4.164238869374099039, 41.80374883491397497, 8.674139862899312516E-16 ) ) ;
#96405 =( NAMED_UNIT ( * ) SI_UNIT ( $, .STERADIAN. ) SOLID_ANGLE_UNIT ( ) );
#96407 = DIRECTION ( 'NONE',  ( 0.000000000000000000, 0.000000000000000000, 1.000000000000000000 ) ) ;
#96406 = DIRECTION ( 'NONE',  ( 0.000000000000000000, 0.000000000000000000, -1.000000000000000000 ) ) ;
#96408 = CARTESIAN_POINT ( 'NONE',  ( 20.88017736071110875, 20.77201867748816611, -2.915334737309920765 ) ) ;
#96409 = CARTESIAN_POINT ( 'NONE',  ( 0.6178305044545818747, 38.49863466993042493, -9.382169495545419124 ) ) ;
#96410 = CARTESIAN_POINT ( 'NONE',  ( -10.32896413005679648, 10.10497603579418247, 5.963430220938290560 ) ) ;
#96411 = CARTESIAN_POINT ( 'NONE',  ( 13.43411237798105340, 20.58196800326374643, 12.81628187352647963 ) ) ;
#96412 = CARTESIAN_POINT ( 'NONE',  ( 16.40814093676323893, 55.79030133659708923, 11.09922568453595026 ) ) ;
#96413 = ORIENTED_EDGE ( 'NONE', *, *, #71490, .F. ) ;
#96414 = VECTOR ( 'NONE', #49431, 1000.000000000000000 ) ;
#96415 = CARTESIAN_POINT ( 'NONE',  ( 5.365144748710862110, -17.52568678401977920, -4.000000000000000000 ) ) ;
#96416 = DIRECTION ( 'NONE',  ( 0.000000000000000000, 0.000000000000000000, 1.000000000000000000 ) ) ;
#96417 = CARTESIAN_POINT ( 'NONE',  ( 24.16423886937410614, 24.51208216824730002, -3.795296366450302550 ) ) ;
#96418 = CARTESIAN_POINT ( 'NONE',  ( 2.917880565312950480, 0.9704155015806342766, -12.26659068614894821 ) ) ;
#96419 = LINE ( 'NONE', #58382, #40715 ) ;
#96420 = CARTESIAN_POINT ( 'NONE',  ( -0.8801773607111008646, 28.27201867748817321, 2.915334737309923430 ) ) ;
#96421 = CARTESIAN_POINT ( 'NONE',  ( 8.375939845167756914, 0.000000000000000000, -11.52849216984298941 ) ) ;
#96422 = DIRECTION ( 'NONE',  ( 0.000000000000000000, -1.000000000000000000, 0.000000000000000000 ) ) ;
#96424 = B_SPLINE_CURVE_WITH_KNOTS ( 'NONE', 3,
 ( #42850, #5357, #11853, #4861, #35337, #97347, #89332, #13835 ),
 .UNSPECIFIED., .F., .F.,
 ( 4, 2, 2, 4 ),
 ( 0.009612260643802141014, 0.01201872016511521847, 0.01442517968642829593, 0.01923809872905445084 ),
 .UNSPECIFIED. ) ;
#96423 = CARTESIAN_POINT ( 'NONE',  ( 2.035157376598822676, 37.43868534415484106, -7.964842623401177768 ) ) ;
#96425 = CARTESIAN_POINT ( 'NONE',  ( 20.88017736071110519, 55.56368534415484817, 2.639326808657452039E-16 ) ) ;
#96426 = CARTESIAN_POINT ( 'NONE',  ( 10.00000000000000178, 10.37363466993041961, 12.81628187352647608 ) ) ;
#96427 = CARTESIAN_POINT ( 'NONE',  ( 0.9537732071275217827, 0.6838673512643470564, 6.500000000000001776 ) ) ;
#96428 = CARTESIAN_POINT ( 'NONE',  ( 18.52753015748618282, 28.92559781766745175, -4.923371831947291888 ) ) ;
#96429 = EDGE_CURVE ( 'NONE', #46057, #78138, #36390, .T. ) ;
#96430 = SURFACE_STYLE_FILL_AREA ( #35407 ) ;
#96431 = CARTESIAN_POINT ( 'NONE',  ( 7.084665262690076126, 39.10535201082150536, 10.88017736071109987 ) ) ;
#96432 = EDGE_CURVE ( 'NONE', #4350, #30913, #66884, .T. ) ;
#96433 = CARTESIAN_POINT ( 'NONE',  ( 10.00000000000000000, 2.873634669930420049, -12.81628187352647608 ) ) ;
#96434 = CARTESIAN_POINT ( 'NONE',  ( 15.00000000000000000, 11.50000000000000000, 6.500000000000000888 ) ) ;
#96435 = ADVANCED_FACE ( 'NONE', ( #74875 ), #20901, .T. ) ;
#96436 = CARTESIAN_POINT ( 'NONE',  ( 2.791683348922240793, 26.63393115100078745, 7.208316651077764092 ) ) ;
#96437 = CARTESIAN_POINT ( 'NONE',  ( 21.09922568453594849, 46.20696800326376064, 6.408140936763242479 ) ) ;
#96438 = CARTESIAN_POINT ( 'NONE',  ( 10.00000000000000178, 7.258931151000785675, 9.846743663894594434 ) ) ;
#96439 = ORIENTED_EDGE ( 'NONE', *, *, #26204, .F. ) ;
#96440 = LINE ( 'NONE', #88426, #34073 ) ;
#96441 = CARTESIAN_POINT ( 'NONE',  ( 0.000000000000000000, 14.49999999999999822, 0.000000000000000000 ) ) ;
#96442 = CARTESIAN_POINT ( 'NONE',  ( -0.8801773607110991993, 22.85535201082150181, -2.915334737309923874 ) ) ;
#96444 = CARTESIAN_POINT ( 'NONE',  ( 6.204703633549690345, 35.76208216824729647, -14.16423886937410259 ) ) ;
#96443 = DIRECTION ( 'NONE',  ( 0.000000000000000000, 1.000000000000000000, 0.000000000000000000 ) ) ;
#96445 = CARTESIAN_POINT ( 'NONE',  ( 19.84674366389459266, 28.71726448433411960, -2.638427012816827677 ) ) ;
#96446 = CARTESIAN_POINT ( 'NONE',  ( 19.42250999205614193, 15.14701867748817143, 5.440088680355555262 ) ) ;
#96447 = CARTESIAN_POINT ( 'NONE',  ( 20.36894250292379382, 63.67874883491396787, 10.36894250292379205 ) ) ;
#96448 = ORIENTED_EDGE ( 'NONE', *, *, #13324, .T. ) ;
#96449 = CARTESIAN_POINT ( 'NONE',  ( 10.00000000000000000, 6.813685344154838397, -10.88017736071110342 ) ) ;
#96450 = CARTESIAN_POINT ( 'NONE',  ( 10.00000000000000000, 36.81368534415484106, -10.88017736071110342 ) ) ;
#96452 = CARTESIAN_POINT ( 'NONE',  ( 10.00000000000000178, 44.31368534415484106, 10.88017736071110342 ) ) ;
#96451 = CARTESIAN_POINT ( 'NONE',  ( -12.03768810259473732, 15.00000000000000533, -8.306778944023500699 ) ) ;
#96453 = ORIENTED_EDGE ( 'NONE', *, *, #16828, .F. ) ;
#96454 = CARTESIAN_POINT ( 'NONE',  ( 7.361572987183170547, 62.05059781766745886, 9.846743663894590881 ) ) ;
#96455 = CARTESIAN_POINT ( 'NONE',  ( 10.00000000000000178, 39.31368534415484106, 10.88017736071110342 ) ) ;
#96456 = SURFACE_SIDE_STYLE ('',( #36431 ) ) ;
#96457 = PLANE ( 'NONE',  #32982 ) ;
#96458 = CARTESIAN_POINT ( 'NONE',  ( 19.38216949554541202, 60.99863466993042493, 9.382169495545424454 ) ) ;
#96459 = CARTESIAN_POINT ( 'NONE',  ( 0.000000000000000000, 14.49999999999999822, 0.000000000000000000 ) ) ;
#96460 = CARTESIAN_POINT ( 'NONE',  ( 24.16423886937409904, 39.09541550158062506, 3.795296366450317205 ) ) ;
#96461 = CARTESIAN_POINT ( 'NONE',  ( 0.5774900079438607392, 48.48035201082150536, 5.440088680355550821 ) ) ;
#96462 = B_SPLINE_CURVE_WITH_KNOTS ( 'NONE', 3,
 ( #87922, #2985, #18952, #49927, #11440, #2499 ),
 .UNSPECIFIED., .F., .F.,
 ( 4, 2, 4 ),
 ( 3.409110551494641945E-05, 0.0004400426677367920468, 0.0008459942299586376132 ),
 .UNSPECIFIED. ) ;
#96463 = CARTESIAN_POINT ( 'NONE',  ( 19.42250999205614548, 30.98035201082150536, -5.440088680355545492 ) ) ;
#96464 = CARTESIAN_POINT ( 'NONE',  ( 7.361572987183170547, 67.05059781766746596, 9.846743663894590881 ) ) ;
#96465 = CARTESIAN_POINT ( 'NONE',  ( -10.19513985507840736, 0.5000000000000004441, 11.00268709613209950 ) ) ;
#96466 = CARTESIAN_POINT ( 'NONE',  ( 12.63842701281683922, 49.55059781766744464, -9.846743663894590881 ) ) ;
#96467 = ORIENTED_EDGE ( 'NONE', *, *, #17867, .F. ) ;
#96468 = EDGE_CURVE ( 'NONE', #62128, #68797, #75466, .T. ) ;
#96469 = CARTESIAN_POINT ( 'NONE',  ( 17.20831665107776587, 27.88393115100078390, 7.208316651077764980 ) ) ;
#96470 = CARTESIAN_POINT ( 'NONE',  ( 11.09922568453595026, -18.79303199673624292, 6.408140936763232709 ) ) ;
#96471 = CARTESIAN_POINT ( 'NONE',  ( 19.42250999205614193, 10.14701867748816966, 5.440088680355555262 ) ) ;
#96472 = CARTESIAN_POINT ( 'NONE',  ( 1.472469842513823179, 26.42559781766745175, 4.923371831947296329 ) ) ;
#96473 = CARTESIAN_POINT ( 'NONE',  ( 22.81628187352648496, 6.831968003263753531, -3.434112377981050290 ) ) ;
#96474 = CARTESIAN_POINT ( 'NONE',  ( 19.42250999205614193, 55.14701867748817676, 5.440088680355555262 ) ) ;
#96476 = CARTESIAN_POINT ( 'NONE',  ( 6.565887622018943937, 53.08196800326374643, -12.81628187352647608 ) ) ;
#96475 = CARTESIAN_POINT ( 'NONE',  ( 15.44008868035555260, 19.73035201082150536, 9.422509992056143702 ) ) ;
#96477 = CARTESIAN_POINT ( 'NONE',  ( 22.26659068614895176, 39.72041550158063217, -7.082119434687042414 ) ) ;
#96478 = EDGE_CURVE ( 'NONE', #1436, #73387, #83369, .T. ) ;
#96479 = AXIS2_PLACEMENT_3D ( 'NONE', #94994, #87498, #19013 ) ;
#96480 = CARTESIAN_POINT ( 'NONE',  ( -44.76220231628991542, 105.1780506895835998, 5.381450656841352043 ) ) ;
#96481 = EDGE_LOOP ( 'NONE', ( #79083, #82643, #10941, #81802, #47882, #73557 ) ) ;
#96482 = CARTESIAN_POINT ( 'NONE',  ( 1.472469842513823179, 65.59226448433412315, -4.923371831947296329 ) ) ;
#96483 = CARTESIAN_POINT ( 'NONE',  ( 2.035157376598824452, 13.68868534415483751, 7.964842623401179544 ) ) ;
#96484 = CARTESIAN_POINT ( 'NONE',  ( 19.42250999205614548, 35.98035201082151247, -5.440088680355545492 ) ) ;
#96485 = CARTESIAN_POINT ( 'NONE',  ( 10.00000000000000178, 57.25893115100078745, 9.846743663894594434 ) ) ;
#96486 = VECTOR ( 'NONE', #10189, 1000.000000000000000 ) ;
#96487 = VERTEX_POINT ( 'NONE', #44861 ) ;
#96488 = CARTESIAN_POINT ( 'NONE',  ( 0.1532563361054083140, 21.00893115100078745, 1.131784320476157264E-15 ) ) ;
#96489 = CARTESIAN_POINT ( 'NONE',  ( 1.472469842513823179, 15.59226448433411960, -4.923371831947296329 ) ) ;
#96490 = CARTESIAN_POINT ( 'NONE',  ( 10.00000000000000178, 17.25893115100078745, 9.846743663894594434 ) ) ;
#96491 = CARTESIAN_POINT ( 'NONE',  ( 12.63842701281683922, 4.550597817667451750, -9.846743663894590881 ) ) ;
#96492 = CARTESIAN_POINT ( 'NONE',  ( 18.52753015748617571, 3.092264484334118269, 4.923371831947298993 ) ) ;
#96493 = DIRECTION ( 'NONE',  ( 0.000000000000000000, 1.000000000000000000, -6.938893903907221278E-15 ) ) ;
#96495 = DIRECTION ( 'NONE',  ( 0.9588197348681964938, 0.000000000000000000, -0.2840153447039108214 ) ) ;
#96494 = CARTESIAN_POINT ( 'NONE',  ( 2.035157376598822676, 67.43868534415484817, -7.964842623401177768 ) ) ;
#96496 = CARTESIAN_POINT ( 'NONE',  ( 18.52753015748617571, 3.092264484334118269, 4.923371831947298993 ) ) ;
#96498 = ORIENTED_EDGE ( 'NONE', *, *, #10801, .T. ) ;
#96497 = CARTESIAN_POINT ( 'NONE',  ( 18.52753015748618282, 18.92559781766745175, -4.923371831947291888 ) ) ;
#96499 = CARTESIAN_POINT ( 'NONE',  ( 18.72515096720583827, 56.07228050351029225, -6.499999999999802824 ) ) ;
#96500 = CARTESIAN_POINT ( 'NONE',  ( 22.81628187352647785, 1.623634669930420271, 6.195893100308588602E-16 ) ) ;
#96501 = ORIENTED_EDGE ( 'NONE', *, *, #2089, .T. ) ;
#96502 = DIRECTION ( 'NONE',  ( 0.9848077530122086864, 0.1736481776669271671, 0.000000000000000000 ) ) ;
#96503 = CARTESIAN_POINT ( 'NONE',  ( 10.00000000000000178, 18.05374883491396787, 14.16423886937410082 ) ) ;
#96504 = UNCERTAINTY_MEASURE_WITH_UNIT (LENGTH_MEASURE( 1.000000000000000082E-05 ), #80794, 'distance_accuracy_value', 'NONE');
#96505 = DIRECTION ( 'NONE',  ( 0.1822355254921448342, 0.000000000000000000, 0.9832549075639550606 ) ) ;
#96506 = CARTESIAN_POINT ( 'NONE',  ( -2.266590686148945544, 16.38708216824730357, -7.082119434687050408 ) ) ;
#96507 = CARTESIAN_POINT ( 'NONE',  ( 6.204703633549690345, 45.76208216824729647, -14.16423886937410259 ) ) ;
#96508 = ADVANCED_FACE ( 'NONE', ( #45362 ), #45292, .T. ) ;
#96509 = SURFACE_STYLE_USAGE ( .BOTH. , #72990 ) ;
#96511 = DIRECTION ( 'NONE',  ( 1.000000000000000000, 0.000000000000000000, 0.000000000000000000 ) ) ;
#96510 = CARTESIAN_POINT ( 'NONE',  ( -2.266590686148945544, 6.387082168247300906, -7.082119434687050408 ) ) ;
#96512 = CARTESIAN_POINT ( 'NONE',  ( 2.035157376598822676, 37.43868534415484106, -7.964842623401177768 ) ) ;
#96513 = SPHERICAL_SURFACE ( 'NONE', #40388, 0.2500000000000000000 ) ;
#96514 = ORIENTED_EDGE ( 'NONE', *, *, #86940, .T. ) ;
#96515 = CARTESIAN_POINT ( 'NONE',  ( 19.84674366389459266, 13.30059781766745353, 2.638427012816836559 ) ) ;
#96517 = CARTESIAN_POINT ( 'NONE',  ( 19.84674366389459266, 28.71726448433411960, -2.638427012816827677 ) ) ;
#96516 = CARTESIAN_POINT ( 'NONE',  ( 2.035157376598822676, 62.43868534415483396, -7.964842623401177768 ) ) ;
#96518 = CARTESIAN_POINT ( 'NONE',  ( -0.8801773607111009756, 8.063685344154837509, 1.068504757029289695E-15 ) ) ;
#96519 = CARTESIAN_POINT ( 'NONE',  ( -1.099225684535947600, 63.70696800326376774, -6.408140936763238038 ) ) ;
#96520 = CARTESIAN_POINT ( 'NONE',  ( 0.1532563361054083140, 56.00893115100078745, 1.131784320476157264E-15 ) ) ;
#96522 = EDGE_CURVE ( 'NONE', #49230, #30576, #68378, .T. ) ;
#96521 = VECTOR ( 'NONE', #61255, 1000.000000000000000 ) ;
#96523 = CARTESIAN_POINT ( 'NONE',  ( 19.38216949554541202, 35.99863466993041072, 9.382169495545424454 ) ) ;
#96524 = CARTESIAN_POINT ( 'NONE',  ( 10.36894250292379027, -31.32125116508602858, 10.36894250292378672 ) ) ;
#96525 = CARTESIAN_POINT ( 'NONE',  ( 19.84674366389459266, 33.71726448433410894, -2.638427012816827677 ) ) ;
#96526 = CARTESIAN_POINT ( 'NONE',  ( -0.3689425029237898834, 31.17874883491396787, -10.36894250292378850 ) ) ;
#96527 = ORIENTED_EDGE ( 'NONE', *, *, #67082, .F. ) ;
#96528 = CARTESIAN_POINT ( 'NONE',  ( -11.48952521350030587, 15.00000000000000000, 8.845383562533664090 ) ) ;
#96529 = CARTESIAN_POINT ( 'NONE',  ( 20.88017736071110164, 45.35535201082149115, 2.915334737309930979 ) ) ;
#96530 = CARTESIAN_POINT ( 'NONE',  ( 10.00000000000000000, 61.81368534415484106, -10.88017736071110342 ) ) ;
#96531 = CARTESIAN_POINT ( 'NONE',  ( 2.917880565312948704, 42.63708216824729647, 12.26659068614894643 ) ) ;
#96532 = CARTESIAN_POINT ( 'NONE',  ( 18.52753015748618282, 63.92559781766745886, -4.923371831947291888 ) ) ;
#96533 = CARTESIAN_POINT ( 'NONE',  ( 21.09922568453595559, 62.04030133659709634, -6.408140936763230044 ) ) ;
#96534 = CARTESIAN_POINT ( 'NONE',  ( -0.8801773607110991993, 42.85535201082150536, -2.915334737309923874 ) ) ;
#96535 = CARTESIAN_POINT ( 'NONE',  ( -4.285591316845103194, -17.54293119412274038, -2.500000000000001776 ) ) ;
#96536 = CARTESIAN_POINT ( 'NONE',  ( -1.099225684535947600, 28.70696800326375353, -6.408140936763238038 ) ) ;
#96537 = CARTESIAN_POINT ( 'NONE',  ( 2.791683348922240793, 51.63393115100078745, 7.208316651077764092 ) ) ;
#96538 = CARTESIAN_POINT ( 'NONE',  ( -5.440088680355547268, 13.89701867748818032, 9.422509992056143702 ) ) ;
#96539 = CARTESIAN_POINT ( 'NONE',  ( 19.42250999205614193, 5.147018677488171434, 5.440088680355555262 ) ) ;
#96540 = ORIENTED_EDGE ( 'NONE', *, *, #98121, .T. ) ;
#96541 = FILL_AREA_STYLE_COLOUR ( '', #16250 ) ;
#96542 = CARTESIAN_POINT ( 'NONE',  ( 20.15039907845753575, 65.60158574516643171, -6.262539305110073506 ) ) ;
#96543 = CARTESIAN_POINT ( 'NONE',  ( 2.035157376598824452, 68.68868534415484817, 7.964842623401179544 ) ) ;
#96544 = CARTESIAN_POINT ( 'NONE',  ( 15.44008868035555260, 64.73035201082151957, 9.422509992056143702 ) ) ;
#96545 = CARTESIAN_POINT ( 'NONE',  ( -13.61464873478165138, 14.49999999999999112, -6.296136897218031159 ) ) ;
#96546 = ADVANCED_FACE ( 'NONE', ( #51390 ), #81876, .T. ) ;
#96547 = VECTOR ( 'NONE', #77407, 1000.000000000000000 ) ;
#96548 = CARTESIAN_POINT ( 'NONE',  ( 5.076628168052704559, 35.17559781766745175, -8.527530157486179263 ) ) ;
#96549 = CARTESIAN_POINT ( 'NONE',  ( 10.00000000000000178, 19.31368534415484106, 10.88017736071110342 ) ) ;
#96550 = EDGE_CURVE ( 'NONE', #91827, #59823, #58051, .T. ) ;
#96551 = CARTESIAN_POINT ( 'NONE',  ( -1.099225684535947600, 3.706968003263753531, -6.408140936763238038 ) ) ;
#96553 = CARTESIAN_POINT ( 'NONE',  ( 3.195792623639593266, 9.120456701841145986, 11.92686044187653494 ) ) ;
#96552 = CARTESIAN_POINT ( 'NONE',  ( 20.88017736071110164, 30.35535201082151247, 2.915334737309930979 ) ) ;
#96554 = DIRECTION ( 'NONE',  ( 0.000000000000000000, 1.000000000000000000, -0.000000000000000000 ) ) ;
#96555 = CARTESIAN_POINT ( 'NONE',  ( -2.816281873526473856, 39.12363466993041783, 9.499525473075851096E-16 ) ) ;
#96556 = VERTEX_POINT ( 'NONE', #84370 ) ;
#96557 = CARTESIAN_POINT ( 'NONE',  ( 19.42250999205614548, 65.98035201082151957, -5.440088680355545492 ) ) ;
#96558 = AXIS2_PLACEMENT_3D ( 'NONE', #33049, #1605, #32054 ) ;
#96560 = CARTESIAN_POINT ( 'NONE',  ( 6.689969769698956625, 15.00000000000000000, -12.58200319823970226 ) ) ;
#96559 = CARTESIAN_POINT ( 'NONE',  ( 13.43411237798105340, 15.58196800326374998, 12.81628187352647963 ) ) ;
#96561 = CARTESIAN_POINT ( 'NONE',  ( 19.42250999205614548, 35.98035201082151247, -5.440088680355545492 ) ) ;
#96562 = CARTESIAN_POINT ( 'NONE',  ( 19.84674366389459266, 63.30059781766745886, 2.638427012816836559 ) ) ;
#96563 = CARTESIAN_POINT ( 'NONE',  ( 22.26659068614894466, 63.88708216824730357, 7.082119434687054849 ) ) ;
#96564 = CARTESIAN_POINT ( 'NONE',  ( 18.52753015748617571, 48.09226448433412315, 4.923371831947298993 ) ) ;
#96565 = CARTESIAN_POINT ( 'NONE',  ( 7.361572987183170547, 7.050597817667451750, 9.846743663894590881 ) ) ;
#96566 = CARTESIAN_POINT ( 'NONE',  ( -0.8801773607110991993, 67.85535201082151957, -2.915334737309923874 ) ) ;
#96567 = CARTESIAN_POINT ( 'NONE',  ( 13.40508947812166873, 4.119406375368599477E-16, -5.527528931046103544 ) ) ;
#96568 = CARTESIAN_POINT ( 'NONE',  ( 24.16423886937410614, 24.30374883491396787, 8.672049930838204340E-16 ) ) ;
#96569 = DIRECTION ( 'NONE',  ( 0.1736481776669272503, -0.9848077530122086864, 0.000000000000000000 ) ) ;
#96570 = ORIENTED_EDGE ( 'NONE', *, *, #91225, .T. ) ;
#96571 = CARTESIAN_POINT ( 'NONE',  ( 2.917880565312948704, 62.63708216824730357, 12.26659068614894643 ) ) ;
#96572 = CARTESIAN_POINT ( 'NONE',  ( -2.266590686148945544, 46.38708216824730357, -7.082119434687050408 ) ) ;
#96573 = CARTESIAN_POINT ( 'NONE',  ( 14.92337183194729633, 27.67559781766745530, 8.527530157486181039 ) ) ;
#96574 = AXIS2_PLACEMENT_3D ( 'NONE', #61828, #37878, #46828 ) ;
#96575 = CARTESIAN_POINT ( 'NONE',  ( 6.565887622018943937, 25.16530133659708213, 12.81628187352647430 ) ) ;
#96576 = LINE ( 'NONE', #53019, #1273 ) ;
#96577 = FILL_AREA_STYLE ('',( #67048 ) ) ;
#96578 = CARTESIAN_POINT ( 'NONE',  ( 0.5774900079438607392, 13.48035201082150358, 5.440088680355550821 ) ) ;
#96579 = CARTESIAN_POINT ( 'NONE',  ( 13.79529636645030344, 63.26208216824730357, 14.16423886937410614 ) ) ;
#96580 = EDGE_CURVE ( 'NONE', #87437, #50168, #85334, .T. ) ;
#96581 = CARTESIAN_POINT ( 'NONE',  ( 12.25993886608605976, 14.63595249122790953, -8.642563219313631251 ) ) ;
#96582 = CARTESIAN_POINT ( 'NONE',  ( 2.791683348922237240, 5.383931151000785675, -7.208316651077763204 ) ) ;
#96583 = EDGE_CURVE ( 'NONE', #94075, #31231, #81963, .T. ) ;
#96584 = CARTESIAN_POINT ( 'NONE',  ( 18.04007052943773104, 3.015283700948082402, 5.767676674365838529 ) ) ;
#96585 = CARTESIAN_POINT ( 'NONE',  ( -3.469446951953614189E-15, -0.2410688489992082739, -9.846743663894594434 ) ) ;
#96586 = ORIENTED_EDGE ( 'NONE', *, *, #75964, .T. ) ;
#96587 =( BOUNDED_CURVE ( )  B_SPLINE_CURVE ( 3, ( #12087, #34088, #26593, #35070 ),
 .UNSPECIFIED., .F., .F. ) 
 B_SPLINE_CURVE_WITH_KNOTS ( ( 4, 4 ),
 ( 4.712388980384680792, 6.283185307179586232 ),
 .UNSPECIFIED. ) 
 CURVE ( )  GEOMETRIC_REPRESENTATION_ITEM ( )  RATIONAL_B_SPLINE_CURVE ( ( 1.000000000000000000, 0.8047378541243628280, 0.8047378541243628280, 1.000000000000000000 ) ) 
 REPRESENTATION_ITEM ( '' )  );
#96588 = VERTEX_POINT ( 'NONE', #55829 ) ;
#96589 = PRESENTATION_STYLE_ASSIGNMENT (( #66061 ) ) ;
#96590 = ORIENTED_EDGE ( 'NONE', *, *, #54183, .T. ) ;
#96592 = CARTESIAN_POINT ( 'NONE',  ( 12.91533473730992121, 29.52201867748817321, 10.88017736071110164 ) ) ;
#96591 = CARTESIAN_POINT ( 'NONE',  ( 2.035157376598822676, 22.43868534415483396, -7.964842623401177768 ) ) ;
#96594 = CARTESIAN_POINT ( 'NONE',  ( 22.81628187352647785, 21.41530133659708923, 3.434112377981063169 ) ) ;
#96593 = CARTESIAN_POINT ( 'NONE',  ( 1.472469842513823179, 55.59226448433412315, -4.923371831947296329 ) ) ;
#96595 = DIRECTION ( 'NONE',  ( -0.5547001962252291474, -0.8320502943378437211, -0.000000000000000000 ) ) ;
#96596 = AXIS2_PLACEMENT_3D ( 'NONE', #17645, #46638, #47633 ) ;
#96597 = CARTESIAN_POINT ( 'NONE',  ( 19.38216949554541202, 35.99863466993041072, 9.382169495545424454 ) ) ;
#96599 = ORIENTED_EDGE ( 'NONE', *, *, #33254, .F. ) ;
#96598 = CARTESIAN_POINT ( 'NONE',  ( 0.1532563361054083140, 1.008931151000784787, 1.131784320476157264E-15 ) ) ;
#96600 = CARTESIAN_POINT ( 'NONE',  ( 0.1532563361054100626, 25.80059781766744820, -2.638427012816831230 ) ) ;
#96601 = CARTESIAN_POINT ( 'NONE',  ( 17.08211943468705840, 65.13708216824730357, -12.26659068614894466 ) ) ;
#96602 = EDGE_LOOP ( 'NONE', ( #36441, #4720, #82311, #37423 ) ) ;
#96603 = CARTESIAN_POINT ( 'NONE',  ( 17.08211943468705840, 65.13708216824730357, -12.26659068614894466 ) ) ;
#96604 = ORIENTED_EDGE ( 'NONE', *, *, #88957, .F. ) ;
#96605 = CARTESIAN_POINT ( 'NONE',  ( 2.035157376598824452, 43.68868534415484106, 7.964842623401179544 ) ) ;
#96606 = CARTESIAN_POINT ( 'NONE',  ( 7.084665262690076126, 47.02201867748818387, -10.88017736071110164 ) ) ;
#96607 = CARTESIAN_POINT ( 'NONE',  ( 2.035157376598824452, 48.68868534415483396, 7.964842623401179544 ) ) ;
#96608 = LINE ( 'NONE', #74072, #4290 ) ;
#96609 = CARTESIAN_POINT ( 'NONE',  ( 12.91533473730993009, 46.60535201082150536, -10.88017736071109987 ) ) ;
#96610 = CARTESIAN_POINT ( 'NONE',  ( 20.15039907845753575, 65.60158574516643171, -6.262539305110073506 ) ) ;
#96612 = ORIENTED_EDGE ( 'NONE', *, *, #57903, .T. ) ;
#96611 = CARTESIAN_POINT ( 'NONE',  ( -8.900000000000002132, 80.99999999999994316, 0.000000000000000000 ) ) ;
#96613 =( GEOMETRIC_REPRESENTATION_CONTEXT ( 3 ) GLOBAL_UNCERTAINTY_ASSIGNED_CONTEXT ( ( #82465 ) ) GLOBAL_UNIT_ASSIGNED_CONTEXT ( ( #45837, #363, #90824 ) ) REPRESENTATION_CONTEXT ( 'NONE', 'WORKASPACE' ) );
#96614 = CARTESIAN_POINT ( 'NONE',  ( 17.20831665107776587, 32.88393115100078745, 7.208316651077764980 ) ) ;
#96615 = ORIENTED_EDGE ( 'NONE', *, *, #49353, .T. ) ;
#96616 = CARTESIAN_POINT ( 'NONE',  ( 12.63842701281683922, 64.55059781766745175, -9.846743663894590881 ) ) ;
#96617 = CARTESIAN_POINT ( 'NONE',  ( 0.000000000000000000, 15.00000000000000000, 0.000000000000000000 ) ) ;
#96618 = FILL_AREA_STYLE_COLOUR ( '', #68361 ) ;
#96619 = EDGE_LOOP ( 'NONE', ( #93962, #76941, #78037, #96439 ) ) ;
#96620 =( NAMED_UNIT ( * ) PLANE_ANGLE_UNIT ( ) SI_UNIT ( $, .RADIAN. ) );
#96621 = DIRECTION ( 'NONE',  ( -0.5519369853120501546, 0.000000000000000000, -0.8338858220671735433 ) ) ;
#96623 = CARTESIAN_POINT ( 'NONE',  ( 18.52753015748617571, 38.09226448433412315, 4.923371831947298993 ) ) ;
#96622 = DIRECTION ( 'NONE',  ( 0.7604059656000297096, 0.000000000000000000, 0.6494480483301851015 ) ) ;
#96624 = CARTESIAN_POINT ( 'NONE',  ( -2.266590686148945544, 62.22041550158063927, 7.082119434687048631 ) ) ;
#96625 = CARTESIAN_POINT ( 'NONE',  ( 18.17829156368510723, 64.16792564121900000, 6.499999999999953815 ) ) ;
#96626 = VERTEX_POINT ( 'NONE', #15868 ) ;
#96627 = DIRECTION ( 'NONE',  ( 0.000000000000000000, 0.000000000000000000, -1.000000000000000000 ) ) ;
#96628 = CARTESIAN_POINT ( 'NONE',  ( 1.472469842513823179, 31.42559781766745530, 4.923371831947296329 ) ) ;
#96629 = LINE ( 'NONE', #22105, #45131 ) ;
#96630 = CARTESIAN_POINT ( 'NONE',  ( 0.6178305044545818747, 8.498634669930421381, -9.382169495545419124 ) ) ;
#96631 = CARTESIAN_POINT ( 'NONE',  ( 7.361572987183169658, 4.967264484334119601, -9.846743663894592657 ) ) ;
#96632 = EDGE_CURVE ( 'NONE', #27349, #24643, #47322, .T. ) ;
#96633 = LINE ( 'NONE', #46084, #85706 ) ;
#96634 = CARTESIAN_POINT ( 'NONE',  ( 7.361572987183170547, 7.050597817667451750, 9.846743663894590881 ) ) ;
#96635 = CARTESIAN_POINT ( 'NONE',  ( 0.6178305044545818747, 3.498634669930420049, -9.382169495545419124 ) ) ;
#96636 = DIRECTION ( 'NONE',  ( -0.000000000000000000, -0.000000000000000000, -1.000000000000000000 ) ) ;
#96637 = CIRCLE ( 'NONE', #88614, 14.49999999999999822 ) ;
#96638 = ORIENTED_EDGE ( 'NONE', *, *, #94043, .T. ) ;
#96639 = CARTESIAN_POINT ( 'NONE',  ( 17.96484262340118221, 11.18868534415484106, -7.964842623401177768 ) ) ;
#96640 = CARTESIAN_POINT ( 'NONE',  ( 13.79529636645030344, 3.262082168247301350, 14.16423886937410614 ) ) ;
#96641 = CARTESIAN_POINT ( 'NONE',  ( 2.791683348922237240, 25.38393115100078390, -7.208316651077763204 ) ) ;
#96642 = CARTESIAN_POINT ( 'NONE',  ( 4.559911319644449179, 52.23035201082151247, -9.422509992056141925 ) ) ;
#96644 = PLANE ( 'NONE',  #20855 ) ;
#96643 = CARTESIAN_POINT ( 'NONE',  ( 3.591859063236761518, 29.95696800326375708, 11.09922568453594849 ) ) ;
#96645 = CARTESIAN_POINT ( 'NONE',  ( 20.88017736071110875, 5.772018677488170546, -2.915334737309920765 ) ) ;
#96646 = CARTESIAN_POINT ( 'NONE',  ( -9.972640495195461696, -0.03417435944610275333, 12.50695158660338890 ) ) ;
#96647 = CARTESIAN_POINT ( 'NONE',  ( -6.000000000000014211, 80.07179676972448590, 6.250000000000000000 ) ) ;
#96648 = CARTESIAN_POINT ( 'NONE',  ( 0.6178305044545838731, 4.748634669930420493, 9.382169495545420901 ) ) ;
#96649 = CARTESIAN_POINT ( 'NONE',  ( 2.791683348922237240, 60.38393115100078745, -7.208316651077763204 ) ) ;
#96650 = CARTESIAN_POINT ( 'NONE',  ( 14.92337183194729633, 12.67559781766745353, 8.527530157486181039 ) ) ;
#96651 = CARTESIAN_POINT ( 'NONE',  ( -9.422509992056136596, -31.51964798917848753, 5.440088680355559703 ) ) ;
#96652 = CARTESIAN_POINT ( 'NONE',  ( 13.43411237798105340, 25.58196800326374998, 12.81628187352647963 ) ) ;
#96653 = CARTESIAN_POINT ( 'NONE',  ( 1.492507162822262590, 52.19955587570481725, -6.500000000000077272 ) ) ;
#96654 = CARTESIAN_POINT ( 'NONE',  ( 2.035157376598822676, 27.43868534415483396, -7.964842623401177768 ) ) ;
#96655 = CARTESIAN_POINT ( 'NONE',  ( -6.599999999999995204, -97.00000000000000000, 3.750000000000000000 ) ) ;
#96656 = CIRCLE ( 'NONE', #63089, 15.00000000000000000 ) ;
#96657 = CARTESIAN_POINT ( 'NONE',  ( 24.16423886937410614, 54.51208216824730357, -3.795296366450302550 ) ) ;
#96658 = DIRECTION ( 'NONE',  ( 0.9914448613738104932, 0.000000000000000000, -0.1305261922200514901 ) ) ;
#96659 = CARTESIAN_POINT ( 'NONE',  ( 17.96484262340118221, 24.93868534415484461, 7.964842623401181321 ) ) ;
#96660 = CARTESIAN_POINT ( 'NONE',  ( 2.791683348922240793, 51.63393115100078745, 7.208316651077764092 ) ) ;
#96661 = ADVANCED_FACE ( 'NONE', ( #30851 ), #64395, .T. ) ;
#96662 = CARTESIAN_POINT ( 'NONE',  ( 15.44008868035555793, 51.39701867748816966, -9.422509992056140149 ) ) ;
#96663 = AXIS2_PLACEMENT_3D ( 'NONE', #29734, #92223, #53237 ) ;
#96664 = CARTESIAN_POINT ( 'NONE',  ( 2.917880565312948704, 32.63708216824730357, 12.26659068614894643 ) ) ;
#96665 = CARTESIAN_POINT ( 'NONE',  ( 4.838527690343618737, 15.00000000000000000, -14.19819177887726624 ) ) ;
#96666 = ADVANCED_FACE ( 'NONE', ( #85833 ), #77330, .F. ) ;
#96667 = CARTESIAN_POINT ( 'NONE',  ( 14.92337183194729633, 42.67559781766745886, 8.527530157486181039 ) ) ;
#96668 = CARTESIAN_POINT ( 'NONE',  ( -1.099225684535947600, 58.70696800326375353, -6.408140936763238038 ) ) ;
#96669 = CARTESIAN_POINT ( 'NONE',  ( 21.09922568453595559, 2.040301336597086568, -6.408140936763230044 ) ) ;
#96670 = VERTEX_POINT ( 'NONE', #69355 ) ;
#96671 = CARTESIAN_POINT ( 'NONE',  ( 12.91533473730992121, 24.52201867748816966, 10.88017736071110164 ) ) ;
#96672 = CARTESIAN_POINT ( 'NONE',  ( 19.88701968852525326, 11.79427333184086635, 6.480634945678620973 ) ) ;
#96673 = CARTESIAN_POINT ( 'NONE',  ( 19.42250999205614193, 5.147018677488171434, 5.440088680355555262 ) ) ;
#96674 = CARTESIAN_POINT ( 'NONE',  ( -0.8801773607111009756, 8.063685344154837509, 1.068504757029289695E-15 ) ) ;
#96675 = CARTESIAN_POINT ( 'NONE',  ( 2.035157376598824452, 63.68868534415484106, 7.964842623401179544 ) ) ;
#96676 = CARTESIAN_POINT ( 'NONE',  ( -0.3689425029237898834, 26.17874883491396432, -10.36894250292378850 ) ) ;
#96677 = CARTESIAN_POINT ( 'NONE',  ( 5.076628168052704559, 10.17559781766745175, -8.527530157486179263 ) ) ;
#96678 = CARTESIAN_POINT ( 'NONE',  ( 1.472469842513823179, 60.59226448433412315, -4.923371831947296329 ) ) ;
#96679 = CARTESIAN_POINT ( 'NONE',  ( 17.96484262340118221, 36.18868534415484106, -7.964842623401177768 ) ) ;
#96680 = TOROIDAL_SURFACE ( 'NONE', #23237, 14.49999999999999822, 0.5000000000000000000 ) ;
#96681 = CARTESIAN_POINT ( 'NONE',  ( -2.962741594152892510, -0.03417435944610275333, -13.93860331045676837 ) ) ;
#96682 = CARTESIAN_POINT ( 'NONE',  ( 8.209432707284868513, 0.3640475087720981828, -12.55409154915486525 ) ) ;
#96683 = ORIENTED_EDGE ( 'NONE', *, *, #72012, .F. ) ;
#96684 = VECTOR ( 'NONE', #59533, 1000.000000000000000 ) ;
#96685 = CARTESIAN_POINT ( 'NONE',  ( 4.130000000000002558, 1.019547802438462547, 2.500000000000000000 ) ) ;
#96686 = CARTESIAN_POINT ( 'NONE',  ( 5.076628168052704559, 50.17559781766745886, -8.527530157486179263 ) ) ;
#96687 = ORIENTED_EDGE ( 'NONE', *, *, #27413, .T. ) ;
#96688 = VERTEX_POINT ( 'NONE', #16847 ) ;
#96689 = CARTESIAN_POINT ( 'NONE',  ( -0.8801773607110990882, 62.85535201082149825, -2.915334737309924318 ) ) ;
#96690 = CARTESIAN_POINT ( 'NONE',  ( -4.164238869374099039, 26.80374883491397142, 8.674139862899312516E-16 ) ) ;
#96691 = CARTESIAN_POINT ( 'NONE',  ( 10.00000000000000000, 5.553748834913967869, -14.16423886937410082 ) ) ;
#96692 = CARTESIAN_POINT ( 'NONE',  ( 17.96484262340118221, 66.18868534415483396, -7.964842623401177768 ) ) ;
#96693 = CARTESIAN_POINT ( 'NONE',  ( 20.36894250292379738, 54.92874883491396076, -10.36894250292379027 ) ) ;
#96694 = CARTESIAN_POINT ( 'NONE',  ( 2.791683348922240793, 66.63393115100079456, 7.208316651077764092 ) ) ;
#96695 = CARTESIAN_POINT ( 'NONE',  ( 17.20831665107776587, 37.88393115100078745, 7.208316651077764980 ) ) ;
#96696 = CARTESIAN_POINT ( 'NONE',  ( -10.91898769996044827, -97.58648078763678768, 3.750000000000000000 ) ) ;
#96698 = CARTESIAN_POINT ( 'NONE',  ( 0.6178305044545838731, 4.748634669930420493, 9.382169495545420901 ) ) ;
#96697 = CARTESIAN_POINT ( 'NONE',  ( 12.91533473730993009, 31.60535201082150891, -10.88017736071109987 ) ) ;
#96699 = CARTESIAN_POINT ( 'NONE',  ( 20.36894250292379738, 19.92874883491396787, -10.36894250292379027 ) ) ;
#96700 = CARTESIAN_POINT ( 'NONE',  ( 24.16423886937409904, 54.09541550158063217, 3.795296366450317205 ) ) ;
#96701 = AXIS2_PLACEMENT_3D ( 'NONE', #59710, #96252, #97747 ) ;
#96702 = CARTESIAN_POINT ( 'NONE',  ( 12.91533473730993009, 16.60535201082150891, -10.88017736071109987 ) ) ;
#96703 = CARTESIAN_POINT ( 'NONE',  ( 14.48718990079890112, 15.00000000000000000, -0.6093675230840328583 ) ) ;
#96704 = CARTESIAN_POINT ( 'NONE',  ( 3.969999999999999751, 37.00000000000000000, -2.750000000000000000 ) ) ;
#96705 = CARTESIAN_POINT ( 'NONE',  ( 12.91533473730993009, 41.60535201082149825, -10.88017736071109987 ) ) ;
#96706 = CARTESIAN_POINT ( 'NONE',  ( -9.846743663894590881, -38.78273551566588395, 2.638427012816840111 ) ) ;
#96707 = ORIENTED_EDGE ( 'NONE', *, *, #94046, .F. ) ;
#96708 = DIRECTION ( 'NONE',  ( 0.000000000000000000, 1.000000000000000000, 0.000000000000000000 ) ) ;
#96709 = ORIENTED_EDGE ( 'NONE', *, *, #73587, .F. ) ;
#96710 = ORIENTED_EDGE ( 'NONE', *, *, #891, .F. ) ;
#96711 = CARTESIAN_POINT ( 'NONE',  ( 17.08211943468705130, 48.47041550158063927, 12.26659068614894998 ) ) ;
#96712 = CARTESIAN_POINT ( 'NONE',  ( 17.20831665107776587, 47.88393115100078745, 7.208316651077764980 ) ) ;
#96713 = CARTESIAN_POINT ( 'NONE',  ( 20.88017736071110875, 50.77201867748817676, -2.915334737309920765 ) ) ;
#96714 = EDGE_CURVE ( 'NONE', #60892, #27552, #74204, .T. ) ;
#96715 = PLANE ( 'NONE',  #86142 ) ;
#96716 = CARTESIAN_POINT ( 'NONE',  ( 17.96484262340118221, 51.18868534415483396, -7.964842623401177768 ) ) ;
#96717 = AXIS2_PLACEMENT_3D ( 'NONE', #69960, #1479, #70452 ) ;
#96718 = B_SPLINE_CURVE_WITH_KNOTS ( 'NONE', 3,
 ( #31173, #38213, #52699, #719, #16191, #98229 ),
 .UNSPECIFIED., .F., .F.,
 ( 4, 2, 4 ),
 ( 0.0002800338592613166202, 0.0006862394199319977583, 0.001092444980602678842 ),
 .UNSPECIFIED. ) ;
#96719 = CARTESIAN_POINT ( 'NONE',  ( -3.434112377981067610, 8.081968003263751754, -12.81628187352647252 ) ) ;
#96720 = ORIENTED_EDGE ( 'NONE', *, *, #1810, .F. ) ;
#96721 = CARTESIAN_POINT ( 'NONE',  ( 17.08211943468705130, 23.47041550158063572, 12.26659068614894998 ) ) ;
#96722 = CARTESIAN_POINT ( 'NONE',  ( 6.565887622018943937, 25.16530133659708213, 12.81628187352647430 ) ) ;
#96723 = VERTEX_POINT ( 'NONE', #38864 ) ;
#96724 = CARTESIAN_POINT ( 'NONE',  ( -2.816281873526473856, 44.33196800326375353, 3.434112377981055619 ) ) ;
#96725 = CARTESIAN_POINT ( 'NONE',  ( 20.88017736071110519, 15.56368534415483751, 2.639326808657452039E-16 ) ) ;
#96726 = CARTESIAN_POINT ( 'NONE',  ( 5.076628168052704559, 35.17559781766745175, -8.527530157486179263 ) ) ;
#96727 = CARTESIAN_POINT ( 'NONE',  ( 2.035157376598822676, 12.43868534415483751, -7.964842623401177768 ) ) ;
#96728 = CARTESIAN_POINT ( 'NONE',  ( 10.00000000000000178, 55.37363466993042493, 12.81628187352647608 ) ) ;
#96729 = PLANE ( 'NONE',  #36825 ) ;
#96730 = CARTESIAN_POINT ( 'NONE',  ( 7.361572987183170547, 42.05059781766745886, 9.846743663894590881 ) ) ;
#96731 = CIRCLE ( 'NONE', #26476, 0.2500000000000002220 ) ;
#96733 = ORIENTED_EDGE ( 'NONE', *, *, #17431, .T. ) ;
#96732 = DIRECTION ( 'NONE',  ( -3.730349362740526607E-14, 0.000000000000000000, 1.000000000000000000 ) ) ;
#96734 = AXIS2_PLACEMENT_3D ( 'NONE', #43291, #65291, #35294 ) ;
#96735 = CARTESIAN_POINT ( 'NONE',  ( -0.03932841506543251903, 3.121614419605014401, 6.397827110478961465 ) ) ;
#96736 = CARTESIAN_POINT ( 'NONE',  ( 2.603489959281582777, 31.58210964143329136, 6.499999999999995559 ) ) ;
#96737 = DIRECTION ( 'NONE',  ( 1.000000000000000000, 0.000000000000000000, 0.000000000000000000 ) ) ;
#96738 = CARTESIAN_POINT ( 'NONE',  ( 2.849309504156536832, 0.000000000000000000, -4.649650521509789414 ) ) ;
#96739 = CARTESIAN_POINT ( 'NONE',  ( 10.00000000000000000, 19.75893115100078390, -9.846743663894594434 ) ) ;
#96740 = CARTESIAN_POINT ( 'NONE',  ( 16.40814093676324603, 22.45696800326375353, -11.09922568453594671 ) ) ;
#96741 = FILL_AREA_STYLE_COLOUR ( '', #13174 ) ;
#96742 = VERTEX_POINT ( 'NONE', #78317 ) ;
#96743 = CARTESIAN_POINT ( 'NONE',  ( -9.520529577030568902, 4.404571325722360777E-16, 11.10395710204414499 ) ) ;
#96744 = CARTESIAN_POINT ( 'NONE',  ( 20.36894250292379382, 18.67874883491397142, 10.36894250292379205 ) ) ;
#96745 = CARTESIAN_POINT ( 'NONE',  ( 12.63842701281683922, 49.55059781766744464, -9.846743663894590881 ) ) ;
#96746 = CARTESIAN_POINT ( 'NONE',  ( -2.816281873526473856, 44.12363466993042493, 9.499525473075851096E-16 ) ) ;
#96748 = CARTESIAN_POINT ( 'NONE',  ( 1.042145700049407431, 9.742161081720029259, -6.499999999999879208 ) ) ;
#96747 = DIRECTION ( 'NONE',  ( 0.000000000000000000, -1.000000000000000000, 0.000000000000000000 ) ) ;
#96749 = CARTESIAN_POINT ( 'NONE',  ( 19.42250999205614548, 65.98035201082151957, -5.440088680355545492 ) ) ;
#96750 = DIRECTION ( 'NONE',  ( 1.000000000000000000, 1.273191542001295551E-15, 0.000000000000000000 ) ) ;
#96751 = CARTESIAN_POINT ( 'NONE',  ( 14.92337183194729633, 32.67559781766745175, 8.527530157486181039 ) ) ;
#96752 = CARTESIAN_POINT ( 'NONE',  ( 12.91533473730992121, 34.52201867748817676, 10.88017736071110164 ) ) ;
#96753 = EDGE_CURVE ( 'NONE', #21313, #58402, #23869, .T. ) ;
#96754 = CARTESIAN_POINT ( 'NONE',  ( -1.099225684535947600, 39.54030133659708923, 6.408140936763237150 ) ) ;
#96755 = COLOUR_RGB ( '', 0.40784314, 0.44705882, 0.49803922) ;
#96756 = CARTESIAN_POINT ( 'NONE',  ( 2.791683348922240793, 31.63393115100078745, 7.208316651077764092 ) ) ;
#96757 = DIRECTION ( 'NONE',  ( -0.000000000000000000, -0.000000000000000000, 1.000000000000000000 ) ) ;
#96758 = PRESENTATION_LAYER_ASSIGNMENT (  '', '', ( #77599 ) ) ;
#96759 = VECTOR ( 'NONE', #14862, 1000.000000000000114 ) ;
#96760 = CARTESIAN_POINT ( 'NONE',  ( 10.00000000000000178, 34.31368534415484106, 10.88017736071110342 ) ) ;
#96761 = VECTOR ( 'NONE', #88923, 1000.000000000000000 ) ;
#96762 = ORIENTED_EDGE ( 'NONE', *, *, #39416, .F. ) ;
#96763 = FACE_OUTER_BOUND ( 'NONE', #56122, .T. ) ;
#96764 = CARTESIAN_POINT ( 'NONE',  ( 20.88017736071110875, 15.77201867748817143, -2.915334737309920765 ) ) ;
#96766 = CARTESIAN_POINT ( 'NONE',  ( 17.96484262340118221, 41.18868534415484106, -7.964842623401177768 ) ) ;
#96765 = CARTESIAN_POINT ( 'NONE',  ( 7.361572987183170547, 62.05059781766745886, 9.846743663894590881 ) ) ;
#96767 = CARTESIAN_POINT ( 'NONE',  ( 0.000000000000000000, 0.5000000000000004441, 0.000000000000000000 ) ) ;
#96768 = CARTESIAN_POINT ( 'NONE',  ( 10.00000000000000178, 59.31368534415484106, 10.88017736071110342 ) ) ;
#96769 = CARTESIAN_POINT ( 'NONE',  ( 20.88017736071110875, 25.77201867748816966, -2.915334737309920765 ) ) ;
#96770 = CARTESIAN_POINT ( 'NONE',  ( 17.20831665107776587, 4.133931151000785675, -7.208316651077762316 ) ) ;
#96771 = CARTESIAN_POINT ( 'NONE',  ( 18.52753015748617571, 18.09226448433411960, 4.923371831947298993 ) ) ;
#96772 = FACE_OUTER_BOUND ( 'NONE', #9269, .T. ) ;
#96773 = CARTESIAN_POINT ( 'NONE',  ( 14.16423886937410082, 9.512082168247301794, -3.795296366450314096 ) ) ;
#96774 = CARTESIAN_POINT ( 'NONE',  ( 2.791683348922237240, 45.38393115100079456, -7.208316651077763204 ) ) ;
#96776 = PRESENTATION_STYLE_ASSIGNMENT (( #73252 ) ) ;
#96775 = CARTESIAN_POINT ( 'NONE',  ( 20.36894250292379382, 53.67874883491397497, 10.36894250292379205 ) ) ;
#96777 = CYLINDRICAL_SURFACE ( 'NONE', #35406, 0.2499999999999997780 ) ;
#96778 = CARTESIAN_POINT ( 'NONE',  ( 17.08211943468705130, 8.470415501580635720, 12.26659068614894998 ) ) ;
#96779 = CARTESIAN_POINT ( 'NONE',  ( -0.3689425029237881626, 42.42874883491396787, 10.36894250292379027 ) ) ;
#96780 = CARTESIAN_POINT ( 'NONE',  ( 0.6178305044545818747, -1.501365330069579951, -9.382169495545419124 ) ) ;
#96781 = ORIENTED_EDGE ( 'NONE', *, *, #88065, .T. ) ;
#96782 = EDGE_CURVE ( 'NONE', #95488, #13782, #54332, .T. ) ;
#96783 = CARTESIAN_POINT ( 'NONE',  ( 20.88017736071110164, 10.35535201082150714, 2.915334737309930979 ) ) ;
#96784 = CARTESIAN_POINT ( 'NONE',  ( 10.00000000000000000, 29.75893115100078745, -9.846743663894594434 ) ) ;
#96786 = CARTESIAN_POINT ( 'NONE',  ( -8.000000000000000000, 80.99999999999994316, 0.000000000000000000 ) ) ;
#96785 = CARTESIAN_POINT ( 'NONE',  ( 0.000000000000000000, 14.49999999999999822, 0.000000000000000000 ) ) ;
#96787 = SURFACE_STYLE_FILL_AREA ( #20773 ) ;
#96788 = CARTESIAN_POINT ( 'NONE',  ( 18.52753015748618282, 3.925597817667451306, -4.923371831947291888 ) ) ;
#96789 = CARTESIAN_POINT ( 'NONE',  ( 3.591859063236763294, 18.29030133659708568, -11.09922568453595026 ) ) ;
#96790 = CARTESIAN_POINT ( 'NONE',  ( 10.00000000000000000, 24.75893115100078745, -9.846743663894594434 ) ) ;
#96792 = ORIENTED_EDGE ( 'NONE', *, *, #65690, .F. ) ;
#96791 = EDGE_CURVE ( 'NONE', #2489, #71703, #86323, .T. ) ;
#96793 = CARTESIAN_POINT ( 'NONE',  ( 10.00000000000000000, 14.75893115100078568, -9.846743663894594434 ) ) ;
#96794 = CARTESIAN_POINT ( 'NONE',  ( -12.84737282370062061, -0.03417435944610275333, -9.530079116402557560 ) ) ;
#96795 = CARTESIAN_POINT ( 'NONE',  ( 20.36894250292379382, 63.67874883491396787, 10.36894250292379205 ) ) ;
#96796 = CARTESIAN_POINT ( 'NONE',  ( 0.5774900079438607392, 13.48035201082150358, 5.440088680355550821 ) ) ;
#96797 = CARTESIAN_POINT ( 'NONE',  ( -2.266590686148945544, 41.38708216824729647, -7.082119434687050408 ) ) ;
#96798 = CARTESIAN_POINT ( 'NONE',  ( 7.084665262690076126, 47.02201867748818387, -10.88017736071110164 ) ) ;
#96799 = CARTESIAN_POINT ( 'NONE',  ( 15.44008868035555793, 56.39701867748817676, -9.422509992056140149 ) ) ;
#96800 = CARTESIAN_POINT ( 'NONE',  ( 8.564643372776615138, 0.5000000000000004441, -12.31449893000740836 ) ) ;
#96801 = DIRECTION ( 'NONE',  ( 0.9914448613738104932, 0.000000000000000000, -0.1305261922200514901 ) ) ;
#96802 = CARTESIAN_POINT ( 'NONE',  ( 18.52753015748617571, 28.09226448433411960, 4.923371831947298993 ) ) ;
#96803 = SURFACE_STYLE_USAGE ( .BOTH. , #51279 ) ;
#96804 = CARTESIAN_POINT ( 'NONE',  ( 7.361572987183170547, 12.05059781766744997, 9.846743663894590881 ) ) ;
#96805 = CARTESIAN_POINT ( 'NONE',  ( 17.20831665107776587, 32.88393115100078745, 7.208316651077764980 ) ) ;
#96806 = CARTESIAN_POINT ( 'NONE',  ( 19.84674366389459266, 63.30059781766745886, 2.638427012816836559 ) ) ;
#96807 = PRESENTATION_LAYER_ASSIGNMENT (  '', '', ( #98462 ) ) ;
#96808 = AXIS2_PLACEMENT_3D ( 'NONE', #73110, #73607, #35112 ) ;
#96809 = CARTESIAN_POINT ( 'NONE',  ( 19.42250999205614193, 35.14701867748816966, 5.440088680355555262 ) ) ;
#96810 = ORIENTED_EDGE ( 'NONE', *, *, #7017, .F. ) ;
#96811 = CARTESIAN_POINT ( 'NONE',  ( 22.81628187352647785, 61.62363466993041783, 6.195893100308588602E-16 ) ) ;
#96812 =( NAMED_UNIT ( * ) PLANE_ANGLE_UNIT ( ) SI_UNIT ( $, .RADIAN. ) );
#96813 = CARTESIAN_POINT ( 'NONE',  ( 4.559911319644449179, 63.89701867748817676, 9.422509992056141925 ) ) ;
#96814 = CARTESIAN_POINT ( 'NONE',  ( 16.40814093676324603, 42.45696800326375353, -11.09922568453594671 ) ) ;
#96816 = CARTESIAN_POINT ( 'NONE',  ( 17.20831665107776587, 29.13393115100078390, -7.208316651077762316 ) ) ;
#96815 = CARTESIAN_POINT ( 'NONE',  ( 2.917880565312948704, 62.63708216824730357, 12.26659068614894643 ) ) ;
#96817 = CARTESIAN_POINT ( 'NONE',  ( -19.92076923076924189, 82.65384615384614619, -9.500000000000000000 ) ) ;
#96818 = CARTESIAN_POINT ( 'NONE',  ( 7.361572987183170547, 62.05059781766745886, 9.846743663894590881 ) ) ;
#96819 = CARTESIAN_POINT ( 'NONE',  ( 2.917880565312950480, 20.97041550158063217, -12.26659068614894821 ) ) ;
#96820 = CARTESIAN_POINT ( 'NONE',  ( 20.36894250292379382, 38.67874883491396076, 10.36894250292379205 ) ) ;
#96821 = CARTESIAN_POINT ( 'NONE',  ( 10.00000000000000178, 42.25893115100078745, 9.846743663894594434 ) ) ;
#96822 = DIRECTION ( 'NONE',  ( 0.000000000000000000, -1.000000000000000000, 0.000000000000000000 ) ) ;
#96823 = CARTESIAN_POINT ( 'NONE',  ( 4.559911319644449179, 32.23035201082150536, -9.422509992056141925 ) ) ;
#96824 = CARTESIAN_POINT ( 'NONE',  ( 2.035157376598822676, 62.43868534415483396, -7.964842623401177768 ) ) ;
#96825 = CARTESIAN_POINT ( 'NONE',  ( -0.1082834614903535886, 0.1165887514553498872, 6.323045919668897952 ) ) ;
#96826 = ORIENTED_EDGE ( 'NONE', *, *, #74961, .T. ) ;
#96827 = CARTESIAN_POINT ( 'NONE',  ( 22.81628187352648496, 46.83196800326376064, -3.434112377981050290 ) ) ;
#96828 = ORIENTED_EDGE ( 'NONE', *, *, #54303, .T. ) ;
#96829 = CARTESIAN_POINT ( 'NONE',  ( 2.035157376598822676, 67.43868534415484817, -7.964842623401177768 ) ) ;
#96830 = ORIENTED_EDGE ( 'NONE', *, *, #15869, .F. ) ;
#96831 = CARTESIAN_POINT ( 'NONE',  ( 6.204703633549690345, 7.845415501580634832, 14.16423886937410082 ) ) ;
#96832 = CARTESIAN_POINT ( 'NONE',  ( 14.92337183194729633, 2.675597817667451750, 8.527530157486181039 ) ) ;
#96833 = ADVANCED_FACE ( 'NONE', ( #54822 ), #51855, .T. ) ;
#96834 = DIRECTION ( 'NONE',  ( -0.6755902076156540259, 0.000000000000000000, -0.7372773368101297464 ) ) ;
#96835 = VECTOR ( 'NONE', #10660, 999.9999999999998863 ) ;
#96836 = EDGE_LOOP ( 'NONE', ( #60155, #33020, #47088, #47955 ) ) ;
#96837 = VECTOR ( 'NONE', #34816, 1000.000000000000114 ) ;
#96838 = CARTESIAN_POINT ( 'NONE',  ( -0.8801773607110991993, 12.85535201082150358, -2.915334737309923874 ) ) ;
#96839 = CARTESIAN_POINT ( 'NONE',  ( 17.39651004071841456, 9.082109641433294911, -6.500000000000003553 ) ) ;
#96840 = CARTESIAN_POINT ( 'NONE',  ( -2.266590686148945544, 22.22041550158063572, 7.082119434687048631 ) ) ;
#96841 = AXIS2_PLACEMENT_3D ( 'NONE', #93275, #86276, #10279 ) ;
#96842 = ORIENTED_EDGE ( 'NONE', *, *, #2891, .F. ) ;
#96843 = CARTESIAN_POINT ( 'NONE',  ( 4.559911319644449179, 23.89701867748817321, 9.422509992056141925 ) ) ;
#96844 = CARTESIAN_POINT ( 'NONE',  ( 0.1532563361054083140, 56.00893115100078745, 1.131784320476157264E-15 ) ) ;
#96845 = ORIENTED_EDGE ( 'NONE', *, *, #6639, .F. ) ;
#96846 = CARTESIAN_POINT ( 'NONE',  ( 0.1532563361054083140, 56.00893115100078745, 1.131784320476157264E-15 ) ) ;
#96847 = ORIENTED_EDGE ( 'NONE', *, *, #63090, .T. ) ;
#96848 = CARTESIAN_POINT ( 'NONE',  ( 4.559911319644449179, 67.23035201082150536, -9.422509992056141925 ) ) ;
#96849 = CARTESIAN_POINT ( 'NONE',  ( 7.361572987183169658, 59.96726448433410894, -9.846743663894592657 ) ) ;
#96851 = CARTESIAN_POINT ( 'NONE',  ( 0.000000000000000000, 15.00000000000000000, 0.000000000000000000 ) ) ;
#96850 = CARTESIAN_POINT ( 'NONE',  ( 0.5774900079438590739, 12.64701867748817143, -5.440088680355550821 ) ) ;
#96852 = CARTESIAN_POINT ( 'NONE',  ( 19.84674366389459266, 3.300597817667451750, 2.638427012816836559 ) ) ;
#96853 = CARTESIAN_POINT ( 'NONE',  ( -0.8801773607110991993, 22.85535201082150181, -2.915334737309923874 ) ) ;
#96854 = TOROIDAL_SURFACE ( 'NONE', #5835, 14.49999999999999822, 0.5000000000000000000 ) ;
#96855 = MECHANICAL_DESIGN_GEOMETRIC_PRESENTATION_REPRESENTATION (  '', ( #80921 ), #42594 ) ;
#96856 = ORIENTED_EDGE ( 'NONE', *, *, #37300, .T. ) ;
#96857 = AXIS2_PLACEMENT_3D ( 'NONE', #22108, #14620, #43115 ) ;
#96858 = CARTESIAN_POINT ( 'NONE',  ( 4.559911319644449179, 38.89701867748817676, 9.422509992056141925 ) ) ;
#96859 = CARTESIAN_POINT ( 'NONE',  ( 17.75000000000000000, 84.07179676972448590, -3.750000000000000000 ) ) ;
#96860 = CARTESIAN_POINT ( 'NONE',  ( 22.81628187352647785, 36.62363466993041783, 6.195893100308588602E-16 ) ) ;
#96861 = CARTESIAN_POINT ( 'NONE',  ( 2.035157376598824452, 53.68868534415484817, 7.964842623401179544 ) ) ;
#96862 = CARTESIAN_POINT ( 'NONE',  ( 14.92337183194729633, 57.67559781766745886, 8.527530157486181039 ) ) ;
#96863 = ORIENTED_EDGE ( 'NONE', *, *, #28457, .T. ) ;
#96864 = CARTESIAN_POINT ( 'NONE',  ( 0.1955144967548773649, 49.32703681773342197, -6.500000000002692957 ) ) ;
#96865 = CARTESIAN_POINT ( 'NONE',  ( 19.84674366389459266, 23.71726448433412315, -2.638427012816827677 ) ) ;
#96866 = CARTESIAN_POINT ( 'NONE',  ( 13.43411237798106583, 12.66530133659708746, -12.81628187352647252 ) ) ;
#96868 = CARTESIAN_POINT ( 'NONE',  ( -7.313705784284733724, 14.49999999999999112, 13.09617149020743199 ) ) ;
#96867 = CARTESIAN_POINT ( 'NONE',  ( -13.78553237914111129, 90.91070185254878311, -7.842545424067505877 ) ) ;
#96869 = CARTESIAN_POINT ( 'NONE',  ( 10.00000000000000178, 19.31368534415484106, 10.88017736071110342 ) ) ;
#96870 = CARTESIAN_POINT ( 'NONE',  ( 18.52753015748618282, 53.92559781766745175, -4.923371831947291888 ) ) ;
#96871 = CARTESIAN_POINT ( 'NONE',  ( 0.000000000000000000, 15.00000000000000000, 0.000000000000000000 ) ) ;
#96872 = AXIS2_PLACEMENT_3D ( 'NONE', #26976, #87968, #34466 ) ;
#96873 = CARTESIAN_POINT ( 'NONE',  ( 10.00000000000000178, 7.258931151000785675, 9.846743663894594434 ) ) ;
#96874 = CARTESIAN_POINT ( 'NONE',  ( 18.04007052943791933, 29.00257860105346097, -5.767676674365512568 ) ) ;
#96875 = EDGE_CURVE ( 'NONE', #86520, #23897, #64601, .T. ) ;
#96877 = ORIENTED_EDGE ( 'NONE', *, *, #56988, .F. ) ;
#96876 = CARTESIAN_POINT ( 'NONE',  ( 21.09922568453594849, 1.206968003263753531, 6.408140936763242479 ) ) ;
#96878 = CARTESIAN_POINT ( 'NONE',  ( -10.91061041304835300, 14.76930270348882068, 10.20767530377041332 ) ) ;
#96879 = DIRECTION ( 'NONE',  ( -0.000000000000000000, -1.000000000000000000, -0.000000000000000000 ) ) ;
#96880 = CARTESIAN_POINT ( 'NONE',  ( 22.81628187352647785, 36.41530133659707502, 3.434112377981063169 ) ) ;
#96881 = CARTESIAN_POINT ( 'NONE',  ( 5.076628168052703671, 31.84226448433412315, 8.527530157486179263 ) ) ;
#96882 = CARTESIAN_POINT ( 'NONE',  ( 3.014428414850129911, 8.659700295649312096, -11.25000000000000000 ) ) ;
#96884 = EDGE_CURVE ( 'NONE', #12573, #43815, #96294, .T. ) ;
#96883 = CARTESIAN_POINT ( 'NONE',  ( 22.26659068614894466, 53.88708216824731068, 7.082119434687054849 ) ) ;
#96885 = CARTESIAN_POINT ( 'NONE',  ( 17.20831665107776587, 32.88393115100078745, 7.208316651077764980 ) ) ;
#96886 = TOROIDAL_SURFACE ( 'NONE', #93722, 2.500000000000001776, 0.5000000000000000000 ) ;
#96887 = FACE_OUTER_BOUND ( 'NONE', #49267, .T. ) ;
#96888 = CARTESIAN_POINT ( 'NONE',  ( 7.084665262690076126, 7.022018677488170546, -10.88017736071110164 ) ) ;
#96889 = DIRECTION ( 'NONE',  ( 1.000000000000000000, 0.000000000000000000, 0.000000000000000000 ) ) ;
#96890 = CARTESIAN_POINT ( 'NONE',  ( -0.8801773607111009756, 13.06368534415483929, 1.068504757029289695E-15 ) ) ;
#96891 = CARTESIAN_POINT ( 'NONE',  ( 20.36894250292379382, 53.67874883491397497, 10.36894250292379205 ) ) ;
#96892 = CARTESIAN_POINT ( 'NONE',  ( -2.266590686148945544, 46.38708216824730357, -7.082119434687050408 ) ) ;
#96893 =( BOUNDED_CURVE ( )  B_SPLINE_CURVE ( 2, ( #62242, #76759, #47239, #94218, #93234, #77741, #78235, #17263, #2272 ),
 .UNSPECIFIED., .F., .T. ) 
 B_SPLINE_CURVE_WITH_KNOTS ( ( 3, 2, 2, 2, 3 ),
 ( 0.5472837940830884707, 0.5476190476190476719, 0.5535714285714286031, 0.5595238095238095344, 0.5598590630597686246 ),
 .UNSPECIFIED. ) 
 CURVE ( )  GEOMETRIC_REPRESENTATION_ITEM ( )  RATIONAL_B_SPLINE_CURVE ( ( 0.9963778908391753841, 0.9980808541467917072, 1.000000000000000000, 0.9659258262890682012, 1.000000000000000000, 0.9659258262890682012, 1.000000000000000000, 0.9980808541467922623, 0.9963778908391764944 ) ) 
 REPRESENTATION_ITEM ( '' )  );
#96894 = CARTESIAN_POINT ( 'NONE',  ( 10.00000000000000178, 7.258931151000785675, 9.846743663894594434 ) ) ;
#96895 = CARTESIAN_POINT ( 'NONE',  ( 18.52753015748617571, 63.09226448433412315, 4.923371831947298993 ) ) ;
#96896 = CARTESIAN_POINT ( 'NONE',  ( 17.96484262340118221, 44.93868534415483396, 7.964842623401181321 ) ) ;
#96897 = DIRECTION ( 'NONE',  ( 1.000000000000000000, 1.257402221000611116E-16, -0.000000000000000000 ) ) ;
#96898 = CARTESIAN_POINT ( 'NONE',  ( 1.472469842513823179, 61.42559781766745175, 4.923371831947296329 ) ) ;
#96899 = CARTESIAN_POINT ( 'NONE',  ( 0.000000000000000000, 0.5000000000000004441, 0.000000000000000000 ) ) ;
#96900 = VECTOR ( 'NONE', #80268, 1000.000000000000000 ) ;
#96901 = CARTESIAN_POINT ( 'NONE',  ( 1.472469842513823179, 65.59226448433412315, -4.923371831947296329 ) ) ;
#96902 = CARTESIAN_POINT ( 'NONE',  ( 10.00000000000000178, 3.053748834913967425, 14.16423886937410082 ) ) ;
#96903 = CARTESIAN_POINT ( 'NONE',  ( -9.347645168806021587, 88.42200471242378512, 5.276767730577756055 ) ) ;
#96904 = CARTESIAN_POINT ( 'NONE',  ( 22.26659068614894466, 33.88708216824730357, 7.082119434687054849 ) ) ;
#96905 = B_SPLINE_SURFACE_WITH_KNOTS ( 'NONE', 3, 1, ( 
 ( #5139, #13122 ),
 ( #43618, #90593 ),
 ( #59606, #28620 ),
 ( #82607, #35630 ),
 ( #67620, #98128 ),
 ( #60091, #22120 ),
 ( #52600, #14631 ),
 ( #20129, #50633 ),
 ( #38598, #133 ),
 ( #78066, #68605 ),
 ( #69096, #62555 ),
 ( #60595, #47063 ),
 ( #31568, #54562 ),
 ( #62064, #76094 ),
 ( #76582, #61574 ),
 ( #53585, #32052 ),
 ( #38116, #39590 ),
 ( #46098, #8102 ) ),
 .UNSPECIFIED., .F., .F., .F.,
 ( 4, 2, 2, 2, 2, 2, 2, 2, 4 ),
 ( 2, 2 ),
 ( 0.000000000000000000, 0.06249999999999988898, 0.1249999999999998890, 0.2499999999999997780, 0.4999999999999994449, 0.5624999999999994449, 0.6249999999999994449, 0.7499999999999995559, 0.8570805329376184334 ),
 ( 0.000000000000000000, 1.000000000000000000 ),
 .UNSPECIFIED. ) ;
#96906 = AXIS2_PLACEMENT_3D ( 'NONE', #73097, #11624, #35606 ) ;
#96907 = CARTESIAN_POINT ( 'NONE',  ( 0.1532563361054100626, 0.8005978176674514168, -2.638427012816831230 ) ) ;
#96909 = CARTESIAN_POINT ( 'NONE',  ( -9.742785792574940373, 7.505135511184873209, -5.624999999999991118 ) ) ;
#96908 = DIRECTION ( 'NONE',  ( 0.9914448613738084948, 0.000000000000000000, 0.1305261922200653124 ) ) ;
#96910 = CARTESIAN_POINT ( 'NONE',  ( 10.00000000000000178, 39.31368534415484106, 10.88017736071110342 ) ) ;
#96911 = CARTESIAN_POINT ( 'NONE',  ( 0.6178305044545838731, 44.74863466993042493, 9.382169495545420901 ) ) ;
#96912 = CARTESIAN_POINT ( 'NONE',  ( 0.6178305044545818747, 28.49863466993041783, -9.382169495545419124 ) ) ;
#96913 = CARTESIAN_POINT ( 'NONE',  ( 13.43411237798106583, 62.66530133659708923, -12.81628187352647252 ) ) ;
#96915 = ADVANCED_FACE ( 'NONE', ( #56797 ), #95794, .F. ) ;
#96914 = EDGE_LOOP ( 'NONE', ( #5123, #19038, #74081, #30985, #1318, #11502 ) ) ;
#96916 = DIRECTION ( 'NONE',  ( -2.569960705150826877E-16, 1.000000000000000000, 0.000000000000000000 ) ) ;
#96917 = DIRECTION ( 'NONE',  ( -5.818595309480553908E-17, -1.000000000000000000, -0.000000000000000000 ) ) ;
#96918 = CARTESIAN_POINT ( 'NONE',  ( 13.79529636645031943, 30.34541550158063927, -14.16423886937409904 ) ) ;
#96919 = CARTESIAN_POINT ( 'NONE',  ( 1.354709868695515684, 15.00000000000000000, 14.93870011653152652 ) ) ;
#96920 = CARTESIAN_POINT ( 'NONE',  ( 20.88017736071110164, 20.35535201082150891, 2.915334737309930979 ) ) ;
#96921 = CARTESIAN_POINT ( 'NONE',  ( -7.750000000000000000, 1.019547802438466100, 3.750000000000000000 ) ) ;
#96922 = CARTESIAN_POINT ( 'NONE',  ( 0.5774900079438607392, 58.48035201082151247, 5.440088680355550821 ) ) ;
#96923 = CARTESIAN_POINT ( 'NONE',  ( 10.00000000000000000, 51.81368534415484106, -10.88017736071110342 ) ) ;
#96924 = CARTESIAN_POINT ( 'NONE',  ( 3.591859063236761518, 9.956968003263753531, 11.09922568453594849 ) ) ;
#96925 = CARTESIAN_POINT ( 'NONE',  ( -0.03932841506541961962, 48.12161441960502373, 6.397827110479001433 ) ) ;
#96926 = CARTESIAN_POINT ( 'NONE',  ( 64.56412365047461321, 29.50000000000000000, 10.00000000000000000 ) ) ;
#96927 = CARTESIAN_POINT ( 'NONE',  ( 5.076628168052703671, 16.84226448433411960, 8.527530157486179263 ) ) ;
#96928 = VECTOR ( 'NONE', #21409, 1000.000000000000227 ) ;
#96929 = DIRECTION ( 'NONE',  ( -0.000000000000000000, -0.000000000000000000, -1.000000000000000000 ) ) ;
#96930 = CARTESIAN_POINT ( 'NONE',  ( 10.00000000000000000, 41.81368534415484106, -10.88017736071110342 ) ) ;
#96931 = VECTOR ( 'NONE', #10106, 1000.000000000000114 ) ;
#96932 = CIRCLE ( 'NONE', #71374, 6.349999999999995204 ) ;
#96933 = CARTESIAN_POINT ( 'NONE',  ( 13.43411237798105340, 5.581968003263753531, 12.81628187352647963 ) ) ;
#96934 = CARTESIAN_POINT ( 'NONE',  ( 0.5774900079438607392, 43.48035201082151247, 5.440088680355550821 ) ) ;
#96935 = CARTESIAN_POINT ( 'NONE',  ( 12.63842701281683922, 29.55059781766745175, -9.846743663894590881 ) ) ;
#96936 = CARTESIAN_POINT ( 'NONE',  ( 21.09922568453594849, 51.20696800326375353, 6.408140936763242479 ) ) ;
#96938 = SURFACE_STYLE_USAGE ( .BOTH. , #43894 ) ;
#96937 = CARTESIAN_POINT ( 'NONE',  ( 7.361572987183169658, 24.96726448433412315, -9.846743663894592657 ) ) ;
#96939 = ORIENTED_EDGE ( 'NONE', *, *, #79732, .T. ) ;
#96940 = CARTESIAN_POINT ( 'NONE',  ( -4.164238869374099039, 1.803748834913967647, 8.674139862899312516E-16 ) ) ;
#96941 = DIRECTION ( 'NONE',  ( 0.8320502943378436100, -0.5547001962252291474, 0.000000000000000000 ) ) ;
#96942 = CARTESIAN_POINT ( 'NONE',  ( 4.559911319644449179, 22.23035201082150536, -9.422509992056141925 ) ) ;
#96944 = CARTESIAN_POINT ( 'NONE',  ( 20.36894250292379382, 33.67874883491396076, 10.36894250292379205 ) ) ;
#96943 = DIRECTION ( 'NONE',  ( 0.9483236552062023206, 0.000000000000000000, -0.3173046564050834295 ) ) ;
#96945 = CARTESIAN_POINT ( 'NONE',  ( 10.00000000000000178, 32.25893115100078745, 9.846743663894594434 ) ) ;
#96946 = CARTESIAN_POINT ( 'NONE',  ( 4.559911319644449179, 18.89701867748817321, 9.422509992056141925 ) ) ;
#96947 = CARTESIAN_POINT ( 'NONE',  ( 24.16423886937410614, 64.30374883491396076, 8.672049930838204340E-16 ) ) ;
#96948 = ORIENTED_EDGE ( 'NONE', *, *, #6450, .T. ) ;
#96949 = PRESENTATION_LAYER_ASSIGNMENT (  '', '', ( #69809 ) ) ;
#96950 = CARTESIAN_POINT ( 'NONE',  ( 12.91533473730993009, 21.60535201082150536, -10.88017736071109987 ) ) ;
#96951 = ADVANCED_FACE ( 'NONE', ( #18812 ), #4392, .T. ) ;
#96952 = CARTESIAN_POINT ( 'NONE',  ( 0.5774900079438607392, 38.48035201082150536, 5.440088680355550821 ) ) ;
#96953 = CARTESIAN_POINT ( 'NONE',  ( -2.962741594153171842, -0.03417435944610275333, 13.93860331045670975 ) ) ;
#96954 = ORIENTED_EDGE ( 'NONE', *, *, #37571, .F. ) ;
#96955 = CARTESIAN_POINT ( 'NONE',  ( 12.63842701281683922, 59.55059781766744464, -9.846743663894590881 ) ) ;
#96956 = CARTESIAN_POINT ( 'NONE',  ( 19.42250999205614193, 40.14701867748817676, 5.440088680355555262 ) ) ;
#96957 = CARTESIAN_POINT ( 'NONE',  ( 4.380000000000000782, 1.019547802438464545, 3.750000000000000000 ) ) ;
#96958 = CARTESIAN_POINT ( 'NONE',  ( 3.969999999999999751, 10.00000000000000000, 3.750000000000000000 ) ) ;
#96959 = CARTESIAN_POINT ( 'NONE',  ( 0.6178305044545838731, 64.74863466993043914, 9.382169495545420901 ) ) ;
#96960 = CARTESIAN_POINT ( 'NONE',  ( 14.99999999999997868, 80.07179676972448590, -6.250000000000000000 ) ) ;
#96961 = CARTESIAN_POINT ( 'NONE',  ( -4.164238869374099927, 32.01208216824730357, 3.795296366450308767 ) ) ;
#96962 = CARTESIAN_POINT ( 'NONE',  ( 2.035157376598822676, 47.43868534415484817, -7.964842623401177768 ) ) ;
#96963 = B_SPLINE_CURVE_WITH_KNOTS ( 'NONE', 3,
 ( #71328, #41337, #25824, #77822, #10817, #8843 ),
 .UNSPECIFIED., .F., .F.,
 ( 4, 2, 4 ),
 ( 0.000000000000000000, 0.0002701661927229330592, 0.0005403323854458661184 ),
 .UNSPECIFIED. ) ;
#96964 = CARTESIAN_POINT ( 'NONE',  ( 18.29284471827483571, 50.40189080397284016, -6.499999999999912070 ) ) ;
#96965 = CIRCLE ( 'NONE', #82514, 11.92686044187656513 ) ;
#96966 = DIRECTION ( 'NONE',  ( 0.7716245833877193316, 0.000000000000000000, -0.6360782202777648386 ) ) ;
#96967 = CARTESIAN_POINT ( 'NONE',  ( 5.076628168052703671, 51.84226448433412315, 8.527530157486179263 ) ) ;
#96968 = CARTESIAN_POINT ( 'NONE',  ( 17.20831665107776587, 4.133931151000785675, -7.208316651077762316 ) ) ;
#96969 = ORIENTED_EDGE ( 'NONE', *, *, #85356, .T. ) ;
#96970 = CARTESIAN_POINT ( 'NONE',  ( 18.52753015748617571, 23.09226448433411960, 4.923371831947298993 ) ) ;
#96971 = CARTESIAN_POINT ( 'NONE',  ( 3.434112377981060948, -14.41803199673624469, 12.81628187352647430 ) ) ;
#96972 = CARTESIAN_POINT ( 'NONE',  ( 15.44008868035555793, 31.39701867748817676, -9.422509992056140149 ) ) ;
#96973 = CARTESIAN_POINT ( 'NONE',  ( 7.361572987183169658, 24.96726448433412315, -9.846743663894592657 ) ) ;
#96974 = CARTESIAN_POINT ( 'NONE',  ( 2.035157376598822676, 62.43868534415483396, -7.964842623401177768 ) ) ;
#96976 = CARTESIAN_POINT ( 'NONE',  ( -2.816281873526471635, 58.91530133659707502, -3.434112377981056508 ) ) ;
#96975 = CARTESIAN_POINT ( 'NONE',  ( 12.91533473730993009, 26.60535201082150536, -10.88017736071109987 ) ) ;
#96977 = CARTESIAN_POINT ( 'NONE',  ( 24.16423886937410614, 44.30374883491397497, 8.672049930838204340E-16 ) ) ;
#96978 = AXIS2_PLACEMENT_3D ( 'NONE', #66766, #22763, #13769 ) ;
#96980 = DIRECTION ( 'NONE',  ( -0.000000000000000000, -1.000000000000000000, -0.000000000000000000 ) ) ;
#96979 = PRESENTATION_LAYER_ASSIGNMENT (  '', '', ( #44277 ) ) ;
#96981 = VERTEX_POINT ( 'NONE', #31233 ) ;
#96982 = CARTESIAN_POINT ( 'NONE',  ( 13.43411237798106583, 2.665301336597086568, -12.81628187352647252 ) ) ;
#96983 = CARTESIAN_POINT ( 'NONE',  ( 15.44008868035555793, 11.39701867748817143, -9.422509992056140149 ) ) ;
#96984 = CARTESIAN_POINT ( 'NONE',  ( 2.035157376598822676, 42.43868534415483396, -7.964842623401177768 ) ) ;
#96985 = CARTESIAN_POINT ( 'NONE',  ( 17.20831665107776587, 57.88393115100078745, 7.208316651077764980 ) ) ;
#96986 = EDGE_LOOP ( 'NONE', ( #6634, #5880, #98828, #31625 ) ) ;
#96987 = CARTESIAN_POINT ( 'NONE',  ( 18.52753015748617571, 18.09226448433411960, 4.923371831947298993 ) ) ;
#96988 = MECHANICAL_DESIGN_GEOMETRIC_PRESENTATION_REPRESENTATION (  '', ( #85770 ), #53864 ) ;
#96989 = CARTESIAN_POINT ( 'NONE',  ( 15.44008868035555260, 54.73035201082150536, 9.422509992056143702 ) ) ;
#96990 = CARTESIAN_POINT ( 'NONE',  ( 12.63842701281683922, 34.55059781766745886, -9.846743663894590881 ) ) ;
#96991 = CARTESIAN_POINT ( 'NONE',  ( 14.92337183194729633, 27.67559781766745530, 8.527530157486181039 ) ) ;
#96992 = CARTESIAN_POINT ( 'NONE',  ( 2.791683348922237240, 20.38393115100078745, -7.208316651077763204 ) ) ;
#96993 = CARTESIAN_POINT ( 'NONE',  ( -5.780406540405962801, -39.80436905996668884, 2.500000000000000000 ) ) ;
#96995 = AXIS2_PLACEMENT_3D ( 'NONE', #33370, #3391, #33854 ) ;
#96994 = CARTESIAN_POINT ( 'NONE',  ( 0.1532563361054082862, 1.217264484334117824, 2.638427012816831674 ) ) ;
#96997 = ORIENTED_EDGE ( 'NONE', *, *, #89523, .T. ) ;
#96996 = CARTESIAN_POINT ( 'NONE',  ( 19.84674366389459266, 28.71726448433411960, -2.638427012816827677 ) ) ;
#96998 = CIRCLE ( 'NONE', #84217, 0.2500000000000002220 ) ;
#96999 = EDGE_CURVE ( 'NONE', #96102, #97731, #46916, .T. ) ;
#97000 = CARTESIAN_POINT ( 'NONE',  ( 6.825220758711185276, -50.90060425938852973, 3.999999999999999112 ) ) ;
#97001 = CARTESIAN_POINT ( 'NONE',  ( 18.52753015748618282, 63.92559781766745886, -4.923371831947291888 ) ) ;
#97002 = ADVANCED_FACE ( 'NONE', ( #24257 ), #40230, .T. ) ;
#97004 = EDGE_CURVE ( 'NONE', #54629, #5586, #47220, .T. ) ;
#97003 = CARTESIAN_POINT ( 'NONE',  ( 2.917880565312950480, 15.97041550158063217, -12.26659068614894821 ) ) ;
#97005 = CARTESIAN_POINT ( 'NONE',  ( 2.917880565312948704, 12.63708216824730179, 12.26659068614894643 ) ) ;
#97006 = CARTESIAN_POINT ( 'NONE',  ( -2.266590686148945544, 51.38708216824730357, -7.082119434687050408 ) ) ;
#97007 = CARTESIAN_POINT ( 'NONE',  ( -2.266590686148945544, 1.387082168247301128, -7.082119434687050408 ) ) ;
#97009 = CARTESIAN_POINT ( 'NONE',  ( 20.88017736071110875, 65.77201867748817676, -2.915334737309920765 ) ) ;
#97008 = CARTESIAN_POINT ( 'NONE',  ( 20.36894250292379382, 13.67874883491396965, 10.36894250292379205 ) ) ;
#97010 = CARTESIAN_POINT ( 'NONE',  ( 19.42250999205614548, 45.98035201082150536, -5.440088680355545492 ) ) ;
#97011 = CARTESIAN_POINT ( 'NONE',  ( 6.903457398626329677, -84.61157762779829739, -3.750000000000000888 ) ) ;
#97012 = VERTEX_POINT ( 'NONE', #77233 ) ;
#97013 = CARTESIAN_POINT ( 'NONE',  ( 12.63842701281683922, 34.55059781766745886, -9.846743663894590881 ) ) ;
#97015 = CARTESIAN_POINT ( 'NONE',  ( 18.52753015748618282, 23.92559781766745530, -4.923371831947291888 ) ) ;
#97014 = CARTESIAN_POINT ( 'NONE',  ( 5.419894505350588254, 0.3640475087720895231, -13.98659156302459472 ) ) ;
#97016 = VERTEX_POINT ( 'NONE', #39747 ) ;
#97017 = CARTESIAN_POINT ( 'NONE',  ( 4.559911319644449179, 12.23035201082150714, -9.422509992056141925 ) ) ;
#97018 = CARTESIAN_POINT ( 'NONE',  ( 0.6178305044545838731, 54.74863466993042493, 9.382169495545420901 ) ) ;
#97019 = CARTESIAN_POINT ( 'NONE',  ( 2.791683348922237240, 50.38393115100078035, -7.208316651077763204 ) ) ;
#97020 = CARTESIAN_POINT ( 'NONE',  ( 18.00000000000000355, 77.62863619046393637, 4.012044713968255572 ) ) ;
#97021 = CARTESIAN_POINT ( 'NONE',  ( 17.20831665107776587, 32.88393115100078745, 7.208316651077764980 ) ) ;
#97022 = CARTESIAN_POINT ( 'NONE',  ( 10.00000000000000000, 42.87363466993042493, -12.81628187352647608 ) ) ;
#97023 = CARTESIAN_POINT ( 'NONE',  ( -10.36894250292378317, -22.57125116508603213, 10.36894250292379560 ) ) ;
#97024 = CARTESIAN_POINT ( 'NONE',  ( 4.559911319644449179, 43.89701867748816966, 9.422509992056141925 ) ) ;
#97025 = CARTESIAN_POINT ( 'NONE',  ( 14.92337183194729633, 37.67559781766745175, 8.527530157486181039 ) ) ;
#97026 = CARTESIAN_POINT ( 'NONE',  ( 24.16423886937409904, 24.09541550158063927, 3.795296366450317205 ) ) ;
#97027 = EDGE_LOOP ( 'NONE', ( #35535, #43641, #16544, #33478, #93015, #69052 ) ) ;
#97028 = CARTESIAN_POINT ( 'NONE',  ( 22.26659068614895176, 4.720415501580633943, -7.082119434687042414 ) ) ;
#97029 = VECTOR ( 'NONE', #81888, 1000.000000000000000 ) ;
#97030 = CARTESIAN_POINT ( 'NONE',  ( 12.91533473730992121, 49.52201867748817676, 10.88017736071110164 ) ) ;
#97031 = CARTESIAN_POINT ( 'NONE',  ( 12.91533473730992121, 64.52201867748817676, 10.88017736071110164 ) ) ;
#97032 = CARTESIAN_POINT ( 'NONE',  ( -4.164238869374099927, 47.01208216824729647, 3.795296366450308767 ) ) ;
#97033 = CARTESIAN_POINT ( 'NONE',  ( -2.816281873526473856, 4.123634669930420493, 9.499525473075851096E-16 ) ) ;
#97034 = CARTESIAN_POINT ( 'NONE',  ( 2.827051895225687783, 14.76984989550149407, 14.67071941139715108 ) ) ;
#97035 = CARTESIAN_POINT ( 'NONE',  ( 20.88017736071110519, 60.56368534415484106, 2.639326808657452039E-16 ) ) ;
#97036 = ADVANCED_FACE ( 'NONE', ( #47722 ), #8738, .F. ) ;
#97037 = DIRECTION ( 'NONE',  ( 0.000000000000000000, 0.000000000000000000, 1.000000000000000000 ) ) ;
#97038 = CARTESIAN_POINT ( 'NONE',  ( 10.00000000000000178, 25.37363466993041783, 12.81628187352647608 ) ) ;
#97039 = CARTESIAN_POINT ( 'NONE',  ( 19.84674366389459266, 63.71726448433412315, -2.638427012816827677 ) ) ;
#97040 = CARTESIAN_POINT ( 'NONE',  ( -9.422509992056136596, 33.48035201082149825, 5.440088680355559703 ) ) ;
#97041 = CARTESIAN_POINT ( 'NONE',  ( 2.035157376598824452, 18.68868534415484106, 7.964842623401179544 ) ) ;
#97042 = CARTESIAN_POINT ( 'NONE',  ( 12.91533473730992121, 4.522018677488170546, 10.88017736071110164 ) ) ;
#97043 = CARTESIAN_POINT ( 'NONE',  ( 0.000000000000000000, 14.49999999999999822, 0.000000000000000000 ) ) ;
#97044 = ORIENTED_EDGE ( 'NONE', *, *, #82204, .T. ) ;
#97045 = MECHANICAL_DESIGN_GEOMETRIC_PRESENTATION_REPRESENTATION (  '', ( #71482 ), #63471 ) ;
#97046 = DIRECTION ( 'NONE',  ( 1.000000000000000000, 4.163336342344333240E-14, 0.000000000000000000 ) ) ;
#97047 = DIRECTION ( 'NONE',  ( 1.000000000000000000, -8.673617379884027583E-16, 0.000000000000000000 ) ) ;
#97048 = CARTESIAN_POINT ( 'NONE',  ( 19.84674366389459266, 3.300597817667451750, 2.638427012816836559 ) ) ;
#97049 = VECTOR ( 'NONE', #60526, 1000.000000000000000 ) ;
#97050 = CARTESIAN_POINT ( 'NONE',  ( 10.00000000000000178, 32.25893115100078745, 9.846743663894594434 ) ) ;
#97051 = CARTESIAN_POINT ( 'NONE',  ( 19.42250999205614548, 40.98035201082150536, -5.440088680355545492 ) ) ;
#97052 = CARTESIAN_POINT ( 'NONE',  ( 19.38216949554541202, 10.99863466993042138, 9.382169495545424454 ) ) ;
#97054 = CARTESIAN_POINT ( 'NONE',  ( 10.32896413005680181, 9.745456701841140656, 5.963430220938278126 ) ) ;
#97053 = CARTESIAN_POINT ( 'NONE',  ( -0.8801773607111008646, 33.27201867748817676, 2.915334737309923430 ) ) ;
#97055 = DIRECTION ( 'NONE',  ( -6.217248937900876626E-14, 0.000000000000000000, 1.000000000000000000 ) ) ;
#97056 = CARTESIAN_POINT ( 'NONE',  ( -1.099225684535947600, 33.70696800326375353, -6.408140936763238038 ) ) ;
#97057 = ORIENTED_EDGE ( 'NONE', *, *, #32742, .F. ) ;
#97058 = CARTESIAN_POINT ( 'NONE',  ( 2.035157376598822676, 67.43868534415484817, -7.964842623401177768 ) ) ;
#97060 = CARTESIAN_POINT ( 'NONE',  ( 13.79529636645030344, 8.262082168247300018, 14.16423886937410614 ) ) ;
#97059 = CARTESIAN_POINT ( 'NONE',  ( 22.81628187352648496, 36.83196800326376064, -3.434112377981050290 ) ) ;
#97061 = CARTESIAN_POINT ( 'NONE',  ( 21.92686044187656336, 31.97997603579417358, 3.195792623639536423 ) ) ;
#97062 = CARTESIAN_POINT ( 'NONE',  ( 15.44008868035555793, 36.39701867748816966, -9.422509992056140149 ) ) ;
#97063 = CARTESIAN_POINT ( 'NONE',  ( 6.000000000000000000, 11.00000000000000000, 5.000000000000000000 ) ) ;
#97064 = CARTESIAN_POINT ( 'NONE',  ( 13.79529636645031943, 65.34541550158063217, -14.16423886937409904 ) ) ;
#97065 = VECTOR ( 'NONE', #78120, 1000.000000000000114 ) ;
#97066 = CARTESIAN_POINT ( 'NONE',  ( 14.92337183194729633, 57.67559781766745886, 8.527530157486181039 ) ) ;
#97067 = CARTESIAN_POINT ( 'NONE',  ( 12.63842701281683922, 14.55059781766744997, -9.846743663894590881 ) ) ;
#97068 = CARTESIAN_POINT ( 'NONE',  ( 7.084665262690076126, 57.02201867748817676, -10.88017736071110164 ) ) ;
#97069 = CARTESIAN_POINT ( 'NONE',  ( -4.326345305608673364, 0.000000000000000000, 3.319721512309553368 ) ) ;
#97070 = CARTESIAN_POINT ( 'NONE',  ( 24.16423886937410614, 34.51208216824731068, -3.795296366450302550 ) ) ;
#97071 = DIRECTION ( 'NONE',  ( 0.000000000000000000, -1.000000000000000000, 0.000000000000000000 ) ) ;
#97072 = AXIS2_PLACEMENT_3D ( 'NONE', #46215, #92684, #60222 ) ;
#97073 = CARTESIAN_POINT ( 'NONE',  ( 10.88969086829045452, -97.65447219785596644, -3.750000000000000000 ) ) ;
#97074 = CARTESIAN_POINT ( 'NONE',  ( -4.262581423003710235, -13.85606188143285600, -3.750000000000000444 ) ) ;
#97075 = AXIS2_PLACEMENT_3D ( 'NONE', #85746, #31741, #40734 ) ;
#97076 = VERTEX_POINT ( 'NONE', #8261 ) ;
#97077 = CARTESIAN_POINT ( 'NONE',  ( 10.00000000000000000, 60.55374883491397497, -14.16423886937410082 ) ) ;
#97078 = CARTESIAN_POINT ( 'NONE',  ( 0.5774900079438607392, 3.480352010821504916, 5.440088680355550821 ) ) ;
#97079 = CARTESIAN_POINT ( 'NONE',  ( 5.076628168052703671, 26.84226448433411960, 8.527530157486179263 ) ) ;
#97080 = CARTESIAN_POINT ( 'NONE',  ( -1.099225684535947600, 23.70696800326375708, -6.408140936763238038 ) ) ;
#97081 = CYLINDRICAL_SURFACE ( 'NONE', #33197, 0.2500000000000002220 ) ;
#97082 = CARTESIAN_POINT ( 'NONE',  ( -0.1503990784575279516, 43.10158574516643171, 6.262539305110076171 ) ) ;
#97083 = CARTESIAN_POINT ( 'NONE',  ( 2.035157376598822676, 7.438685344154837509, -7.964842623401177768 ) ) ;
#97084 = CARTESIAN_POINT ( 'NONE',  ( 13.79529636645030344, 58.26208216824728936, 14.16423886937410614 ) ) ;
#97085 = CARTESIAN_POINT ( 'NONE',  ( 17.20831665107776587, 32.88393115100078745, 7.208316651077764980 ) ) ;
#97086 = DIRECTION ( 'NONE',  ( -0.06975647374410356982, -0.9975640502598257520, -0.000000000000000000 ) ) ;
#97088 = B_SPLINE_CURVE_WITH_KNOTS ( 'NONE', 3,
 ( #73438, #34449, #4964, #64941, #57459, #11962 ),
 .UNSPECIFIED., .F., .F.,
 ( 4, 2, 4 ),
 ( 0.000000000000000000, 0.0002565770811490921321, 0.0005131541622981842642 ),
 .UNSPECIFIED. ) ;
#97087 = CARTESIAN_POINT ( 'NONE',  ( 14.92337183194729633, 12.67559781766745353, 8.527530157486181039 ) ) ;
#97089 = DIRECTION ( 'NONE',  ( 1.000000000000000000, 0.000000000000000000, 0.000000000000000000 ) ) ;
#97090 = CARTESIAN_POINT ( 'NONE',  ( 3.469446951953614189E-15, 22.25893115100079100, 9.846743663894594434 ) ) ;
#97091 = ORIENTED_EDGE ( 'NONE', *, *, #71268, .T. ) ;
#97092 = ORIENTED_EDGE ( 'NONE', *, *, #98665, .T. ) ;
#97093 = VERTEX_POINT ( 'NONE', #9237 ) ;
#97094 = CARTESIAN_POINT ( 'NONE',  ( 0.1532563361054100626, 40.80059781766745886, -2.638427012816831230 ) ) ;
#97095 = CARTESIAN_POINT ( 'NONE',  ( -0.3689425029237898834, 16.17874883491396076, -10.36894250292378850 ) ) ;
#97097 = CARTESIAN_POINT ( 'NONE',  ( 7.084665262690076126, 24.10535201082150181, 10.88017736071109987 ) ) ;
#97096 = CARTESIAN_POINT ( 'NONE',  ( 20.88017736071110875, 20.77201867748816611, -2.915334737309920765 ) ) ;
#97099 = CARTESIAN_POINT ( 'NONE',  ( 6.565887622018943937, 18.08196800326375708, -12.81628187352647608 ) ) ;
#97098 = SURFACE_SIDE_STYLE ('',( #44556 ) ) ;
#97100 = CARTESIAN_POINT ( 'NONE',  ( 10.00000000000000000, 0.5537488349139675359, -14.16423886937410082 ) ) ;
#97101 = EDGE_CURVE ( 'NONE', #98966, #39344, #62225, .T. ) ;
#97102 = CARTESIAN_POINT ( 'NONE',  ( 22.81628187352648496, 36.83196800326376064, -3.434112377981050290 ) ) ;
#97104 = ORIENTED_EDGE ( 'NONE', *, *, #78101, .T. ) ;
#97103 = CARTESIAN_POINT ( 'NONE',  ( 1.472469842513823179, 1.425597817667451528, 4.923371831947296329 ) ) ;
#97105 = CARTESIAN_POINT ( 'NONE',  ( 0.1532563361054083140, 26.00893115100078745, 1.131784320476157264E-15 ) ) ;
#97106 = CARTESIAN_POINT ( 'NONE',  ( 2.917880565312948704, 67.63708216824730357, 12.26659068614894643 ) ) ;
#97107 = VERTEX_POINT ( 'NONE', #70243 ) ;
#97108 = CARTESIAN_POINT ( 'NONE',  ( 20.36894250292379382, 63.67874883491396787, 10.36894250292379205 ) ) ;
#97109 = VERTEX_POINT ( 'NONE', #78219 ) ;
#97110 = CARTESIAN_POINT ( 'NONE',  ( 20.88017736071110875, 45.77201867748816966, -2.915334737309920765 ) ) ;
#97111 = CARTESIAN_POINT ( 'NONE',  ( -0.8801773607111009756, 63.06368534415484106, 1.068504757029289695E-15 ) ) ;
#97112 = CARTESIAN_POINT ( 'NONE',  ( -0.8801773607111008646, 48.27201867748816966, 2.915334737309923430 ) ) ;
#97113 = CARTESIAN_POINT ( 'NONE',  ( 1.472469842513823179, 1.425597817667451528, 4.923371831947296329 ) ) ;
#97114 = CARTESIAN_POINT ( 'NONE',  ( 4.559911319644449179, 42.23035201082151247, -9.422509992056141925 ) ) ;
#97115 = CARTESIAN_POINT ( 'NONE',  ( 0.000000000000000000, 15.00000000000000000, 0.000000000000000000 ) ) ;
#97117 = VERTEX_POINT ( 'NONE', #16745 ) ;
#97116 = VECTOR ( 'NONE', #85502, 1000.000000000000114 ) ;
#97118 = EDGE_CURVE ( 'NONE', #50286, #56730, #84749, .T. ) ;
#97119 = CARTESIAN_POINT ( 'NONE',  ( 14.92337183194729988, 29.34226448433411960, -8.527530157486177487 ) ) ;
#97120 = ORIENTED_EDGE ( 'NONE', *, *, #40419, .T. ) ;
#97121 = CARTESIAN_POINT ( 'NONE',  ( 0.1532563361054083140, 56.00893115100078745, 1.131784320476157264E-15 ) ) ;
#97123 = EDGE_CURVE ( 'NONE', #55759, #76829, #70738, .T. ) ;
#97122 = CARTESIAN_POINT ( 'NONE',  ( 4.862001128006681938, 4.613545383394330660E-16, 13.66056166602463229 ) ) ;
#97124 = CARTESIAN_POINT ( 'NONE',  ( -4.164238869374099039, 1.803748834913967647, 8.674139862899312516E-16 ) ) ;
#97125 = TOROIDAL_SURFACE ( 'NONE', #17321, 14.49999999999999822, 0.5000000000000000000 ) ;
#97126 = ORIENTED_EDGE ( 'NONE', *, *, #85946, .F. ) ;
#97127 = CARTESIAN_POINT ( 'NONE',  ( 19.05866839779140776, 50.95508385108959004, -6.499999999999956479 ) ) ;
#97128 = CARTESIAN_POINT ( 'NONE',  ( -3.585811805803780672, -2.700665136322976334, 3.750000000000000000 ) ) ;
#97129 = CARTESIAN_POINT ( 'NONE',  ( -3.750000000000000000, 37.25000000000000000, 4.000000000000000000 ) ) ;
#97130 = CARTESIAN_POINT ( 'NONE',  ( 13.79529636645031943, 55.34541550158062506, -14.16423886937409904 ) ) ;
#97131 = CARTESIAN_POINT ( 'NONE',  ( -46.94000000000001194, 103.0000000000000000, 5.000000000000000000 ) ) ;
#97132 = VERTEX_POINT ( 'NONE', #32214 ) ;
#97133 = DIRECTION ( 'NONE',  ( -0.008726535498367549160, 0.000000000000000000, -0.9999619230641714207 ) ) ;
#97134 = CARTESIAN_POINT ( 'NONE',  ( 0.1532563361054083140, 51.00893115100078745, 1.131784320476157264E-15 ) ) ;
#97135 = FACE_OUTER_BOUND ( 'NONE', #42855, .T. ) ;
#97136 = CARTESIAN_POINT ( 'NONE',  ( 22.81628187352647785, 21.41530133659708923, 3.434112377981063169 ) ) ;
#97137 = CARTESIAN_POINT ( 'NONE',  ( 2.791683348922237240, 15.38393115100078212, -7.208316651077763204 ) ) ;
#97138 = CARTESIAN_POINT ( 'NONE',  ( -33.19000000000001194, 92.00000000000000000, 9.500000000000000000 ) ) ;
#97139 = CARTESIAN_POINT ( 'NONE',  ( 19.84674366389459266, 3.717264484334118713, -2.638427012816827677 ) ) ;
#97140 = CARTESIAN_POINT ( 'NONE',  ( -1.099225684535947600, 3.706968003263753531, -6.408140936763238038 ) ) ;
#97141 = VECTOR ( 'NONE', #47004, 1000.000000000000000 ) ;
#97142 = CARTESIAN_POINT ( 'NONE',  ( -6.382347221874512755, 0.5000000000000004441, 13.57444820018223375 ) ) ;
#97143 = VERTEX_POINT ( 'NONE', #69748 ) ;
#97144 = CARTESIAN_POINT ( 'NONE',  ( 20.88017736071110164, 5.355352010821503583, 2.915334737309930979 ) ) ;
#97145 = CARTESIAN_POINT ( 'NONE',  ( 10.00000000000000000, 0.5537488349139675359, -14.16423886937410082 ) ) ;
#97146 = CARTESIAN_POINT ( 'NONE',  ( 12.63842701281683034, 22.46726448433411605, 9.846743663894596210 ) ) ;
#97147 = CARTESIAN_POINT ( 'NONE',  ( 2.035157376598822676, 57.43868534415484106, -7.964842623401177768 ) ) ;
#97149 = CARTESIAN_POINT ( 'NONE',  ( 9.159723438033203990, 0.000000000000000000, -10.91613331444542645 ) ) ;
#97148 = CARTESIAN_POINT ( 'NONE',  ( -1.099225684535947600, 28.70696800326375353, -6.408140936763238038 ) ) ;
#97150 = CARTESIAN_POINT ( 'NONE',  ( 15.44008868035555260, 19.73035201082150536, 9.422509992056143702 ) ) ;
#97151 = EDGE_CURVE ( 'NONE', #45908, #18967, #646, .T. ) ;
#97152 = CARTESIAN_POINT ( 'NONE',  ( -4.873787042390612001, 15.00000000000000000, -13.39061984619925916 ) ) ;
#97153 = DIRECTION ( 'NONE',  ( 0.000000000000000000, 0.000000000000000000, 1.000000000000000000 ) ) ;
#97154 = PRODUCT_DEFINITION_SHAPE ( 'NONE', 'NONE',  #56260 ) ;
#97155 = CARTESIAN_POINT ( 'NONE',  ( -1.099225684535947600, 3.706968003263753531, -6.408140936763238038 ) ) ;
#97156 = CARTESIAN_POINT ( 'NONE',  ( 19.84674366389459621, 58.50893115100078745, 7.409399052514197653E-17 ) ) ;
#97157 = CARTESIAN_POINT ( 'NONE',  ( 18.52753015748618282, 8.925597817667451750, -4.923371831947291888 ) ) ;
#97158 = CARTESIAN_POINT ( 'NONE',  ( 10.88017736071110519, -29.43631465584515894, -2.602085213965210642E-15 ) ) ;
#97159 = CARTESIAN_POINT ( 'NONE',  ( 19.38216949554541557, 37.24863466993041783, -9.382169495545420901 ) ) ;
#97160 = CARTESIAN_POINT ( 'NONE',  ( -11.20030343312800980, -94.46585862447406612, -4.000000000000451195 ) ) ;
#97162 = DIRECTION ( 'NONE',  ( -0.6360782202777597316, 0.000000000000000000, -0.7716245833877234395 ) ) ;
#97161 = CARTESIAN_POINT ( 'NONE',  ( 4.559911319644449179, 37.23035201082150536, -9.422509992056141925 ) ) ;
#97163 = CARTESIAN_POINT ( 'NONE',  ( 13.95697193428312310, 15.00000000000000711, -4.371663894958823349 ) ) ;
#97164 = CARTESIAN_POINT ( 'NONE',  ( -0.8801773607110991993, 22.85535201082150181, -2.915334737309923874 ) ) ;
#97165 = CARTESIAN_POINT ( 'NONE',  ( 4.559911319644449179, 33.89701867748817676, 9.422509992056141925 ) ) ;
#97166 = CARTESIAN_POINT ( 'NONE',  ( 17.20831665107776587, 47.88393115100078745, 7.208316651077764980 ) ) ;
#97167 = CARTESIAN_POINT ( 'NONE',  ( 10.00000000000000178, 54.31368534415484106, 10.88017736071110342 ) ) ;
#97168 = CARTESIAN_POINT ( 'NONE',  ( 13.79529636645031943, 35.34541550158063927, -14.16423886937409904 ) ) ;
#97169 = UNCERTAINTY_MEASURE_WITH_UNIT (LENGTH_MEASURE( 1.000000000000000082E-05 ), #12114, 'distance_accuracy_value', 'NONE');
#97170 = CARTESIAN_POINT ( 'NONE',  ( 14.92337183194729988, 44.34226448433412315, -8.527530157486177487 ) ) ;
#97171 = CARTESIAN_POINT ( 'NONE',  ( 0.6178305044545838731, 59.74863466993041783, 9.382169495545420901 ) ) ;
#97172 = CARTESIAN_POINT ( 'NONE',  ( 16.40814093676323893, 0.7903013365970867898, 11.09922568453595026 ) ) ;
#97173 = VERTEX_POINT ( 'NONE', #62715 ) ;
#97174 = CARTESIAN_POINT ( 'NONE',  ( 2.035157376598822676, 22.43868534415483396, -7.964842623401177768 ) ) ;
#97175 = CARTESIAN_POINT ( 'NONE',  ( 17.96484262340118221, 6.188685344154836621, -7.964842623401177768 ) ) ;
#97176 = CARTESIAN_POINT ( 'NONE',  ( 17.96484262340118221, 16.18868534415483396, -7.964842623401177768 ) ) ;
#97177 = CARTESIAN_POINT ( 'NONE',  ( 0.1532563361054082862, 1.217264484334117824, 2.638427012816831674 ) ) ;
#97178 = CARTESIAN_POINT ( 'NONE',  ( 13.79529636645030344, 18.26208216824730002, 14.16423886937410614 ) ) ;
#97179 = CARTESIAN_POINT ( 'NONE',  ( 19.84674366389459266, 8.717264484334116048, -2.638427012816827677 ) ) ;
#97180 = CARTESIAN_POINT ( 'NONE',  ( 7.361572987183170547, 62.05059781766745886, 9.846743663894590881 ) ) ;
#97181 = CARTESIAN_POINT ( 'NONE',  ( 10.00000000000000178, 39.31368534415484106, 10.88017736071110342 ) ) ;
#97182 = CARTESIAN_POINT ( 'NONE',  ( 18.72515096720577787, 46.07228050351031357, -6.499999999999891642 ) ) ;
#97183 = CARTESIAN_POINT ( 'NONE',  ( 8.157990163924791815, 0.2306972965111897811, -12.51739793958113722 ) ) ;
#97184 = EDGE_LOOP ( 'NONE', ( #78023, #44566, #35304, #4913, #85258, #40249 ) ) ;
#97185 = CIRCLE ( 'NONE', #13733, 15.00000000000000000 ) ;
#97186 = CARTESIAN_POINT ( 'NONE',  ( 13.99999999999999822, 11.00000000000000000, 5.000000000000000000 ) ) ;
#97187 = CARTESIAN_POINT ( 'NONE',  ( 7.361572987183169658, 44.96726448433412315, -9.846743663894592657 ) ) ;
#97188 = ORIENTED_EDGE ( 'NONE', *, *, #45616, .F. ) ;
#97189 = ORIENTED_EDGE ( 'NONE', *, *, #53885, .T. ) ;
#97190 = CARTESIAN_POINT ( 'NONE',  ( -14.52941021839283131, -2.744386749103930633E-16, -1.683622718073243263 ) ) ;
#97191 = CARTESIAN_POINT ( 'NONE',  ( 17.08211943468705130, 28.47041550158063572, 12.26659068614894998 ) ) ;
#97192 = CARTESIAN_POINT ( 'NONE',  ( -2.266590686148945544, 21.38708216824730357, -7.082119434687050408 ) ) ;
#97193 = CARTESIAN_POINT ( 'NONE',  ( 4.559911319644449179, 62.23035201082150536, -9.422509992056141925 ) ) ;
#97194 = CARTESIAN_POINT ( 'NONE',  ( 20.36894250292379382, 58.67874883491396076, 10.36894250292379205 ) ) ;
#97195 = CARTESIAN_POINT ( 'NONE',  ( 19.38216949554541202, 0.9986346699304200492, 9.382169495545424454 ) ) ;
#97196 = CARTESIAN_POINT ( 'NONE',  ( 2.791683348922237240, 55.38393115100078745, -7.208316651077763204 ) ) ;
#97197 = CARTESIAN_POINT ( 'NONE',  ( -10.53011945866295029, -98.59345040283277228, 4.000000000000000000 ) ) ;
#97199 = CARTESIAN_POINT ( 'NONE',  ( -2.816281873526473856, 4.331968003263754419, 3.434112377981055619 ) ) ;
#97198 = CARTESIAN_POINT ( 'NONE',  ( 7.084665262690076126, 44.10535201082151247, 10.88017736071109987 ) ) ;
#97200 = CARTESIAN_POINT ( 'NONE',  ( -2.266590686148945544, 17.22041550158063572, 7.082119434687048631 ) ) ;
#97201 = CARTESIAN_POINT ( 'NONE',  ( 6.204703633549690345, 50.76208216824730357, -14.16423886937410259 ) ) ;
#97202 = CARTESIAN_POINT ( 'NONE',  ( 0.5774900079438590739, 22.64701867748817321, -5.440088680355550821 ) ) ;
#97203 = CARTESIAN_POINT ( 'NONE',  ( 20.24186590665278018, 5.590145880403569301, -6.114288769123027656 ) ) ;
#97204 = CARTESIAN_POINT ( 'NONE',  ( 20.88017736071110875, 40.77201867748818387, -2.915334737309920765 ) ) ;
#97205 = MECHANICAL_DESIGN_GEOMETRIC_PRESENTATION_REPRESENTATION (  '', ( #9386 ), #10957 ) ;
#97206 = CARTESIAN_POINT ( 'NONE',  ( 9.846743663894590881, -21.69940218233254470, 2.638427012816828565 ) ) ;
#97207 = ORIENTED_EDGE ( 'NONE', *, *, #54333, .F. ) ;
#97208 = CARTESIAN_POINT ( 'NONE',  ( 19.80832241502128355, 4.758688159020694641, 6.500000000000000888 ) ) ;
#97209 = ORIENTED_EDGE ( 'NONE', *, *, #38954, .F. ) ;
#97210 = ORIENTED_EDGE ( 'NONE', *, *, #96311, .T. ) ;
#97211 = CARTESIAN_POINT ( 'NONE',  ( 10.00000000000000178, 43.05374883491397497, 14.16423886937410082 ) ) ;
#97212 = CARTESIAN_POINT ( 'NONE',  ( 0.1532563361054083140, 41.00893115100078745, 1.131784320476157264E-15 ) ) ;
#97213 = CARTESIAN_POINT ( 'NONE',  ( 10.00000000000000000, 66.81368534415484817, -10.88017736071110342 ) ) ;
#97214 = EDGE_CURVE ( 'NONE', #74673, #89322, #54906, .T. ) ;
#97215 = AXIS2_PLACEMENT_3D ( 'NONE', #40129, #85137, #40627 ) ;
#97216 = DIRECTION ( 'NONE',  ( 1.000000000000000000, 0.000000000000000000, 0.000000000000000000 ) ) ;
#97217 = MECHANICAL_DESIGN_GEOMETRIC_PRESENTATION_REPRESENTATION (  '', ( #4624 ), #30153 ) ;
#97218 = CARTESIAN_POINT ( 'NONE',  ( 10.00000000000000178, 59.31368534415484106, 10.88017736071110342 ) ) ;
#97219 = CARTESIAN_POINT ( 'NONE',  ( 16.40814093676323893, 60.79030133659709634, 11.09922568453595026 ) ) ;
#97220 = CARTESIAN_POINT ( 'NONE',  ( 12.81628187352647608, 6.415301336597086568, 3.434112377981052511 ) ) ;
#97221 = VERTEX_POINT ( 'NONE', #85241 ) ;
#97222 = CARTESIAN_POINT ( 'NONE',  ( 20.36894250292379382, 13.67874883491396965, 10.36894250292379205 ) ) ;
#97223 = B_SPLINE_CURVE_WITH_KNOTS ( 'NONE', 3,
 ( #72868, #50870, #82343, #81847, #20870, #81362, #12861, #73857, #5387, #44343, #28365, #28841, #58853, #89359, #74849, #59344, #89846, #6350 ),
 .UNSPECIFIED., .F., .F.,
 ( 4, 2, 2, 2, 2, 2, 2, 2, 4 ),
 ( 0.000000000000000000, 0.001337396791554949218, 0.002674793583109898436, 0.004012190374664847438, 0.005349587166219796873, 0.006686983957774746308, 0.008024380749329694876, 0.009361777540884644311, 0.01069917433243959375 ),
 .UNSPECIFIED. ) ;
#97224 = CARTESIAN_POINT ( 'NONE',  ( 21.09922568453594849, 21.20696800326375353, 6.408140936763242479 ) ) ;
#97225 = VERTEX_POINT ( 'NONE', #93215 ) ;
#97226 = CARTESIAN_POINT ( 'NONE',  ( 6.565887622018943937, 40.16530133659708923, 12.81628187352647430 ) ) ;
#97227 = AXIS2_PLACEMENT_3D ( 'NONE', #60188, #37221, #59692 ) ;
#97228 = CARTESIAN_POINT ( 'NONE',  ( 14.92337183194729988, 34.34226448433411605, -8.527530157486177487 ) ) ;
#97229 = CARTESIAN_POINT ( 'NONE',  ( 4.559911319644449179, 12.23035201082150536, -9.422509992056141925 ) ) ;
#97230 = CARTESIAN_POINT ( 'NONE',  ( 16.40814093676323893, 50.79030133659708923, 11.09922568453595026 ) ) ;
#97231 = CARTESIAN_POINT ( 'NONE',  ( 5.991992585808628036, 4.207234274712436881E-16, -13.20401548210295140 ) ) ;
#97232 = CARTESIAN_POINT ( 'NONE',  ( 10.00000000000000000, 39.75893115100078745, -9.846743663894594434 ) ) ;
#97233 = LINE ( 'NONE', #80724, #68064 ) ;
#97234 = EDGE_CURVE ( 'NONE', #98695, #35712, #9731, .T. ) ;
#97235 = CARTESIAN_POINT ( 'NONE',  ( 8.629999999999995453, 40.74999999999999289, -4.000000000000000000 ) ) ;
#97236 = FACE_OUTER_BOUND ( 'NONE', #98120, .T. ) ;
#97237 = CARTESIAN_POINT ( 'NONE',  ( -10.19513985507817821, 0.5000000000000004441, -11.00268709613231088 ) ) ;
#97238 = CARTESIAN_POINT ( 'NONE',  ( 0.9408516040111476464, 67.46693863883976405, -6.499999999999953815 ) ) ;
#97239 = CARTESIAN_POINT ( 'NONE',  ( 5.076628168052704559, 15.17559781766745175, -8.527530157486179263 ) ) ;
#97240 = EDGE_CURVE ( 'NONE', #73676, #27464, #61249, .T. ) ;
#97241 = CARTESIAN_POINT ( 'NONE',  ( -2.816281873526473856, 19.12363466993042138, 9.499525473075851096E-16 ) ) ;
#97242 = CARTESIAN_POINT ( 'NONE',  ( 4.629999999999990123, 76.07179676972444327, 4.250000000000000000 ) ) ;
#97243 = ORIENTED_EDGE ( 'NONE', *, *, #79727, .T. ) ;
#97244 = CARTESIAN_POINT ( 'NONE',  ( 7.361572987183170547, 57.05059781766744464, 9.846743663894590881 ) ) ;
#97245 = CARTESIAN_POINT ( 'NONE',  ( -13.07734668325334759, 2.727446090158847092E-16, -6.551438809693111764 ) ) ;
#97246 = CARTESIAN_POINT ( 'NONE',  ( 20.36894250292379382, 23.67874883491397142, 10.36894250292379205 ) ) ;
#97247 = CARTESIAN_POINT ( 'NONE',  ( 19.84674366389459266, 43.71726448433410894, -2.638427012816827677 ) ) ;
#97248 = CARTESIAN_POINT ( 'NONE',  ( 3.591859063236763294, 48.29030133659708923, -11.09922568453595026 ) ) ;
#97249 = CARTESIAN_POINT ( 'NONE',  ( -14.26295192185806293, 0.04922511925147220885, -3.770186020345214661 ) ) ;
#97250 = CARTESIAN_POINT ( 'NONE',  ( 0.1532563361054100626, 0.8005978176674514168, -2.638427012816831230 ) ) ;
#97251 = CARTESIAN_POINT ( 'NONE',  ( -10.82344394350217875, 0.04922511925147111944, -10.02492699998892967 ) ) ;
#97252 = CARTESIAN_POINT ( 'NONE',  ( 14.92337183194729633, 52.67559781766745175, 8.527530157486181039 ) ) ;
#97253 = CARTESIAN_POINT ( 'NONE',  ( 15.44008868035555793, 36.39701867748816966, -9.422509992056140149 ) ) ;
#97254 = CARTESIAN_POINT ( 'NONE',  ( 18.52753015748618282, 33.92559781766745886, -4.923371831947291888 ) ) ;
#97255 = DIRECTION ( 'NONE',  ( 0.5393770901257355366, -0.8413553826755496567, -0.03454670303188883684 ) ) ;
#97256 = CARTESIAN_POINT ( 'NONE',  ( -8.731067818237040257, 7.037123368507812060, -8.731067818237033151 ) ) ;
#97257 = CARTESIAN_POINT ( 'NONE',  ( 17.96484262340118221, 41.18868534415484106, -7.964842623401177768 ) ) ;
#97258 = EDGE_CURVE ( 'NONE', #61157, #37561, #2254, .T. ) ;
#97259 = ORIENTED_EDGE ( 'NONE', *, *, #36318, .F. ) ;
#97260 = CARTESIAN_POINT ( 'NONE',  ( -3.836325488035988496, 0.3640475087720956293, -14.50112432709428667 ) ) ;
#97261 = CARTESIAN_POINT ( 'NONE',  ( 12.91533473730992121, 9.522018677488171434, 10.88017736071110164 ) ) ;
#97263 = CARTESIAN_POINT ( 'NONE',  ( 15.44008868035555260, 44.73035201082151247, 9.422509992056143702 ) ) ;
#97262 = CARTESIAN_POINT ( 'NONE',  ( 18.52753015748618282, 53.92559781766745175, -4.923371831947291888 ) ) ;
#97264 = CARTESIAN_POINT ( 'NONE',  ( 7.084665262690076126, 57.02201867748817676, -10.88017736071110164 ) ) ;
#97265 = AXIS2_PLACEMENT_3D ( 'NONE', #61743, #92262, #22302 ) ;
#97267 = CARTESIAN_POINT ( 'NONE',  ( -0.000000000000000000, 72.78284190987160684, -5.243908048977683478 ) ) ;
#97266 = CARTESIAN_POINT ( 'NONE',  ( 20.88017736071110164, 25.35535201082150891, 2.915334737309930979 ) ) ;
#97268 = CARTESIAN_POINT ( 'NONE',  ( 19.84674366389459266, 18.71726448433411960, -2.638427012816827677 ) ) ;
#97269 = CARTESIAN_POINT ( 'NONE',  ( -46.43542959741873233, 103.9441885970218351, -5.610226944091871282 ) ) ;
#97270 = CARTESIAN_POINT ( 'NONE',  ( -14.16423886937409726, 7.012082168247292913, 3.795296366450320757 ) ) ;
#97271 = CARTESIAN_POINT ( 'NONE',  ( 19.84674366389459266, 48.30059781766745175, 2.638427012816836559 ) ) ;
#97272 = CARTESIAN_POINT ( 'NONE',  ( 2.917880565312948704, 67.63708216824730357, 12.26659068614894643 ) ) ;
#97273 = CARTESIAN_POINT ( 'NONE',  ( 12.67122524790586269, 0.04922511925147014800, 7.555537761805852348 ) ) ;
#97274 = CARTESIAN_POINT ( 'NONE',  ( -4.164238869374099927, 7.012082168247302683, 3.795296366450308767 ) ) ;
#97275 = COLOUR_RGB ( '', 0.40784314, 0.44705882, 0.49803922) ;
#97276 = CARTESIAN_POINT ( 'NONE',  ( -2.266590686148945544, 52.22041550158064638, 7.082119434687048631 ) ) ;
#97277 = CARTESIAN_POINT ( 'NONE',  ( -1.099225684535947600, 3.706968003263753531, -6.408140936763238038 ) ) ;
#97278 = CARTESIAN_POINT ( 'NONE',  ( 2.035157376598822676, 12.43868534415483751, -7.964842623401177768 ) ) ;
#97279 = CARTESIAN_POINT ( 'NONE',  ( 10.00000000000000178, 47.25893115100078745, 9.846743663894594434 ) ) ;
#97281 = DIRECTION ( 'NONE',  ( -2.569960705150826877E-16, 1.000000000000000000, -0.000000000000000000 ) ) ;
#97280 = CARTESIAN_POINT ( 'NONE',  ( 2.917880565312950480, 0.9704155015806342766, -12.26659068614894821 ) ) ;
#97282 = CARTESIAN_POINT ( 'NONE',  ( 10.69820648722788015, 1.823139558123380688, 5.272416709312279792 ) ) ;
#97283 = CARTESIAN_POINT ( 'NONE',  ( 2.826948239413825892, 0.2306972965111907248, 14.67127868811027724 ) ) ;
#97284 = CARTESIAN_POINT ( 'NONE',  ( -2.816281873526473856, 29.12363466993041783, 9.499525473075851096E-16 ) ) ;
#97285 = CARTESIAN_POINT ( 'NONE',  ( 19.84674366389459266, 23.71726448433412315, -2.638427012816827677 ) ) ;
#97286 = VERTEX_POINT ( 'NONE', #78719 ) ;
#97287 = CARTESIAN_POINT ( 'NONE',  ( 19.84674366389459621, 8.508931151000785675, 7.409399052514197653E-17 ) ) ;
#97288 = CARTESIAN_POINT ( 'NONE',  ( -12.83294900548053086, 0.3640475087720986824, -7.766300266068548730 ) ) ;
#97289 = DIRECTION ( 'NONE',  ( -0.000000000000000000, 1.000000000000000000, -0.000000000000000000 ) ) ;
#97290 = CARTESIAN_POINT ( 'NONE',  ( 0.5774900079438607392, 18.48035201082150536, 5.440088680355550821 ) ) ;
#97291 = CARTESIAN_POINT ( 'NONE',  ( 13.79529636645030344, 43.26208216824730357, 14.16423886937410614 ) ) ;
#97292 = CARTESIAN_POINT ( 'NONE',  ( 20.88017736071110519, 40.56368534415484106, 2.639326808657452039E-16 ) ) ;
#97293 = CARTESIAN_POINT ( 'NONE',  ( 20.88017736071110875, 65.77201867748817676, -2.915334737309920765 ) ) ;
#97294 = CARTESIAN_POINT ( 'NONE',  ( 0.1532563361054083140, 21.00893115100078745, 1.131784320476157264E-15 ) ) ;
#97295 = FILL_AREA_STYLE_COLOUR ( '', #84886 ) ;
#97296 = CARTESIAN_POINT ( 'NONE',  ( 10.00000000000000000, 4.758931151000784787, -9.846743663894594434 ) ) ;
#97297 = CARTESIAN_POINT ( 'NONE',  ( 19.72487221294570858, 1.866073187300754110, 6.500000000000000888 ) ) ;
#97298 = CARTESIAN_POINT ( 'NONE',  ( 0.1532563361054082862, 41.21726448433411605, 2.638427012816831674 ) ) ;
#97299 = CARTESIAN_POINT ( 'NONE',  ( 2.791683348922240793, 61.63393115100079456, 7.208316651077764092 ) ) ;
#97300 = CARTESIAN_POINT ( 'NONE',  ( -0.8801773607110991993, 42.85535201082150536, -2.915334737309923874 ) ) ;
#97301 = UNCERTAINTY_MEASURE_WITH_UNIT (LENGTH_MEASURE( 1.000000000000000082E-05 ), #32129, 'distance_accuracy_value', 'NONE');
#97302 = EDGE_LOOP ( 'NONE', ( #51164, #18449, #17037, #59306, #16032, #58577 ) ) ;
#97303 = CARTESIAN_POINT ( 'NONE',  ( 6.565887622018943937, 55.16530133659709634, 12.81628187352647430 ) ) ;
#97304 = SURFACE_STYLE_FILL_AREA ( #19312 ) ;
#97305 = CARTESIAN_POINT ( 'NONE',  ( 1.472469842513823179, 10.59226448433411782, -4.923371831947296329 ) ) ;
#97306 = CARTESIAN_POINT ( 'NONE',  ( 13.43411237798106583, 47.66530133659709634, -12.81628187352647252 ) ) ;
#97308 = CARTESIAN_POINT ( 'NONE',  ( 0.1532563361054100626, 30.80059781766744820, -2.638427012816831230 ) ) ;
#97307 = CARTESIAN_POINT ( 'NONE',  ( 7.084665262690076126, 12.02201867748817321, -10.88017736071110164 ) ) ;
#97309 = CARTESIAN_POINT ( 'NONE',  ( 0.2751277870542911952, 33.21833443783938122, 6.499999999999992006 ) ) ;
#97310 = CARTESIAN_POINT ( 'NONE',  ( 10.00000000000000178, 18.05374883491396787, 14.16423886937410082 ) ) ;
#97311 = CARTESIAN_POINT ( 'NONE',  ( -0.3689425029237898834, 46.17874883491397497, -10.36894250292378850 ) ) ;
#97312 = CARTESIAN_POINT ( 'NONE',  ( 19.84674366389459266, 48.71726448433413026, -2.638427012816827677 ) ) ;
#97313 = DIRECTION ( 'NONE',  ( 0.000000000000000000, 0.000000000000000000, -1.000000000000000000 ) ) ;
#97314 = CARTESIAN_POINT ( 'NONE',  ( 10.00000000000000178, 39.31368534415484106, 10.88017736071110342 ) ) ;
#97315 = CARTESIAN_POINT ( 'NONE',  ( 14.92337183194729988, 4.342264484334117824, -8.527530157486177487 ) ) ;
#97316 = TOROIDAL_SURFACE ( 'NONE', #94085, 1.000000000000000000, 0.5000000000000000000 ) ;
#97317 = ORIENTED_EDGE ( 'NONE', *, *, #69112, .T. ) ;
#97318 = CARTESIAN_POINT ( 'NONE',  ( 0.6178305044545818747, 63.49863466993043204, -9.382169495545419124 ) ) ;
#97319 = VERTEX_POINT ( 'NONE', #781 ) ;
#97320 = CARTESIAN_POINT ( 'NONE',  ( 7.084665262690076126, 62.02201867748816966, -10.88017736071110164 ) ) ;
#97321 = EDGE_CURVE ( 'NONE', #14921, #75327, #86103, .T. ) ;
#97322 = ORIENTED_EDGE ( 'NONE', *, *, #14142, .T. ) ;
#97323 = CARTESIAN_POINT ( 'NONE',  ( 20.36894250292379738, 4.928748834913967869, -10.36894250292379027 ) ) ;
#97324 = CARTESIAN_POINT ( 'NONE',  ( 18.52753015748617571, 3.092264484334118269, 4.923371831947298993 ) ) ;
#97325 = EDGE_CURVE ( 'NONE', #20168, #42200, #84270, .T. ) ;
#97326 = CARTESIAN_POINT ( 'NONE',  ( -1.780824192092292924, 0.5000000000000004441, -14.89391369643515795 ) ) ;
#97327 = ORIENTED_EDGE ( 'NONE', *, *, #53839, .T. ) ;
#97328 = CARTESIAN_POINT ( 'NONE',  ( 15.44008868035555793, 16.39701867748817321, -9.422509992056140149 ) ) ;
#97329 = CARTESIAN_POINT ( 'NONE',  ( 19.42250999205614548, 60.98035201082151247, -5.440088680355545492 ) ) ;
#97330 = VERTEX_POINT ( 'NONE', #79203 ) ;
#97331 = CARTESIAN_POINT ( 'NONE',  ( 7.084665262690076126, 27.02201867748817676, -10.88017736071110164 ) ) ;
#97332 = CARTESIAN_POINT ( 'NONE',  ( 1.472469842513823179, 56.42559781766745886, 4.923371831947296329 ) ) ;
#97333 = ORIENTED_EDGE ( 'NONE', *, *, #82890, .F. ) ;
#97334 = CARTESIAN_POINT ( 'NONE',  ( 0.1532563361054082862, 66.21726448433413736, 2.638427012816831674 ) ) ;
#97335 = ORIENTED_EDGE ( 'NONE', *, *, #77853, .T. ) ;
#97336 = CARTESIAN_POINT ( 'NONE',  ( 0.5774900079438607392, 68.48035201082150536, 5.440088680355550821 ) ) ;
#97337 = CARTESIAN_POINT ( 'NONE',  ( 0.1532563361054100626, 60.80059781766744464, -2.638427012816831230 ) ) ;
#97338 = CARTESIAN_POINT ( 'NONE',  ( 19.38216949554541202, 40.99863466993042493, 9.382169495545424454 ) ) ;
#97340 = LINE ( 'NONE', #6814, #92550 ) ;
#97339 = CARTESIAN_POINT ( 'NONE',  ( 0.5774900079438607392, 23.48035201082150536, 5.440088680355550821 ) ) ;
#97341 = CARTESIAN_POINT ( 'NONE',  ( 4.559911319644449179, 67.23035201082150536, -9.422509992056141925 ) ) ;
#97342 = CARTESIAN_POINT ( 'NONE',  ( 12.91533473730993009, 16.60535201082150891, -10.88017736071109987 ) ) ;
#97343 = ORIENTED_EDGE ( 'NONE', *, *, #15169, .T. ) ;
#97344 = ADVANCED_FACE ( 'NONE', ( #87190 ), #21379, .T. ) ;
#97345 = CARTESIAN_POINT ( 'NONE',  ( 10.00000000000000000, 57.87363466993042493, -12.81628187352647608 ) ) ;
#97346 = CARTESIAN_POINT ( 'NONE',  ( -0.8801773607110991993, 37.85535201082151247, -2.915334737309923874 ) ) ;
#97347 = CARTESIAN_POINT ( 'NONE',  ( 19.59355871817327710, 95.39900665025442095, 5.130928526377548593 ) ) ;
#97348 = CARTESIAN_POINT ( 'NONE',  ( 0.6178305044545838731, 54.74863466993042493, 9.382169495545420901 ) ) ;
#97349 = CARTESIAN_POINT ( 'NONE',  ( 10.00000000000000178, 49.31368534415484106, 10.88017736071110342 ) ) ;
#97350 = CARTESIAN_POINT ( 'NONE',  ( 2.791683348922240793, 61.63393115100079456, 7.208316651077764092 ) ) ;
#97351 = DIRECTION ( 'NONE',  ( 0.000000000000000000, -1.000000000000000000, 0.000000000000000000 ) ) ;
#97352 = CIRCLE ( 'NONE', #1577, 0.5000000000000000000 ) ;
#97353 = CARTESIAN_POINT ( 'NONE',  ( 10.00000000000000178, 22.25893115100078745, 9.846743663894594434 ) ) ;
#97354 = CARTESIAN_POINT ( 'NONE',  ( 22.81628187352647785, 6.415301336597088344, 3.434112377981063169 ) ) ;
#97356 = CARTESIAN_POINT ( 'NONE',  ( 19.84674366389459266, 58.71726448433411605, -2.638427012816827677 ) ) ;
#97355 = CYLINDRICAL_SURFACE ( 'NONE', #40466, 0.5000000000000004441 ) ;
#97357 = CARTESIAN_POINT ( 'NONE',  ( 17.96484262340118221, 19.93868534415484106, 7.964842623401181321 ) ) ;
#97358 = CARTESIAN_POINT ( 'NONE',  ( 14.92337183194729988, 54.34226448433412315, -8.527530157486177487 ) ) ;
#97359 = DIRECTION ( 'NONE',  ( 0.000000000000000000, 0.000000000000000000, -1.000000000000000000 ) ) ;
#97360 = CARTESIAN_POINT ( 'NONE',  ( 18.52753015748618282, 3.925597817667451306, -4.923371831947291888 ) ) ;
#97361 = CARTESIAN_POINT ( 'NONE',  ( -3.753761956877471384, 0.000000000000000000, -3.955639745193241019 ) ) ;
#97363 = VERTEX_POINT ( 'NONE', #64181 ) ;
#97362 = CARTESIAN_POINT ( 'NONE',  ( 0.1532563361054082862, 66.21726448433413736, 2.638427012816831674 ) ) ;
#97364 = DIRECTION ( 'NONE',  ( 1.000000000000000000, 0.000000000000000000, 0.000000000000000000 ) ) ;
#97365 =( NAMED_UNIT ( * ) SI_UNIT ( $, .STERADIAN. ) SOLID_ANGLE_UNIT ( ) );
#97366 = CARTESIAN_POINT ( 'NONE',  ( 22.81628187352647785, 36.62363466993041783, 6.195893100308588602E-16 ) ) ;
#97367 = CARTESIAN_POINT ( 'NONE',  ( 7.361572987183169658, 34.96726448433411605, -9.846743663894592657 ) ) ;
#97368 = CARTESIAN_POINT ( 'NONE',  ( 0.1077916266722445254, 12.24062864464239020, -6.478736007405951902 ) ) ;
#97369 = CARTESIAN_POINT ( 'NONE',  ( 17.96484262340118221, 6.188685344154837509, -7.964842623401177768 ) ) ;
#97370 = CARTESIAN_POINT ( 'NONE',  ( 10.00000000000000178, 37.25893115100078745, 9.846743663894594434 ) ) ;
#97371 = CYLINDRICAL_SURFACE ( 'NONE', #39230, 0.2500000000000002220 ) ;
#97372 = CARTESIAN_POINT ( 'NONE',  ( -0.8801773607111009756, 3.063685344154838397, 1.068504757029289695E-15 ) ) ;
#97373 = CARTESIAN_POINT ( 'NONE',  ( 1.274849032794102888, 3.572280503510291361, 6.499999999999721112 ) ) ;
#97374 = CARTESIAN_POINT ( 'NONE',  ( 2.035157376598824452, 23.68868534415484461, 7.964842623401179544 ) ) ;
#97375 = CARTESIAN_POINT ( 'NONE',  ( 22.26659068614894466, 43.88708216824729647, 7.082119434687054849 ) ) ;
#97377 = LINE ( 'NONE', #59348, #4803 ) ;
#97376 = CARTESIAN_POINT ( 'NONE',  ( 20.36894250292379382, 53.67874883491397497, 10.36894250292379205 ) ) ;
#97378 = CARTESIAN_POINT ( 'NONE',  ( -0.05723567505238607439, 69.83236346210668444, 6.413539670616451360 ) ) ;
#97379 = EDGE_CURVE ( 'NONE', #55236, #5883, #80180, .T. ) ;
#97380 = CARTESIAN_POINT ( 'NONE',  ( 17.20831665107776587, 9.133931151000787452, -7.208316651077762316 ) ) ;
#97381 = CARTESIAN_POINT ( 'NONE',  ( -1.099225684535947600, 4.540301336597087456, 6.408140936763237150 ) ) ;
#97382 = ORIENTED_EDGE ( 'NONE', *, *, #52405, .F. ) ;
#97383 = CARTESIAN_POINT ( 'NONE',  ( 7.084665262690076126, 54.10535201082151247, 10.88017736071109987 ) ) ;
#97384 = CARTESIAN_POINT ( 'NONE',  ( -12.83294900548073336, 14.49999999999999112, 7.766300266068329350 ) ) ;
#97385 = ADVANCED_FACE ( 'NONE', ( #63696 ), #69286, .T. ) ;
#97386 = DIRECTION ( 'NONE',  ( 1.000000000000000000, 0.000000000000000000, 0.000000000000000000 ) ) ;
#97387 = CARTESIAN_POINT ( 'NONE',  ( 69.60148758828984228, 0.4999999999999982792, 9.500000000000000000 ) ) ;
#97388 =( LENGTH_UNIT ( ) NAMED_UNIT ( * ) SI_UNIT ( .MILLI., .METRE. ) );
#97389 = CARTESIAN_POINT ( 'NONE',  ( 7.361572987183169658, 19.96726448433411960, -9.846743663894592657 ) ) ;
#97390 = DIRECTION ( 'NONE',  ( 0.000000000000000000, -0.000000000000000000, -1.000000000000000000 ) ) ;
#97391 = CARTESIAN_POINT ( 'NONE',  ( 6.204703633549690345, 40.76208216824731778, -14.16423886937410259 ) ) ;
#97392 = CARTESIAN_POINT ( 'NONE',  ( 19.84674366389459266, 8.300597817667451750, 2.638427012816836559 ) ) ;
#97394 = SURFACE_SIDE_STYLE ('',( #59366 ) ) ;
#97393 = CARTESIAN_POINT ( 'NONE',  ( -7.037799269744632547, -86.25965645050756336, -2.499999999999194422 ) ) ;
#97395 = CARTESIAN_POINT ( 'NONE',  ( 17.96484262340118221, 26.18868534415483396, -7.964842623401177768 ) ) ;
#97396 = CARTESIAN_POINT ( 'NONE',  ( 21.09922568453595559, 37.04030133659708923, -6.408140936763230044 ) ) ;
#97397 = CARTESIAN_POINT ( 'NONE',  ( -0.8801773607111009756, 8.063685344154837509, 1.068504757029289695E-15 ) ) ;
#97398 = CARTESIAN_POINT ( 'NONE',  ( 6.565887622018943937, 30.16530133659708568, 12.81628187352647430 ) ) ;
#97399 = CARTESIAN_POINT ( 'NONE',  ( 22.81628187352648496, 61.83196800326376774, -3.434112377981050290 ) ) ;
#97400 = ORIENTED_EDGE ( 'NONE', *, *, #58025, .T. ) ;
#97401 = CARTESIAN_POINT ( 'NONE',  ( 1.602071938427518161, 12.02224192338640130, -6.500000000000021316 ) ) ;
#97402 = EDGE_CURVE ( 'NONE', #63527, #46976, #65665, .T. ) ;
#97403 = CARTESIAN_POINT ( 'NONE',  ( -9.823941624389807004, -32.16601312911085842, -3.999999999999999112 ) ) ;
#97404 = CARTESIAN_POINT ( 'NONE',  ( -4.164238869374099039, 41.80374883491397497, 8.674139862899312516E-16 ) ) ;
#97405 = CARTESIAN_POINT ( 'NONE',  ( 20.36894250292379382, 3.678748834913967869, 10.36894250292379205 ) ) ;
#97406 = CARTESIAN_POINT ( 'NONE',  ( 12.91533473730992121, 4.522018677488169658, 10.88017736071110164 ) ) ;
#97407 = CARTESIAN_POINT ( 'NONE',  ( 10.00000000000000178, 19.31368534415484106, 10.88017736071110342 ) ) ;
#97408 = FACE_OUTER_BOUND ( 'NONE', #37655, .T. ) ;
#97409 = DIRECTION ( 'NONE',  ( 0.000000000000000000, 0.000000000000000000, 1.000000000000000000 ) ) ;
#97410 = CARTESIAN_POINT ( 'NONE',  ( 15.44008868035555793, 56.39701867748817676, -9.422509992056140149 ) ) ;
#97411 = CARTESIAN_POINT ( 'NONE',  ( 10.00000000000000000, 56.81368534415484106, -10.88017736071110342 ) ) ;
#97412 = CARTESIAN_POINT ( 'NONE',  ( 22.81628187352647785, 16.41530133659708923, 3.434112377981063169 ) ) ;
#97413 =( LENGTH_UNIT ( ) NAMED_UNIT ( * ) SI_UNIT ( .MILLI., .METRE. ) );
#97414 = DIRECTION ( 'NONE',  ( -0.000000000000000000, 1.000000000000000000, -0.000000000000000000 ) ) ;
#97415 = CARTESIAN_POINT ( 'NONE',  ( 0.1532563361054082862, 26.21726448433411605, 2.638427012816831674 ) ) ;
#97416 = CARTESIAN_POINT ( 'NONE',  ( 2.035157376598822676, 57.43868534415484106, -7.964842623401177768 ) ) ;
#97417 = UNCERTAINTY_MEASURE_WITH_UNIT (LENGTH_MEASURE( 1.000000000000000082E-05 ), #23265, 'distance_accuracy_value', 'NONE');
#97418 = CARTESIAN_POINT ( 'NONE',  ( 19.38216949554541557, 17.24863466993041783, -9.382169495545420901 ) ) ;
#97419 = FILL_AREA_STYLE_COLOUR ( '', #9038 ) ;
#97420 = CARTESIAN_POINT ( 'NONE',  ( 12.91533473730993009, 6.605352010821504471, -10.88017736071109987 ) ) ;
#97421 = CARTESIAN_POINT ( 'NONE',  ( 18.52753015748618282, 43.92559781766745175, -4.923371831947291888 ) ) ;
#97422 = CARTESIAN_POINT ( 'NONE',  ( 6.565887622018943937, 48.08196800326375353, -12.81628187352647608 ) ) ;
#97423 = CARTESIAN_POINT ( 'NONE',  ( 2.791683348922240793, 21.63393115100078745, 7.208316651077764092 ) ) ;
#97424 = CARTESIAN_POINT ( 'NONE',  ( -2.266590686148945544, 7.220415501580634832, 7.082119434687048631 ) ) ;
#97425 = DIRECTION ( 'NONE',  ( -1.000000000000000000, 0.000000000000000000, 0.000000000000000000 ) ) ;
#97426 = CARTESIAN_POINT ( 'NONE',  ( 4.559911319644449179, 17.23035201082150536, -9.422509992056141925 ) ) ;
#97428 = CARTESIAN_POINT ( 'NONE',  ( 2.917880565312950480, 30.97041550158063572, -12.26659068614894821 ) ) ;
#97427 = LINE ( 'NONE', #27913, #96761 ) ;
#97429 = CARTESIAN_POINT ( 'NONE',  ( 18.52753015748618282, 48.92559781766745886, -4.923371831947291888 ) ) ;
#97430 = VECTOR ( 'NONE', #66265, 1000.000000000000000 ) ;
#97431 = CARTESIAN_POINT ( 'NONE',  ( 12.91533473730992121, 19.52201867748816611, 10.88017736071110164 ) ) ;
#97432 = CARTESIAN_POINT ( 'NONE',  ( 20.88017736071110519, 10.56368534415483929, 2.639326808657452039E-16 ) ) ;
#97433 = ORIENTED_EDGE ( 'NONE', *, *, #35938, .T. ) ;
#97434 = AXIS2_PLACEMENT_3D ( 'NONE', #80839, #49350, #27335 ) ;
#97435 = CARTESIAN_POINT ( 'NONE',  ( 2.035157376598824452, 28.68868534415484106, 7.964842623401179544 ) ) ;
#97436 = AXIS2_PLACEMENT_3D ( 'NONE', #4740, #57716, #41759 ) ;
#97437 = CARTESIAN_POINT ( 'NONE',  ( 13.43411237798106583, 47.66530133659709634, -12.81628187352647252 ) ) ;
#97438 = EDGE_CURVE ( 'NONE', #68868, #8246, #55493, .T. ) ;
#97439 = CARTESIAN_POINT ( 'NONE',  ( 12.91533473730993009, 31.60535201082150891, -10.88017736071109987 ) ) ;
#97440 = CARTESIAN_POINT ( 'NONE',  ( 20.88017736071110519, 35.56368534415484106, 2.639326808657452039E-16 ) ) ;
#97441 = ORIENTED_EDGE ( 'NONE', *, *, #31434, .F. ) ;
#97442 = CARTESIAN_POINT ( 'NONE',  ( 17.20831665107776587, 52.88393115100078035, 7.208316651077764980 ) ) ;
#97443 = CARTESIAN_POINT ( 'NONE',  ( 19.42250999205614548, 30.98035201082150536, -5.440088680355545492 ) ) ;
#97444 = CARTESIAN_POINT ( 'NONE',  ( 4.380000001274070520, 0.08775168531748565870, 4.000000000000000000 ) ) ;
#97445 = FILL_AREA_STYLE ('',( #4384 ) ) ;
#97446 = CYLINDRICAL_SURFACE ( 'NONE', #76395, 0.5000000000000004441 ) ;
#97447 = CARTESIAN_POINT ( 'NONE',  ( -0.3689425029237881626, 52.42874883491396076, 10.36894250292379027 ) ) ;
#97448 = CARTESIAN_POINT ( 'NONE',  ( 7.084665262690076126, 57.02201867748817676, -10.88017736071110164 ) ) ;
#97449 = EDGE_CURVE ( 'NONE', #63997, #46284, #65169, .T. ) ;
#97450 = CARTESIAN_POINT ( 'NONE',  ( 10.00000000000000000, 64.75893115100078035, -9.846743663894594434 ) ) ;
#97451 = CARTESIAN_POINT ( 'NONE',  ( 8.439016546559823695, 15.00000000000000000, 11.79122553964979048 ) ) ;
#97452 = CARTESIAN_POINT ( 'NONE',  ( 14.92337183194729988, 64.34226448433412315, -8.527530157486177487 ) ) ;
#97453 = CARTESIAN_POINT ( 'NONE',  ( 19.84674366389459266, 3.717264484334118713, -2.638427012816827677 ) ) ;
#97454 = CARTESIAN_POINT ( 'NONE',  ( 0.1532563361054100626, 25.80059781766744820, -2.638427012816831230 ) ) ;
#97455 = VERTEX_POINT ( 'NONE', #95689 ) ;
#97456 = CARTESIAN_POINT ( 'NONE',  ( 18.52753015748618282, 23.92559781766745530, -4.923371831947291888 ) ) ;
#97457 = CARTESIAN_POINT ( 'NONE',  ( 9.382169495545419124, -14.00136533006957329, 9.382169495545417348 ) ) ;
#97458 = CARTESIAN_POINT ( 'NONE',  ( 0.5774900079438590739, 32.64701867748816966, -5.440088680355550821 ) ) ;
#97459 = CARTESIAN_POINT ( 'NONE',  ( 17.20831665107776587, 19.13393115100078035, -7.208316651077762316 ) ) ;
#97461 = CARTESIAN_POINT ( 'NONE',  ( -0.8801773607110991993, 57.85535201082149825, -2.915334737309923874 ) ) ;
#97460 = CARTESIAN_POINT ( 'NONE',  ( 20.88017736071110875, 65.77201867748817676, -2.915334737309920765 ) ) ;
#97463 = CARTESIAN_POINT ( 'NONE',  ( 13.43411237798106583, 62.66530133659708923, -12.81628187352647252 ) ) ;
#97462 = CARTESIAN_POINT ( 'NONE',  ( 15.44008868035555260, 29.73035201082150891, 9.422509992056143702 ) ) ;
#97464 = CARTESIAN_POINT ( 'NONE',  ( 13.79529636645031943, 45.34541550158062506, -14.16423886937409904 ) ) ;
#97465 = B_SPLINE_CURVE_WITH_KNOTS ( 'NONE', 3,
 ( #45439, #68454, #60931, #15938, #15465, #22461 ),
 .UNSPECIFIED., .F., .F.,
 ( 4, 2, 4 ),
 ( 3.409110551494480670E-05, 0.0004400426677367911253, 0.0008459942299586375048 ),
 .UNSPECIFIED. ) ;
#97466 = EDGE_CURVE ( 'NONE', #21190, #47609, #80065, .T. ) ;
#97467 = CARTESIAN_POINT ( 'NONE',  ( 21.92686044187657401, 35.37045670184114243, -3.195792623639525765 ) ) ;
#97468 = ORIENTED_EDGE ( 'NONE', *, *, #68437, .F. ) ;
#97469 = CARTESIAN_POINT ( 'NONE',  ( 13.43411237798105340, 5.581968003263753531, 12.81628187352647963 ) ) ;
#97470 = CARTESIAN_POINT ( 'NONE',  ( 20.88017736071110164, 5.355352010821502695, 2.915334737309930979 ) ) ;
#97471 = CARTESIAN_POINT ( 'NONE',  ( 10.00000000000000178, 49.31368534415484106, 10.88017736071110342 ) ) ;
#97473 = EDGE_CURVE ( 'NONE', #93536, #56519, #96187, .T. ) ;
#97472 = CARTESIAN_POINT ( 'NONE',  ( 17.85158348494336167, 24.73726573380441351, -6.499999999999992895 ) ) ;
#97474 = ORIENTED_EDGE ( 'NONE', *, *, #53534, .T. ) ;
#97475 = CARTESIAN_POINT ( 'NONE',  ( 18.52753015748618282, 13.92559781766745175, -4.923371831947291888 ) ) ;
#97476 = CARTESIAN_POINT ( 'NONE',  ( 20.88017736071110164, 60.35535201082151957, 2.915334737309930979 ) ) ;
#97477 = CARTESIAN_POINT ( 'NONE',  ( 7.361572987183169658, 34.96726448433411605, -9.846743663894592657 ) ) ;
#97478 = CARTESIAN_POINT ( 'NONE',  ( 17.20831665107776587, 22.88393115100078745, 7.208316651077764980 ) ) ;
#97479 = CARTESIAN_POINT ( 'NONE',  ( 10.00000000000000178, 17.25893115100078745, 9.846743663894594434 ) ) ;
#97481 = CARTESIAN_POINT ( 'NONE',  ( -2.816281873526471635, 43.91530133659708923, -3.434112377981056508 ) ) ;
#97480 = CARTESIAN_POINT ( 'NONE',  ( 2.603489959281613420, 50.43575266056826933, -6.500000000000031086 ) ) ;
#97483 = LINE ( 'NONE', #58969, #30754 ) ;
#97482 = CARTESIAN_POINT ( 'NONE',  ( 5.076628168052704559, 5.175597817667451750, -8.527530157486179263 ) ) ;
#97484 = CARTESIAN_POINT ( 'NONE',  ( 11.35644480889443386, -65.08008077083093212, 3.750000000000000000 ) ) ;
#97486 = ORIENTED_EDGE ( 'NONE', *, *, #5168, .F. ) ;
#97485 = CARTESIAN_POINT ( 'NONE',  ( 19.84674366389459621, 28.50893115100078745, 7.409399052514197653E-17 ) ) ;
#97487 = VECTOR ( 'NONE', #19184, 1000.000000000000000 ) ;
#97488 = CARTESIAN_POINT ( 'NONE',  ( 22.81628187352647785, 56.62363466993042493, 6.195893100308588602E-16 ) ) ;
#97489 = PLANE ( 'NONE',  #39023 ) ;
#97490 = CARTESIAN_POINT ( 'NONE',  ( 3.591859063236761518, -0.04303199673624671928, 11.09922568453594849 ) ) ;
#97491 = CARTESIAN_POINT ( 'NONE',  ( 12.91533473730992121, 4.522018677488169658, 10.88017736071110164 ) ) ;
#97492 = CARTESIAN_POINT ( 'NONE',  ( 13.79529636645030344, 18.26208216824730002, 14.16423886937410614 ) ) ;
#97493 = TOROIDAL_SURFACE ( 'NONE', #9684, 10.09999999999999787, 0.1000000000000000056 ) ;
#97494 = UNCERTAINTY_MEASURE_WITH_UNIT (LENGTH_MEASURE( 1.000000000000000082E-05 ), #4906, 'distance_accuracy_value', 'NONE');
#97495 = FACE_OUTER_BOUND ( 'NONE', #69154, .T. ) ;
#97496 = CARTESIAN_POINT ( 'NONE',  ( -2.266590686148945544, 36.38708216824730357, -7.082119434687050408 ) ) ;
#97497 = CIRCLE ( 'NONE', #49570, 20.49999999999999645 ) ;
#97498 = CARTESIAN_POINT ( 'NONE',  ( 17.08211943468705130, 43.47041550158063927, 12.26659068614894998 ) ) ;
#97499 = CARTESIAN_POINT ( 'NONE',  ( -2.266590686148945544, 16.38708216824730357, -7.082119434687050408 ) ) ;
#97501 = CARTESIAN_POINT ( 'NONE',  ( 2.618367889266248100E-15, 44.99999999999999289, 7.000000000000000000 ) ) ;
#97500 = CARTESIAN_POINT ( 'NONE',  ( 24.16423886937410614, 14.30374883491396787, 8.672049930838204340E-16 ) ) ;
#97502 = CARTESIAN_POINT ( 'NONE',  ( 7.084665262690076126, 49.10535201082149825, 10.88017736071109987 ) ) ;
#97503 = CARTESIAN_POINT ( 'NONE',  ( 6.829574850499570360, -88.00372650123708240, -2.750000000000000000 ) ) ;
#97504 = CARTESIAN_POINT ( 'NONE',  ( 14.92337183194729633, 32.67559781766745175, 8.527530157486181039 ) ) ;
#97507 = AXIS2_PLACEMENT_3D ( 'NONE', #73833, #74318, #58327 ) ;
#97506 = CARTESIAN_POINT ( 'NONE',  ( 5.076628168052704559, 25.17559781766745175, -8.527530157486179263 ) ) ;
#97505 = CARTESIAN_POINT ( 'NONE',  ( 20.88017736071110519, 65.56368534415483396, 2.639326808657452039E-16 ) ) ;
#97508 = CARTESIAN_POINT ( 'NONE',  ( 20.88017736071110164, 15.35535201082150358, 2.915334737309930979 ) ) ;
#97509 = CARTESIAN_POINT ( 'NONE',  ( 10.00000000000000178, 65.37363466993042493, 12.81628187352647608 ) ) ;
#97510 = CARTESIAN_POINT ( 'NONE',  ( 0.1532563361054100626, 50.80059781766745175, -2.638427012816831230 ) ) ;
#97511 = CARTESIAN_POINT ( 'NONE',  ( 18.00000000000000355, 77.07179676972445748, 4.250000000000000000 ) ) ;
#97512 = EDGE_CURVE ( 'NONE', #15924, #84126, #19685, .T. ) ;
#97513 = CARTESIAN_POINT ( 'NONE',  ( 1.472469842513823179, 25.59226448433412315, -4.923371831947296329 ) ) ;
#97514 = CARTESIAN_POINT ( 'NONE',  ( 21.09922568453595559, 42.04030133659708213, -6.408140936763230044 ) ) ;
#97515 = CARTESIAN_POINT ( 'NONE',  ( -3.795296366450322534, -24.23791783175269643, -14.16423886937409904 ) ) ;
#97516 = CARTESIAN_POINT ( 'NONE',  ( -0.8801773607110991993, 42.85535201082150536, -2.915334737309923874 ) ) ;
#97517 = CARTESIAN_POINT ( 'NONE',  ( 14.92337183194729988, 34.34226448433411605, -8.527530157486177487 ) ) ;
#97518 = CARTESIAN_POINT ( 'NONE',  ( 24.16423886937410614, 29.30374883491396787, 8.672049930838204340E-16 ) ) ;
#97519 = ORIENTED_EDGE ( 'NONE', *, *, #38608, .T. ) ;
#97520 = CARTESIAN_POINT ( 'NONE',  ( -4.164238869374099927, 7.012082168247302683, 3.795296366450308767 ) ) ;
#97521 = CARTESIAN_POINT ( 'NONE',  ( 2.035157376598822676, 57.43868534415484106, -7.964842623401177768 ) ) ;
#97522 = CARTESIAN_POINT ( 'NONE',  ( 15.44008868035555793, 61.39701867748817676, -9.422509992056140149 ) ) ;
#97523 = CARTESIAN_POINT ( 'NONE',  ( -0.3689425029237881626, 62.42874883491396787, 10.36894250292379027 ) ) ;
#97524 = CARTESIAN_POINT ( 'NONE',  ( -2.816281873526473856, -0.8763653300695799508, 9.499525473075851096E-16 ) ) ;
#97525 = CARTESIAN_POINT ( 'NONE',  ( 17.96484262340118221, 56.18868534415484817, -7.964842623401177768 ) ) ;
#97526 = CARTESIAN_POINT ( 'NONE',  ( -0.1503990784575263973, 27.22266099184919241, -6.262539305110081500 ) ) ;
#97527 = TOROIDAL_SURFACE ( 'NONE', #33603, 14.49999999999999822, 0.5000000000000000000 ) ;
#97528 = CARTESIAN_POINT ( 'NONE',  ( 16.40814093676324603, 32.45696800326375353, -11.09922568453594671 ) ) ;
#97529 = CARTESIAN_POINT ( 'NONE',  ( 19.84674366389459266, 63.30059781766745886, 2.638427012816836559 ) ) ;
#97530 = CARTESIAN_POINT ( 'NONE',  ( -9.422509992056145478, 27.64701867748817321, -5.440088680355541939 ) ) ;
#97531 = CARTESIAN_POINT ( 'NONE',  ( 10.00000000000000000, 6.813685344154838397, -10.88017736071110342 ) ) ;
#97532 = CARTESIAN_POINT ( 'NONE',  ( 20.88017736071110875, 10.77201867748817143, -2.915334737309920765 ) ) ;
#97533 = CARTESIAN_POINT ( 'NONE',  ( 1.472469842513823179, 36.42559781766745175, 4.923371831947296329 ) ) ;
#97534 = CARTESIAN_POINT ( 'NONE',  ( 2.148416515056618792, 42.23726573380440641, 6.499999999999959144 ) ) ;
#97535 = ORIENTED_EDGE ( 'NONE', *, *, #2514, .T. ) ;
#97536 =( GEOMETRIC_REPRESENTATION_CONTEXT ( 3 ) GLOBAL_UNCERTAINTY_ASSIGNED_CONTEXT ( ( #78455 ) ) GLOBAL_UNIT_ASSIGNED_CONTEXT ( ( #74105, #12625, #82108 ) ) REPRESENTATION_CONTEXT ( 'NONE', 'WORKASPACE' ) );
#97537 = CARTESIAN_POINT ( 'NONE',  ( 10.00000000000000000, 1.813685344154837731, -10.88017736071110342 ) ) ;
#97538 = CARTESIAN_POINT ( 'NONE',  ( 16.40814093676323893, 10.79030133659708923, 11.09922568453595026 ) ) ;
#97539 = CARTESIAN_POINT ( 'NONE',  ( 2.791683348922237240, 10.38393115100078390, -7.208316651077763204 ) ) ;
#97540 = CIRCLE ( 'NONE', #54392, 1.499999999999998668 ) ;
#97541 = CARTESIAN_POINT ( 'NONE',  ( 10.00000000000000178, 52.25893115100078745, 9.846743663894594434 ) ) ;
#97542 = CARTESIAN_POINT ( 'NONE',  ( 0.5774900079438590739, 42.64701867748816966, -5.440088680355550821 ) ) ;
#97543 = CARTESIAN_POINT ( 'NONE',  ( -2.816281873526471635, 13.91530133659708746, -3.434112377981056508 ) ) ;
#97545 = CARTESIAN_POINT ( 'NONE',  ( 19.72487221294571569, 25.71833443783938478, -6.499999999999989342 ) ) ;
#97544 = CARTESIAN_POINT ( 'NONE',  ( 20.88017736071110164, 55.35535201082149825, 2.915334737309930979 ) ) ;
#97546 = EDGE_CURVE ( 'NONE', #62023, #41634, #67706, .T. ) ;
#97547 = DIRECTION ( 'NONE',  ( 0.000000000000000000, 1.000000000000000000, -0.000000000000000000 ) ) ;
#97548 = CARTESIAN_POINT ( 'NONE',  ( 22.81628187352648496, 46.83196800326376064, -3.434112377981050290 ) ) ;
#97549 = EDGE_LOOP ( 'NONE', ( #88073, #62118, #62223 ) ) ;
#97550 = CARTESIAN_POINT ( 'NONE',  ( 10.00000000000000178, 69.31368534415484817, 10.88017736071110342 ) ) ;
#97552 = CARTESIAN_POINT ( 'NONE',  ( 20.36894250292379382, 8.678748834913967869, 10.36894250292379205 ) ) ;
#97551 = CARTESIAN_POINT ( 'NONE',  ( 6.565887622018943937, 38.08196800326376064, -12.81628187352647608 ) ) ;
#97553 = DIRECTION ( 'NONE',  ( 0.000000000000000000, 0.000000000000000000, 1.000000000000000000 ) ) ;
#97554 = CARTESIAN_POINT ( 'NONE',  ( 19.42250999205614548, 40.98035201082150536, -5.440088680355545492 ) ) ;
#97555 = CARTESIAN_POINT ( 'NONE',  ( 2.791683348922240793, 66.63393115100079456, 7.208316651077764092 ) ) ;
#97556 = CARTESIAN_POINT ( 'NONE',  ( 5.076628168052704559, 50.17559781766745886, -8.527530157486179263 ) ) ;
#97557 = CARTESIAN_POINT ( 'NONE',  ( 1.472469842513823179, 16.42559781766745175, 4.923371831947296329 ) ) ;
#97558 = CARTESIAN_POINT ( 'NONE',  ( 1.472469842513823179, 5.592264484334118713, -4.923371831947296329 ) ) ;
#97559 = DIRECTION ( 'NONE',  ( 1.257568779154408793E-17, 1.000000000000000000, -0.000000000000000000 ) ) ;
#97560 = CARTESIAN_POINT ( 'NONE',  ( 20.36894250292379382, 48.67874883491396076, 10.36894250292379205 ) ) ;
#97561 = CARTESIAN_POINT ( 'NONE',  ( 0.000000000000000000, 15.00000000000000000, 0.000000000000000000 ) ) ;
#97562 = DIRECTION ( 'NONE',  ( -0.3173046564050965856, 0.000000000000000000, 0.9483236552061978797 ) ) ;
#97563 = CARTESIAN_POINT ( 'NONE',  ( 0.2751277870542986892, 7.282175860852375671, -6.500000000000003553 ) ) ;
#97564 = ORIENTED_EDGE ( 'NONE', *, *, #72137, .F. ) ;
#97565 = CARTESIAN_POINT ( 'NONE',  ( -4.164238869374099039, 61.80374883491397497, 8.674139862899312516E-16 ) ) ;
#97566 = CARTESIAN_POINT ( 'NONE',  ( 13.79529636645031943, 60.34541550158063927, -14.16423886937409904 ) ) ;
#97567 = CARTESIAN_POINT ( 'NONE',  ( 5.076628168052704559, 25.17559781766745175, -8.527530157486179263 ) ) ;
#97568 = CARTESIAN_POINT ( 'NONE',  ( 10.00000000000000178, 25.37363466993041783, 12.81628187352647608 ) ) ;
#97569 = DIRECTION ( 'NONE',  ( -0.000000000000000000, -1.000000000000000000, -0.000000000000000000 ) ) ;
#97571 = CARTESIAN_POINT ( 'NONE',  ( 20.36894250292379382, 3.678748834913967869, 10.36894250292379205 ) ) ;
#97570 = CARTESIAN_POINT ( 'NONE',  ( -1.926860441876562247, 42.45379003517447813, -3.195792623639530650 ) ) ;
#97572 = CARTESIAN_POINT ( 'NONE',  ( 7.084665262690076126, 17.02201867748817676, -10.88017736071110164 ) ) ;
#97573 = CARTESIAN_POINT ( 'NONE',  ( 24.16423886937409904, 59.09541550158063217, 3.795296366450317205 ) ) ;
#97574 = EDGE_CURVE ( 'NONE', #1911, #72785, #87679, .T. ) ;
#97575 = EDGE_CURVE ( 'NONE', #76622, #2401, #33201, .T. ) ;
#97576 = CARTESIAN_POINT ( 'NONE',  ( 19.84674366389459621, 33.50893115100078745, 7.409399052514197653E-17 ) ) ;
#97577 = CARTESIAN_POINT ( 'NONE',  ( -15.00000000000000000, 83.99999999999998579, 7.750000000000000000 ) ) ;
#97578 = CARTESIAN_POINT ( 'NONE',  ( 1.472469842513823179, 11.42559781766745175, 4.923371831947296329 ) ) ;
#97579 = PRESENTATION_LAYER_ASSIGNMENT (  '', '', ( #87976 ) ) ;
#97580 = CARTESIAN_POINT ( 'NONE',  ( 0.000000000000000000, 15.00000000000000000, 0.000000000000000000 ) ) ;
#97581 = CARTESIAN_POINT ( 'NONE',  ( -4.923371831947302546, 20.17559781766745175, -8.527530157486173934 ) ) ;
#97582 = ORIENTED_EDGE ( 'NONE', *, *, #97402, .F. ) ;
#97583 = EDGE_LOOP ( 'NONE', ( #24407, #56035, #93250, #90137 ) ) ;
#97584 = DIRECTION ( 'NONE',  ( 0.000000000000000000, 0.000000000000000000, 1.000000000000000000 ) ) ;
#97585 = ORIENTED_EDGE ( 'NONE', *, *, #97325, .T. ) ;
#97586 = CARTESIAN_POINT ( 'NONE',  ( 5.076628168052703671, 46.84226448433412315, 8.527530157486179263 ) ) ;
#97587 = CARTESIAN_POINT ( 'NONE',  ( -4.164238869374099927, 17.01208216824730357, 3.795296366450308767 ) ) ;
#97589 = CARTESIAN_POINT ( 'NONE',  ( 7.084665262690076126, 29.10535201082150181, 10.88017736071109987 ) ) ;
#97588 = CARTESIAN_POINT ( 'NONE',  ( 4.559911319644449179, 22.23035201082150536, -9.422509992056141925 ) ) ;
#97591 = CARTESIAN_POINT ( 'NONE',  ( 10.00000000000000000, 22.87363466993042138, -12.81628187352647608 ) ) ;
#97590 = CARTESIAN_POINT ( 'NONE',  ( 2.791683348922240793, 61.63393115100079456, 7.208316651077764092 ) ) ;
#97592 = CARTESIAN_POINT ( 'NONE',  ( 6.204703633549690345, 5.762082168247301794, -14.16423886937410259 ) ) ;
#97593 = CARTESIAN_POINT ( 'NONE',  ( 20.88017736071110875, 65.77201867748817676, -2.915334737309920765 ) ) ;
#97594 = EDGE_CURVE ( 'NONE', #75712, #63730, #72668, .T. ) ;
#97595 = CARTESIAN_POINT ( 'NONE',  ( 21.09922568453594849, 36.20696800326375353, 6.408140936763242479 ) ) ;
#97596 = VERTEX_POINT ( 'NONE', #27670 ) ;
#97597 = CARTESIAN_POINT ( 'NONE',  ( 14.92337183194729988, 34.34226448433411605, -8.527530157486177487 ) ) ;
#97598 = CARTESIAN_POINT ( 'NONE',  ( -0.3689425029237881626, 67.42874883491396076, 10.36894250292379027 ) ) ;
#97599 = ORIENTED_EDGE ( 'NONE', *, *, #68918, .T. ) ;
#97600 = EDGE_CURVE ( 'NONE', #60663, #90632, #93246, .T. ) ;
#97601 = CARTESIAN_POINT ( 'NONE',  ( 0.5774900079438590739, 7.647018677488171434, -5.440088680355550821 ) ) ;
#97602 = EDGE_LOOP ( 'NONE', ( #55909, #21123, #24146, #64470 ) ) ;
#97603 = CARTESIAN_POINT ( 'NONE',  ( 4.559911319644449179, 53.89701867748817676, 9.422509992056141925 ) ) ;
#97604 = CARTESIAN_POINT ( 'NONE',  ( 10.00000000000000178, 64.31368534415483396, 10.88017736071110342 ) ) ;
#97605 = CARTESIAN_POINT ( 'NONE',  ( -0.8801773607111009756, 68.06368534415484817, 1.068504757029289695E-15 ) ) ;
#97606 = CARTESIAN_POINT ( 'NONE',  ( -13.55255535720598026, -0.03417435944610275333, 4.403492169842870396 ) ) ;
#97607 = CARTESIAN_POINT ( 'NONE',  ( 12.91533473730992121, 59.52201867748816966, 10.88017736071110164 ) ) ;
#97608 = TOROIDAL_SURFACE ( 'NONE', #33678, 7.250000000000002665, 0.2500000000000000000 ) ;
#97609 = CIRCLE ( 'NONE', #41775, 0.09999999999999982514 ) ;
#97610 = DIRECTION ( 'NONE',  ( 0.000000000000000000, 0.000000000000000000, -1.000000000000000000 ) ) ;
#97611 = EDGE_CURVE ( 'NONE', #13980, #47708, #89164, .T. ) ;
#97613 = ORIENTED_EDGE ( 'NONE', *, *, #73553, .T. ) ;
#97612 = CARTESIAN_POINT ( 'NONE',  ( 10.09974179616572521, -32.02510747888860010, 4.000000000000000000 ) ) ;
#97614 = CARTESIAN_POINT ( 'NONE',  ( 10.00000000000000000, 24.75893115100078745, -9.846743663894594434 ) ) ;
#97615 = ORIENTED_EDGE ( 'NONE', *, *, #66486, .F. ) ;
#97616 = CARTESIAN_POINT ( 'NONE',  ( 18.52753015748618282, 53.92559781766745175, -4.923371831947291888 ) ) ;
#97617 = CARTESIAN_POINT ( 'NONE',  ( -36.44000000000001194, 92.00000000000000000, -9.500000000000000000 ) ) ;
#97618 = CARTESIAN_POINT ( 'NONE',  ( -4.164238869374098151, 6.595415501580634832, -3.795296366450310543 ) ) ;
#97619 = DIRECTION ( 'NONE',  ( 0.000000000000000000, 0.000000000000000000, -1.000000000000000000 ) ) ;
#97620 = CARTESIAN_POINT ( 'NONE',  ( 19.89220837332775815, 29.74062864464239553, 6.478736007405959008 ) ) ;
#97621 = CARTESIAN_POINT ( 'NONE',  ( 14.97653319723437626, 15.00000000000000000, 5.619684139539351975 ) ) ;
#97622 = CARTESIAN_POINT ( 'NONE',  ( 10.00000000000000178, 4.313685344154837509, 10.88017736071110342 ) ) ;
#97623 = CARTESIAN_POINT ( 'NONE',  ( 64.56412365047461321, 29.50000000000000000, 10.00000000000000000 ) ) ;
#97624 = ORIENTED_EDGE ( 'NONE', *, *, #67090, .T. ) ;
#97625 = CARTESIAN_POINT ( 'NONE',  ( 9.282040431732685448, 15.00000000000000711, -11.30407325590339696 ) ) ;
#97626 = CARTESIAN_POINT ( 'NONE',  ( 12.63842701281683034, 52.46726448433413026, 9.846743663894596210 ) ) ;
#97627 = CARTESIAN_POINT ( 'NONE',  ( 0.6178305044545818747, 13.49863466993041783, -9.382169495545419124 ) ) ;
#97628 = CARTESIAN_POINT ( 'NONE',  ( 17.20831665107776587, 12.88393115100078390, 7.208316651077764980 ) ) ;
#97629 = DIRECTION ( 'NONE',  ( -0.000000000000000000, -1.000000000000000000, -0.000000000000000000 ) ) ;
#97630 = CARTESIAN_POINT ( 'NONE',  ( 19.38216949554541202, 0.9986346699304200492, 9.382169495545424454 ) ) ;
#97631 = CYLINDRICAL_SURFACE ( 'NONE', #70715, 1.249999999999987121 ) ;
#97632 = AXIS2_PLACEMENT_3D ( 'NONE', #12640, #66129, #97653 ) ;
#97633 = ORIENTED_EDGE ( 'NONE', *, *, #50729, .T. ) ;
#97634 = CARTESIAN_POINT ( 'NONE',  ( 7.084665262690076126, 4.105352010821503583, 10.88017736071109987 ) ) ;
#97635 = CARTESIAN_POINT ( 'NONE',  ( -4.164238869374099039, 16.80374883491396787, 8.674139862899312516E-16 ) ) ;
#97636 = CARTESIAN_POINT ( 'NONE',  ( 14.92337183194729988, 24.34226448433411960, -8.527530157486177487 ) ) ;
#97637 = CARTESIAN_POINT ( 'NONE',  ( 17.96484262340118221, 61.18868534415482685, -7.964842623401177768 ) ) ;
#97639 = CARTESIAN_POINT ( 'NONE',  ( -10.14667048435130781, 4.359436697371537845E-16, -10.35833375027055148 ) ) ;
#97638 = CARTESIAN_POINT ( 'NONE',  ( 3.591859063236763294, 38.29030133659708923, -11.09922568453595026 ) ) ;
#97640 = CARTESIAN_POINT ( 'NONE',  ( 10.00000000000000178, 19.31368534415484106, 10.88017736071110342 ) ) ;
#97641 = FACE_OUTER_BOUND ( 'NONE', #33335, .T. ) ;
#97642 = CARTESIAN_POINT ( 'NONE',  ( 0.000000000000000000, 14.49999999999999822, 0.000000000000000000 ) ) ;
#97643 = CARTESIAN_POINT ( 'NONE',  ( 16.40814093676324603, 12.45696800326375353, -11.09922568453594671 ) ) ;
#97644 = CARTESIAN_POINT ( 'NONE',  ( 0.1532563361054083140, 66.00893115100079456, 1.131784320476157264E-15 ) ) ;
#97645 = CARTESIAN_POINT ( 'NONE',  ( 19.84674366389459266, 28.30059781766745886, 2.638427012816836559 ) ) ;
#97646 = CARTESIAN_POINT ( 'NONE',  ( -7.964842623401179544, -7.561314655845157162, -7.964842623401174215 ) ) ;
#97647 = CARTESIAN_POINT ( 'NONE',  ( -1.099225684535947600, 34.54030133659708923, 6.408140936763237150 ) ) ;
#97648 = DIRECTION ( 'NONE',  ( 0.000000000000000000, 1.000000000000000000, -0.000000000000000000 ) ) ;
#97649 = AXIS2_PLACEMENT_3D ( 'NONE', #91631, #77109, #70608 ) ;
#97651 = CARTESIAN_POINT ( 'NONE',  ( -15.61289147378506748, 15.00000000000000000, -3.480663193108890496 ) ) ;
#97650 = CARTESIAN_POINT ( 'NONE',  ( 15.44008868035555793, 46.39701867748817676, -9.422509992056140149 ) ) ;
#97652 = EDGE_CURVE ( 'NONE', #33114, #98886, #5403, .T. ) ;
#97653 = DIRECTION ( 'NONE',  ( 1.000000000000000000, 0.000000000000000000, 0.000000000000000000 ) ) ;
#97654 = CARTESIAN_POINT ( 'NONE',  ( 7.084665262690076126, 44.10535201082151247, 10.88017736071109987 ) ) ;
#97655 = CARTESIAN_POINT ( 'NONE',  ( 7.084665262690076126, 34.10535201082151247, 10.88017736071109987 ) ) ;
#97656 = CARTESIAN_POINT ( 'NONE',  ( 19.84674366389459266, 63.30059781766745886, 2.638427012816836559 ) ) ;
#97657 = CARTESIAN_POINT ( 'NONE',  ( -0.8801773607111008646, 58.27201867748816966, 2.915334737309923430 ) ) ;
#97658 = CARTESIAN_POINT ( 'NONE',  ( 5.076628168052703671, 41.84226448433411605, 8.527530157486179263 ) ) ;
#97659 = CARTESIAN_POINT ( 'NONE',  ( 15.44008868035555260, 9.730352010821505360, 9.422509992056143702 ) ) ;
#97660 = CARTESIAN_POINT ( 'NONE',  ( -2.816281873526473856, 14.12363466993041961, 9.499525473075851096E-16 ) ) ;
#97661 = ORIENTED_EDGE ( 'NONE', *, *, #4652, .T. ) ;
#97662 = CARTESIAN_POINT ( 'NONE',  ( 10.00000000000000000, 26.81368534415484106, -10.88017736071110342 ) ) ;
#97663 = LINE ( 'NONE', #89641, #76528 ) ;
#97664 = CARTESIAN_POINT ( 'NONE',  ( -0.8801773607111008646, 3.272018677488171434, 2.915334737309923430 ) ) ;
#97665 = CARTESIAN_POINT ( 'NONE',  ( 0.5774900079438590739, 22.64701867748817321, -5.440088680355550821 ) ) ;
#97666 = CARTESIAN_POINT ( 'NONE',  ( 15.44008868035555793, 66.39701867748817676, -9.422509992056140149 ) ) ;
#97667 = CARTESIAN_POINT ( 'NONE',  ( 13.79529636645031943, 20.34541550158063572, -14.16423886937409904 ) ) ;
#97668 = CARTESIAN_POINT ( 'NONE',  ( 18.52753015748618282, 18.92559781766745175, -4.923371831947291888 ) ) ;
#97669 = CARTESIAN_POINT ( 'NONE',  ( -0.8801773607111009756, 43.06368534415484106, 1.068504757029289695E-15 ) ) ;
#97670 = FACE_OUTER_BOUND ( 'NONE', #12382, .T. ) ;
#97671 = FACE_OUTER_BOUND ( 'NONE', #64584, .T. ) ;
#97672 = EDGE_CURVE ( 'NONE', #47550, #66028, #74146, .T. ) ;
#97673 = PRESENTATION_LAYER_ASSIGNMENT (  '', '', ( #22651 ) ) ;
#97674 = EDGE_LOOP ( 'NONE', ( #57274, #89090, #55495, #9032 ) ) ;
#97675 = CARTESIAN_POINT ( 'NONE',  ( -6.349999999999995204, -97.00000000000000000, 4.000000000000000000 ) ) ;
#97676 = CARTESIAN_POINT ( 'NONE',  ( 17.20831665107776587, 47.88393115100078745, 7.208316651077764980 ) ) ;
#97678 = ORIENTED_EDGE ( 'NONE', *, *, #11165, .T. ) ;
#97677 = EDGE_CURVE ( 'NONE', #39990, #16062, #94401, .T. ) ;
#97679 = ORIENTED_EDGE ( 'NONE', *, *, #56725, .T. ) ;
#97680 = FILL_AREA_STYLE_COLOUR ( '', #15053 ) ;
#97681 = CARTESIAN_POINT ( 'NONE',  ( 22.26659068614895176, 19.72041550158063572, -7.082119434687042414 ) ) ;
#97682 = CARTESIAN_POINT ( 'NONE',  ( -4.164238869374099039, 26.80374883491397142, 8.674139862899312516E-16 ) ) ;
#97683 = CARTESIAN_POINT ( 'NONE',  ( 15.44008868035555793, 61.39701867748817676, -9.422509992056140149 ) ) ;
#97684 = CARTESIAN_POINT ( 'NONE',  ( 6.204703633549690345, 62.84541550158063927, 14.16423886937410082 ) ) ;
#97685 = CARTESIAN_POINT ( 'NONE',  ( 6.565887622018943937, 5.165301336597086568, 12.81628187352647430 ) ) ;
#97686 = CARTESIAN_POINT ( 'NONE',  ( 19.84674366389459266, 53.30059781766744464, 2.638427012816836559 ) ) ;
#97688 = CARTESIAN_POINT ( 'NONE',  ( 6.565887622018943937, 10.16530133659708746, 12.81628187352647430 ) ) ;
#97687 = CARTESIAN_POINT ( 'NONE',  ( 15.44008868035555793, 51.39701867748816966, -9.422509992056140149 ) ) ;
#97689 = CARTESIAN_POINT ( 'NONE',  ( 13.79529636645031943, 10.34541550158063394, -14.16423886937409904 ) ) ;
#97690 = CARTESIAN_POINT ( 'NONE',  ( -0.8801773607111009756, 13.06368534415483929, 1.068504757029289695E-15 ) ) ;
#97691 = EDGE_CURVE ( 'NONE', #14505, #52889, #5185, .T. ) ;
#97692 = CARTESIAN_POINT ( 'NONE',  ( 4.559911319644449179, 23.89701867748817321, 9.422509992056141925 ) ) ;
#97693 = DIRECTION ( 'NONE',  ( -0.000000000000000000, -0.000000000000000000, -1.000000000000000000 ) ) ;
#97694 = CARTESIAN_POINT ( 'NONE',  ( 12.91533473730992121, 44.52201867748816966, 10.88017736071110164 ) ) ;
#97695 = CARTESIAN_POINT ( 'NONE',  ( 13.43411237798105340, 50.58196800326375353, 12.81628187352647963 ) ) ;
#97696 = CARTESIAN_POINT ( 'NONE',  ( -2.638427012816824124, -27.94940218233254470, 9.846743663894596210 ) ) ;
#97697 = EDGE_LOOP ( 'NONE', ( #29708, #85803, #465, #44647 ) ) ;
#97698 = CARTESIAN_POINT ( 'NONE',  ( -3.750000000000000888, 1.019547802438453887, -3.750000000000000000 ) ) ;
#97699 = VERTEX_POINT ( 'NONE', #52154 ) ;
#97700 = EDGE_LOOP ( 'NONE', ( #33200, #81785 ) ) ;
#97701 = CARTESIAN_POINT ( 'NONE',  ( -7.232415441807423129, -88.12698951299773853, 4.000000000000000000 ) ) ;
#97703 = CARTESIAN_POINT ( 'NONE',  ( 2.035157376598824452, 8.688685344154839285, 7.964842623401179544 ) ) ;
#97702 = CARTESIAN_POINT ( 'NONE',  ( 2.917880565312948704, 47.63708216824730357, 12.26659068614894643 ) ) ;
#97705 = CARTESIAN_POINT ( 'NONE',  ( 0.1532563361054100626, 45.80059781766745886, -2.638427012816831230 ) ) ;
#97704 = CARTESIAN_POINT ( 'NONE',  ( 14.92337183194729988, 24.34226448433411960, -8.527530157486177487 ) ) ;
#97706 = CARTESIAN_POINT ( 'NONE',  ( 8.879999999999991900, 20.99999999999999645, 1.249999999999987121 ) ) ;
#97707 = DIRECTION ( 'NONE',  ( -0.000000000000000000, -1.000000000000000000, -0.000000000000000000 ) ) ;
#97708 = AXIS2_PLACEMENT_3D ( 'NONE', #86079, #55582, #10081 ) ;
#97709 = CARTESIAN_POINT ( 'NONE',  ( 19.84674366389459266, 3.717264484334118713, -2.638427012816827677 ) ) ;
#97710 = VECTOR ( 'NONE', #23825, 1000.000000000000000 ) ;
#97711 = B_SPLINE_CURVE_WITH_KNOTS ( 'NONE', 3,
 ( #26553, #33068, #3584, #41589 ),
 .UNSPECIFIED., .F., .F.,
 ( 4, 4 ),
 ( 1.283695372222837250E-16, 0.001060528352562002848 ),
 .UNSPECIFIED. ) ;
#97712 = CARTESIAN_POINT ( 'NONE',  ( 3.434112377981054287, 22.66530133659709634, -12.81628187352647608 ) ) ;
#97713 = VERTEX_POINT ( 'NONE', #51670 ) ;
#97714 = AXIS2_PLACEMENT_3D ( 'NONE', #23806, #92765, #61768 ) ;
#97715 = CARTESIAN_POINT ( 'NONE',  ( 6.204703633549690345, 27.84541550158063217, 14.16423886937410082 ) ) ;
#97716 = ADVANCED_FACE ( 'NONE', ( #20675 ), #18248, .T. ) ;
#97717 = CARTESIAN_POINT ( 'NONE',  ( 0.6178305044545818747, 18.49863466993041428, -9.382169495545419124 ) ) ;
#97718 = ORIENTED_EDGE ( 'NONE', *, *, #14589, .F. ) ;
#97719 = CARTESIAN_POINT ( 'NONE',  ( 16.40814093676324603, 42.45696800326375353, -11.09922568453594671 ) ) ;
#97720 = CARTESIAN_POINT ( 'NONE',  ( 20.88017736071110875, 15.77201867748817143, -2.915334737309920765 ) ) ;
#97721 = CARTESIAN_POINT ( 'NONE',  ( 1.472469842513823179, 40.59226448433411605, -4.923371831947296329 ) ) ;
#97722 = CARTESIAN_POINT ( 'NONE',  ( -0.8801773607111009756, 18.06368534415484106, 1.068504757029289695E-15 ) ) ;
#97723 = CIRCLE ( 'NONE', #37040, 15.00000000000000000 ) ;
#97724 = CARTESIAN_POINT ( 'NONE',  ( 6.565887622018943937, 63.08196800326376064, -12.81628187352647608 ) ) ;
#97725 = CARTESIAN_POINT ( 'NONE',  ( -5.038135815954129626, 0.000000000000000000, 2.086864184045826853 ) ) ;
#97726 = CARTESIAN_POINT ( 'NONE',  ( 17.20831665107776587, 47.88393115100078745, 7.208316651077764980 ) ) ;
#97727 = CARTESIAN_POINT ( 'NONE',  ( 0.1532563361054100626, 55.80059781766745175, -2.638427012816831230 ) ) ;
#97728 = EDGE_CURVE ( 'NONE', #15789, #92979, #74652, .T. ) ;
#97730 = ORIENTED_EDGE ( 'NONE', *, *, #90908, .F. ) ;
#97729 = DIRECTION ( 'NONE',  ( 0.9762960071199331402, -0.000000000000000000, 0.2164396139381037087 ) ) ;
#97731 = VERTEX_POINT ( 'NONE', #28168 ) ;
#97732 = LINE ( 'NONE', #29193, #10985 ) ;
#97733 = DIRECTION ( 'NONE',  ( -0.000000000000000000, -1.000000000000000000, -0.000000000000000000 ) ) ;
#97734 = SURFACE_SIDE_STYLE ('',( #60680 ) ) ;
#97735 = CARTESIAN_POINT ( 'NONE',  ( 17.20831665107776587, 14.13393115100078568, -7.208316651077762316 ) ) ;
#97736 = CARTESIAN_POINT ( 'NONE',  ( 6.565887622018943937, 43.08196800326374643, -12.81628187352647608 ) ) ;
#97737 = DIRECTION ( 'NONE',  ( -1.000000000000000000, 0.000000000000000000, 0.000000000000000000 ) ) ;
#97738 = ORIENTED_EDGE ( 'NONE', *, *, #40647, .F. ) ;
#97739 = CARTESIAN_POINT ( 'NONE',  ( 10.00000000000000178, 52.25893115100078745, 9.846743663894594434 ) ) ;
#97740 = CARTESIAN_POINT ( 'NONE',  ( -14.35840480524203855, 0.3640475087720986824, 4.340070442838750431 ) ) ;
#97741 = CARTESIAN_POINT ( 'NONE',  ( 24.16423886937410614, 34.51208216824731068, -3.795296366450302550 ) ) ;
#97742 = CARTESIAN_POINT ( 'NONE',  ( 10.00000000000000000, 44.75893115100078745, -9.846743663894594434 ) ) ;
#97743 = CARTESIAN_POINT ( 'NONE',  ( 19.38216949554541557, 52.24863466993041072, -9.382169495545420901 ) ) ;
#97745 = SURFACE_STYLE_USAGE ( .BOTH. , #66217 ) ;
#97744 = CARTESIAN_POINT ( 'NONE',  ( -4.431036607602702126, 14.49999999999999112, 14.33059365769913462 ) ) ;
#97746 = CARTESIAN_POINT ( 'NONE',  ( 17.20831665107776587, 7.883931151000784787, 7.208316651077764980 ) ) ;
#97747 = DIRECTION ( 'NONE',  ( 0.000000000000000000, 0.000000000000000000, 1.000000000000000000 ) ) ;
#97748 = CARTESIAN_POINT ( 'NONE',  ( 5.076628168052703671, 51.84226448433412315, 8.527530157486179263 ) ) ;
#97749 = CARTESIAN_POINT ( 'NONE',  ( 20.88017736071110875, 40.77201867748818387, -2.915334737309920765 ) ) ;
#97750 = DIRECTION ( 'NONE',  ( -0.8616291604415232674, 0.000000000000000000, -0.5075383629607084224 ) ) ;
#97751 = STYLED_ITEM ( 'NONE', ( #54021 ), #81586 ) ;
#97752 = CARTESIAN_POINT ( 'NONE',  ( 10.00000000000000000, 41.81368534415484106, -10.88017736071110342 ) ) ;
#97753 = ORIENTED_EDGE ( 'NONE', *, *, #26485, .T. ) ;
#97754 = LINE ( 'NONE', #35740, #12242 ) ;
#97755 = CARTESIAN_POINT ( 'NONE',  ( 20.88017736071110875, 20.77201867748816611, -2.915334737309920765 ) ) ;
#97757 = CARTESIAN_POINT ( 'NONE',  ( 0.5774900079438607392, 38.48035201082150536, 5.440088680355550821 ) ) ;
#97756 = CARTESIAN_POINT ( 'NONE',  ( 22.81628187352647785, 6.415301336597088344, 3.434112377981063169 ) ) ;
#97758 = CARTESIAN_POINT ( 'NONE',  ( -0.1503990784575294781, 48.10158574516642460, 6.262539305110072618 ) ) ;
#97759 = CARTESIAN_POINT ( 'NONE',  ( 19.42250999205614193, 65.14701867748817676, 5.440088680355555262 ) ) ;
#97760 = CARTESIAN_POINT ( 'NONE',  ( 13.40508947812163143, 15.00000000000000000, 5.527528931046191474 ) ) ;
#97762 = CARTESIAN_POINT ( 'NONE',  ( -46.76855771576528298, 100.6387111820534415, 9.385180859874349579 ) ) ;
#97761 = CARTESIAN_POINT ( 'NONE',  ( -0.8801773607110991993, 32.85535201082151247, -2.915334737309923874 ) ) ;
#97763 = CARTESIAN_POINT ( 'NONE',  ( 0.1532563361054100626, 10.80059781766745175, -2.638427012816831230 ) ) ;
#97764 = EDGE_CURVE ( 'NONE', #26202, #37993, #7612, .T. ) ;
#97765 = CARTESIAN_POINT ( 'NONE',  ( 10.00000000000000178, 27.25893115100078390, 9.846743663894594434 ) ) ;
#97766 = CARTESIAN_POINT ( 'NONE',  ( -7.750000000000000000, 40.74999999999999289, 4.250000000000000000 ) ) ;
#97767 =( BOUNDED_SURFACE ( )  B_SPLINE_SURFACE ( 1, 2, ( 
 ( #51075, #66576, #94734, #73567, #66070, #63732, #96598, #13074, #97103, #94232, #25764, #41269, #36439, #74419, #6424, #28440, #66932, #21439, #89437, #97453, #66433, #96968, #58937, #20950, #51437, #81927, #13435, #86613, #17633, #56116, #78617, #48104, #10126, #79099, #9627, #40623, #71121, #18123, #48595, #40126, #70626, #2154, #53166, #45668, #38661, #30644, #22684, #83670, #53657, #46166, #61153, #76165, #91663, #689, #31142, #7686, #38183, #3996, #72848, #79882, #56409, #62910, #33382, #71419, #17916, #48400, #55417, #41426, #3408, #24935, #40919, #47413, #33869, #34370, #18405, #71887, #77914, #48887, #93412, #78903, #63400, #10412, #85925, #40429, #18904, #17434, #47902, #26384, #64376, #93906, #2935, #78406, #64860, #63880, #79399, #26881, #94391, #9423, #86895, #32901, #41910, #95380, #25907, #9925, #94885, #70925, #2445, #25433, #85423, #55916, #86415, #56883, #10904, #87386, #16933, #49381, #11388, #70428, #72371, #3902, #39926, #1947, #32409, #28838, #57374, #12857, #19869, #89356, #28361, #66346, #74337, #95889, #59340, #20373, #81359, #20866, #19385, #67347, #27857, #35857, #50867, #42876, #44339, #43355, #36356, #51851, #49869, #6345, #21358, #65857, #73853, #58345, #5383, #74845, #4886, #12370, #89843, #82339, #57862, #96885, #88864, #97873, #87869, #27369, #66851, #42386, #50363, #88373, #80872, #13859, #58850, #51357, #81842, #96385, #36856, #13356, #73359, #43841, #5862, #35364, #97370, #80383, #11883, #72863, #4398, #34867, #65360, #61314, #84338, #90324, #91826, #6846, #22848, #7353, #91321, #37358, #83336, #61805, #98369, #67851, #69325, #46325, #37854, #53322, #90828, #10174, #83829, #23344, #71171, #15356, #21863, #30816, #75832, #86172, #78668, #7844, #29825, #38831, #52830, #60335, #22354, #40672, #14860, #45333, #845, #38341, #68344, #29333, #31304, #53826, #14358, #45841, #15840, #76812, #68836, #59831, #93659, #52342, #76325, #98865, #8327, #367, #25195, #55672, #30319, #17681, #48155, #82837, #44827, #75333, #60821, #72133, #80130, #95126, #87134, #88611, #26634, #80633, #96137, #94149, #50624, #65610, #11146, #57132, #3660, #87629, #20121, #49146, #56649, #35111, #27618, #3167, #19143, #34124, #43118, #2696, #41177, #12129, #86661, #94645, #33629, #71658, #58105, #49619, #42152, #64616, #41665, #81115, #72617, #64128, #11637, #12617, #63642, #33148, #4152, #42630, #34617, #10662, #25676, #26155, #56170, #65114, #79149, #95635, #27122, #18658, #18166, #57623, #88121, #19632, #50123, #48646, #73108, #79648, #4649, #91080, #35621, #53083, #74602, #83092, #29095, #81602, #15109, #43609, #68101 ),
 ( #28111, #21118, #67611, #13113, #52106, #5131, #98117, #22110, #98628, #5629, #51617, #30079, #75592, #36107, #44598, #97630, #74096, #82099, #22605, #83594, #13612, #44092, #45087, #7104, #66612, #14621, #66105, #96635, #97140, #52591, #6115, #73606, #60586, #36620, #67106, #59595, #82598, #37607, #29578, #90092, #60082, #58611, #90585, #89113, #14114, #21619, #75094, #20625, #28610, #6601, #37114, #51114, #59099, #89608, #31065, #47556, #70558, #38105, #16577, #1095, #84579, #77548, #31557, #39578, #92556, #25074, #68595, #46566, #85562, #92074, #54064, #38587, #2085, #47052, #16079, #122, #15601, #46086, #32545, #30572, #7611, #78054, #63046, #53573, #23102, #8578, #69575, #62542, #84087, #62053, #39081, #9067, #61564, #76572, #9557, #70070, #40058, #93542, #55556, #17073, #61074, #23600, #1591, #8091, #24082, #76083, #32040, #93048, #86058, #69085, #77065, #45586, #91587, #619, #24582, #54549, #85067, #55043, #34996, #96021, #64015, #26047, #88008, #19520, #10544, #27013, #10059, #40557, #56054, #95520, #56537, #65499, #42518, #94527, #87027, #11035, #95012, #64994, #42043, #18539, #72507, #4532, #34502, #27502, #26521, #49030, #34011, #57511, #79031, #79535, #41557, #72021, #50016, #57017, #3065, #80520, #73001, #71057, #87519, #3550, #64508, #49510, #19033, #11519, #80017, #57998, #2581, #4040, #12018, #17569, #48035, #41054, #78547, #33036, #63532, #94040, #86547, #18054, #25563, #48531, #71553, #33519, #44970, #96523, #65995, #51493, #13499, #6485, #27995, #43978, #81987, #21498, #73989, #58492, #90465, #82484, #22000, #6990, #37494, #21006, #74981, #67982, #29464, #20510, #66991, #50995, #43008, #35500, #81490, #36992, #73490, #74482, #97514, #28977, #59970, #82980, #97022, #89003, #52475, #12993, #28499, #43489, #6004, #98509, #5516, #36499, #58993, #29963, #59480, #66496, #89981, #67488, #35993, #89495, #51995, #14002, #98010, #44479, #14500, #75475, #88504, #81006, #20007, #50508, #12507, #5017, #15962, #54437, #8457, #39941, #52963, #61448, #1470, #7977, #68969, #53455, #16948, #31437, #500, #14996, #30455, #60954, #47433, #45466, #22490, #62424, #77932, #68480, #37988, #23484, #84464, #77430, #6, #46454, #53957, #92440, #45972, #91463, #92927, #84946, #24459, #9440, #70444, #91954, #46937, #1961, #31924, #22989, #38963, #83962, #75966, #7494, #15489, #8942, #76462, #76947, #69456, #974, #54925, #85441, #30949, #38476, #60469, #61938, #23963, #16457, #39461, #90958, #69951, #83474, #2949, #72388, #85941, #78919, #26398, #70945, #10917, #62928, #56898, #79897, #26898, #63421, #10429, #87883, #34385 ) ),
 .UNSPECIFIED., .F., .F., .F. ) 
 B_SPLINE_SURFACE_WITH_KNOTS ( ( 2, 2 ),
 ( 3, 2, 2, 2, 2, 2, 2, 2, 2, 2, 2, 2, 2, 2, 2, 2, 2, 2, 2, 2, 2, 2, 2, 2, 2, 2, 2, 2, 2, 2, 2, 2, 2, 2, 2, 2, 2, 2, 2, 2, 2, 2, 2, 2, 2, 2, 2, 2, 2, 2, 2, 2, 2, 2, 2, 2, 2, 2, 2, 2, 2, 2, 2, 2, 2, 2, 2, 2, 2, 2, 2, 2, 2, 2, 2, 2, 2, 2, 2, 2, 2, 2, 2, 2, 2, 2, 2, 2, 2, 2, 2, 2, 2, 2, 2, 2, 2, 2, 2, 2, 2, 2, 2, 2, 2, 2, 2, 2, 2, 2, 2, 2, 2, 2, 2, 2, 2, 2, 2, 2, 2, 2, 2, 2, 2, 2, 2, 2, 2, 2, 2, 2, 2, 2, 2, 2, 2, 2, 2, 2, 2, 2, 2, 2, 2, 2, 2, 2, 2, 2, 2, 2, 2, 2, 2, 2, 2, 2, 2, 2, 2, 2, 3 ),
 ( 0.000000000000000000, 1.000000000000000000 ),
 ( 0.000000000000000000, 0.005952380952380952051, 0.01190476190476190410, 0.01785714285714285615, 0.02380952380952380820, 0.02976190476190476025, 0.03571428571428571230, 0.04166666666666666435, 0.04761904761904761640, 0.05357142857142856845, 0.05952380952380952051, 0.06547619047619047949, 0.07142857142857142461, 0.07738095238095238360, 0.08333333333333332871, 0.08928571428571428770, 0.09523809523809523281, 0.1011904761904761918, 0.1071428571428571369, 0.1130952380952380959, 0.1190476190476190410, 0.1250000000000000000, 0.1309523809523809590, 0.1369047619047619180, 0.1428571428571428492, 0.1488095238095238082, 0.1547619047619047672, 0.1607142857142857262, 0.1666666666666666574, 0.1726190476190476164, 0.1785714285714285754, 0.1845238095238095344, 0.1904761904761904656, 0.1964285714285714246, 0.2023809523809523836, 0.2083333333333333426, 0.2142857142857142738, 0.2202380952380952328, 0.2261904761904761918, 0.2321428571428571508, 0.2380952380952380820, 0.2440476190476190410, 0.2500000000000000000, 0.2559523809523809312, 0.2619047619047619180, 0.2678571428571428492, 0.2738095238095238360, 0.2797619047619047672, 0.2857142857142856984, 0.2916666666666666852, 0.2976190476190476164, 0.3035714285714285476, 0.3095238095238095344, 0.3154761904761904656, 0.3214285714285714524, 0.3273809523809523836, 0.3333333333333333148, 0.3392857142857143016, 0.3452380952380952328, 0.3511904761904761640, 0.3571428571428571508, 0.3630952380952380820, 0.3690476190476190688, 0.3750000000000000000, 0.3809523809523809312, 0.3869047619047619180, 0.3928571428571428492, 0.3988095238095238360, 0.4047619047619047672, 0.4107142857142856984, 0.4166666666666666852, 0.4226190476190476164, 0.4285714285714285476, 0.4345238095238095344, 0.4404761904761904656, 0.4464285714285714524, 0.4523809523809523836, 0.4583333333333333148, 0.4642857142857143016, 0.4702380952380952328, 0.4761904761904761640, 0.4821428571428571508, 0.4880952380952380820, 0.4940476190476190688, 0.5000000000000000000, 0.5059523809523809312, 0.5119047619047618625, 0.5178571428571429047, 0.5238095238095238360, 0.5297619047619047672, 0.5357142857142856984, 0.5416666666666666297, 0.5476190476190476719, 0.5535714285714286031, 0.5595238095238095344, 0.5654761904761904656, 0.5714285714285713969, 0.5773809523809523281, 0.5833333333333333703, 0.5892857142857143016, 0.5952380952380952328, 0.6011904761904761640, 0.6071428571428570953, 0.6130952380952381375, 0.6190476190476190688, 0.6250000000000000000, 0.6309523809523809312, 0.6369047619047618625, 0.6428571428571429047, 0.6488095238095238360, 0.6547619047619047672, 0.6607142857142856984, 0.6666666666666666297, 0.6726190476190476719, 0.6785714285714286031, 0.6845238095238095344, 0.6904761904761904656, 0.6964285714285713969, 0.7023809523809523281, 0.7083333333333333703, 0.7142857142857143016, 0.7202380952380952328, 0.7261904761904761640, 0.7321428571428570953, 0.7380952380952381375, 0.7440476190476190688, 0.7500000000000000000, 0.7559523809523809312, 0.7619047619047618625, 0.7678571428571429047, 0.7738095238095238360, 0.7797619047619047672, 0.7857142857142856984, 0.7916666666666666297, 0.7976190476190476719, 0.8035714285714286031, 0.8095238095238095344, 0.8154761904761904656, 0.8214285714285713969, 0.8273809523809523281, 0.8333333333333333703, 0.8392857142857143016, 0.8452380952380952328, 0.8511904761904761640, 0.8571428571428570953, 0.8630952380952381375, 0.8690476190476190688, 0.8750000000000000000, 0.8809523809523809312, 0.8869047619047618625, 0.8928571428571429047, 0.8988095238095238360, 0.9047619047619047672, 0.9107142857142856984, 0.9166666666666666297, 0.9226190476190476719, 0.9285714285714286031, 0.9345238095238095344, 0.9404761904761904656, 0.9464285714285713969, 0.9523809523809523281, 0.9583333333333333703, 0.9642857142857143016 ),
 .UNSPECIFIED. ) 
 GEOMETRIC_REPRESENTATION_ITEM ( )  RATIONAL_B_SPLINE_SURFACE ( (
 ( 1.000000000000000000, 0.9659258262890683122, 1.000000000000000000, 0.9659258262890683122, 1.000000000000000000, 0.9659258262890683122, 1.000000000000000000, 0.9659258262890683122, 1.000000000000000000, 0.9659258262890683122, 1.000000000000000000, 0.9659258262890683122, 1.000000000000000000, 0.9659258262890683122, 1.000000000000000000, 0.9659258262890683122, 1.000000000000000000, 0.9659258262890683122, 1.000000000000000000, 0.9659258262890683122, 1.000000000000000000, 0.9659258262890683122, 1.000000000000000000, 0.9659258262890683122, 1.000000000000000000, 0.9659258262890683122, 1.000000000000000000, 0.9659258262890683122, 1.000000000000000000, 0.9659258262890683122, 1.000000000000000000, 0.9659258262890683122, 1.000000000000000000, 0.9659258262890683122, 1.000000000000000000, 0.9659258262890683122, 1.000000000000000000, 0.9659258262890683122, 1.000000000000000000, 0.9659258262890683122, 1.000000000000000000, 0.9659258262890683122, 1.000000000000000000, 0.9659258262890683122, 1.000000000000000000, 0.9659258262890683122, 1.000000000000000000, 0.9659258262890683122, 1.000000000000000000, 0.9659258262890683122, 1.000000000000000000, 0.9659258262890683122, 1.000000000000000000, 0.9659258262890683122, 1.000000000000000000, 0.9659258262890683122, 1.000000000000000000, 0.9659258262890683122, 1.000000000000000000, 0.9659258262890683122, 1.000000000000000000, 0.9659258262890683122, 1.000000000000000000, 0.9659258262890683122, 1.000000000000000000, 0.9659258262890683122, 1.000000000000000000, 0.9659258262890683122, 1.000000000000000000, 0.9659258262890683122, 1.000000000000000000, 0.9659258262890683122, 1.000000000000000000, 0.9659258262890683122, 1.000000000000000000, 0.9659258262890683122, 1.000000000000000000, 0.9659258262890683122, 1.000000000000000000, 0.9659258262890683122, 1.000000000000000000, 0.9659258262890683122, 1.000000000000000000, 0.9659258262890683122, 1.000000000000000000, 0.9659258262890683122, 1.000000000000000000, 0.9659258262890683122, 1.000000000000000000, 0.9659258262890683122, 1.000000000000000000, 0.9659258262890683122, 1.000000000000000000, 0.9659258262890683122, 1.000000000000000000, 0.9659258262890683122, 1.000000000000000000, 0.9659258262890683122, 1.000000000000000000, 0.9659258262890683122, 1.000000000000000000, 0.9659258262890683122, 1.000000000000000000, 0.9659258262890683122, 1.000000000000000000, 0.9659258262890683122, 1.000000000000000000, 0.9659258262890683122, 1.000000000000000000, 0.9659258262890683122, 1.000000000000000000, 0.9659258262890683122, 1.000000000000000000, 0.9659258262890683122, 1.000000000000000000, 0.9659258262890683122, 1.000000000000000000, 0.9659258262890683122, 1.000000000000000000, 0.9659258262890683122, 1.000000000000000000, 0.9659258262890683122, 1.000000000000000000, 0.9659258262890683122, 1.000000000000000000, 0.9659258262890683122, 1.000000000000000000, 0.9659258262890683122, 1.000000000000000000, 0.9659258262890683122, 1.000000000000000000, 0.9659258262890683122, 1.000000000000000000, 0.9659258262890683122, 1.000000000000000000, 0.9659258262890683122, 1.000000000000000000, 0.9659258262890683122, 1.000000000000000000, 0.9659258262890683122, 1.000000000000000000, 0.9659258262890683122, 1.000000000000000000, 0.9659258262890683122, 1.000000000000000000, 0.9659258262890683122, 1.000000000000000000, 0.9659258262890683122, 1.000000000000000000, 0.9659258262890683122, 1.000000000000000000, 0.9659258262890683122, 1.000000000000000000, 0.9659258262890683122, 1.000000000000000000, 0.9659258262890683122, 1.000000000000000000, 0.9659258262890683122, 1.000000000000000000, 0.9659258262890683122, 1.000000000000000000, 0.9659258262890683122, 1.000000000000000000, 0.9659258262890683122, 1.000000000000000000, 0.9659258262890683122, 1.000000000000000000, 0.9659258262890683122, 1.000000000000000000, 0.9659258262890683122, 1.000000000000000000, 0.9659258262890683122, 1.000000000000000000, 0.9659258262890683122, 1.000000000000000000, 0.9659258262890683122, 1.000000000000000000, 0.9659258262890683122, 1.000000000000000000, 0.9659258262890683122, 1.000000000000000000, 0.9659258262890683122, 1.000000000000000000, 0.9659258262890683122, 1.000000000000000000, 0.9659258262890683122, 1.000000000000000000, 0.9659258262890683122, 1.000000000000000000, 0.9659258262890683122, 1.000000000000000000, 0.9659258262890683122, 1.000000000000000000, 0.9659258262890683122, 1.000000000000000000, 0.9659258262890683122, 1.000000000000000000, 0.9659258262890683122, 1.000000000000000000, 0.9659258262890683122, 1.000000000000000000, 0.9659258262890683122, 1.000000000000000000, 0.9659258262890683122, 1.000000000000000000, 0.9659258262890683122, 1.000000000000000000, 0.9659258262890683122, 1.000000000000000000, 0.9659258262890683122, 1.000000000000000000, 0.9659258262890683122, 1.000000000000000000, 0.9659258262890683122, 1.000000000000000000, 0.9659258262890683122, 1.000000000000000000, 0.9659258262890683122, 1.000000000000000000, 0.9659258262890683122, 1.000000000000000000, 0.9659258262890683122, 1.000000000000000000, 0.9659258262890683122, 1.000000000000000000, 0.9659258262890683122, 1.000000000000000000, 0.9659258262890683122, 1.000000000000000000, 0.9659258262890683122, 1.000000000000000000, 0.9659258262890683122, 1.000000000000000000, 0.9659258262890683122, 1.000000000000000000, 0.9659258262890683122, 1.000000000000000000, 0.9659258262890683122, 1.000000000000000000, 0.9659258262890683122, 1.000000000000000000, 0.9659258262890683122, 1.000000000000000000, 0.9659258262890683122, 1.000000000000000000, 0.9659258262890683122, 1.000000000000000000, 0.9659258262890683122, 1.000000000000000000, 0.9659258262890683122, 1.000000000000000000, 0.9659258262890683122, 1.000000000000000000, 0.9659258262890683122, 1.000000000000000000, 0.9659258262890683122, 1.000000000000000000, 0.9659258262890683122, 1.000000000000000000, 0.9659258262890683122, 1.000000000000000000, 0.9659258262890683122, 1.000000000000000000, 0.9659258262890683122, 1.000000000000000000, 0.9659258262890683122, 1.000000000000000000, 0.9659258262890683122, 1.000000000000000000, 0.9659258262890683122, 1.000000000000000000, 0.9659258262890683122, 1.000000000000000000, 0.9659258262890683122, 1.000000000000000000, 0.9659258262890683122, 1.000000000000000000, 0.9659258262890683122, 1.000000000000000000, 0.9659258262890683122, 1.000000000000000000, 0.9659258262890683122, 1.000000000000000000, 0.9659258262890683122, 1.000000000000000000, 0.9659258262890683122, 1.000000000000000000, 0.9659258262890683122, 1.000000000000000000, 0.9659258262890683122, 1.000000000000000000, 0.9659258262890683122, 1.000000000000000000, 0.9659258262890683122, 1.000000000000000000, 0.9659258262890683122, 1.000000000000000000, 0.9659258262890683122, 1.000000000000000000, 0.9659258262890683122, 1.000000000000000000, 0.9659258262890683122, 1.000000000000000000, 0.9659258262890683122, 1.000000000000000000, 0.9659258262890683122, 1.000000000000000000, 0.9659258262890683122, 1.000000000000000000, 0.9659258262890683122, 1.000000000000000000, 0.9659258262890683122, 1.000000000000000000, 0.9659258262890683122, 1.000000000000000000, 0.9659258262890683122, 1.000000000000000000, 0.9659258262890683122, 1.000000000000000000, 0.9659258262890683122, 1.000000000000000000, 0.9659258262890683122, 1.000000000000000000, 0.9659258262890683122, 1.000000000000000000),
 ( 1.000000000000000000, 0.9659258262890683122, 1.000000000000000000, 0.9659258262890683122, 1.000000000000000000, 0.9659258262890683122, 1.000000000000000000, 0.9659258262890683122, 1.000000000000000000, 0.9659258262890683122, 1.000000000000000000, 0.9659258262890683122, 1.000000000000000000, 0.9659258262890683122, 1.000000000000000000, 0.9659258262890683122, 1.000000000000000000, 0.9659258262890683122, 1.000000000000000000, 0.9659258262890683122, 1.000000000000000000, 0.9659258262890683122, 1.000000000000000000, 0.9659258262890683122, 1.000000000000000000, 0.9659258262890683122, 1.000000000000000000, 0.9659258262890683122, 1.000000000000000000, 0.9659258262890683122, 1.000000000000000000, 0.9659258262890683122, 1.000000000000000000, 0.9659258262890683122, 1.000000000000000000, 0.9659258262890683122, 1.000000000000000000, 0.9659258262890683122, 1.000000000000000000, 0.9659258262890683122, 1.000000000000000000, 0.9659258262890683122, 1.000000000000000000, 0.9659258262890683122, 1.000000000000000000, 0.9659258262890683122, 1.000000000000000000, 0.9659258262890683122, 1.000000000000000000, 0.9659258262890683122, 1.000000000000000000, 0.9659258262890683122, 1.000000000000000000, 0.9659258262890683122, 1.000000000000000000, 0.9659258262890683122, 1.000000000000000000, 0.9659258262890683122, 1.000000000000000000, 0.9659258262890683122, 1.000000000000000000, 0.9659258262890683122, 1.000000000000000000, 0.9659258262890683122, 1.000000000000000000, 0.9659258262890683122, 1.000000000000000000, 0.9659258262890683122, 1.000000000000000000, 0.9659258262890683122, 1.000000000000000000, 0.9659258262890683122, 1.000000000000000000, 0.9659258262890683122, 1.000000000000000000, 0.9659258262890683122, 1.000000000000000000, 0.9659258262890683122, 1.000000000000000000, 0.9659258262890683122, 1.000000000000000000, 0.9659258262890683122, 1.000000000000000000, 0.9659258262890683122, 1.000000000000000000, 0.9659258262890683122, 1.000000000000000000, 0.9659258262890683122, 1.000000000000000000, 0.9659258262890683122, 1.000000000000000000, 0.9659258262890683122, 1.000000000000000000, 0.9659258262890683122, 1.000000000000000000, 0.9659258262890683122, 1.000000000000000000, 0.9659258262890683122, 1.000000000000000000, 0.9659258262890683122, 1.000000000000000000, 0.9659258262890683122, 1.000000000000000000, 0.9659258262890683122, 1.000000000000000000, 0.9659258262890683122, 1.000000000000000000, 0.9659258262890683122, 1.000000000000000000, 0.9659258262890683122, 1.000000000000000000, 0.9659258262890683122, 1.000000000000000000, 0.9659258262890683122, 1.000000000000000000, 0.9659258262890683122, 1.000000000000000000, 0.9659258262890683122, 1.000000000000000000, 0.9659258262890683122, 1.000000000000000000, 0.9659258262890683122, 1.000000000000000000, 0.9659258262890683122, 1.000000000000000000, 0.9659258262890683122, 1.000000000000000000, 0.9659258262890683122, 1.000000000000000000, 0.9659258262890683122, 1.000000000000000000, 0.9659258262890683122, 1.000000000000000000, 0.9659258262890683122, 1.000000000000000000, 0.9659258262890683122, 1.000000000000000000, 0.9659258262890683122, 1.000000000000000000, 0.9659258262890683122, 1.000000000000000000, 0.9659258262890683122, 1.000000000000000000, 0.9659258262890683122, 1.000000000000000000, 0.9659258262890683122, 1.000000000000000000, 0.9659258262890683122, 1.000000000000000000, 0.9659258262890683122, 1.000000000000000000, 0.9659258262890683122, 1.000000000000000000, 0.9659258262890683122, 1.000000000000000000, 0.9659258262890683122, 1.000000000000000000, 0.9659258262890683122, 1.000000000000000000, 0.9659258262890683122, 1.000000000000000000, 0.9659258262890683122, 1.000000000000000000, 0.9659258262890683122, 1.000000000000000000, 0.9659258262890683122, 1.000000000000000000, 0.9659258262890683122, 1.000000000000000000, 0.9659258262890683122, 1.000000000000000000, 0.9659258262890683122, 1.000000000000000000, 0.9659258262890683122, 1.000000000000000000, 0.9659258262890683122, 1.000000000000000000, 0.9659258262890683122, 1.000000000000000000, 0.9659258262890683122, 1.000000000000000000, 0.9659258262890683122, 1.000000000000000000, 0.9659258262890683122, 1.000000000000000000, 0.9659258262890683122, 1.000000000000000000, 0.9659258262890683122, 1.000000000000000000, 0.9659258262890683122, 1.000000000000000000, 0.9659258262890683122, 1.000000000000000000, 0.9659258262890683122, 1.000000000000000000, 0.9659258262890683122, 1.000000000000000000, 0.9659258262890683122, 1.000000000000000000, 0.9659258262890683122, 1.000000000000000000, 0.9659258262890683122, 1.000000000000000000, 0.9659258262890683122, 1.000000000000000000, 0.9659258262890683122, 1.000000000000000000, 0.9659258262890683122, 1.000000000000000000, 0.9659258262890683122, 1.000000000000000000, 0.9659258262890683122, 1.000000000000000000, 0.9659258262890683122, 1.000000000000000000, 0.9659258262890683122, 1.000000000000000000, 0.9659258262890683122, 1.000000000000000000, 0.9659258262890683122, 1.000000000000000000, 0.9659258262890683122, 1.000000000000000000, 0.9659258262890683122, 1.000000000000000000, 0.9659258262890683122, 1.000000000000000000, 0.9659258262890683122, 1.000000000000000000, 0.9659258262890683122, 1.000000000000000000, 0.9659258262890683122, 1.000000000000000000, 0.9659258262890683122, 1.000000000000000000, 0.9659258262890683122, 1.000000000000000000, 0.9659258262890683122, 1.000000000000000000, 0.9659258262890683122, 1.000000000000000000, 0.9659258262890683122, 1.000000000000000000, 0.9659258262890683122, 1.000000000000000000, 0.9659258262890683122, 1.000000000000000000, 0.9659258262890683122, 1.000000000000000000, 0.9659258262890683122, 1.000000000000000000, 0.9659258262890683122, 1.000000000000000000, 0.9659258262890683122, 1.000000000000000000, 0.9659258262890683122, 1.000000000000000000, 0.9659258262890683122, 1.000000000000000000, 0.9659258262890683122, 1.000000000000000000, 0.9659258262890683122, 1.000000000000000000, 0.9659258262890683122, 1.000000000000000000, 0.9659258262890683122, 1.000000000000000000, 0.9659258262890683122, 1.000000000000000000, 0.9659258262890683122, 1.000000000000000000, 0.9659258262890683122, 1.000000000000000000, 0.9659258262890683122, 1.000000000000000000, 0.9659258262890683122, 1.000000000000000000, 0.9659258262890683122, 1.000000000000000000, 0.9659258262890683122, 1.000000000000000000, 0.9659258262890683122, 1.000000000000000000, 0.9659258262890683122, 1.000000000000000000, 0.9659258262890683122, 1.000000000000000000, 0.9659258262890683122, 1.000000000000000000, 0.9659258262890683122, 1.000000000000000000, 0.9659258262890683122, 1.000000000000000000, 0.9659258262890683122, 1.000000000000000000, 0.9659258262890683122, 1.000000000000000000, 0.9659258262890683122, 1.000000000000000000, 0.9659258262890683122, 1.000000000000000000, 0.9659258262890683122, 1.000000000000000000, 0.9659258262890683122, 1.000000000000000000, 0.9659258262890683122, 1.000000000000000000, 0.9659258262890683122, 1.000000000000000000, 0.9659258262890683122, 1.000000000000000000, 0.9659258262890683122, 1.000000000000000000, 0.9659258262890683122, 1.000000000000000000, 0.9659258262890683122, 1.000000000000000000, 0.9659258262890683122, 1.000000000000000000, 0.9659258262890683122, 1.000000000000000000, 0.9659258262890683122, 1.000000000000000000, 0.9659258262890683122, 1.000000000000000000) ) ) 
 REPRESENTATION_ITEM ( '' )  SURFACE ( )  );
#97768 = CARTESIAN_POINT ( 'NONE',  ( 7.082119434687054849, 13.47041550158064460, 12.26659068614894288 ) ) ;
#97769 = CARTESIAN_POINT ( 'NONE',  ( 3.591859063236763294, -1.709698663402913210, -11.09922568453595026 ) ) ;
#97770 = CARTESIAN_POINT ( 'NONE',  ( 10.00000000000000000, 65.55374883491396076, -14.16423886937410082 ) ) ;
#97771 = DIRECTION ( 'NONE',  ( 0.000000000000000000, 0.000000000000000000, 1.000000000000000000 ) ) ;
#97772 = EDGE_CURVE ( 'NONE', #16059, #33129, #86530, .T. ) ;
#97773 = CARTESIAN_POINT ( 'NONE',  ( 20.36894250292379738, 4.928748834913967869, -10.36894250292379027 ) ) ;
#97774 = CARTESIAN_POINT ( 'NONE',  ( -0.3689425029237881626, 47.42874883491396787, 10.36894250292379027 ) ) ;
#97775 = STYLED_ITEM ( 'NONE', ( #52419 ), #64438 ) ;
#97776 = CARTESIAN_POINT ( 'NONE',  ( 0.000000000000000000, 15.00000000000000000, 0.000000000000000000 ) ) ;
#97777 = ORIENTED_EDGE ( 'NONE', *, *, #87049, .F. ) ;
#97778 = CARTESIAN_POINT ( 'NONE',  ( 19.84674366389459621, 23.50893115100078390, 7.409399052514197653E-17 ) ) ;
#97779 = CARTESIAN_POINT ( 'NONE',  ( -0.8801773607111008646, 8.272018677488171434, 2.915334737309923430 ) ) ;
#97780 = CARTESIAN_POINT ( 'NONE',  ( 1.472469842513823179, 51.42559781766745886, 4.923371831947296329 ) ) ;
#97782 = CARTESIAN_POINT ( 'NONE',  ( -10.28286150160603363, 89.18763609516977908, -5.839555419999089558 ) ) ;
#97781 = CARTESIAN_POINT ( 'NONE',  ( 0.2751277870542911952, 34.36607318730131055, -6.499999999999992006 ) ) ;
#97783 = B_SPLINE_CURVE_WITH_KNOTS ( 'NONE', 3,
 ( #48519, #2571, #47545, #49016, #93532, #48024 ),
 .UNSPECIFIED., .F., .F.,
 ( 4, 2, 4 ),
 ( 0.000000000000000000, 0.0002701661927229356613, 0.0005403323854458713226 ),
 .UNSPECIFIED. ) ;
#97784 = CIRCLE ( 'NONE', #37095, 0.5000000000000004441 ) ;
#97785 = VECTOR ( 'NONE', #94637, 1000.000000000000000 ) ;
#97786 = CARTESIAN_POINT ( 'NONE',  ( 0.1532563361054083140, 1.008931151000784787, 1.131784320476157264E-15 ) ) ;
#97787 = CARTESIAN_POINT ( 'NONE',  ( 10.00000000000000000, 22.87363466993042138, -12.81628187352647608 ) ) ;
#97788 = CARTESIAN_POINT ( 'NONE',  ( 18.52753015748618282, 43.92559781766745175, -4.923371831947291888 ) ) ;
#97789 = ORIENTED_EDGE ( 'NONE', *, *, #38762, .T. ) ;
#97790 = CARTESIAN_POINT ( 'NONE',  ( 17.20831665107776587, 9.133931151000787452, -7.208316651077762316 ) ) ;
#97791 = STYLED_ITEM ( 'NONE', ( #58052 ), #91278 ) ;
#97792 = CARTESIAN_POINT ( 'NONE',  ( 9.511402282428090160, -15.49422404099892248, -4.000000000000000000 ) ) ;
#97793 = CARTESIAN_POINT ( 'NONE',  ( 0.2751277870542909176, 59.36607318730130345, -6.499999999999992006 ) ) ;
#97794 = CARTESIAN_POINT ( 'NONE',  ( 17.96484262340118221, 11.18868534415483929, -7.964842623401177768 ) ) ;
#97795 = CARTESIAN_POINT ( 'NONE',  ( 2.917880565312948704, 37.63708216824731068, 12.26659068614894643 ) ) ;
#97796 = CARTESIAN_POINT ( 'NONE',  ( -0.8801773607110991993, 42.85535201082150536, -2.915334737309923874 ) ) ;
#97797 = CARTESIAN_POINT ( 'NONE',  ( 4.559911319644449179, 62.23035201082150536, -9.422509992056141925 ) ) ;
#97798 = CARTESIAN_POINT ( 'NONE',  ( -12.25993886608613792, 0.3639311184075819106, 8.642563219313560197 ) ) ;
#97799 = CARTESIAN_POINT ( 'NONE',  ( 0.1532563361054082862, 26.21726448433411605, 2.638427012816831674 ) ) ;
#97800 = CARTESIAN_POINT ( 'NONE',  ( 4.559911319644449179, 12.23035201082150536, -9.422509992056141925 ) ) ;
#97801 = CARTESIAN_POINT ( 'NONE',  ( 5.076628168052703671, 11.84226448433411960, 8.527530157486179263 ) ) ;
#97802 = AXIS2_PLACEMENT_3D ( 'NONE', #67000, #22997, #60964 ) ;
#97803 = CARTESIAN_POINT ( 'NONE',  ( -46.67755760958102229, 101.1477792333171664, 8.700766897918562393 ) ) ;
#97804 = CARTESIAN_POINT ( 'NONE',  ( 19.84674366389459266, 38.71726448433412315, -2.638427012816827677 ) ) ;
#97805 = CARTESIAN_POINT ( 'NONE',  ( 0.5774900079438607392, 38.48035201082150536, 5.440088680355550821 ) ) ;
#97806 = VECTOR ( 'NONE', #84460, 1000.000000000000114 ) ;
#97807 = EDGE_CURVE ( 'NONE', #1901, #35164, #42010, .T. ) ;
#97808 = ORIENTED_EDGE ( 'NONE', *, *, #14472, .F. ) ;
#97809 = CARTESIAN_POINT ( 'NONE',  ( 3.591859063236761518, 59.95696800326375353, 11.09922568453594849 ) ) ;
#97810 = CARTESIAN_POINT ( 'NONE',  ( -5.204170427930421283E-15, 6.671802177851543725, -11.25000000000000178 ) ) ;
#97811 = CARTESIAN_POINT ( 'NONE',  ( 7.361572987183169658, 9.967264484334119601, -9.846743663894592657 ) ) ;
#97812 = CARTESIAN_POINT ( 'NONE',  ( 3.591859063236763294, 48.29030133659708923, -11.09922568453595026 ) ) ;
#97814 = CARTESIAN_POINT ( 'NONE',  ( 19.84674366389459266, 38.71726448433412315, -2.638427012816827677 ) ) ;
#97813 = CARTESIAN_POINT ( 'NONE',  ( 20.88017736071110164, 10.35535201082150714, 2.915334737309930979 ) ) ;
#97815 = LINE ( 'NONE', #60270, #43904 ) ;
#97816 = EDGE_CURVE ( 'NONE', #42622, #48181, #11014, .T. ) ;
#97817 = CARTESIAN_POINT ( 'NONE',  ( 2.917880565312950480, 40.97041550158063217, -12.26659068614894821 ) ) ;
#97818 = CARTESIAN_POINT ( 'NONE',  ( 18.52753015748617571, 43.09226448433412315, 4.923371831947298993 ) ) ;
#97819 = CARTESIAN_POINT ( 'NONE',  ( 19.42250999205614548, 40.98035201082150536, -5.440088680355545492 ) ) ;
#97820 = CARTESIAN_POINT ( 'NONE',  ( 10.00000000000000178, 2.258931151000784787, 9.846743663894594434 ) ) ;
#97821 = CARTESIAN_POINT ( 'NONE',  ( -3.772435416983038525, -6.430908609849964819, 4.000000000001613820 ) ) ;
#97822 = VERTEX_POINT ( 'NONE', #78527 ) ;
#97823 = CARTESIAN_POINT ( 'NONE',  ( 21.09922568453595559, 57.04030133659708923, -6.408140936763230044 ) ) ;
#97824 = CARTESIAN_POINT ( 'NONE',  ( -0.8801773607111009756, 68.06368534415484817, 1.068504757029289695E-15 ) ) ;
#97825 = ORIENTED_EDGE ( 'NONE', *, *, #21255, .F. ) ;
#97826 = CARTESIAN_POINT ( 'NONE',  ( -2.266590686148945544, 11.38708216824730179, -7.082119434687050408 ) ) ;
#97827 = CARTESIAN_POINT ( 'NONE',  ( 1.472469842513823179, 11.42559781766745175, 4.923371831947296329 ) ) ;
#97828 = CARTESIAN_POINT ( 'NONE',  ( 14.49999999999999822, 11.00000000000000000, -6.000000000000000000 ) ) ;
#97829 = ORIENTED_EDGE ( 'NONE', *, *, #5483, .T. ) ;
#97830 = CARTESIAN_POINT ( 'NONE',  ( 12.91533473730993009, 31.60535201082150891, -10.88017736071109987 ) ) ;
#97831 = CIRCLE ( 'NONE', #14820, 0.5000000000000004441 ) ;
#97832 = VERTEX_POINT ( 'NONE', #33983 ) ;
#97833 = CARTESIAN_POINT ( 'NONE',  ( 15.44008868035555793, 41.39701867748817676, -9.422509992056140149 ) ) ;
#97834 = ORIENTED_EDGE ( 'NONE', *, *, #70485, .F. ) ;
#97835 = EDGE_CURVE ( 'NONE', #76829, #70343, #42229, .T. ) ;
#97836 = EDGE_LOOP ( 'NONE', ( #48108, #14072, #34671, #36770 ) ) ;
#97837 = CARTESIAN_POINT ( 'NONE',  ( 10.00000000000000000, 66.81368534415484817, -10.88017736071110342 ) ) ;
#97838 = CARTESIAN_POINT ( 'NONE',  ( 17.20831665107776587, 64.13393115100079456, -7.208316651077762316 ) ) ;
#97840 = LINE ( 'NONE', #37330, #17565 ) ;
#97839 = CARTESIAN_POINT ( 'NONE',  ( 19.42250999205614548, 20.98035201082150891, -5.440088680355545492 ) ) ;
#97841 = CARTESIAN_POINT ( 'NONE',  ( 4.559911319644449179, 68.89701867748817676, 9.422509992056141925 ) ) ;
#97842 = CARTESIAN_POINT ( 'NONE',  ( -0.8801773607111009756, 18.06368534415484106, 1.068504757029289695E-15 ) ) ;
#97843 = ORIENTED_EDGE ( 'NONE', *, *, #81811, .T. ) ;
#97844 = CARTESIAN_POINT ( 'NONE',  ( 22.81628187352648496, 51.83196800326376064, -3.434112377981050290 ) ) ;
#97845 = CARTESIAN_POINT ( 'NONE',  ( 19.42250999205614193, 50.14701867748817676, 5.440088680355555262 ) ) ;
#97846 = DIRECTION ( 'NONE',  ( 0.6246950475544238435, 0.7808688094430307203, 0.000000000000000000 ) ) ;
#97847 = CARTESIAN_POINT ( 'NONE',  ( 19.38216949554541202, 55.99863466993041072, 9.382169495545424454 ) ) ;
#97848 = CARTESIAN_POINT ( 'NONE',  ( 19.42250999205614548, 50.98035201082151247, -5.440088680355545492 ) ) ;
#97849 = COLOUR_RGB ( '', 0.31764706, 0.68627451, 0.89019608) ;
#97850 = CARTESIAN_POINT ( 'NONE',  ( 10.00000000000000178, 67.25893115100079456, 9.846743663894594434 ) ) ;
#97851 =( LENGTH_UNIT ( ) NAMED_UNIT ( * ) SI_UNIT ( .MILLI., .METRE. ) );
#97852 = CARTESIAN_POINT ( 'NONE',  ( 1.472469842513823179, 11.42559781766745175, 4.923371831947296329 ) ) ;
#97853 = AXIS2_PLACEMENT_3D ( 'NONE', #14884, #9326, #98889 ) ;
#97854 = CARTESIAN_POINT ( 'NONE',  ( 3.591859063236761518, 9.956968003263753531, 11.09922568453594849 ) ) ;
#97856 = CARTESIAN_POINT ( 'NONE',  ( 7.361572987183170547, 67.05059781766746596, 9.846743663894590881 ) ) ;
#97855 = CARTESIAN_POINT ( 'NONE',  ( -8.375939845167836850, -0.03417435944610275333, 11.52849216984293257 ) ) ;
#97857 = CARTESIAN_POINT ( 'NONE',  ( 12.91533473730993009, 41.60535201082149825, -10.88017736071109987 ) ) ;
#97858 = CARTESIAN_POINT ( 'NONE',  ( 0.1532563361054100626, 45.80059781766745886, -2.638427012816831230 ) ) ;
#97859 = DIRECTION ( 'NONE',  ( 0.000000000000000000, 0.000000000000000000, -1.000000000000000000 ) ) ;
#97860 = CARTESIAN_POINT ( 'NONE',  ( 2.791683348922240793, 26.63393115100078745, 7.208316651077764092 ) ) ;
#97861 = CARTESIAN_POINT ( 'NONE',  ( 7.361572987183169658, 14.96726448433411960, -9.846743663894592657 ) ) ;
#97863 = ORIENTED_EDGE ( 'NONE', *, *, #42129, .F. ) ;
#97862 = CARTESIAN_POINT ( 'NONE',  ( -2.816281873526473856, 9.331968003263753531, 3.434112377981055619 ) ) ;
#97864 = CIRCLE ( 'NONE', #54717, 15.00000000000000000 ) ;
#97865 = B_SPLINE_CURVE_WITH_KNOTS ( 'NONE', 3,
 ( #7713, #13217, #38208, #43712 ),
 .UNSPECIFIED., .F., .F.,
 ( 4, 4 ),
 ( 5.989547311264452633E-17, 0.001060528352562006968 ),
 .UNSPECIFIED. ) ;
#97866 = SURFACE_SIDE_STYLE ('',( #74837 ) ) ;
#97867 = DIRECTION ( 'NONE',  ( -0.000000000000000000, -1.000000000000000000, -0.000000000000000000 ) ) ;
#97868 = CARTESIAN_POINT ( 'NONE',  ( -1.915564264621532287, 4.395349792408769378E-16, 14.37291249357989287 ) ) ;
#97869 = CARTESIAN_POINT ( 'NONE',  ( 6.565887622018943937, 53.08196800326374643, -12.81628187352647608 ) ) ;
#97870 = CARTESIAN_POINT ( 'NONE',  ( 7.361572987183170547, 37.05059781766744464, 9.846743663894590881 ) ) ;
#97871 = CARTESIAN_POINT ( 'NONE',  ( 6.910443788319881264, -84.29081344359276784, -2.499999999992758681 ) ) ;
#97872 = CARTESIAN_POINT ( 'NONE',  ( -0.8801773607110991993, 12.85535201082150358, -2.915334737309923874 ) ) ;
#97873 = CARTESIAN_POINT ( 'NONE',  ( 19.84674366389459266, 33.30059781766744464, 2.638427012816836559 ) ) ;
#97874 = ORIENTED_EDGE ( 'NONE', *, *, #7044, .F. ) ;
#97875 = DIRECTION ( 'NONE',  ( 0.000000000000000000, -1.000000000000000000, -0.000000000000000000 ) ) ;
#97876 = CARTESIAN_POINT ( 'NONE',  ( 4.559911319644449179, 8.897018677488173211, 9.422509992056141925 ) ) ;
#97877 = CARTESIAN_POINT ( 'NONE',  ( -0.8801773607111009756, 13.06368534415483929, 1.068504757029289695E-15 ) ) ;
#97878 = CARTESIAN_POINT ( 'NONE',  ( 20.88017736071110164, 25.35535201082150891, 2.915334737309930979 ) ) ;
#97879 = CARTESIAN_POINT ( 'NONE',  ( 24.16423886937410614, 49.30374883491396787, 8.672049930838204340E-16 ) ) ;
#97881 = CARTESIAN_POINT ( 'NONE',  ( 2.603489959281614308, 41.58210964143329846, 6.500000000000031086 ) ) ;
#97880 = CARTESIAN_POINT ( 'NONE',  ( 6.204703633549690345, 52.84541550158062506, 14.16423886937410082 ) ) ;
#97882 = CARTESIAN_POINT ( 'NONE',  ( 19.72487221294570858, 70.00000000000000000, -6.000000000000000000 ) ) ;
#97883 = CARTESIAN_POINT ( 'NONE',  ( 7.361572987183169658, 19.96726448433411960, -9.846743663894592657 ) ) ;
#97884 = CARTESIAN_POINT ( 'NONE',  ( 21.09922568453595559, 2.040301336597086568, -6.408140936763230044 ) ) ;
#97885 = ORIENTED_EDGE ( 'NONE', *, *, #66413, .F. ) ;
#97886 = CARTESIAN_POINT ( 'NONE',  ( -14.35840480524194440, 0.5000000000000004441, -4.340070442839038201 ) ) ;
#97887 = CARTESIAN_POINT ( 'NONE',  ( -18.89999999999999503, 92.00000000000000000, -7.750000000000000000 ) ) ;
#97888 = EDGE_CURVE ( 'NONE', #97596, #26759, #41033, .T. ) ;
#97889 = CARTESIAN_POINT ( 'NONE',  ( -46.31228368244003946, 103.3337736655113588, 5.775421524742653467 ) ) ;
#97890 = CARTESIAN_POINT ( 'NONE',  ( 0.1532563361054082862, 66.21726448433413736, 2.638427012816831674 ) ) ;
#97891 = CARTESIAN_POINT ( 'NONE',  ( 24.16423886937410614, 14.30374883491396787, 8.672049930838204340E-16 ) ) ;
#97892 = VECTOR ( 'NONE', #47767, 1000.000000000000000 ) ;
#97893 = CARTESIAN_POINT ( 'NONE',  ( 7.361572987183169658, 29.96726448433411960, -9.846743663894592657 ) ) ;
#97894 = CARTESIAN_POINT ( 'NONE',  ( 0.000000000000000000, 14.49999999999999822, 0.000000000000000000 ) ) ;
#97895 = EDGE_LOOP ( 'NONE', ( #12972, #36521, #90049, #70684 ) ) ;
#97896 = EDGE_CURVE ( 'NONE', #46043, #57430, #68220, .T. ) ;
#97897 = CARTESIAN_POINT ( 'NONE',  ( -4.164238869374099039, 36.80374883491396787, 8.674139862899312516E-16 ) ) ;
#97898 = CARTESIAN_POINT ( 'NONE',  ( 5.076628168052704559, 10.17559781766745175, -8.527530157486179263 ) ) ;
#97900 = CARTESIAN_POINT ( 'NONE',  ( 0.2751277870542967463, 70.00000000000000000, -6.500000000000000888 ) ) ;
#97899 = CARTESIAN_POINT ( 'NONE',  ( -7.121341127193570486, -73.24353698637885657, -2.750000000000000000 ) ) ;
#97901 = CARTESIAN_POINT ( 'NONE',  ( 17.96484262340118221, 34.93868534415482685, 7.964842623401181321 ) ) ;
#97902 = CARTESIAN_POINT ( 'NONE',  ( 16.40814093676324603, 37.45696800326376064, -11.09922568453594671 ) ) ;
#97903 = CARTESIAN_POINT ( 'NONE',  ( 10.00000000000000178, 4.313685344154837509, 10.88017736071110342 ) ) ;
#97904 = CARTESIAN_POINT ( 'NONE',  ( 0.6178305044545838731, 29.74863466993042138, 9.382169495545420901 ) ) ;
#97905 = CARTESIAN_POINT ( 'NONE',  ( 16.40814093676324603, 62.45696800326376064, -11.09922568453594671 ) ) ;
#97906 = EDGE_LOOP ( 'NONE', ( #51189, #68640, #2172, #67931, #41059, #62047, #51030, #17067, #17276, #10950, #63112, #69461, #84369, #93865, #24256, #36689, #53891, #56620, #89008, #59301, #66805, #60855, #65663, #46392, #63854, #19714, #1894, #38073, #83085, #2467 ) ) ;
#97907 = CARTESIAN_POINT ( 'NONE',  ( 19.89103541497709315, 35.66234555792572536, -6.479102184480822757 ) ) ;
#97908 = CARTESIAN_POINT ( 'NONE',  ( -2.266590686148945544, 41.38708216824729647, -7.082119434687050408 ) ) ;
#97909 = CARTESIAN_POINT ( 'NONE',  ( 6.204703633549690345, 2.845415501580634388, 14.16423886937410082 ) ) ;
#97910 = CARTESIAN_POINT ( 'NONE',  ( 4.559911319644449179, 3.897018677488170990, 9.422509992056141925 ) ) ;
#97911 = CARTESIAN_POINT ( 'NONE',  ( 7.084665262690076126, 24.10535201082150181, 10.88017736071109987 ) ) ;
#97912 = CARTESIAN_POINT ( 'NONE',  ( 0.000000000000000000, 15.00000000000000000, 0.000000000000000000 ) ) ;
#97913 = CARTESIAN_POINT ( 'NONE',  ( 10.58981376305282041, -0.03417435944610275333, 9.535111140613782510 ) ) ;
#97914 = CARTESIAN_POINT ( 'NONE',  ( 7.084665262690076126, 57.02201867748817676, -10.88017736071110164 ) ) ;
#97915 = LINE ( 'NONE', #16363, #33747 ) ;
#97916 = CARTESIAN_POINT ( 'NONE',  ( 6.565887622018943937, 33.08196800326374643, -12.81628187352647608 ) ) ;
#97917 = DIRECTION ( 'NONE',  ( 1.000000000000000000, 0.000000000000000000, 0.000000000000000000 ) ) ;
#97918 = CARTESIAN_POINT ( 'NONE',  ( 19.84674366389459621, 28.50893115100078745, 7.409399052514197653E-17 ) ) ;
#97919 = CARTESIAN_POINT ( 'NONE',  ( 7.084665262690076126, 59.10535201082150536, 10.88017736071109987 ) ) ;
#97920 = EDGE_CURVE ( 'NONE', #63150, #46169, #90095, .T. ) ;
#97921 = CARTESIAN_POINT ( 'NONE',  ( 0.6178305044545838731, 19.74863466993042138, 9.382169495545420901 ) ) ;
#97922 = CARTESIAN_POINT ( 'NONE',  ( 0.8952175423694743728, 42.60160829253886305, -5.990408912944304554 ) ) ;
#97923 = CARTESIAN_POINT ( 'NONE',  ( 7.084665262690076126, 7.022018677488169658, -10.88017736071110164 ) ) ;
#97924 = CARTESIAN_POINT ( 'NONE',  ( 17.20831665107776587, 39.13393115100079456, -7.208316651077762316 ) ) ;
#97925 = CARTESIAN_POINT ( 'NONE',  ( 10.00000000000000000, 57.87363466993042493, -12.81628187352647608 ) ) ;
#97926 = TOROIDAL_SURFACE ( 'NONE', #72396, 14.49999999999999822, 0.5000000000000000000 ) ;
#97927 = CARTESIAN_POINT ( 'NONE',  ( 2.791683348922240793, 16.63393115100078745, 7.208316651077764092 ) ) ;
#97928 = EDGE_CURVE ( 'NONE', #57215, #56371, #46997, .T. ) ;
#97929 = VECTOR ( 'NONE', #57383, 1000.000000000000000 ) ;
#97930 =( NAMED_UNIT ( * ) PLANE_ANGLE_UNIT ( ) SI_UNIT ( $, .RADIAN. ) );
#97931 = DIRECTION ( 'NONE',  ( -1.000000000000000000, 2.081668171172166620E-14, 0.000000000000000000 ) ) ;
#97932 = CARTESIAN_POINT ( 'NONE',  ( 4.559911319644449179, 28.89701867748817321, 9.422509992056141925 ) ) ;
#97933 = CARTESIAN_POINT ( 'NONE',  ( -0.8801773607111009756, 3.063685344154837509, 1.068504757029289695E-15 ) ) ;
#97934 = CARTESIAN_POINT ( 'NONE',  ( 14.92337183194729988, 39.34226448433412315, -8.527530157486177487 ) ) ;
#97935 = VECTOR ( 'NONE', #30590, 1000.000000000000000 ) ;
#97936 = CARTESIAN_POINT ( 'NONE',  ( 2.035157376598824452, 38.68868534415483396, 7.964842623401179544 ) ) ;
#97937 = CARTESIAN_POINT ( 'NONE',  ( 15.44008868035555793, 21.39701867748817321, -9.422509992056140149 ) ) ;
#97938 = ORIENTED_EDGE ( 'NONE', *, *, #65588, .T. ) ;
#97939 = CARTESIAN_POINT ( 'NONE',  ( 0.5774900079438590739, 27.64701867748817676, -5.440088680355550821 ) ) ;
#97940 = CARTESIAN_POINT ( 'NONE',  ( 10.00000000000000178, 40.37363466993042493, 12.81628187352647608 ) ) ;
#97941 = CARTESIAN_POINT ( 'NONE',  ( 17.96484262340118221, 36.18868534415484106, -7.964842623401177768 ) ) ;
#97942 = CARTESIAN_POINT ( 'NONE',  ( -0.8801773607110991993, 42.85535201082150536, -2.915334737309923874 ) ) ;
#97943 = EDGE_LOOP ( 'NONE', ( #52073, #71135, #55675, #57517 ) ) ;
#97944 = CARTESIAN_POINT ( 'NONE',  ( 1.472469842513823179, 56.42559781766745886, 4.923371831947296329 ) ) ;
#97945 = CARTESIAN_POINT ( 'NONE',  ( 4.559911319644449179, 37.23035201082150536, -9.422509992056141925 ) ) ;
#97946 = CARTESIAN_POINT ( 'NONE',  ( 10.58981376305288613, -0.03417435944610275333, -9.535111140613709679 ) ) ;
#97947 = CARTESIAN_POINT ( 'NONE',  ( 4.999999999999999112, 11.00000000000000000, 6.000000000000000000 ) ) ;
#97948 = CARTESIAN_POINT ( 'NONE',  ( 13.79529636645030344, 43.26208216824730357, 14.16423886937410614 ) ) ;
#97949 = CARTESIAN_POINT ( 'NONE',  ( 20.88017736071110164, 50.35535201082151247, 2.915334737309930979 ) ) ;
#97950 = CARTESIAN_POINT ( 'NONE',  ( 0.000000000000000000, 15.00000000000000000, 0.000000000000000000 ) ) ;
#97951 = DIRECTION ( 'NONE',  ( -1.000000000000000000, 0.000000000000000000, 0.000000000000000000 ) ) ;
#97952 = CARTESIAN_POINT ( 'NONE',  ( 1.472469842513823179, 66.42559781766745175, 4.923371831947296329 ) ) ;
#97953 = CARTESIAN_POINT ( 'NONE',  ( 7.084665262690076126, 2.022018677488170990, -10.88017736071110164 ) ) ;
#97954 = CARTESIAN_POINT ( 'NONE',  ( 2.791683348922240793, 26.63393115100078745, 7.208316651077764092 ) ) ;
#97955 = ORIENTED_EDGE ( 'NONE', *, *, #70277, .T. ) ;
#97956 = CARTESIAN_POINT ( 'NONE',  ( 5.076628168052704559, 20.17559781766745175, -8.527530157486179263 ) ) ;
#97957 = CARTESIAN_POINT ( 'NONE',  ( 6.408140936763236262, -22.54303199673624292, -11.09922568453595026 ) ) ;
#97958 = ADVANCED_FACE ( 'NONE', ( #71534 ), #77315, .T. ) ;
#97959 = CARTESIAN_POINT ( 'NONE',  ( 20.88017736071110875, 25.77201867748816966, -2.915334737309920765 ) ) ;
#97960 = CARTESIAN_POINT ( 'NONE',  ( 14.92337183194729988, 24.34226448433411960, -8.527530157486177487 ) ) ;
#97962 = CARTESIAN_POINT ( 'NONE',  ( 0.5774900079438607392, 63.48035201082149825, 5.440088680355550821 ) ) ;
#97961 = CARTESIAN_POINT ( 'NONE',  ( 0.000000000000000000, 15.00000000000000000, 0.000000000000000000 ) ) ;
#97964 = CARTESIAN_POINT ( 'NONE',  ( 10.00000000000000000, 1.813685344154837731, -10.88017736071110342 ) ) ;
#97963 = CARTESIAN_POINT ( 'NONE',  ( 20.88017736071110164, 30.35535201082151247, 2.915334737309930979 ) ) ;
#97965 = CARTESIAN_POINT ( 'NONE',  ( 24.16423886937410614, 44.51208216824730357, -3.795296366450302550 ) ) ;
#97966 = EDGE_CURVE ( 'NONE', #6107, #40043, #48559, .T. ) ;
#97967 = AXIS2_PLACEMENT_3D ( 'NONE', #65966, #96493, #27966 ) ;
#97968 = DIRECTION ( 'NONE',  ( 0.000000000000000000, 0.000000000000000000, 1.000000000000000000 ) ) ;
#97969 = VERTEX_POINT ( 'NONE', #63515 ) ;
#97970 = CARTESIAN_POINT ( 'NONE',  ( 13.43411237798105340, 10.58196800326375353, 12.81628187352647963 ) ) ;
#97971 = CARTESIAN_POINT ( 'NONE',  ( 4.559911319644449179, 8.897018677488171434, 9.422509992056141925 ) ) ;
#97972 = CARTESIAN_POINT ( 'NONE',  ( 10.00000000000000000, 51.81368534415484106, -10.88017736071110342 ) ) ;
#97973 = FACE_OUTER_BOUND ( 'NONE', #13736, .T. ) ;
#97974 = EDGE_LOOP ( 'NONE', ( #76064, #7279, #82330, #47642 ) ) ;
#97975 = CARTESIAN_POINT ( 'NONE',  ( 19.42250999205614548, 55.98035201082150536, -5.440088680355545492 ) ) ;
#97976 = CARTESIAN_POINT ( 'NONE',  ( 0.1532563361054100626, 40.80059781766745886, -2.638427012816831230 ) ) ;
#97977 = CARTESIAN_POINT ( 'NONE',  ( 19.84674366389459266, 23.30059781766745530, 2.638427012816836559 ) ) ;
#97978 = CARTESIAN_POINT ( 'NONE',  ( 12.63842701281683034, 12.46726448433411782, 9.846743663894596210 ) ) ;
#97980 = CARTESIAN_POINT ( 'NONE',  ( -2.816281873526473856, 34.12363466993042493, 9.499525473075851096E-16 ) ) ;
#97979 = DIRECTION ( 'NONE',  ( 1.000000000000000000, 0.000000000000000000, 0.000000000000000000 ) ) ;
#97982 = PLANE ( 'NONE',  #19560 ) ;
#97981 = CARTESIAN_POINT ( 'NONE',  ( 1.472469842513823179, 5.592264484334118713, -4.923371831947296329 ) ) ;
#97983 = LINE ( 'NONE', #67959, #72916 ) ;
#97985 = ORIENTED_EDGE ( 'NONE', *, *, #43014, .F. ) ;
#97984 = CARTESIAN_POINT ( 'NONE',  ( 12.63842701281683034, 27.46726448433411250, 9.846743663894596210 ) ) ;
#97986 = CARTESIAN_POINT ( 'NONE',  ( 21.09922568453594849, 56.20696800326375353, 6.408140936763242479 ) ) ;
#97987 = CARTESIAN_POINT ( 'NONE',  ( 0.3093388210927780491, 0.3639309406664013036, 14.99680997725069531 ) ) ;
#97988 = CARTESIAN_POINT ( 'NONE',  ( 10.00000000000000000, -2.126365330069579951, -12.81628187352647608 ) ) ;
#97989 = AXIS2_PLACEMENT_3D ( 'NONE', #17347, #2354, #8842 ) ;
#97990 = CARTESIAN_POINT ( 'NONE',  ( 6.204703633549690345, 27.84541550158063217, 14.16423886937410082 ) ) ;
#97991 = AXIS2_PLACEMENT_3D ( 'NONE', #15212, #68209, #62148 ) ;
#97992 = DIRECTION ( 'NONE',  ( 0.000000000000000000, 0.000000000000000000, -1.000000000000000000 ) ) ;
#97993 = COLOUR_RGB ( '', 0.31764706, 0.68627451, 0.89019608) ;
#97994 = CARTESIAN_POINT ( 'NONE',  ( -4.164238869374098151, 36.59541550158063217, -3.795296366450310543 ) ) ;
#97995 = CARTESIAN_POINT ( 'NONE',  ( 20.36894250292379738, 39.92874883491396787, -10.36894250292379027 ) ) ;
#97996 = CARTESIAN_POINT ( 'NONE',  ( 13.79529636645031943, 5.345415501580634832, -14.16423886937409904 ) ) ;
#97998 = CARTESIAN_POINT ( 'NONE',  ( -0.8801773607110991993, 67.85535201082151957, -2.915334737309923874 ) ) ;
#97997 = CARTESIAN_POINT ( 'NONE',  ( 6.204703633549690345, 10.76208216824729824, -14.16423886937410259 ) ) ;
#97999 = CARTESIAN_POINT ( 'NONE',  ( 12.91533473730992121, 44.52201867748816966, 10.88017736071110164 ) ) ;
#98000 = DIRECTION ( 'NONE',  ( -0.000000000000000000, -1.000000000000000000, -0.000000000000000000 ) ) ;
#98002 = COLOUR_RGB ( '', 0.08235294, 0.09019608, 0.10196078) ;
#98001 = CARTESIAN_POINT ( 'NONE',  ( 5.076628168052704559, 30.17559781766745175, -8.527530157486179263 ) ) ;
#98004 = CARTESIAN_POINT ( 'NONE',  ( 19.84674366389459266, 33.30059781766744464, 2.638427012816836559 ) ) ;
#98003 = CARTESIAN_POINT ( 'NONE',  ( 4.559911319644449179, 67.23035201082150536, -9.422509992056141925 ) ) ;
#98005 = CARTESIAN_POINT ( 'NONE',  ( 2.035157376598824452, 23.68868534415484461, 7.964842623401179544 ) ) ;
#98006 = CARTESIAN_POINT ( 'NONE',  ( 6.565887622018943937, 53.08196800326374643, -12.81628187352647608 ) ) ;
#98007 = CARTESIAN_POINT ( 'NONE',  ( 17.20831665107776587, 62.88393115100078745, 7.208316651077764980 ) ) ;
#98008 = ADVANCED_FACE ( 'NONE', ( #18517 ), #11500, .F. ) ;
#98009 = CARTESIAN_POINT ( 'NONE',  ( 14.92337183194729633, 22.67559781766745175, 8.527530157486181039 ) ) ;
#98010 = CARTESIAN_POINT ( 'NONE',  ( 21.09922568453595559, 47.04030133659708923, -6.408140936763230044 ) ) ;
#98011 = CARTESIAN_POINT ( 'NONE',  ( -7.082119434687044190, -22.36291783175269288, 12.26659068614894998 ) ) ;
#98012 = CARTESIAN_POINT ( 'NONE',  ( 19.42250999205614548, 40.98035201082150536, -5.440088680355545492 ) ) ;
#98013 = CARTESIAN_POINT ( 'NONE',  ( 17.20831665107776587, 52.88393115100078035, 7.208316651077764980 ) ) ;
#98014 = CARTESIAN_POINT ( 'NONE',  ( -4.164238869374099927, 32.01208216824730357, 3.795296366450308767 ) ) ;
#98015 = ORIENTED_EDGE ( 'NONE', *, *, #76326, .F. ) ;
#98016 = SURFACE_SIDE_STYLE ('',( #22006 ) ) ;
#98017 = CARTESIAN_POINT ( 'NONE',  ( -0.8801773607110991993, 67.85535201082151957, -2.915334737309923874 ) ) ;
#98018 = DIRECTION ( 'NONE',  ( 1.000000000000000000, 1.776356839400250465E-15, 0.000000000000000000 ) ) ;
#98019 = CARTESIAN_POINT ( 'NONE',  ( 24.16423886937409904, 64.09541550158064638, 3.795296366450317205 ) ) ;
#98020 = CARTESIAN_POINT ( 'NONE',  ( -2.816281873526473856, -0.6680319967362464695, 3.434112377981055619 ) ) ;
#98021 = CARTESIAN_POINT ( 'NONE',  ( 19.42250999205614193, 50.14701867748817676, 5.440088680355555262 ) ) ;
#98022 = CARTESIAN_POINT ( 'NONE',  ( -0.1503990784575263973, 27.22266099184919241, -6.262539305110081500 ) ) ;
#98023 = CARTESIAN_POINT ( 'NONE',  ( 21.09922568453595559, 32.04030133659708923, -6.408140936763230044 ) ) ;
#98024 = CARTESIAN_POINT ( 'NONE',  ( -10.88017736071110164, 22.85535201082150891, -2.915334737309917212 ) ) ;
#98025 = CARTESIAN_POINT ( 'NONE',  ( 2.035157376598822676, 7.438685344154837509, -7.964842623401177768 ) ) ;
#98026 = CARTESIAN_POINT ( 'NONE',  ( 10.00000000000000000, 11.81368534415483751, -10.88017736071110342 ) ) ;
#98027 = CARTESIAN_POINT ( 'NONE',  ( 1.472469842513823179, 56.42559781766745886, 4.923371831947296329 ) ) ;
#98028 = CARTESIAN_POINT ( 'NONE',  ( 13.43411237798106583, 47.66530133659709634, -12.81628187352647252 ) ) ;
#98029 = CARTESIAN_POINT ( 'NONE',  ( -15.33206046421386759, -0.03417435944610275333, -4.561284726668966449 ) ) ;
#98030 = ORIENTED_EDGE ( 'NONE', *, *, #22055, .T. ) ;
#98031 = CARTESIAN_POINT ( 'NONE',  ( 12.91533473730993009, 21.60535201082150536, -10.88017736071109987 ) ) ;
#98032 = CARTESIAN_POINT ( 'NONE',  ( 19.38216949554541202, 15.99863466993042138, 9.382169495545424454 ) ) ;
#98033 = CARTESIAN_POINT ( 'NONE',  ( 64.56412365047461321, 44.99999999999998579, -7.000000000000000000 ) ) ;
#98034 = CARTESIAN_POINT ( 'NONE',  ( 12.63842701281683034, 17.46726448433411250, 9.846743663894596210 ) ) ;
#98035 = EDGE_CURVE ( 'NONE', #59012, #47538, #35958, .T. ) ;
#98036 = CARTESIAN_POINT ( 'NONE',  ( 1.472469842513823179, 45.59226448433412315, -4.923371831947296329 ) ) ;
#98037 = CARTESIAN_POINT ( 'NONE',  ( 20.88017736071110164, 35.35535201082150536, 2.915334737309930979 ) ) ;
#98038 = CARTESIAN_POINT ( 'NONE',  ( 13.43411237798105340, 10.58196800326375353, 12.81628187352647963 ) ) ;
#98040 = CARTESIAN_POINT ( 'NONE',  ( 8.630000000000000782, 1.019547802438459216, 3.750000000000000000 ) ) ;
#98039 = CARTESIAN_POINT ( 'NONE',  ( 12.91533473730992121, 49.52201867748817676, 10.88017736071110164 ) ) ;
#98041 = DIRECTION ( 'NONE',  ( -1.000000000000000000, 6.608470384673545847E-17, 0.000000000000000000 ) ) ;
#98042 = CARTESIAN_POINT ( 'NONE',  ( 3.591859063236763294, 58.29030133659708923, -11.09922568453595026 ) ) ;
#98043 = ORIENTED_EDGE ( 'NONE', *, *, #31392, .F. ) ;
#98044 = CARTESIAN_POINT ( 'NONE',  ( 12.91533473730993009, 61.60535201082150536, -10.88017736071109987 ) ) ;
#98045 = EDGE_CURVE ( 'NONE', #57827, #96234, #57490, .T. ) ;
#98046 = CARTESIAN_POINT ( 'NONE',  ( -2.816281873526473856, 39.12363466993041783, 9.499525473075851096E-16 ) ) ;
#98047 = CARTESIAN_POINT ( 'NONE',  ( -0.8801773607111009756, 38.06368534415484106, 1.068504757029289695E-15 ) ) ;
#98048 = CARTESIAN_POINT ( 'NONE',  ( 14.92337183194729988, 19.34226448433411960, -8.527530157486177487 ) ) ;
#98049 = CARTESIAN_POINT ( 'NONE',  ( -6.000000000000000000, 78.07179676972447169, -4.000000000000000000 ) ) ;
#98050 = CARTESIAN_POINT ( 'NONE',  ( 10.00000000000000178, 12.25893115100078568, 9.846743663894594434 ) ) ;
#98051 = CARTESIAN_POINT ( 'NONE',  ( 7.361572987183170547, 12.05059781766744997, 9.846743663894590881 ) ) ;
#98052 = DIRECTION ( 'NONE',  ( 0.000000000000000000, 0.000000000000000000, -1.000000000000000000 ) ) ;
#98053 = CARTESIAN_POINT ( 'NONE',  ( -0.3689425029237898834, 46.17874883491397497, -10.36894250292378850 ) ) ;
#98054 = LINE ( 'NONE', #14046, #36196 ) ;
#98055 = CARTESIAN_POINT ( 'NONE',  ( 10.72255383998327005, -40.29605683832149765, -3.750000000000002220 ) ) ;
#98056 = CARTESIAN_POINT ( 'NONE',  ( -6.060988839905886216, -36.09899559454662210, -4.000000000000000000 ) ) ;
#98057 = EDGE_LOOP ( 'NONE', ( #86038, #51608, #86357, #28790, #30740, #41036 ) ) ;
#98058 = CARTESIAN_POINT ( 'NONE',  ( 10.00000000000000178, 58.05374883491397497, 14.16423886937410082 ) ) ;
#98059 = CARTESIAN_POINT ( 'NONE',  ( 17.08211943468705840, 65.13708216824730357, -12.26659068614894466 ) ) ;
#98060 = CARTESIAN_POINT ( 'NONE',  ( 12.63842701281683922, 29.55059781766745175, -9.846743663894590881 ) ) ;
#98061 = CARTESIAN_POINT ( 'NONE',  ( -2.816281873526473856, 44.33196800326375353, 3.434112377981055619 ) ) ;
#98063 = CARTESIAN_POINT ( 'NONE',  ( 24.16423886937410614, 9.303748834913967869, 8.672049930838204340E-16 ) ) ;
#98062 = CARTESIAN_POINT ( 'NONE',  ( 2.603489959281199972, 21.58210964143324873, 6.499999999999559464 ) ) ;
#98064 = CARTESIAN_POINT ( 'NONE',  ( 20.88017736071110164, 15.35535201082150358, 2.915334737309930979 ) ) ;
#98065 = CARTESIAN_POINT ( 'NONE',  ( -0.3689425029237898834, 56.17874883491396076, -10.36894250292378850 ) ) ;
#98066 = CARTESIAN_POINT ( 'NONE',  ( 0.1532563361054083140, 31.00893115100078390, 1.131784320476157264E-15 ) ) ;
#98067 = CARTESIAN_POINT ( 'NONE',  ( 18.72515096720571393, 41.07228050351032778, -6.499999999999974243 ) ) ;
#98068 = CARTESIAN_POINT ( 'NONE',  ( 18.52753015748618282, 28.92559781766745175, -4.923371831947291888 ) ) ;
#98069 = CIRCLE ( 'NONE', #27802, 0.2500000000000002220 ) ;
#98070 = LINE ( 'NONE', #65557, #24298 ) ;
#98071 = CARTESIAN_POINT ( 'NONE',  ( 9.846743663894590881, 18.71726448433412315, -2.638427012816833894 ) ) ;
#98072 = ORIENTED_EDGE ( 'NONE', *, *, #86597, .T. ) ;
#98073 = VERTEX_POINT ( 'NONE', #42497 ) ;
#98074 = PRESENTATION_STYLE_ASSIGNMENT (( #14071 ) ) ;
#98075 = B_SPLINE_CURVE_WITH_KNOTS ( 'NONE', 3,
 ( #32517, #24556, #56507, #17044 ),
 .UNSPECIFIED., .F., .F.,
 ( 4, 4 ),
 ( 0.000000000000000000, 0.0006041882680322483833 ),
 .UNSPECIFIED. ) ;
#98076 = ORIENTED_EDGE ( 'NONE', *, *, #17240, .T. ) ;
#98077 = CARTESIAN_POINT ( 'NONE',  ( 10.00000000000000178, 42.25893115100078745, 9.846743663894594434 ) ) ;
#98078 = CARTESIAN_POINT ( 'NONE',  ( 6.204703633549690345, 15.76208216824730179, -14.16423886937410259 ) ) ;
#98080 = CARTESIAN_POINT ( 'NONE',  ( 19.42250999205614193, 40.14701867748817676, 5.440088680355555262 ) ) ;
#98079 = CARTESIAN_POINT ( 'NONE',  ( -0.8801773607110991993, 27.85535201082150181, -2.915334737309923874 ) ) ;
#98082 = CARTESIAN_POINT ( 'NONE',  ( 16.40814093676323893, 15.79030133659708746, 11.09922568453595026 ) ) ;
#98081 = CARTESIAN_POINT ( 'NONE',  ( 0.1532563361054082862, 61.21726448433412315, 2.638427012816831674 ) ) ;
#98083 = EDGE_CURVE ( 'NONE', #48512, #67942, #2065, .T. ) ;
#98084 = CARTESIAN_POINT ( 'NONE',  ( -0.8801773607110991993, 67.85535201082151957, -2.915334737309923874 ) ) ;
#98085 = CARTESIAN_POINT ( 'NONE',  ( 0.6178305044545818747, 33.49863466993042493, -9.382169495545419124 ) ) ;
#98086 = ORIENTED_EDGE ( 'NONE', *, *, #65153, .T. ) ;
#98087 = CARTESIAN_POINT ( 'NONE',  ( 1.472469842513823179, 46.42559781766745175, 4.923371831947296329 ) ) ;
#98088 = CARTESIAN_POINT ( 'NONE',  ( 4.559911319644449179, 7.230352010821505360, -9.422509992056141925 ) ) ;
#98089 = ORIENTED_EDGE ( 'NONE', *, *, #44760, .T. ) ;
#98090 = CARTESIAN_POINT ( 'NONE',  ( 17.96484262340118221, 14.93868534415484106, 7.964842623401181321 ) ) ;
#98091 = ORIENTED_EDGE ( 'NONE', *, *, #90103, .T. ) ;
#98092 = CARTESIAN_POINT ( 'NONE',  ( 19.42250999205614193, 45.14701867748817676, 5.440088680355555262 ) ) ;
#98093 = CARTESIAN_POINT ( 'NONE',  ( 2.035157376598822676, 57.43868534415484106, -7.964842623401177768 ) ) ;
#98094 = CARTESIAN_POINT ( 'NONE',  ( 10.00000000000000000, 61.81368534415484106, -10.88017736071110342 ) ) ;
#98095 = CARTESIAN_POINT ( 'NONE',  ( 0.000000000000000000, 0.5000000000000004441, 0.000000000000000000 ) ) ;
#98096 = CARTESIAN_POINT ( 'NONE',  ( 0.5774900079438607392, 53.48035201082151247, 5.440088680355550821 ) ) ;
#98098 = ORIENTED_EDGE ( 'NONE', *, *, #15028, .T. ) ;
#98097 = CYLINDRICAL_SURFACE ( 'NONE', #4250, 0.5000000000000004441 ) ;
#98099 = CARTESIAN_POINT ( 'NONE',  ( 14.92337183194729633, 22.67559781766745175, 8.527530157486181039 ) ) ;
#98100 = VERTEX_POINT ( 'NONE', #40540 ) ;
#98101 = CARTESIAN_POINT ( 'NONE',  ( 1.472469842513823179, 66.42559781766745175, 4.923371831947296329 ) ) ;
#98102 = FILL_AREA_STYLE_COLOUR ( '', #57300 ) ;
#98103 = CARTESIAN_POINT ( 'NONE',  ( 22.26659068614895176, 4.720415501580633943, -7.082119434687042414 ) ) ;
#98104 = DIRECTION ( 'NONE',  ( -0.000000000000000000, -1.000000000000000000, -0.000000000000000000 ) ) ;
#98106 = CARTESIAN_POINT ( 'NONE',  ( 2.791683348922240793, 36.63393115100078035, 7.208316651077764092 ) ) ;
#98105 = CARTESIAN_POINT ( 'NONE',  ( -7.750000000000000000, 41.24999999999999289, -6.500000000000000888 ) ) ;
#98107 = CARTESIAN_POINT ( 'NONE',  ( 4.559911319644449179, 13.89701867748817321, 9.422509992056141925 ) ) ;
#98108 = CARTESIAN_POINT ( 'NONE',  ( 9.159723438033129383, 15.00000000000000000, 10.91613331444548507 ) ) ;
#98109 = VERTEX_POINT ( 'NONE', #74456 ) ;
#98110 = CARTESIAN_POINT ( 'NONE',  ( -3.195792623639464924, 5.729976035794186018, 11.92686044187660421 ) ) ;
#98111 = CARTESIAN_POINT ( 'NONE',  ( 5.076628168052704559, 40.17559781766745175, -8.527530157486179263 ) ) ;
#98112 = DIRECTION ( 'NONE',  ( -4.707345624410664362E-14, 0.000000000000000000, 1.000000000000000000 ) ) ;
#98113 = CARTESIAN_POINT ( 'NONE',  ( -2.816281873526473856, 14.33196800326375531, 3.434112377981055619 ) ) ;
#98114 = CARTESIAN_POINT ( 'NONE',  ( 19.84674366389459266, 13.30059781766745353, 2.638427012816836559 ) ) ;
#98115 = CARTESIAN_POINT ( 'NONE',  ( -0.08248232600719085372, 0.1423898869303599768, 6.349449577244200782 ) ) ;
#98116 = EDGE_CURVE ( 'NONE', #90692, #73812, #13475, .T. ) ;
#98117 = CARTESIAN_POINT ( 'NONE',  ( -2.816281873526473856, -0.8763653300695799508, 9.499525473075851096E-16 ) ) ;
#98118 = CARTESIAN_POINT ( 'NONE',  ( 0.000000000000000000, 35.00000000000000000, 0.000000000000000000 ) ) ;
#98119 = VECTOR ( 'NONE', #49991, 1000.000000000000114 ) ;
#98120 = EDGE_LOOP ( 'NONE', ( #45173, #83286, #89562, #85226, #47101, #93213 ) ) ;
#98121 = EDGE_CURVE ( 'NONE', #82667, #47240, #29444, .T. ) ;
#98122 = ORIENTED_EDGE ( 'NONE', *, *, #3524, .T. ) ;
#98123 = CARTESIAN_POINT ( 'NONE',  ( 15.44008868035555793, 21.39701867748817321, -9.422509992056140149 ) ) ;
#98124 = CARTESIAN_POINT ( 'NONE',  ( -2.266590686148945544, 22.22041550158063572, 7.082119434687048631 ) ) ;
#98125 = CARTESIAN_POINT ( 'NONE',  ( 0.1532563361054082862, 31.21726448433412315, 2.638427012816831674 ) ) ;
#98126 = CARTESIAN_POINT ( 'NONE',  ( 19.42250999205614548, 60.98035201082151247, -5.440088680355545492 ) ) ;
#98128 = CARTESIAN_POINT ( 'NONE',  ( -3.711005778769052021, -5.293034685380286319, -3.750000000000000000 ) ) ;
#98127 = CARTESIAN_POINT ( 'NONE',  ( 22.81628187352648496, 41.83196800326375353, -3.434112377981050290 ) ) ;
#98129 = CARTESIAN_POINT ( 'NONE',  ( 2.035157376598824452, 13.68868534415483751, 7.964842623401179544 ) ) ;
#98130 = AXIS2_PLACEMENT_3D ( 'NONE', #29106, #21631, #52117 ) ;
#98131 = CARTESIAN_POINT ( 'NONE',  ( -14.35840480524194440, 0.5000000000000004441, -4.340070442839038201 ) ) ;
#98132 = FACE_OUTER_BOUND ( 'NONE', #4198, .T. ) ;
#98133 = CARTESIAN_POINT ( 'NONE',  ( -2.816281873526473856, 14.12363466993041961, 9.499525473075851096E-16 ) ) ;
#98134 = CARTESIAN_POINT ( 'NONE',  ( 21.09922568453594849, 11.20696800326375531, 6.408140936763242479 ) ) ;
#98135 = CARTESIAN_POINT ( 'NONE',  ( 0.1532563361054082862, 21.21726448433412315, 2.638427012816831674 ) ) ;
#98136 = CARTESIAN_POINT ( 'NONE',  ( -5.204170427930421283E-15, -18.18631465584515894, -10.88017736071110342 ) ) ;
#98137 = CARTESIAN_POINT ( 'NONE',  ( 21.09922568453594849, 41.20696800326375353, 6.408140936763242479 ) ) ;
#98138 =( NAMED_UNIT ( * ) PLANE_ANGLE_UNIT ( ) SI_UNIT ( $, .RADIAN. ) );
#98139 = EDGE_CURVE ( 'NONE', #74236, #11914, #58972, .T. ) ;
#98141 = CARTESIAN_POINT ( 'NONE',  ( 5.500000000000000000, 61.00000000000000711, -6.500000000000000888 ) ) ;
#98140 = CARTESIAN_POINT ( 'NONE',  ( 17.96484262340118221, 41.18868534415484106, -7.964842623401177768 ) ) ;
#98142 = CARTESIAN_POINT ( 'NONE',  ( 11.34661744925197624, 54.08985607419764818, -3.000000000000000000 ) ) ;
#98143 = CARTESIAN_POINT ( 'NONE',  ( 19.89103541497711447, 20.66234555792571115, -6.479102184480773907 ) ) ;
#98144 = CARTESIAN_POINT ( 'NONE',  ( 4.559911319644449179, 47.23035201082150536, -9.422509992056141925 ) ) ;
#98145 = CARTESIAN_POINT ( 'NONE',  ( 17.96484262340118221, 41.18868534415484106, -7.964842623401177768 ) ) ;
#98146 = CARTESIAN_POINT ( 'NONE',  ( 18.52753015748618282, 58.92559781766745886, -4.923371831947291888 ) ) ;
#98147 = B_SPLINE_CURVE_WITH_KNOTS ( 'NONE', 3,
 ( #10673, #86185, #93176, #10190, #11651, #89125 ),
 .UNSPECIFIED., .F., .F.,
 ( 4, 2, 4 ),
 ( 3.409110551478550352E-05, 0.0004400426677366311512, 0.0008459942299584768260 ),
 .UNSPECIFIED. ) ;
#98148 = EDGE_CURVE ( 'NONE', #41784, #62860, #69341, .T. ) ;
#98149 = CARTESIAN_POINT ( 'NONE',  ( -12.35505582470280572, 15.00000000000000000, 10.16021613965622095 ) ) ;
#98150 = UNCERTAINTY_MEASURE_WITH_UNIT (LENGTH_MEASURE( 1.000000000000000082E-05 ), #7931, 'distance_accuracy_value', 'NONE');
#98151 =( BOUNDED_CURVE ( )  B_SPLINE_CURVE ( 2, ( #20188, #27684, #5198, #80193, #34687, #66169, #58169, #27186, #4217 ),
 .UNSPECIFIED., .F., .F. ) 
 B_SPLINE_CURVE_WITH_KNOTS ( ( 3, 2, 2, 2, 3 ),
 ( 0.5453713073319822469, 0.5476190476190476719, 0.5535714285714286031, 0.5595238095238095344, 0.5617715498108749594 ),
 .UNSPECIFIED. ) 
 CURVE ( )  GEOMETRIC_REPRESENTATION_ITEM ( )  RATIONAL_B_SPLINE_CURVE ( ( 0.9839835555609424134, 0.9871328979762477029, 1.000000000000000000, 0.9659258262890683122, 1.000000000000000000, 0.9659258262890683122, 1.000000000000000000, 0.9871328979762474809, 0.9839835555609424134 ) ) 
 REPRESENTATION_ITEM ( '' )  );
#98152 = CARTESIAN_POINT ( 'NONE',  ( 17.20831665107776587, 32.88393115100078745, 7.208316651077764980 ) ) ;
#98153 = CARTESIAN_POINT ( 'NONE',  ( 17.96484262340118221, 4.938685344154837509, 7.964842623401181321 ) ) ;
#98154 = CARTESIAN_POINT ( 'NONE',  ( 22.81628187352648496, 16.83196800326374998, -3.434112377981050290 ) ) ;
#98155 = ORIENTED_EDGE ( 'NONE', *, *, #76214, .F. ) ;
#98156 = CARTESIAN_POINT ( 'NONE',  ( 10.00000000000000178, 19.31368534415484106, 10.88017736071110342 ) ) ;
#98157 = EDGE_CURVE ( 'NONE', #52889, #93734, #6462, .T. ) ;
#98158 = FACE_OUTER_BOUND ( 'NONE', #62386, .T. ) ;
#98159 = CARTESIAN_POINT ( 'NONE',  ( 10.00000000000000178, 4.313685344154837509, 10.88017736071110342 ) ) ;
#98160 = CARTESIAN_POINT ( 'NONE',  ( 7.084665262690076126, 22.02201867748817321, -10.88017736071110164 ) ) ;
#98161 = CARTESIAN_POINT ( 'NONE',  ( 7.361572987183169658, -0.03273551566588185635, -9.846743663894592657 ) ) ;
#98162 = CARTESIAN_POINT ( 'NONE',  ( 24.16423886937409904, 44.09541550158063927, 3.795296366450317205 ) ) ;
#98163 = CARTESIAN_POINT ( 'NONE',  ( 19.84674366389459266, 13.71726448433411782, -2.638427012816827677 ) ) ;
#98164 = CARTESIAN_POINT ( 'NONE',  ( 10.00000000000000178, 44.31368534415484106, 10.88017736071110342 ) ) ;
#98165 = CARTESIAN_POINT ( 'NONE',  ( 3.059999999999993392, 76.92054879330447648, 9.500000000000000000 ) ) ;
#98166 = CARTESIAN_POINT ( 'NONE',  ( 20.36894250292379738, 4.928748834913967869, -10.36894250292379027 ) ) ;
#98167 = ORIENTED_EDGE ( 'NONE', *, *, #20667, .T. ) ;
#98168 = DIRECTION ( 'NONE',  ( 0.000000000000000000, 0.000000000000000000, -1.000000000000000000 ) ) ;
#98169 = CARTESIAN_POINT ( 'NONE',  ( 10.00000000000000178, 57.25893115100078745, 9.846743663894594434 ) ) ;
#98170 = ORIENTED_EDGE ( 'NONE', *, *, #87102, .F. ) ;
#98171 = ORIENTED_EDGE ( 'NONE', *, *, #17895, .F. ) ;
#98172 = CARTESIAN_POINT ( 'NONE',  ( 4.431036607602561794, 15.00000000000000000, -14.33059365769911153 ) ) ;
#98173 = CARTESIAN_POINT ( 'NONE',  ( 22.26659068614894466, 18.88708216824730002, 7.082119434687054849 ) ) ;
#98174 = CARTESIAN_POINT ( 'NONE',  ( 10.00000000000000000, 25.55374883491396787, -14.16423886937410082 ) ) ;
#98175 = CARTESIAN_POINT ( 'NONE',  ( 4.559911319644449179, 63.89701867748817676, 9.422509992056141925 ) ) ;
#98176 = CARTESIAN_POINT ( 'NONE',  ( 24.16423886937410614, 64.30374883491396076, 8.672049930838204340E-16 ) ) ;
#98177 = CARTESIAN_POINT ( 'NONE',  ( -2.816281873526471635, -1.084698663402913210, -3.434112377981056508 ) ) ;
#98178 = CARTESIAN_POINT ( 'NONE',  ( 1.472469842513823179, 45.59226448433412315, -4.923371831947296329 ) ) ;
#98179 = CARTESIAN_POINT ( 'NONE',  ( -7.778993154286912848, -1.060766117536017017, 4.000000000000000000 ) ) ;
#98181 = CARTESIAN_POINT ( 'NONE',  ( -1.099225684535947600, 23.70696800326375708, -6.408140936763238038 ) ) ;
#98180 = CARTESIAN_POINT ( 'NONE',  ( 20.88017736071110519, 45.56368534415484106, 2.639326808657452039E-16 ) ) ;
#98182 = CARTESIAN_POINT ( 'NONE',  ( -0.3689425029237898834, 11.17874883491396787, -10.36894250292378850 ) ) ;
#98183 = CARTESIAN_POINT ( 'NONE',  ( 17.96484262340118221, 14.93868534415484106, 7.964842623401181321 ) ) ;
#98184 = CARTESIAN_POINT ( 'NONE',  ( 2.035157376598822676, 17.43868534415483751, -7.964842623401177768 ) ) ;
#98185 = SURFACE_SIDE_STYLE ('',( #13178 ) ) ;
#98186 = CARTESIAN_POINT ( 'NONE',  ( 15.44008868035555793, 56.39701867748817676, -9.422509992056140149 ) ) ;
#98187 = CARTESIAN_POINT ( 'NONE',  ( -9.846743663894590881, -28.78273551566588040, 2.638427012816840111 ) ) ;
#98188 = ORIENTED_EDGE ( 'NONE', *, *, #28594, .F. ) ;
#98189 = CARTESIAN_POINT ( 'NONE',  ( -45.94000000000001194, 103.9981609152045650, -5.961202730336927047 ) ) ;
#98190 = COLOUR_RGB ( '', 0.09019608, 0.27058824, 0.51372549) ;
#98191 = ORIENTED_EDGE ( 'NONE', *, *, #27880, .T. ) ;
#98192 = DIRECTION ( 'NONE',  ( 0.000000000000000000, -1.000000000000000000, 0.000000000000000000 ) ) ;
#98193 = VERTEX_POINT ( 'NONE', #65474 ) ;
#98194 = SURFACE_SIDE_STYLE ('',( #50313 ) ) ;
#98196 = CARTESIAN_POINT ( 'NONE',  ( 13.79529636645031943, 65.34541550158063217, -14.16423886937409904 ) ) ;
#98195 = CARTESIAN_POINT ( 'NONE',  ( 17.08211943468705840, 50.13708216824730357, -12.26659068614894466 ) ) ;
#98198 = CARTESIAN_POINT ( 'NONE',  ( 12.63842701281683922, 44.55059781766745175, -9.846743663894590881 ) ) ;
#98197 = CARTESIAN_POINT ( 'NONE',  ( 19.84674366389459266, 23.30059781766745530, 2.638427012816836559 ) ) ;
#98199 = CARTESIAN_POINT ( 'NONE',  ( 20.15039907845753220, 60.60158574516643881, -6.262539305110077947 ) ) ;
#98200 = DIRECTION ( 'NONE',  ( 0.000000000000000000, 0.000000000000000000, 1.000000000000000000 ) ) ;
#98201 = EDGE_CURVE ( 'NONE', #12692, #91503, #13302, .T. ) ;
#98202 = CARTESIAN_POINT ( 'NONE',  ( 10.00000000000000000, 66.81368534415484817, -10.88017736071110342 ) ) ;
#98203 = B_SPLINE_CURVE_WITH_KNOTS ( 'NONE', 3,
 ( #12163, #19671, #72172, #96672, #27158, #73147 ),
 .UNSPECIFIED., .F., .F.,
 ( 4, 2, 4 ),
 ( 0.000000000000000000, 0.0002626113303184800848, 0.0005252226606369601696 ),
 .UNSPECIFIED. ) ;
#98204 = CARTESIAN_POINT ( 'NONE',  ( -9.382169495545413795, 19.74863466993042138, 9.382169495545428006 ) ) ;
#98205 = VERTEX_POINT ( 'NONE', #34975 ) ;
#98206 = CARTESIAN_POINT ( 'NONE',  ( 24.16423886937410614, 29.30374883491396787, 8.672049930838204340E-16 ) ) ;
#98207 = CARTESIAN_POINT ( 'NONE',  ( 13.43411237798106583, 22.66530133659708923, -12.81628187352647252 ) ) ;
#98208 = ORIENTED_EDGE ( 'NONE', *, *, #67989, .T. ) ;
#98209 = CARTESIAN_POINT ( 'NONE',  ( -1.099225684535947600, 64.54030133659709634, 6.408140936763237150 ) ) ;
#98210 = CARTESIAN_POINT ( 'NONE',  ( 17.96484262340118221, 31.18868534415483751, -7.964842623401177768 ) ) ;
#98211 = CARTESIAN_POINT ( 'NONE',  ( 2.791683348922240793, 41.63393115100078745, 7.208316651077764092 ) ) ;
#98212 = CARTESIAN_POINT ( 'NONE',  ( 0.5774900079438590739, 27.64701867748817676, -5.440088680355550821 ) ) ;
#98213 = CARTESIAN_POINT ( 'NONE',  ( 13.43411237798106583, 62.66530133659708923, -12.81628187352647252 ) ) ;
#98214 = CARTESIAN_POINT ( 'NONE',  ( 7.361572987183169658, 44.96726448433412315, -9.846743663894592657 ) ) ;
#98215 = CARTESIAN_POINT ( 'NONE',  ( 5.076628168052703671, 56.84226448433412315, 8.527530157486179263 ) ) ;
#98217 = ORIENTED_EDGE ( 'NONE', *, *, #3195, .T. ) ;
#98216 = DIRECTION ( 'NONE',  ( 0.000000000000000000, 0.000000000000000000, -1.000000000000000000 ) ) ;
#98218 = TOROIDAL_SURFACE ( 'NONE', #56651, 14.49999999999999822, 0.5000000000000000000 ) ;
#98219 = DIRECTION ( 'NONE',  ( -0.000000000000000000, -0.000000000000000000, 1.000000000000000000 ) ) ;
#98220 = LINE ( 'NONE', #51715, #30645 ) ;
#98221 = DIRECTION ( 'NONE',  ( 0.000000000000000000, -1.000000000000000000, 0.000000000000000000 ) ) ;
#98222 = DIRECTION ( 'NONE',  ( 0.000000000000000000, 0.000000000000000000, 1.000000000000000000 ) ) ;
#98223 = CARTESIAN_POINT ( 'NONE',  ( 17.20831665107776587, 34.13393115100078745, -7.208316651077762316 ) ) ;
#98224 = FACE_OUTER_BOUND ( 'NONE', #53074, .T. ) ;
#98225 = CARTESIAN_POINT ( 'NONE',  ( 6.565887622018943937, 38.08196800326376064, -12.81628187352647608 ) ) ;
#98226 = CARTESIAN_POINT ( 'NONE',  ( 8.629999999999995453, 41.24999999999999289, -4.250000000000000000 ) ) ;
#98227 = ORIENTED_EDGE ( 'NONE', *, *, #53620, .T. ) ;
#98228 = CARTESIAN_POINT ( 'NONE',  ( 5.076628168052703671, 56.84226448433412315, 8.527530157486179263 ) ) ;
#98229 = CARTESIAN_POINT ( 'NONE',  ( -11.62719953690055164, 14.49999999999999112, -9.476720473302012948 ) ) ;
#98230 = CARTESIAN_POINT ( 'NONE',  ( 18.52753015748617571, 38.09226448433412315, 4.923371831947298993 ) ) ;
#98231 = CARTESIAN_POINT ( 'NONE',  ( 6.204703633549690345, 27.84541550158063217, 14.16423886937410082 ) ) ;
#98232 = CARTESIAN_POINT ( 'NONE',  ( 5.076628168052704559, 50.17559781766745886, -8.527530157486179263 ) ) ;
#98233 = CARTESIAN_POINT ( 'NONE',  ( 10.00000000000000000, 42.87363466993042493, -12.81628187352647608 ) ) ;
#98235 =( NAMED_UNIT ( * ) SI_UNIT ( $, .STERADIAN. ) SOLID_ANGLE_UNIT ( ) );
#98234 = DIRECTION ( 'NONE',  ( 0.000000000000000000, -1.000000000000000000, 0.000000000000000000 ) ) ;
#98236 = CARTESIAN_POINT ( 'NONE',  ( 5.076628168052704559, 5.175597817667451750, -8.527530157486179263 ) ) ;
#98237 = ADVANCED_FACE ( 'NONE', ( #19984 ), #97489, .F. ) ;
#98238 = CARTESIAN_POINT ( 'NONE',  ( 20.24186590665276597, 46.76028685723174760, 6.114288769123062295 ) ) ;
#98239 = VECTOR ( 'NONE', #72094, 1000.000000000000000 ) ;
#98240 = CARTESIAN_POINT ( 'NONE',  ( 18.52753015748618282, 43.92559781766745175, -4.923371831947291888 ) ) ;
#98241 = CARTESIAN_POINT ( 'NONE',  ( 20.88017736071110519, 35.56368534415484106, 2.639326808657452039E-16 ) ) ;
#98242 = CARTESIAN_POINT ( 'NONE',  ( 0.1532563361054082862, 41.21726448433411605, 2.638427012816831674 ) ) ;
#98243 = CONTEXT_DEPENDENT_SHAPE_REPRESENTATION ( #29600, #17149 ) ;
#98244 = DIRECTION ( 'NONE',  ( 0.000000000000000000, 1.000000000000000000, 0.000000000000000000 ) ) ;
#98245 = EDGE_CURVE ( 'NONE', #5309, #14873, #34710, .T. ) ;
#98246 = EDGE_LOOP ( 'NONE', ( #18169, #63024, #93732, #74671 ) ) ;
#98247 = CARTESIAN_POINT ( 'NONE',  ( 19.42250999205614548, 50.98035201082151247, -5.440088680355545492 ) ) ;
#98248 = EDGE_CURVE ( 'NONE', #10214, #48471, #43955, .T. ) ;
#98249 = EDGE_CURVE ( 'NONE', #51046, #40424, #4995, .T. ) ;
#98250 = ORIENTED_EDGE ( 'NONE', *, *, #36018, .T. ) ;
#98251 = CARTESIAN_POINT ( 'NONE',  ( 0.2751277870542909731, 22.28217586085237656, -6.499999999999992006 ) ) ;
#98252 = CARTESIAN_POINT ( 'NONE',  ( 4.559911319644449179, 17.23035201082150536, -9.422509992056141925 ) ) ;
#98254 = CARTESIAN_POINT ( 'NONE',  ( 15.44008868035555260, 39.73035201082150536, 9.422509992056143702 ) ) ;
#98253 = CARTESIAN_POINT ( 'NONE',  ( 19.84674366389459266, 63.71726448433412315, -2.638427012816827677 ) ) ;
#98256 = B_SPLINE_CURVE_WITH_KNOTS ( 'NONE', 3,
 ( #5300, #58772, #89761, #89275 ),
 .UNSPECIFIED., .F., .F.,
 ( 4, 4 ),
 ( 0.000000000000000000, 0.002562518741975551920 ),
 .UNSPECIFIED. ) ;
#98255 = CARTESIAN_POINT ( 'NONE',  ( 2.603489959281115151, 16.58210964143323807, 6.499999999999462652 ) ) ;
#98257 = DIRECTION ( 'NONE',  ( 1.000000000000000000, -5.782411586589362323E-17, 0.000000000000000000 ) ) ;
#98258 = CARTESIAN_POINT ( 'NONE',  ( 13.59972906620397026, 14.95037118612373384, 5.718800721548674915 ) ) ;
#98260 = CARTESIAN_POINT ( 'NONE',  ( 67.06412365047464164, 14.00000000000000888, -9.500000000000000000 ) ) ;
#98259 = CARTESIAN_POINT ( 'NONE',  ( 12.91533473730992121, 34.52201867748817676, 10.88017736071110164 ) ) ;
#98261 = CARTESIAN_POINT ( 'NONE',  ( 2.791683348922240793, 11.63393115100078568, 7.208316651077764092 ) ) ;
#98262 = AXIS2_PLACEMENT_3D ( 'NONE', #94999, #35484, #64981 ) ;
#98263 = CARTESIAN_POINT ( 'NONE',  ( 0.1532563361054083140, 26.00893115100078745, 1.131784320476157264E-15 ) ) ;
#98264 = CARTESIAN_POINT ( 'NONE',  ( -8.000000000000000000, 1.019547802438458550, 3.750000000000000000 ) ) ;
#98265 = CARTESIAN_POINT ( 'NONE',  ( 3.795296366450306547, 25.34541550158063927, -14.16423886937410259 ) ) ;
#98266 = CARTESIAN_POINT ( 'NONE',  ( 17.20831665107776587, 64.13393115100079456, -7.208316651077762316 ) ) ;
#98267 = CARTESIAN_POINT ( 'NONE',  ( 2.035157376598822676, 2.438685344154838397, -7.964842623401177768 ) ) ;
#98268 = EDGE_CURVE ( 'NONE', #62480, #51116, #57385, .T. ) ;
#98269 = CARTESIAN_POINT ( 'NONE',  ( -9.997910040112678587, 4.195612547371048347E-16, 10.50199004140710812 ) ) ;
#98270 = CARTESIAN_POINT ( 'NONE',  ( 13.79529636645030344, 18.26208216824730002, 14.16423886937410614 ) ) ;
#98271 = CARTESIAN_POINT ( 'NONE',  ( 22.26659068614895176, 54.72041550158063217, -7.082119434687042414 ) ) ;
#98272 = ORIENTED_EDGE ( 'NONE', *, *, #15084, .T. ) ;
#98273 = CARTESIAN_POINT ( 'NONE',  ( 14.92337183194729988, 19.34226448433411960, -8.527530157486177487 ) ) ;
#98274 = CARTESIAN_POINT ( 'NONE',  ( 4.559911319644449179, 8.897018677488173211, 9.422509992056141925 ) ) ;
#98275 = CARTESIAN_POINT ( 'NONE',  ( 12.63842701281683034, 52.46726448433413026, 9.846743663894596210 ) ) ;
#98277 = PRESENTATION_STYLE_ASSIGNMENT (( #21772 ) ) ;
#98276 = CARTESIAN_POINT ( 'NONE',  ( -0.3689425029237881626, 2.428748834913967869, 10.36894250292379027 ) ) ;
#98278 = CARTESIAN_POINT ( 'NONE',  ( -8.099999999999999645, 75.73428692542562146, -2.900000000000000355 ) ) ;
#98279 = AXIS2_PLACEMENT_3D ( 'NONE', #83821, #75821, #31786 ) ;
#98280 = CARTESIAN_POINT ( 'NONE',  ( 14.92337183194729633, 2.675597817667451750, 8.527530157486181039 ) ) ;
#98281 = CARTESIAN_POINT ( 'NONE',  ( 22.81628187352647785, 41.41530133659708923, 3.434112377981063169 ) ) ;
#98282 = CARTESIAN_POINT ( 'NONE',  ( 5.076628168052703671, 46.84226448433412315, 8.527530157486179263 ) ) ;
#98283 = ORIENTED_EDGE ( 'NONE', *, *, #41805, .T. ) ;
#98284 = CARTESIAN_POINT ( 'NONE',  ( 0.1532563361054100626, 10.80059781766745175, -2.638427012816831230 ) ) ;
#98285 = ADVANCED_FACE ( 'NONE', ( #90438 ), #21981, .T. ) ;
#98286 = CARTESIAN_POINT ( 'NONE',  ( 10.09973302567988362, -32.02492402194155119, -4.000000000000000000 ) ) ;
#98287 = DIRECTION ( 'NONE',  ( -1.000000000000000000, 0.000000000000000000, 0.000000000000000000 ) ) ;
#98288 = CARTESIAN_POINT ( 'NONE',  ( 4.559911319644449179, 13.89701867748817321, 9.422509992056141925 ) ) ;
#98289 = CARTESIAN_POINT ( 'NONE',  ( 6.204703633549690345, 60.76208216824730357, -14.16423886937410259 ) ) ;
#98290 = CARTESIAN_POINT ( 'NONE',  ( 4.219999999999999751, 10.25000000000000000, -3.750000000000000000 ) ) ;
#98291 = CARTESIAN_POINT ( 'NONE',  ( 0.000000000000000000, 0.5000000000000004441, 0.000000000000000000 ) ) ;
#98292 = CARTESIAN_POINT ( 'NONE',  ( 10.00000000000000178, 27.25893115100078390, 9.846743663894594434 ) ) ;
#98293 = CARTESIAN_POINT ( 'NONE',  ( 12.91533473730993009, 11.60535201082150536, -10.88017736071109987 ) ) ;
#98294 = CARTESIAN_POINT ( 'NONE',  ( 1.472469842513823179, 6.425597817667451750, 4.923371831947296329 ) ) ;
#98295 = CARTESIAN_POINT ( 'NONE',  ( 17.20831665107776587, 49.13393115100078745, -7.208316651077762316 ) ) ;
#98296 = CARTESIAN_POINT ( 'NONE',  ( 19.42250999205614193, 30.14701867748817321, 5.440088680355555262 ) ) ;
#98297 = EDGE_CURVE ( 'NONE', #49746, #28421, #50482, .T. ) ;
#98298 = UNCERTAINTY_MEASURE_WITH_UNIT (LENGTH_MEASURE( 1.000000000000000082E-05 ), #1384, 'distance_accuracy_value', 'NONE');
#98299 = ORIENTED_EDGE ( 'NONE', *, *, #27562, .T. ) ;
#98300 = CARTESIAN_POINT ( 'NONE',  ( 19.38216949554541557, 62.24863466993041072, -9.382169495545420901 ) ) ;
#98301 = CIRCLE ( 'NONE', #61502, 0.2500000000000002220 ) ;
#98302 = CARTESIAN_POINT ( 'NONE',  ( 0.000000000000000000, 0.000000000000000000, -14.25000000000000000 ) ) ;
#98303 = CARTESIAN_POINT ( 'NONE',  ( 0.1532563361054083140, 11.00893115100078568, 1.131784320476157264E-15 ) ) ;
#98304 = CARTESIAN_POINT ( 'NONE',  ( 10.00000000000000178, 45.37363466993041783, 12.81628187352647608 ) ) ;
#98306 = CARTESIAN_POINT ( 'NONE',  ( 17.20831665107776587, 34.13393115100078745, -7.208316651077762316 ) ) ;
#98305 = CARTESIAN_POINT ( 'NONE',  ( 15.44008868035555260, 4.730352010821505360, 9.422509992056143702 ) ) ;
#98307 = CARTESIAN_POINT ( 'NONE',  ( 20.00000000000000711, 98.59912998021083297, 4.500000000000000888 ) ) ;
#98308 = DIRECTION ( 'NONE',  ( 1.000000000000000000, 0.000000000000000000, 0.000000000000000000 ) ) ;
#98309 = CARTESIAN_POINT ( 'NONE',  ( 22.26659068614895176, 29.72041550158063572, -7.082119434687042414 ) ) ;
#98310 = CARTESIAN_POINT ( 'NONE',  ( -4.164238869374099039, 46.80374883491397497, 8.674139862899312516E-16 ) ) ;
#98311 = CARTESIAN_POINT ( 'NONE',  ( 14.92337183194729988, 54.34226448433412315, -8.527530157486177487 ) ) ;
#98312 = CARTESIAN_POINT ( 'NONE',  ( 3.469446951953614189E-15, 9.171802177851546389, 11.25000000000000355 ) ) ;
#98313 = CARTESIAN_POINT ( 'NONE',  ( 2.035157376598824452, 43.68868534415484106, 7.964842623401179544 ) ) ;
#98314 = CARTESIAN_POINT ( 'NONE',  ( 5.076628168052703671, 6.842264484334118713, 8.527530157486179263 ) ) ;
#98315 = ORIENTED_EDGE ( 'NONE', *, *, #98297, .F. ) ;
#98316 = CARTESIAN_POINT ( 'NONE',  ( -1.099225684535947600, 54.54030133659708923, 6.408140936763237150 ) ) ;
#98317 = ORIENTED_EDGE ( 'NONE', *, *, #69290, .T. ) ;
#98318 = CARTESIAN_POINT ( 'NONE',  ( 0.1532563361054082862, 1.217264484334117824, 2.638427012816831674 ) ) ;
#98319 = VERTEX_POINT ( 'NONE', #76927 ) ;
#98320 = AXIS2_PLACEMENT_3D ( 'NONE', #81727, #34751, #42760 ) ;
#98321 = CARTESIAN_POINT ( 'NONE',  ( 20.36894250292379738, 9.928748834913966093, -10.36894250292379027 ) ) ;
#98322 = CARTESIAN_POINT ( 'NONE',  ( 19.84674366389459621, 8.508931151000785675, 7.409399052514197653E-17 ) ) ;
#98323 = CARTESIAN_POINT ( 'NONE',  ( 7.084665262690076126, 32.02201867748816966, -10.88017736071110164 ) ) ;
#98324 = ORIENTED_EDGE ( 'NONE', *, *, #11977, .F. ) ;
#98325 = CARTESIAN_POINT ( 'NONE',  ( -0.8801773607111008646, 28.27201867748817321, 2.915334737309923430 ) ) ;
#98326 = VERTEX_POINT ( 'NONE', #68947 ) ;
#98327 = CARTESIAN_POINT ( 'NONE',  ( 20.88017736071110519, 35.56368534415484106, 2.639326808657452039E-16 ) ) ;
#98328 = CARTESIAN_POINT ( 'NONE',  ( 0.2751277870542876425, 45.30223176428830811, 6.499999999999984901 ) ) ;
#98329 = ORIENTED_EDGE ( 'NONE', *, *, #1387, .T. ) ;
#98330 = VERTEX_POINT ( 'NONE', #46433 ) ;
#98331 = CARTESIAN_POINT ( 'NONE',  ( -2.816281873526471635, 13.91530133659708746, -3.434112377981056508 ) ) ;
#98332 = EDGE_CURVE ( 'NONE', #19080, #32896, #22967, .T. ) ;
#98333 = CARTESIAN_POINT ( 'NONE',  ( 12.63842701281683034, 2.467264484334118269, 9.846743663894596210 ) ) ;
#98334 = SURFACE_SIDE_STYLE ('',( #31268 ) ) ;
#98336 = DIRECTION ( 'NONE',  ( -1.000000000000000000, -2.107602052970794797E-16, 0.000000000000000000 ) ) ;
#98335 = CARTESIAN_POINT ( 'NONE',  ( 7.084665262690076126, 19.10535201082150181, 10.88017736071109987 ) ) ;
#98337 = CARTESIAN_POINT ( 'NONE',  ( 0.1532563361054100626, 0.8005978176674514168, -2.638427012816831230 ) ) ;
#98338 = CARTESIAN_POINT ( 'NONE',  ( 10.00000000000000000, 21.81368534415484106, -10.88017736071110342 ) ) ;
#98339 = EDGE_CURVE ( 'NONE', #60281, #13116, #6226, .T. ) ;
#98340 = AXIS2_PLACEMENT_3D ( 'NONE', #85927, #70431, #9424 ) ;
#98341 = ORIENTED_EDGE ( 'NONE', *, *, #52504, .F. ) ;
#98342 = CARTESIAN_POINT ( 'NONE',  ( 10.00000000000000178, 55.37363466993042493, 12.81628187352647608 ) ) ;
#98343 = CARTESIAN_POINT ( 'NONE',  ( 2.035157376598822676, 42.43868534415483396, -7.964842623401177768 ) ) ;
#98344 = CARTESIAN_POINT ( 'NONE',  ( -1.175527996597229841, 6.200281173901476510E-16, 14.57931687975697876 ) ) ;
#98345 = STYLED_ITEM ( 'NONE', ( #23507 ), #86447 ) ;
#98346 = CARTESIAN_POINT ( 'NONE',  ( 19.38216949554541557, 57.24863466993042493, -9.382169495545420901 ) ) ;
#98347 = CARTESIAN_POINT ( 'NONE',  ( 12.91533473730993009, 51.60535201082149825, -10.88017736071109987 ) ) ;
#98348 = CARTESIAN_POINT ( 'NONE',  ( 18.52753015748617571, 63.09226448433412315, 4.923371831947298993 ) ) ;
#98349 = CYLINDRICAL_SURFACE ( 'NONE', #73828, 11.92686044187656513 ) ;
#98350 = CARTESIAN_POINT ( 'NONE',  ( 17.20831665107776587, 19.13393115100078035, -7.208316651077762316 ) ) ;
#98351 = CARTESIAN_POINT ( 'NONE',  ( 0.6178305044545838731, 59.74863466993041783, 9.382169495545420901 ) ) ;
#98352 = FACE_OUTER_BOUND ( 'NONE', #77098, .T. ) ;
#98353 = CARTESIAN_POINT ( 'NONE',  ( 1.472469842513823179, 11.42559781766745175, 4.923371831947296329 ) ) ;
#98354 = CARTESIAN_POINT ( 'NONE',  ( 21.09922568453595559, 2.040301336597086568, -6.408140936763230044 ) ) ;
#98356 = CARTESIAN_POINT ( 'NONE',  ( 10.00000000000000178, 62.25893115100078745, 9.846743663894594434 ) ) ;
#98355 = DIRECTION ( 'NONE',  ( -1.000000000000000000, -1.257402221000612102E-16, 0.000000000000000000 ) ) ;
#98357 = CARTESIAN_POINT ( 'NONE',  ( 19.42250999205614548, 35.98035201082151247, -5.440088680355545492 ) ) ;
#98358 = CARTESIAN_POINT ( 'NONE',  ( 7.361572987183169658, 44.96726448433412315, -9.846743663894592657 ) ) ;
#98359 = CARTESIAN_POINT ( 'NONE',  ( -0.2418659066527486246, 33.09014588040358262, 6.114288769123083611 ) ) ;
#98360 = CARTESIAN_POINT ( 'NONE',  ( 17.20831665107776587, 22.88393115100078745, 7.208316651077764980 ) ) ;
#98361 = CARTESIAN_POINT ( 'NONE',  ( 19.84674366389459621, 3.508931151000785231, 7.409399052514197653E-17 ) ) ;
#98363 = EDGE_LOOP ( 'NONE', ( #45294, #17733, #68201, #16549 ) ) ;
#98362 = CARTESIAN_POINT ( 'NONE',  ( 16.40814093676324603, 7.456968003263754419, -11.09922568453594671 ) ) ;
#98364 = CARTESIAN_POINT ( 'NONE',  ( 1.472469842513823179, 66.42559781766745175, 4.923371831947296329 ) ) ;
#98365 = EDGE_CURVE ( 'NONE', #95619, #31275, #35789, .T. ) ;
#98366 = TOROIDAL_SURFACE ( 'NONE', #44007, 3.500000000000000888, 0.5000000000000000000 ) ;
#98367 = CARTESIAN_POINT ( 'NONE',  ( 4.572805491839753600, -6.390838093316509649, -2.500000000000000000 ) ) ;
#98368 = CARTESIAN_POINT ( 'NONE',  ( -0.8801773607111009756, 3.063685344154838397, 1.068504757029289695E-15 ) ) ;
#98369 = CARTESIAN_POINT ( 'NONE',  ( 0.1532563361054083140, 41.00893115100078745, 1.131784320476157264E-15 ) ) ;
#98370 = EDGE_CURVE ( 'NONE', #39149, #69767, #15470, .T. ) ;
#98371 = VERTEX_POINT ( 'NONE', #61425 ) ;
#98372 = DIRECTION ( 'NONE',  ( 0.000000000000000000, 1.000000000000000000, 0.000000000000000000 ) ) ;
#98373 = CARTESIAN_POINT ( 'NONE',  ( -0.8801773607110991993, 2.855352010821504471, -2.915334737309923874 ) ) ;
#98374 = CARTESIAN_POINT ( 'NONE',  ( 20.15039907845753930, 69.92552686551195507, -6.262539305110068177 ) ) ;
#98375 = CARTESIAN_POINT ( 'NONE',  ( 4.559911319644449179, 23.89701867748817321, 9.422509992056141925 ) ) ;
#98376 = CARTESIAN_POINT ( 'NONE',  ( 24.16423886937410614, 54.30374883491396787, 8.672049930838204340E-16 ) ) ;
#98378 = DIRECTION ( 'NONE',  ( 0.9975640502598243087, -0.06975647374412544122, -0.000000000000000000 ) ) ;
#98377 = CARTESIAN_POINT ( 'NONE',  ( 7.084665262690076126, 2.022018677488171434, -10.88017736071110164 ) ) ;
#98379 = CARTESIAN_POINT ( 'NONE',  ( 10.00000000000000000, -0.2410688489992152128, -9.846743663894594434 ) ) ;
#98380 = CARTESIAN_POINT ( 'NONE',  ( 0.1532563361054083140, 21.00893115100078745, 1.131784320476157264E-15 ) ) ;
#98381 = CARTESIAN_POINT ( 'NONE',  ( 6.565887622018943937, 15.16530133659708568, 12.81628187352647430 ) ) ;
#98382 = LINE ( 'NONE', #29838, #63321 ) ;
#98383 = AXIS2_PLACEMENT_3D ( 'NONE', #12534, #42540, #73024 ) ;
#98384 = FACE_OUTER_BOUND ( 'NONE', #71480, .T. ) ;
#98385 = CARTESIAN_POINT ( 'NONE',  ( 1.472469842513823179, 55.59226448433412315, -4.923371831947296329 ) ) ;
#98386 = CARTESIAN_POINT ( 'NONE',  ( 0.000000000000000000, 14.49999999999999822, 0.000000000000000000 ) ) ;
#98387 = CARTESIAN_POINT ( 'NONE',  ( 19.72487221294570858, 29.78217586085238366, 6.499999999999992895 ) ) ;
#98388 = CARTESIAN_POINT ( 'NONE',  ( 2.917880565312950480, 15.97041550158063217, -12.26659068614894821 ) ) ;
#98389 = CARTESIAN_POINT ( 'NONE',  ( 2.791683348922240793, 21.63393115100078745, 7.208316651077764092 ) ) ;
#98390 = DIRECTION ( 'NONE',  ( -0.000000000000000000, 0.000000000000000000, 1.000000000000000000 ) ) ;
#98391 = ORIENTED_EDGE ( 'NONE', *, *, #82079, .T. ) ;
#98392 = CARTESIAN_POINT ( 'NONE',  ( 24.16423886937409904, 44.09541550158063927, 3.795296366450317205 ) ) ;
#98393 = CARTESIAN_POINT ( 'NONE',  ( 10.00000000000000178, 7.258931151000785675, 9.846743663894594434 ) ) ;
#98395 = CARTESIAN_POINT ( 'NONE',  ( 4.391700990647064984, 14.76930270348882956, 14.28114200970192016 ) ) ;
#98394 = CARTESIAN_POINT ( 'NONE',  ( -0.1503990784575277573, 63.10158574516643171, 6.262539305110076171 ) ) ;
#98396 = CARTESIAN_POINT ( 'NONE',  ( 7.084665262690076126, 34.10535201082151247, 10.88017736071109987 ) ) ;
#98397 = CARTESIAN_POINT ( 'NONE',  ( -2.816281873526473856, 54.12363466993041783, 9.499525473075851096E-16 ) ) ;
#98398 = CARTESIAN_POINT ( 'NONE',  ( 4.559911319644449179, 8.897018677488171434, 9.422509992056141925 ) ) ;
#98399 = CARTESIAN_POINT ( 'NONE',  ( 3.591859063236761518, 39.95696800326375353, 11.09922568453594849 ) ) ;
#98400 = CARTESIAN_POINT ( 'NONE',  ( 10.00000000000000178, 7.258931151000785675, 9.846743663894594434 ) ) ;
#98401 = ORIENTED_EDGE ( 'NONE', *, *, #51744, .F. ) ;
#98402 = EDGE_CURVE ( 'NONE', #86489, #52526, #91934, .T. ) ;
#98403 = CYLINDRICAL_SURFACE ( 'NONE', #57391, 0.5000000000000004441 ) ;
#98404 = CARTESIAN_POINT ( 'NONE',  ( 10.00000000000000000, 40.55374883491397497, -14.16423886937410082 ) ) ;
#98405 = CARTESIAN_POINT ( 'NONE',  ( 10.00000000000000000, 10.55374883491396787, -14.16423886937410082 ) ) ;
#98406 = CARTESIAN_POINT ( 'NONE',  ( 15.44008868035555260, 9.730352010821505360, 9.422509992056143702 ) ) ;
#98407 = CARTESIAN_POINT ( 'NONE',  ( 17.96484262340118221, 26.18868534415483396, -7.964842623401177768 ) ) ;
#98408 = DIRECTION ( 'NONE',  ( 1.545430450278217904E-13, 0.000000000000000000, 1.000000000000000000 ) ) ;
#98409 = LINE ( 'NONE', #58894, #6466 ) ;
#98410 = CARTESIAN_POINT ( 'NONE',  ( -0.8801773607111008646, 58.27201867748816966, 2.915334737309923430 ) ) ;
#98411 = CARTESIAN_POINT ( 'NONE',  ( -0.8801773607111009756, 58.06368534415484106, 1.068504757029289695E-15 ) ) ;
#98412 = CARTESIAN_POINT ( 'NONE',  ( 6.565887622018943937, 23.08196800326375708, -12.81628187352647608 ) ) ;
#98413 = CARTESIAN_POINT ( 'NONE',  ( 4.880290883660320489, 0.000000000000000000, 2.433223276543894364 ) ) ;
#98414 = CARTESIAN_POINT ( 'NONE',  ( 14.97687855664607781, 0.5000000000000004441, 0.8325315005901553489 ) ) ;
#98415 = CARTESIAN_POINT ( 'NONE',  ( 19.84674366389459266, 23.30059781766745530, 2.638427012816836559 ) ) ;
#98416 = VECTOR ( 'NONE', #17914, 1000.000000000000000 ) ;
#98417 = UNCERTAINTY_MEASURE_WITH_UNIT (LENGTH_MEASURE( 1.000000000000000082E-05 ), #12541, 'distance_accuracy_value', 'NONE');
#98418 = VECTOR ( 'NONE', #7680, 1000.000000000000114 ) ;
#98419 = CARTESIAN_POINT ( 'NONE',  ( 10.00000000000000178, 25.37363466993041783, 12.81628187352647608 ) ) ;
#98420 = PRESENTATION_STYLE_ASSIGNMENT (( #13912 ) ) ;
#98421 = CARTESIAN_POINT ( 'NONE',  ( 0.5774900079438590739, 12.64701867748817143, -5.440088680355550821 ) ) ;
#98422 = AXIS2_PLACEMENT_3D ( 'NONE', #82798, #30279, #83296 ) ;
#98423 = CARTESIAN_POINT ( 'NONE',  ( 10.00000000000000178, 32.25893115100078745, 9.846743663894594434 ) ) ;
#98424 = CARTESIAN_POINT ( 'NONE',  ( 6.565887622018943937, 65.16530133659709634, 12.81628187352647430 ) ) ;
#98425 = CARTESIAN_POINT ( 'NONE',  ( 17.20831665107776587, 19.13393115100078035, -7.208316651077762316 ) ) ;
#98426 = CARTESIAN_POINT ( 'NONE',  ( 24.50000000000000000, 35.99999999999997158, -10.00000000000000000 ) ) ;
#98427 = CARTESIAN_POINT ( 'NONE',  ( -0.8801773607111008646, 28.27201867748817321, 2.915334737309923430 ) ) ;
#98429 = CARTESIAN_POINT ( 'NONE',  ( 2.917880565312950480, 35.97041550158063217, -12.26659068614894821 ) ) ;
#98428 =( LENGTH_UNIT ( ) NAMED_UNIT ( * ) SI_UNIT ( .MILLI., .METRE. ) );
#98430 = CARTESIAN_POINT ( 'NONE',  ( 19.84674366389459266, 48.30059781766745175, 2.638427012816836559 ) ) ;
#98431 = CARTESIAN_POINT ( 'NONE',  ( 10.00000000000000178, 29.31368534415483751, 10.88017736071110342 ) ) ;
#98432 = CARTESIAN_POINT ( 'NONE',  ( 12.91533473730992121, 19.52201867748816611, 10.88017736071110164 ) ) ;
#98433 = VERTEX_POINT ( 'NONE', #60446 ) ;
#98434 = CARTESIAN_POINT ( 'NONE',  ( 12.91533473730993009, 31.60535201082150891, -10.88017736071109987 ) ) ;
#98435 = CARTESIAN_POINT ( 'NONE',  ( 22.81628187352648496, 51.83196800326376064, -3.434112377981050290 ) ) ;
#98436 = CARTESIAN_POINT ( 'NONE',  ( 12.91533473730993009, 41.60535201082149825, -10.88017736071109987 ) ) ;
#98438 = CARTESIAN_POINT ( 'NONE',  ( 4.559911319644449179, 37.23035201082150536, -9.422509992056141925 ) ) ;
#98437 = DIRECTION ( 'NONE',  ( 1.000000000000000000, 0.000000000000000000, 0.000000000000000000 ) ) ;
#98439 = EDGE_LOOP ( 'NONE', ( #34695, #19016, #72204, #66863 ) ) ;
#98440 = CARTESIAN_POINT ( 'NONE',  ( -0.8801773607111008646, 33.27201867748817676, 2.915334737309923430 ) ) ;
#98441 = PLANE ( 'NONE',  #48221 ) ;
#98442 = SURFACE_STYLE_FILL_AREA ( #28430 ) ;
#98443 = CARTESIAN_POINT ( 'NONE',  ( 19.72487221294570858, 70.00000000000000000, 6.500000000000000888 ) ) ;
#98444 = CARTESIAN_POINT ( 'NONE',  ( -2.266590686148945544, 42.22041550158063217, 7.082119434687048631 ) ) ;
#98445 = CARTESIAN_POINT ( 'NONE',  ( 7.084665262690076126, 49.10535201082149825, 10.88017736071109987 ) ) ;
#98446 = CARTESIAN_POINT ( 'NONE',  ( -15.41943733314634635, 15.00000000000000000, 4.256565371896233962 ) ) ;
#98447 = DIRECTION ( 'NONE',  ( 1.257568779154408793E-17, 1.000000000000000000, -0.000000000000000000 ) ) ;
#98448 = CARTESIAN_POINT ( 'NONE',  ( 7.361572987183169658, 64.96726448433412315, -9.846743663894592657 ) ) ;
#98449 = DIRECTION ( 'NONE',  ( -0.9975640502598257520, 0.06975647374410356982, 0.000000000000000000 ) ) ;
#98450 = CARTESIAN_POINT ( 'NONE',  ( 7.361572987183170547, 37.05059781766744464, 9.846743663894590881 ) ) ;
#98451 = ORIENTED_EDGE ( 'NONE', *, *, #98463, .F. ) ;
#98452 = CARTESIAN_POINT ( 'NONE',  ( 18.52753015748617571, 38.09226448433412315, 4.923371831947298993 ) ) ;
#98453 = CARTESIAN_POINT ( 'NONE',  ( 12.81628187352647608, -23.37636533006957507, -2.602085213965210642E-15 ) ) ;
#98454 = CARTESIAN_POINT ( 'NONE',  ( 19.42250999205614193, 25.14701867748817321, 5.440088680355555262 ) ) ;
#98455 = CARTESIAN_POINT ( 'NONE',  ( 17.20831665107776587, 32.88393115100078745, 7.208316651077764980 ) ) ;
#98456 = CARTESIAN_POINT ( 'NONE',  ( 22.81628187352648496, 26.83196800326374998, -3.434112377981050290 ) ) ;
#98458 = CARTESIAN_POINT ( 'NONE',  ( 4.559911319644449179, 57.23035201082150536, -9.422509992056141925 ) ) ;
#98457 = LINE ( 'NONE', #29913, #5202 ) ;
#98460 = CARTESIAN_POINT ( 'NONE',  ( 17.96484262340118221, 4.938685344154837509, 7.964842623401181321 ) ) ;
#98459 = CARTESIAN_POINT ( 'NONE',  ( -0.8801773607111009756, 28.06368534415484106, 1.068504757029289695E-15 ) ) ;
#98461 = CARTESIAN_POINT ( 'NONE',  ( 6.204703633549690345, 47.84541550158064638, 14.16423886937410082 ) ) ;
#98462 = STYLED_ITEM ( 'NONE', ( #39229 ), #55104 ) ;
#98463 = EDGE_CURVE ( 'NONE', #48799, #24087, #17812, .T. ) ;
#98464 = COLOUR_RGB ( '', 0.72549020, 0.75294118, 0.79215686) ;
#98465 = FACE_OUTER_BOUND ( 'NONE', #7086, .T. ) ;
#98466 = ORIENTED_EDGE ( 'NONE', *, *, #71412, .T. ) ;
#98467 = CARTESIAN_POINT ( 'NONE',  ( 13.43411237798105340, 15.58196800326374998, 12.81628187352647963 ) ) ;
#98468 = CARTESIAN_POINT ( 'NONE',  ( -0.8801773607111008646, 8.272018677488171434, 2.915334737309923430 ) ) ;
#98469 = AXIS2_PLACEMENT_3D ( 'NONE', #90396, #21935, #52415 ) ;
#98470 = CARTESIAN_POINT ( 'NONE',  ( 17.96484262340118221, 44.93868534415483396, 7.964842623401181321 ) ) ;
#98471 = ORIENTED_EDGE ( 'NONE', *, *, #89157, .T. ) ;
#98472 = CARTESIAN_POINT ( 'NONE',  ( 17.96484262340118221, 61.18868534415482685, -7.964842623401177768 ) ) ;
#98473 = CARTESIAN_POINT ( 'NONE',  ( 1.472469842513823179, 31.42559781766745530, 4.923371831947296329 ) ) ;
#98474 = CARTESIAN_POINT ( 'NONE',  ( 10.00000000000000178, 27.25893115100078390, 9.846743663894594434 ) ) ;
#98475 = CARTESIAN_POINT ( 'NONE',  ( 19.84674366389459621, 13.50893115100078568, 7.409399052514197653E-17 ) ) ;
#98476 = CARTESIAN_POINT ( 'NONE',  ( 14.88585913060025945, 14.76984981697140142, -1.278057234793439800 ) ) ;
#98478 = CARTESIAN_POINT ( 'NONE',  ( 16.40814093676323893, 40.79030133659708923, 11.09922568453595026 ) ) ;
#98477 = CARTESIAN_POINT ( 'NONE',  ( -7.037799270021981357, -86.25965645051654462, 2.749999999998387956 ) ) ;
#98480 = CARTESIAN_POINT ( 'NONE',  ( 0.6081133539230531015, 33.33703382326400089, 6.499999999999970690 ) ) ;
#98479 = CARTESIAN_POINT ( 'NONE',  ( 18.52753015748618282, 18.92559781766745175, -4.923371831947291888 ) ) ;
#98481 = CARTESIAN_POINT ( 'NONE',  ( 7.160365893312771846, -84.29711206764778808, -4.000000000000000000 ) ) ;
#98482 = AXIS2_PLACEMENT_3D ( 'NONE', #53711, #69219, #745 ) ;
#98484 = ORIENTED_EDGE ( 'NONE', *, *, #18200, .T. ) ;
#98483 = CARTESIAN_POINT ( 'NONE',  ( 18.52753015748617571, 33.09226448433411605, 4.923371831947298993 ) ) ;
#98485 = DIRECTION ( 'NONE',  ( 1.000000000000000000, -0.000000000000000000, -0.000000000000000000 ) ) ;
#98486 = EDGE_CURVE ( 'NONE', #55365, #22543, #77569, .T. ) ;
#98487 = CARTESIAN_POINT ( 'NONE',  ( 16.40814093676323893, 5.790301336597087456, 11.09922568453595026 ) ) ;
#98488 = CARTESIAN_POINT ( 'NONE',  ( 4.559911319644449179, 47.23035201082150536, -9.422509992056141925 ) ) ;
#98489 = CARTESIAN_POINT ( 'NONE',  ( -0.3689425029237898834, 26.17874883491396432, -10.36894250292378850 ) ) ;
#98490 =( BOUNDED_CURVE ( )  B_SPLINE_CURVE ( 3, ( #41545, #72009, #80006, #87997 ),
 .UNSPECIFIED., .F., .F. ) 
 B_SPLINE_CURVE_WITH_KNOTS ( ( 4, 4 ),
 ( 0.000000000000000000, 1.570796326794896558 ),
 .UNSPECIFIED. ) 
 CURVE ( )  GEOMETRIC_REPRESENTATION_ITEM ( )  RATIONAL_B_SPLINE_CURVE ( ( 1.000000000000000000, 0.8047378541243649375, 0.8047378541243649375, 1.000000000000000000 ) ) 
 REPRESENTATION_ITEM ( '' )  );
#98491 = EDGE_CURVE ( 'NONE', #69569, #7550, #28018, .T. ) ;
#98492 = LINE ( 'NONE', #5988, #95088 ) ;
#98493 = CARTESIAN_POINT ( 'NONE',  ( 2.917880565312948704, 32.63708216824730357, 12.26659068614894643 ) ) ;
#98494 = CARTESIAN_POINT ( 'NONE',  ( 24.16423886937409904, 49.09541550158063217, 3.795296366450317205 ) ) ;
#98495 = CARTESIAN_POINT ( 'NONE',  ( 22.26659068614894466, 13.88708216824730179, 7.082119434687054849 ) ) ;
#98497 = CARTESIAN_POINT ( 'NONE',  ( -0.1503990784575247319, 37.22266099184918176, -6.262539305110083276 ) ) ;
#98496 = CARTESIAN_POINT ( 'NONE',  ( 22.26659068614894466, 13.88708216824730179, 7.082119434687054849 ) ) ;
#98498 = CARTESIAN_POINT ( 'NONE',  ( 10.00000000000000178, 44.31368534415484106, 10.88017736071110342 ) ) ;
#98499 = CARTESIAN_POINT ( 'NONE',  ( -9.742785792574940373, 9.701366962315987053, -5.624999999999991118 ) ) ;
#98500 = CARTESIAN_POINT ( 'NONE',  ( 19.84674366389459266, 33.30059781766744464, 2.638427012816836559 ) ) ;
#98502 = CARTESIAN_POINT ( 'NONE',  ( 2.791683348922240793, 46.63393115100077324, 7.208316651077764092 ) ) ;
#98501 = LINE ( 'NONE', #5509, #88405 ) ;
#98503 = VECTOR ( 'NONE', #285, 999.9999999999998863 ) ;
#98504 = CARTESIAN_POINT ( 'NONE',  ( 2.035157376598824452, 28.68868534415484106, 7.964842623401179544 ) ) ;
#98505 = CARTESIAN_POINT ( 'NONE',  ( 13.43411237798106583, 62.66530133659708923, -12.81628187352647252 ) ) ;
#98506 = CARTESIAN_POINT ( 'NONE',  ( 12.63842701281683922, 64.55059781766745175, -9.846743663894590881 ) ) ;
#98507 = CARTESIAN_POINT ( 'NONE',  ( 14.26139399674457309, 4.693468746458063789E-16, -2.619664342929806988 ) ) ;
#98508 = CARTESIAN_POINT ( 'NONE',  ( 18.52753015748618282, 23.92559781766745530, -4.923371831947291888 ) ) ;
#98509 = CARTESIAN_POINT ( 'NONE',  ( -2.816281873526473856, 44.33196800326375353, 3.434112377981055619 ) ) ;
#98510 = CARTESIAN_POINT ( 'NONE',  ( 14.16423886937410259, -25.69625116508602858, -2.602085213965210642E-15 ) ) ;
#98511 = AXIS2_PLACEMENT_3D ( 'NONE', #78652, #710, #47657 ) ;
#98512 = CARTESIAN_POINT ( 'NONE',  ( 15.44008868035555260, 44.73035201082151247, 9.422509992056143702 ) ) ;
#98513 = CARTESIAN_POINT ( 'NONE',  ( 18.52753015748617571, 48.09226448433412315, 4.923371831947298993 ) ) ;
#98514 = CARTESIAN_POINT ( 'NONE',  ( 13.79529636645030344, 28.26208216824729647, 14.16423886937410614 ) ) ;
#98515 = VECTOR ( 'NONE', #74600, 1000.000000000000000 ) ;
#98516 = ORIENTED_EDGE ( 'NONE', *, *, #15946, .F. ) ;
#98517 = FILL_AREA_STYLE ('',( #74988 ) ) ;
#98518 = CARTESIAN_POINT ( 'NONE',  ( 20.88017736071110164, 65.35535201082150536, 2.915334737309930979 ) ) ;
#98519 = CARTESIAN_POINT ( 'NONE',  ( -0.8801773607111009756, 68.06368534415484817, 1.068504757029289695E-15 ) ) ;
#98520 = CARTESIAN_POINT ( 'NONE',  ( 13.79529636645031943, 65.34541550158063217, -14.16423886937409904 ) ) ;
#98521 = CARTESIAN_POINT ( 'NONE',  ( -1.099225684535947600, 3.706968003263753531, -6.408140936763238038 ) ) ;
#98522 = FACE_OUTER_BOUND ( 'NONE', #47458, .T. ) ;
#98523 = CARTESIAN_POINT ( 'NONE',  ( 20.88017736071110875, 50.77201867748817676, -2.915334737309920765 ) ) ;
#98524 = CARTESIAN_POINT ( 'NONE',  ( 8.629999999999995453, 41.24999999999999289, -6.250000000000000000 ) ) ;
#98525 = CARTESIAN_POINT ( 'NONE',  ( 3.640395162852214650, 89.00000000000000000, 9.500000000000000000 ) ) ;
#98526 = CARTESIAN_POINT ( 'NONE',  ( -1.099225684535947600, 29.54030133659708923, 6.408140936763237150 ) ) ;
#98527 = CARTESIAN_POINT ( 'NONE',  ( -4.164238869374098151, 51.59541550158063217, -3.795296366450310543 ) ) ;
#98528 = CARTESIAN_POINT ( 'NONE',  ( 7.964842623401177768, 31.18868534415484461, -7.964842623401181321 ) ) ;
#98529 = CARTESIAN_POINT ( 'NONE',  ( 7.084665262690076126, 7.022018677488169658, -10.88017736071110164 ) ) ;
#98530 = CARTESIAN_POINT ( 'NONE',  ( 20.88017736071110519, 20.56368534415484106, 2.639326808657452039E-16 ) ) ;
#98531 = CARTESIAN_POINT ( 'NONE',  ( 19.84674366389459621, 53.50893115100078745, 7.409399052514197653E-17 ) ) ;
#98532 = CARTESIAN_POINT ( 'NONE',  ( 3.591859063236763294, 48.29030133659708923, -11.09922568453595026 ) ) ;
#98533 = DIRECTION ( 'NONE',  ( -0.9812560818990571088, -0.1927083333333329818, 0.000000000000000000 ) ) ;
#98534 = ORIENTED_EDGE ( 'NONE', *, *, #95617, .T. ) ;
#98535 = EDGE_CURVE ( 'NONE', #70022, #1146, #70999, .T. ) ;
#98536 = CARTESIAN_POINT ( 'NONE',  ( 19.42250999205614548, 20.98035201082150891, -5.440088680355545492 ) ) ;
#98537 = CARTESIAN_POINT ( 'NONE',  ( 16.40814093676323893, 15.79030133659708746, 11.09922568453595026 ) ) ;
#98538 = LINE ( 'NONE', #91495, #59270 ) ;
#98539 = AXIS2_PLACEMENT_3D ( 'NONE', #49119, #19111, #49591 ) ;
#98540 = CARTESIAN_POINT ( 'NONE',  ( 18.52753015748617571, 48.09226448433412315, 4.923371831947298993 ) ) ;
#98541 = CARTESIAN_POINT ( 'NONE',  ( 12.91533473730992121, 34.52201867748817676, 10.88017736071110164 ) ) ;
#98542 = CARTESIAN_POINT ( 'NONE',  ( 22.81628187352648496, 21.83196800326374643, -3.434112377981050290 ) ) ;
#98544 = DIRECTION ( 'NONE',  ( 5.818595309480553908E-17, 1.000000000000000000, 0.000000000000000000 ) ) ;
#98543 = CARTESIAN_POINT ( 'NONE',  ( 0.5774900079438607392, 48.48035201082150536, 5.440088680355550821 ) ) ;
#98545 = CYLINDRICAL_SURFACE ( 'NONE', #44930, 0.5000000000000004441 ) ;
#98546 = CARTESIAN_POINT ( 'NONE',  ( 21.09922568453595559, 47.04030133659708923, -6.408140936763230044 ) ) ;
#98547 = VERTEX_POINT ( 'NONE', #6965 ) ;
#98548 = CARTESIAN_POINT ( 'NONE',  ( 0.5774900079438590739, 42.64701867748816966, -5.440088680355550821 ) ) ;
#98550 = CARTESIAN_POINT ( 'NONE',  ( 2.917880565312950480, 0.9704155015806342766, -12.26659068614894821 ) ) ;
#98549 = CARTESIAN_POINT ( 'NONE',  ( -2.816281873526473856, 34.12363466993042493, 9.499525473075851096E-16 ) ) ;
#98551 = CARTESIAN_POINT ( 'NONE',  ( 12.63842701281683922, 9.550597817667449974, -9.846743663894590881 ) ) ;
#98552 = CARTESIAN_POINT ( 'NONE',  ( 4.559911319644449179, 38.89701867748817676, 9.422509992056141925 ) ) ;
#98553 = CARTESIAN_POINT ( 'NONE',  ( 19.84674366389459266, 63.71726448433412315, -2.638427012816827677 ) ) ;
#98554 = SURFACE_SIDE_STYLE ('',( #7031 ) ) ;
#98555 = CARTESIAN_POINT ( 'NONE',  ( 19.84674366389459621, 23.50893115100078390, 7.409399052514197653E-17 ) ) ;
#98556 = CARTESIAN_POINT ( 'NONE',  ( 0.1532563361054100626, 5.800597817667452638, -2.638427012816831230 ) ) ;
#98557 = DIRECTION ( 'NONE',  ( 0.000000000000000000, 1.000000000000000000, 0.000000000000000000 ) ) ;
#98558 = CARTESIAN_POINT ( 'NONE',  ( 24.16423886937410614, 44.51208216824730357, -3.795296366450302550 ) ) ;
#98559 = CARTESIAN_POINT ( 'NONE',  ( 6.336100170400922771, 14.76984879808201434, -13.53056138701887967 ) ) ;
#98560 = CARTESIAN_POINT ( 'NONE',  ( 10.00000000000000000, 6.813685344154838397, -10.88017736071110342 ) ) ;
#98561 = CARTESIAN_POINT ( 'NONE',  ( 17.35999999999999943, 33.99999999999997158, 9.500000000000000000 ) ) ;
#98562 = ORIENTED_EDGE ( 'NONE', *, *, #88208, .T. ) ;
#98563 = CARTESIAN_POINT ( 'NONE',  ( -0.8801773607111008646, 13.27201867748817321, 2.915334737309923430 ) ) ;
#98564 = CARTESIAN_POINT ( 'NONE',  ( -0.3689425029237881626, 62.42874883491396787, 10.36894250292379027 ) ) ;
#98565 = CARTESIAN_POINT ( 'NONE',  ( 17.20831665107776587, 47.88393115100078745, 7.208316651077764980 ) ) ;
#98566 = CARTESIAN_POINT ( 'NONE',  ( 21.09922568453595559, 37.04030133659708923, -6.408140936763230044 ) ) ;
#98567 = CARTESIAN_POINT ( 'NONE',  ( 4.096035146093531587, 15.00000000000000000, -13.90943910019259278 ) ) ;
#98569 = CARTESIAN_POINT ( 'NONE',  ( 22.26659068614895176, 4.720415501580633943, -7.082119434687042414 ) ) ;
#98568 = CARTESIAN_POINT ( 'NONE',  ( -13.80105244024794331, 90.89655890636515778, -7.750000000004162892 ) ) ;
#98570 = CARTESIAN_POINT ( 'NONE',  ( 19.42250999205614193, 10.14701867748816966, 5.440088680355555262 ) ) ;
#98571 = CARTESIAN_POINT ( 'NONE',  ( 10.00000000000000178, 58.05374883491397497, 14.16423886937410082 ) ) ;
#98572 = PRODUCT ( '1.4 Rivet', '1.4 Rivet', '', ( #89719 ) ) ;
#98573 = AXIS2_PLACEMENT_3D ( 'NONE', #96124, #88597, #12604 ) ;
#98574 = CARTESIAN_POINT ( 'NONE',  ( 12.63842701281683922, 39.55059781766744464, -9.846743663894590881 ) ) ;
#98575 = CARTESIAN_POINT ( 'NONE',  ( -0.1306922352674164955, 0.1302365040536442309, 6.294480393734140478 ) ) ;
#98576 = CARTESIAN_POINT ( 'NONE',  ( 17.20831665107776587, 19.13393115100078035, -7.208316651077762316 ) ) ;
#98577 = CARTESIAN_POINT ( 'NONE',  ( 5.076628168052704559, 0.1755978176674514724, -8.527530157486179263 ) ) ;
#98578 = CARTESIAN_POINT ( 'NONE',  ( -8.527530157486173934, 16.42559781766746241, 4.923371831947302546 ) ) ;
#98579 = AXIS2_PLACEMENT_3D ( 'NONE', #47765, #96110, #40766 ) ;
#98580 = ORIENTED_EDGE ( 'NONE', *, *, #68707, .F. ) ;
#98581 = ORIENTED_EDGE ( 'NONE', *, *, #84783, .F. ) ;
#98582 = APPLICATION_CONTEXT ( 'automotive_design' ) ;
#98583 = EDGE_LOOP ( 'NONE', ( #77627, #87983, #96351, #84697 ) ) ;
#98585 = CARTESIAN_POINT ( 'NONE',  ( 18.52753015748617571, 53.09226448433412315, 4.923371831947298993 ) ) ;
#98584 = AXIS2_PLACEMENT_3D ( 'NONE', #86433, #64873, #2463 ) ;
#98587 = CARTESIAN_POINT ( 'NONE',  ( 7.084665262690076126, 32.02201867748816966, -10.88017736071110164 ) ) ;
#98586 = CARTESIAN_POINT ( 'NONE',  ( 0.5774900079438590739, 37.64701867748817676, -5.440088680355550821 ) ) ;
#98589 = CARTESIAN_POINT ( 'NONE',  ( 19.38216949554541557, 27.24863466993041783, -9.382169495545420901 ) ) ;
#98588 = CARTESIAN_POINT ( 'NONE',  ( 10.00000000000000178, 57.25893115100078745, 9.846743663894594434 ) ) ;
#98590 =( NAMED_UNIT ( * ) SI_UNIT ( $, .STERADIAN. ) SOLID_ANGLE_UNIT ( ) );
#98591 = EDGE_CURVE ( 'NONE', #48625, #24045, #37473, .T. ) ;
#98592 = VECTOR ( 'NONE', #46552, 999.9999999999998863 ) ;
#98593 = CARTESIAN_POINT ( 'NONE',  ( 22.81628187352647785, 31.41530133659709279, 3.434112377981063169 ) ) ;
#98594 = EDGE_LOOP ( 'NONE', ( #94833, #8643, #81671, #84067, #82794, #76561 ) ) ;
#98595 = CARTESIAN_POINT ( 'NONE',  ( 12.63842701281683034, 42.46726448433412315, 9.846743663894596210 ) ) ;
#98596 = CARTESIAN_POINT ( 'NONE',  ( 0.5774900079438607392, 3.480352010821504916, 5.440088680355550821 ) ) ;
#98597 = ORIENTED_EDGE ( 'NONE', *, *, #58950, .F. ) ;
#98598 = CARTESIAN_POINT ( 'NONE',  ( 7.084665262690076126, 12.02201867748817321, -10.88017736071110164 ) ) ;
#98599 = ORIENTED_EDGE ( 'NONE', *, *, #74975, .T. ) ;
#98600 = CARTESIAN_POINT ( 'NONE',  ( 12.91533473730993009, 66.60535201082150536, -10.88017736071109987 ) ) ;
#98601 = CARTESIAN_POINT ( 'NONE',  ( 12.91533473730992121, 54.52201867748816255, 10.88017736071110164 ) ) ;
#98602 = CARTESIAN_POINT ( 'NONE',  ( 19.42250999205614548, 60.98035201082151247, -5.440088680355545492 ) ) ;
#98603 = PRODUCT ( '1.2 Movable Jaw', '1.2 Movable Jaw', '', ( #80252 ) ) ;
#98604 = CARTESIAN_POINT ( 'NONE',  ( 7.084665262690076126, 54.10535201082151247, 10.88017736071109987 ) ) ;
#98605 = CARTESIAN_POINT ( 'NONE',  ( -0.1503990784575328643, 30.12777174578613781, 6.262539305110068177 ) ) ;
#98606 = CARTESIAN_POINT ( 'NONE',  ( -46.94000000000001194, 100.8028158894829289, 8.422108456579607605 ) ) ;
#98607 = ORIENTED_EDGE ( 'NONE', *, *, #36807, .F. ) ;
#98608 = EDGE_CURVE ( 'NONE', #17079, #75926, #22465, .T. ) ;
#98609 = CARTESIAN_POINT ( 'NONE',  ( 14.92337183194729633, 47.67559781766745175, 8.527530157486181039 ) ) ;
#98610 = ORIENTED_EDGE ( 'NONE', *, *, #39906, .F. ) ;
#98611 = CARTESIAN_POINT ( 'NONE',  ( 1.983216688680936812, 15.00000000000000000, -14.11131997956737649 ) ) ;
#98612 =( NAMED_UNIT ( * ) PLANE_ANGLE_UNIT ( ) SI_UNIT ( $, .RADIAN. ) );
#98613 = COLOUR_RGB ( '', 0.40784314, 0.44705882, 0.49803922) ;
#98614 = ADVANCED_FACE ( 'NONE', ( #52941 ), #53341, .T. ) ;
#98615 = CARTESIAN_POINT ( 'NONE',  ( 20.36894250292379382, 3.678748834913967869, 10.36894250292379205 ) ) ;
#98616 = ORIENTED_EDGE ( 'NONE', *, *, #59796, .T. ) ;
#98617 = CARTESIAN_POINT ( 'NONE',  ( 4.431036607602466759, 15.00000000000000000, 14.33059365769913818 ) ) ;
#98618 = DIRECTION ( 'NONE',  ( -0.000000000000000000, -1.000000000000000000, -0.000000000000000000 ) ) ;
#98619 = CARTESIAN_POINT ( 'NONE',  ( -0.8801773607111009756, 3.063685344154838397, 1.068504757029289695E-15 ) ) ;
#98621 = ORIENTED_EDGE ( 'NONE', *, *, #89428, .T. ) ;
#98620 = CARTESIAN_POINT ( 'NONE',  ( 13.43411237798106583, 37.66530133659708923, -12.81628187352647252 ) ) ;
#98622 = CARTESIAN_POINT ( 'NONE',  ( 11.62719953690066355, 0.3639310419529870333, -9.476720473301831760 ) ) ;
#98623 = CARTESIAN_POINT ( 'NONE',  ( 1.472469842513823179, 46.42559781766745175, 4.923371831947296329 ) ) ;
#98624 = CARTESIAN_POINT ( 'NONE',  ( 6.761389522993885848, 14.76930270348881002, -13.32372569557300146 ) ) ;
#98625 = CARTESIAN_POINT ( 'NONE',  ( 19.38216949554541557, 12.24863466993041961, -9.382169495545420901 ) ) ;
#98626 = CARTESIAN_POINT ( 'NONE',  ( 7.361572987183169658, 24.96726448433412315, -9.846743663894592657 ) ) ;
#98627 = CARTESIAN_POINT ( 'NONE',  ( 1.046131998950049491, 35.73810908735726599, 6.499999999999992006 ) ) ;
#98628 = CARTESIAN_POINT ( 'NONE',  ( -1.099225684535947600, -0.4596986634029132657, 6.408140936763237150 ) ) ;
#98629 = DIRECTION ( 'NONE',  ( 0.000000000000000000, 0.000000000000000000, 1.000000000000000000 ) ) ;
#98630 = EDGE_LOOP ( 'NONE', ( #2746, #28530, #21422, #81010 ) ) ;
#98631 = ORIENTED_EDGE ( 'NONE', *, *, #54420, .F. ) ;
#98632 = CARTESIAN_POINT ( 'NONE',  ( 20.88017736071110164, 25.35535201082150891, 2.915334737309930979 ) ) ;
#98633 = CARTESIAN_POINT ( 'NONE',  ( 2.917880565312950480, 20.97041550158063217, -12.26659068614894821 ) ) ;
#98634 = CARTESIAN_POINT ( 'NONE',  ( 19.84674366389459621, 23.50893115100078390, 7.409399052514197653E-17 ) ) ;
#98635 = CARTESIAN_POINT ( 'NONE',  ( 4.559911319644449179, 68.89701867748817676, 9.422509992056141925 ) ) ;
#98637 = DIRECTION ( 'NONE',  ( 0.000000000000000000, 0.000000000000000000, -1.000000000000000000 ) ) ;
#98636 = CARTESIAN_POINT ( 'NONE',  ( -2.816281873526473856, 39.12363466993041783, 9.499525473075851096E-16 ) ) ;
#98638 = CARTESIAN_POINT ( 'NONE',  ( 17.96484262340118221, 16.18868534415483396, -7.964842623401177768 ) ) ;
#98639 = B_SPLINE_CURVE_WITH_KNOTS ( 'NONE', 3,
 ( #23223, #76211, #68709, #30688, #76690, #59216 ),
 .UNSPECIFIED., .F., .F.,
 ( 4, 2, 4 ),
 ( 0.0002800124554063431175, 0.0006862178066574521314, 0.001092423157908561145 ),
 .UNSPECIFIED. ) ;
#98640 = CARTESIAN_POINT ( 'NONE',  ( 7.109031286574862385, 14.95037114371795894, -12.92745085449638509 ) ) ;
#98641 = EDGE_CURVE ( 'NONE', #93159, #57516, #14973, .T. ) ;
#98642 = CARTESIAN_POINT ( 'NONE',  ( 3.591859063236763294, 13.29030133659708746, -11.09922568453595026 ) ) ;
#98643 = CARTESIAN_POINT ( 'NONE',  ( 19.38216949554541202, 5.998634669930420493, 9.382169495545424454 ) ) ;
#98644 = CARTESIAN_POINT ( 'NONE',  ( 12.63842701281683922, 29.55059781766745175, -9.846743663894590881 ) ) ;
#98645 = CARTESIAN_POINT ( 'NONE',  ( 9.422509992056141925, -9.019647989178487535, -5.440088680355554374 ) ) ;
#98646 = CARTESIAN_POINT ( 'NONE',  ( -2.816281873526471635, 38.91530133659708213, -3.434112377981056508 ) ) ;
#98647 = CARTESIAN_POINT ( 'NONE',  ( 11.34661744925197624, 54.08985607419764818, 0.000000000000000000 ) ) ;
#98649 = CARTESIAN_POINT ( 'NONE',  ( 14.97687855664608314, 0.3640475087720990155, 0.8325315005901587906 ) ) ;
#98648 = CARTESIAN_POINT ( 'NONE',  ( -0.8801773607111009756, 43.06368534415484106, 1.068504757029289695E-15 ) ) ;
#98650 = AXIS2_PLACEMENT_3D ( 'NONE', #46337, #76823, #69834 ) ;
#98651 = EDGE_CURVE ( 'NONE', #46867, #48771, #64458, .T. ) ;
#98652 = AXIS2_PLACEMENT_3D ( 'NONE', #34356, #57361, #19375 ) ;
#98653 = DIRECTION ( 'NONE',  ( -0.000000000000000000, -1.000000000000000000, -0.000000000000000000 ) ) ;
#98654 = CARTESIAN_POINT ( 'NONE',  ( 7.084665262690076126, 67.02201867748817676, -10.88017736071110164 ) ) ;
#98655 = CARTESIAN_POINT ( 'NONE',  ( 20.88017736071110164, 40.35535201082150536, 2.915334737309930979 ) ) ;
#98656 = CARTESIAN_POINT ( 'NONE',  ( 4.559911319644449179, 42.23035201082151247, -9.422509992056141925 ) ) ;
#98657 = CARTESIAN_POINT ( 'NONE',  ( 1.472469842513823179, 60.59226448433412315, -4.923371831947296329 ) ) ;
#98658 = CARTESIAN_POINT ( 'NONE',  ( 2.035157376598824452, 68.68868534415484817, 7.964842623401179544 ) ) ;
#98659 = CARTESIAN_POINT ( 'NONE',  ( 19.84674366389459266, 48.30059781766745175, 2.638427012816836559 ) ) ;
#98661 = CARTESIAN_POINT ( 'NONE',  ( -4.182615635448458491, 26.60017725333985794, 10.00000000000000000 ) ) ;
#98660 = CARTESIAN_POINT ( 'NONE',  ( 20.88017736071110164, 5.355352010821502695, 2.915334737309930979 ) ) ;
#98662 = CARTESIAN_POINT ( 'NONE',  ( 19.38216949554541557, 17.24863466993041783, -9.382169495545420901 ) ) ;
#98663 = ORIENTED_EDGE ( 'NONE', *, *, #46768, .F. ) ;
#98664 = CARTESIAN_POINT ( 'NONE',  ( 12.91533473730993009, 36.60535201082151247, -10.88017736071109987 ) ) ;
#98665 = EDGE_CURVE ( 'NONE', #87189, #61498, #29423, .T. ) ;
#98666 = DIRECTION ( 'NONE',  ( 0.000000000000000000, 0.000000000000000000, 1.000000000000000000 ) ) ;
#98667 = CARTESIAN_POINT ( 'NONE',  ( 20.88017736071110519, 5.563685344154837509, 2.639326808657452039E-16 ) ) ;
#98668 = CARTESIAN_POINT ( 'NONE',  ( 15.44008868035555793, 26.39701867748817321, -9.422509992056140149 ) ) ;
#98669 = CARTESIAN_POINT ( 'NONE',  ( 20.36894250292379382, 43.67874883491397497, 10.36894250292379205 ) ) ;
#98670 = CARTESIAN_POINT ( 'NONE',  ( 0.1532563361054100626, 20.80059781766744464, -2.638427012816831230 ) ) ;
#98671 = CARTESIAN_POINT ( 'NONE',  ( 20.88017736071110875, 50.77201867748817676, -2.915334737309920765 ) ) ;
#98672 = SURFACE_SIDE_STYLE ('',( #7146 ) ) ;
#98673 = CARTESIAN_POINT ( 'NONE',  ( 5.783708210301603536, -36.05554043948455245, 2.500000000000000000 ) ) ;
#98674 = CARTESIAN_POINT ( 'NONE',  ( 12.63842701281683034, 62.46726448433410894, 9.846743663894596210 ) ) ;
#98675 = ORIENTED_EDGE ( 'NONE', *, *, #68407, .T. ) ;
#98676 = VERTEX_POINT ( 'NONE', #39922 ) ;
#98677 = CARTESIAN_POINT ( 'NONE',  ( -4.164238869374098151, 16.59541550158063927, -3.795296366450310543 ) ) ;
#98678 = CARTESIAN_POINT ( 'NONE',  ( 22.26659068614894466, 23.88708216824730357, 7.082119434687054849 ) ) ;
#98679 = CARTESIAN_POINT ( 'NONE',  ( 10.00000000000000178, 59.31368534415484106, 10.88017736071110342 ) ) ;
#98680 = CARTESIAN_POINT ( 'NONE',  ( 10.00000000000000178, 68.05374883491397497, 14.16423886937410082 ) ) ;
#98681 = CARTESIAN_POINT ( 'NONE',  ( 14.92337183194729633, 47.67559781766745175, 8.527530157486181039 ) ) ;
#98682 = CARTESIAN_POINT ( 'NONE',  ( -8.000000002517667852, -0.01653120533954156174, 4.000000000000000000 ) ) ;
#98684 = CARTESIAN_POINT ( 'NONE',  ( 16.40814093676324603, 17.45696800326375353, -11.09922568453594671 ) ) ;
#98683 = CARTESIAN_POINT ( 'NONE',  ( 2.035157376598822676, 42.43868534415483396, -7.964842623401177768 ) ) ;
#98685 = CARTESIAN_POINT ( 'NONE',  ( 24.16423886937409904, 19.09541550158063927, 3.795296366450317205 ) ) ;
#98686 = CARTESIAN_POINT ( 'NONE',  ( 12.91533473730992121, 9.522018677488171434, 10.88017736071110164 ) ) ;
#98687 = CARTESIAN_POINT ( 'NONE',  ( 19.42250999205614548, 30.98035201082150536, -5.440088680355545492 ) ) ;
#98688 = CARTESIAN_POINT ( 'NONE',  ( -0.8801773607111009756, 58.06368534415484106, 1.068504757029289695E-15 ) ) ;
#98689 = CARTESIAN_POINT ( 'NONE',  ( 22.81628187352648496, 46.83196800326376064, -3.434112377981050290 ) ) ;
#98690 = CARTESIAN_POINT ( 'NONE',  ( 2.638427012816829897, -30.44940218233254825, -9.846743663894592657 ) ) ;
#98691 = ORIENTED_EDGE ( 'NONE', *, *, #67760, .F. ) ;
#98692 = CARTESIAN_POINT ( 'NONE',  ( 19.72487221294571569, 34.78217586085237656, 6.499999999999993783 ) ) ;
#98693 = VERTEX_POINT ( 'NONE', #95375 ) ;
#98694 = CARTESIAN_POINT ( 'NONE',  ( 3.969999999999999751, 10.00000000000000000, -2.750000000000000000 ) ) ;
#98695 = VERTEX_POINT ( 'NONE', #2439 ) ;
#98696 = CARTESIAN_POINT ( 'NONE',  ( -0.7577696756377649834, 0.2301502180065688186, 14.92139465029743839 ) ) ;
#98698 = CARTESIAN_POINT ( 'NONE',  ( -0.3689425029237881626, 67.42874883491396076, 10.36894250292379027 ) ) ;
#98697 = CARTESIAN_POINT ( 'NONE',  ( -0.3689425029237898834, 66.17874883491396076, -10.36894250292378850 ) ) ;
#98700 = CARTESIAN_POINT ( 'NONE',  ( 14.92337183194729988, 54.34226448433412315, -8.527530157486177487 ) ) ;
#98699 = CARTESIAN_POINT ( 'NONE',  ( 5.076628168052703671, 16.84226448433411960, 8.527530157486179263 ) ) ;
#98701 = CYLINDRICAL_SURFACE ( 'NONE', #69453, 0.2500000000000002220 ) ;
#98702 = EDGE_CURVE ( 'NONE', #19349, #91342, #64371, .T. ) ;
#98703 = CONICAL_SURFACE ( 'NONE', #22028, 11.25000000000000178, 0.7853981633974497223 ) ;
#98704 = CARTESIAN_POINT ( 'NONE',  ( 0.5774900079438590739, 67.64701867748817676, -5.440088680355550821 ) ) ;
#98705 = EDGE_CURVE ( 'NONE', #21472, #81788, #77909, .T. ) ;
#98706 = CARTESIAN_POINT ( 'NONE',  ( -11.09922568453595382, 23.70696800326376064, -6.408140936763226492 ) ) ;
#98707 = ORIENTED_EDGE ( 'NONE', *, *, #17287, .T. ) ;
#98708 = CARTESIAN_POINT ( 'NONE',  ( -0.3689425029237881626, 27.42874883491397142, 10.36894250292379027 ) ) ;
#98709 = ORIENTED_EDGE ( 'NONE', *, *, #3851, .T. ) ;
#98710 = CARTESIAN_POINT ( 'NONE',  ( 10.00000000000000178, 43.05374883491397497, 14.16423886937410082 ) ) ;
#98711 = ORIENTED_EDGE ( 'NONE', *, *, #57984, .T. ) ;
#98712 = CARTESIAN_POINT ( 'NONE',  ( 22.81628187352647785, 61.62363466993041783, 6.195893100308588602E-16 ) ) ;
#98713 = VECTOR ( 'NONE', #30186, 1000.000000000000000 ) ;
#98714 = CARTESIAN_POINT ( 'NONE',  ( 18.52753015748618282, 48.92559781766745886, -4.923371831947291888 ) ) ;
#98715 = CARTESIAN_POINT ( 'NONE',  ( 19.42250999205614193, 25.14701867748817321, 5.440088680355555262 ) ) ;
#98716 = CARTESIAN_POINT ( 'NONE',  ( 6.565887622018943937, 65.16530133659709634, 12.81628187352647430 ) ) ;
#98717 = PLANE ( 'NONE',  #44733 ) ;
#98718 = CARTESIAN_POINT ( 'NONE',  ( 10.00000000000000000, 54.75893115100078745, -9.846743663894594434 ) ) ;
#98719 = CARTESIAN_POINT ( 'NONE',  ( 19.84674366389459266, 48.71726448433413026, -2.638427012816827677 ) ) ;
#98720 = AXIS2_PLACEMENT_3D ( 'NONE', #71579, #11063, #3090 ) ;
#98721 = TOROIDAL_SURFACE ( 'NONE', #12464, 14.49999999999999822, 0.5000000000000000000 ) ;
#98723 = EDGE_LOOP ( 'NONE', ( #38432, #73846, #73417, #55240 ) ) ;
#98722 = CARTESIAN_POINT ( 'NONE',  ( 7.108715748589172101, 0.04922511925147215334, -12.92719074505367161 ) ) ;
#98724 = ADVANCED_FACE ( 'NONE', ( #18399 ), #78897, .T. ) ;
#98725 = CARTESIAN_POINT ( 'NONE',  ( 10.00000000000000000, 4.758931151000784787, -9.846743663894594434 ) ) ;
#98726 = DIRECTION ( 'NONE',  ( 1.000000000000000000, 0.000000000000000000, 0.000000000000000000 ) ) ;
#98727 = ORIENTED_EDGE ( 'NONE', *, *, #42576, .F. ) ;
#98728 = CARTESIAN_POINT ( 'NONE',  ( 19.67388484268946058, 87.39743296926540950, 5.439657303569386926 ) ) ;
#98729 = CARTESIAN_POINT ( 'NONE',  ( 19.84674366389459266, 28.30059781766745886, 2.638427012816836559 ) ) ;
#98730 = DIRECTION ( 'NONE',  ( 0.8070303256584299145, -0.5905099943842175847, 0.000000000000000000 ) ) ;
#98731 = CARTESIAN_POINT ( 'NONE',  ( 22.81628187352648496, 36.83196800326376064, -3.434112377981050290 ) ) ;
#98732 = EDGE_CURVE ( 'NONE', #35821, #4466, #38270, .T. ) ;
#98733 = CARTESIAN_POINT ( 'NONE',  ( 5.803070148808231465, 3.918713670743053586E-16, 13.28812917035392260 ) ) ;
#98734 = LINE ( 'NONE', #4873, #17194 ) ;
#98735 = DIRECTION ( 'NONE',  ( -0.000000000000000000, -0.000000000000000000, 1.000000000000000000 ) ) ;
#98736 = CARTESIAN_POINT ( 'NONE',  ( -14.09356342482601043, 0.04922511925147129291, 4.360913911515280184 ) ) ;
#98737 = CARTESIAN_POINT ( 'NONE',  ( 10.00000000000000000, 39.75893115100078745, -9.846743663894594434 ) ) ;
#98738 = CARTESIAN_POINT ( 'NONE',  ( 24.16423886937410614, 34.30374883491396787, 8.672049930838204340E-16 ) ) ;
#98739 = CARTESIAN_POINT ( 'NONE',  ( 5.076628168052703671, 51.84226448433412315, 8.527530157486179263 ) ) ;
#98740 = B_SPLINE_CURVE_WITH_KNOTS ( 'NONE', 3,
 ( #63252, #70290, #25773, #56267, #32262, #25290 ),
 .UNSPECIFIED., .F., .F.,
 ( 4, 2, 4 ),
 ( 3.409110551493946023E-05, 0.0004400426677367865174, 0.0008459942299586336017 ),
 .UNSPECIFIED. ) ;
#98741 = CARTESIAN_POINT ( 'NONE',  ( -9.402796353261210882, 14.63595249122789177, 11.68706210897751951 ) ) ;
#98742 = CARTESIAN_POINT ( 'NONE',  ( 10.00000000000000000, 4.758931151000784787, -9.846743663894594434 ) ) ;
#98743 = B_SPLINE_CURVE_WITH_KNOTS ( 'NONE', 3,
 ( #66743, #51244, #12256, #5758 ),
 .UNSPECIFIED., .F., .F.,
 ( 4, 4 ),
 ( 0.000000000000000000, 0.001036303429213369194 ),
 .UNSPECIFIED. ) ;
#98744 = CARTESIAN_POINT ( 'NONE',  ( 20.32896413005680003, 46.77164270246085209, 5.963430220938287007 ) ) ;
#98745 = CARTESIAN_POINT ( 'NONE',  ( 18.52753015748617571, 48.09226448433412315, 4.923371831947298993 ) ) ;
#98746 = CARTESIAN_POINT ( 'NONE',  ( 15.44008868035555793, 51.39701867748816966, -9.422509992056140149 ) ) ;
#98747 = CARTESIAN_POINT ( 'NONE',  ( 17.20831665107776587, 44.13393115100078745, -7.208316651077762316 ) ) ;
#98748 = CARTESIAN_POINT ( 'NONE',  ( 20.15039907845753220, 31.74884699246888786, 6.262539305110077059 ) ) ;
#98749 = CARTESIAN_POINT ( 'NONE',  ( -0.8801773607111008646, 43.27201867748817676, 2.915334737309923430 ) ) ;
#98750 = ORIENTED_EDGE ( 'NONE', *, *, #80288, .T. ) ;
#98751 = CARTESIAN_POINT ( 'NONE',  ( 5.129999999999995453, 43.00000000000000711, 6.250000000000000000 ) ) ;
#98752 = CARTESIAN_POINT ( 'NONE',  ( 15.44008868035555260, 19.73035201082150536, 9.422509992056143702 ) ) ;
#98754 = CARTESIAN_POINT ( 'NONE',  ( 0.5774900079438590739, 42.64701867748816966, -5.440088680355550821 ) ) ;
#98753 = CARTESIAN_POINT ( 'NONE',  ( 13.43411237798106583, 2.665301336597086568, -12.81628187352647252 ) ) ;
#98755 = CARTESIAN_POINT ( 'NONE',  ( 0.2751277870542979120, 15.30223176428831344, 6.500000000000003553 ) ) ;
#98756 = CARTESIAN_POINT ( 'NONE',  ( 19.84674366389459266, 13.30059781766745175, 2.638427012816836559 ) ) ;
#98757 = DIRECTION ( 'NONE',  ( 0.000000000000000000, 0.000000000000000000, 1.000000000000000000 ) ) ;
#98759 = CARTESIAN_POINT ( 'NONE',  ( 6.000000000000000000, 61.00000000000000711, 6.000000000000000000 ) ) ;
#98758 = CARTESIAN_POINT ( 'NONE',  ( 7.084665262690076126, 39.10535201082150536, 10.88017736071109987 ) ) ;
#98760 = CARTESIAN_POINT ( 'NONE',  ( 19.84674366389459621, 8.508931151000785675, 7.409399052514197653E-17 ) ) ;
#98761 = CARTESIAN_POINT ( 'NONE',  ( 12.63842701281683034, 42.46726448433412315, 9.846743663894596210 ) ) ;
#98762 = DIRECTION ( 'NONE',  ( 0.000000000000000000, 0.000000000000000000, 1.000000000000000000 ) ) ;
#98763 = CARTESIAN_POINT ( 'NONE',  ( -7.082119434687058401, 25.97041550158063572, -12.26659068614894110 ) ) ;
#98764 = CARTESIAN_POINT ( 'NONE',  ( 22.81628187352647785, 1.415301336597087012, 3.434112377981063169 ) ) ;
#98765 = CARTESIAN_POINT ( 'NONE',  ( 0.5774900079438607392, 3.480352010821504916, 5.440088680355550821 ) ) ;
#98766 = CARTESIAN_POINT ( 'NONE',  ( -10.09792486685197943, 0.04962894416274191839, 10.75589247084405109 ) ) ;
#98767 = CARTESIAN_POINT ( 'NONE',  ( 17.08211943468705840, 25.13708216824730357, -12.26659068614894466 ) ) ;
#98768 = EDGE_CURVE ( 'NONE', #87897, #74488, #14368, .T. ) ;
#98769 = CARTESIAN_POINT ( 'NONE',  ( 6.204703633549690345, 50.76208216824730357, -14.16423886937410259 ) ) ;
#98770 = AXIS2_PLACEMENT_3D ( 'NONE', #23541, #77008, #8033 ) ;
#98771 = DIRECTION ( 'NONE',  ( 0.000000000000000000, 0.000000000000000000, -1.000000000000000000 ) ) ;
#98772 = EDGE_LOOP ( 'NONE', ( #73876, #58469, #32727, #5067 ) ) ;
#98773 = CARTESIAN_POINT ( 'NONE',  ( 0.1532563361054083140, 21.00893115100078745, 1.131784320476157264E-15 ) ) ;
#98774 = CARTESIAN_POINT ( 'NONE',  ( 15.44008868035555793, 31.39701867748817676, -9.422509992056140149 ) ) ;
#98775 = CARTESIAN_POINT ( 'NONE',  ( 0.1532563361054100626, 45.80059781766745886, -2.638427012816831230 ) ) ;
#98777 = DIRECTION ( 'NONE',  ( -0.000000000000000000, -0.000000000000000000, -1.000000000000000000 ) ) ;
#98776 = CARTESIAN_POINT ( 'NONE',  ( 20.36894250292379738, 9.928748834913966093, -10.36894250292379027 ) ) ;
#98778 = CARTESIAN_POINT ( 'NONE',  ( -14.03351048042399007, -0.03417435944610275333, 2.474486531753619989 ) ) ;
#98779 = DIRECTION ( 'NONE',  ( 0.000000000000000000, 0.000000000000000000, 1.000000000000000000 ) ) ;
#98780 = CARTESIAN_POINT ( 'NONE',  ( -1.099225684535947600, 44.54030133659708923, 6.408140936763237150 ) ) ;
#98781 = CARTESIAN_POINT ( 'NONE',  ( 2.791683348922240793, 41.63393115100078745, 7.208316651077764092 ) ) ;
#98782 = ORIENTED_EDGE ( 'NONE', *, *, #83216, .T. ) ;
#98783 = CARTESIAN_POINT ( 'NONE',  ( 14.92337183194729633, 7.675597817667451750, 8.527530157486181039 ) ) ;
#98784 = CARTESIAN_POINT ( 'NONE',  ( 11.43665875895689332, -81.61983315981103715, -4.000000000003584688 ) ) ;
#98785 = CARTESIAN_POINT ( 'NONE',  ( 3.969999999999999751, 37.00000000000000000, 2.750000000000000000 ) ) ;
#98786 = CARTESIAN_POINT ( 'NONE',  ( 17.08211943468705840, 55.13708216824731068, -12.26659068614894466 ) ) ;
#98787 = CARTESIAN_POINT ( 'NONE',  ( 17.96484262340118221, 44.93868534415483396, 7.964842623401181321 ) ) ;
#98788 = COLOUR_RGB ( '', 0.31764706, 0.68627451, 0.89019608) ;
#98789 = SURFACE_SIDE_STYLE ('',( #92234 ) ) ;
#98790 = SURFACE_STYLE_FILL_AREA ( #3097 ) ;
#98791 = CARTESIAN_POINT ( 'NONE',  ( 14.92337183194729633, 32.67559781766745175, 8.527530157486181039 ) ) ;
#98792 = CARTESIAN_POINT ( 'NONE',  ( 10.00000000000000178, 9.313685344154839285, 10.88017736071110342 ) ) ;
#98793 = CARTESIAN_POINT ( 'NONE',  ( 7.361572987183169658, 34.96726448433411605, -9.846743663894592657 ) ) ;
#98794 = CARTESIAN_POINT ( 'NONE',  ( 18.18329248733322601, 2.602906685120200070, 6.499999999999992006 ) ) ;
#98795 = CARTESIAN_POINT ( 'NONE',  ( 10.00000000000000178, 57.25893115100078745, 9.846743663894594434 ) ) ;
#98796 = CARTESIAN_POINT ( 'NONE',  ( 10.00000000000000000, 51.81368534415484106, -10.88017736071110342 ) ) ;
#98797 = PRESENTATION_LAYER_ASSIGNMENT (  '', '', ( #76419 ) ) ;
#98798 = ORIENTED_EDGE ( 'NONE', *, *, #89195, .F. ) ;
#98799 = ORIENTED_EDGE ( 'NONE', *, *, #46871, .F. ) ;
#98800 = CARTESIAN_POINT ( 'NONE',  ( 19.38216949554541557, 52.24863466993041072, -9.382169495545420901 ) ) ;
#98801 = CARTESIAN_POINT ( 'NONE',  ( 8.564643372776615138, 0.5000000000000004441, -12.31449893000740836 ) ) ;
#98802 = CARTESIAN_POINT ( 'NONE',  ( 2.791683348922240793, 11.63393115100078568, 7.208316651077764092 ) ) ;
#98803 = CARTESIAN_POINT ( 'NONE',  ( 22.81628187352647785, 56.62363466993042493, 6.195893100308588602E-16 ) ) ;
#98805 = CARTESIAN_POINT ( 'NONE',  ( 19.84674366389459621, 53.50893115100078745, 7.409399052514197653E-17 ) ) ;
#98804 = CARTESIAN_POINT ( 'NONE',  ( 7.084665262690076126, 7.022018677488170546, -10.88017736071110164 ) ) ;
#98806 = CARTESIAN_POINT ( 'NONE',  ( 20.00000000000000711, 92.20777562798386384, 4.885465336098351763 ) ) ;
#98807 = FILL_AREA_STYLE_COLOUR ( '', #98190 ) ;
#98808 = CARTESIAN_POINT ( 'NONE',  ( 13.79529636645031943, 25.34541550158063572, -14.16423886937409904 ) ) ;
#98809 = CARTESIAN_POINT ( 'NONE',  ( 13.79529636645030344, 48.26208216824728936, 14.16423886937410614 ) ) ;
#98810 = CARTESIAN_POINT ( 'NONE',  ( 12.63842701281683034, 57.46726448433411605, 9.846743663894596210 ) ) ;
#98811 = CARTESIAN_POINT ( 'NONE',  ( 6.324651560460970323, -50.88858560564519706, -2.500000000000001776 ) ) ;
#98812 = CARTESIAN_POINT ( 'NONE',  ( 15.44008868035555793, 46.39701867748817676, -9.422509992056140149 ) ) ;
#98813 = CARTESIAN_POINT ( 'NONE',  ( 17.20831665107776587, 7.883931151000784787, 7.208316651077764980 ) ) ;
#98814 = EDGE_LOOP ( 'NONE', ( #69887, #16253, #24878, #80601, #4639, #94996 ) ) ;
#98815 = CARTESIAN_POINT ( 'NONE',  ( 3.591859063236761518, 59.95696800326375353, 11.09922568453594849 ) ) ;
#98816 = CARTESIAN_POINT ( 'NONE',  ( 10.00000000000000000, 14.75893115100078568, -9.846743663894594434 ) ) ;
#98817 = EDGE_LOOP ( 'NONE', ( #79614, #16729, #40740, #15802, #9680 ) ) ;
#98818 = CARTESIAN_POINT ( 'NONE',  ( -4.164238869374099039, 21.80374883491396787, 8.674139862899312516E-16 ) ) ;
#98819 = CARTESIAN_POINT ( 'NONE',  ( 10.00000000000000178, 7.258931151000785675, 9.846743663894594434 ) ) ;
#98820 = CARTESIAN_POINT ( 'NONE',  ( 2.035157376598822676, 32.43868534415483396, -7.964842623401177768 ) ) ;
#98821 = DIRECTION ( 'NONE',  ( -1.000000000000000000, -2.799047438454523236E-16, 0.000000000000000000 ) ) ;
#98822 = ORIENTED_EDGE ( 'NONE', *, *, #78485, .T. ) ;
#98823 = CARTESIAN_POINT ( 'NONE',  ( 4.559911319644449179, 32.23035201082150536, -9.422509992056141925 ) ) ;
#98824 = ADVANCED_FACE ( 'NONE', ( #34364 ), #64532, .T. ) ;
#98825 = EDGE_CURVE ( 'NONE', #62932, #56371, #75761, .T. ) ;
#98826 = ORIENTED_EDGE ( 'NONE', *, *, #9396, .F. ) ;
#98827 = VERTEX_POINT ( 'NONE', #20368 ) ;
#98828 = ORIENTED_EDGE ( 'NONE', *, *, #2099, .T. ) ;
#98829 = CARTESIAN_POINT ( 'NONE',  ( 0.6178305044545838731, 14.74863466993041783, 9.382169495545420901 ) ) ;
#98830 = AXIS2_PLACEMENT_3D ( 'NONE', #46721, #9715, #85228 ) ;
#98831 = CARTESIAN_POINT ( 'NONE',  ( 10.00000000000000178, 69.31368534415484817, 10.88017736071110342 ) ) ;
#98832 = DIRECTION ( 'NONE',  ( 0.9961946980917458783, -0.08715574274765407192, 0.000000000000000000 ) ) ;
#98833 = CARTESIAN_POINT ( 'NONE',  ( 19.84674366389459266, 18.30059781766745175, 2.638427012816836559 ) ) ;
#98834 = CARTESIAN_POINT ( 'NONE',  ( 12.91533473730993009, 31.60535201082150891, -10.88017736071109987 ) ) ;
#98835 = EDGE_LOOP ( 'NONE', ( #56136, #14309, #93867, #44161, #68052 ) ) ;
#98836 = CARTESIAN_POINT ( 'NONE',  ( 11.96291822454881348, 3.986488846351010315E-16, -8.193813980849080636 ) ) ;
#98837 = CARTESIAN_POINT ( 'NONE',  ( 12.91533473730992121, 39.52201867748817676, 10.88017736071110164 ) ) ;
#98838 = CARTESIAN_POINT ( 'NONE',  ( -1.926860441876562247, 22.45379003517447103, -3.195792623639530650 ) ) ;
#98839 = CARTESIAN_POINT ( 'NONE',  ( 3.591859063236761518, 49.95696800326375353, 11.09922568453594849 ) ) ;
#98840 = CARTESIAN_POINT ( 'NONE',  ( 2.035157376598824452, 63.68868534415484106, 7.964842623401179544 ) ) ;
#98841 = CARTESIAN_POINT ( 'NONE',  ( 19.84674366389459621, 63.50893115100078745, 7.409399052514197653E-17 ) ) ;
#98842 = EDGE_CURVE ( 'NONE', #26206, #32549, #57857, .T. ) ;
#98843 = CARTESIAN_POINT ( 'NONE',  ( 69.60148758828984228, -4.049828892140921146E-15, -9.500000000000000000 ) ) ;
#98844 = AXIS2_PLACEMENT_3D ( 'NONE', #12905, #43401, #64419 ) ;
#98845 = CARTESIAN_POINT ( 'NONE',  ( 1.472469842513823179, 15.59226448433411960, -4.923371831947296329 ) ) ;
#98846 = CARTESIAN_POINT ( 'NONE',  ( -2.816281873526473856, 49.33196800326374643, 3.434112377981055619 ) ) ;
#98847 = DIRECTION ( 'NONE',  ( -1.000000000000000000, 0.000000000000000000, 0.000000000000000000 ) ) ;
#98848 = CARTESIAN_POINT ( 'NONE',  ( 5.076628168052704559, 5.175597817667451750, -8.527530157486179263 ) ) ;
#98849 = CARTESIAN_POINT ( 'NONE',  ( 13.43411237798106583, 17.66530133659708923, -12.81628187352647252 ) ) ;
#98851 = DIRECTION ( 'NONE',  ( -6.608470384673550777E-17, -1.000000000000000000, 0.000000000000000000 ) ) ;
#98850 = LINE ( 'NONE', #69310, #6913 ) ;
#98852 = CARTESIAN_POINT ( 'NONE',  ( 12.91533473730993009, 31.60535201082150891, -10.88017736071109987 ) ) ;
#98853 = CARTESIAN_POINT ( 'NONE',  ( -1.099225684535947600, -1.293031996736246469, -6.408140936763238038 ) ) ;
#98854 = CARTESIAN_POINT ( 'NONE',  ( 3.969999999999999751, 36.75000000000000000, 4.000000000000000000 ) ) ;
#98856 = CARTESIAN_POINT ( 'NONE',  ( 18.52753015748617571, 18.09226448433411960, 4.923371831947298993 ) ) ;
#98855 = AXIS2_PLACEMENT_3D ( 'NONE', #70630, #86125, #2159 ) ;
#98857 = CARTESIAN_POINT ( 'NONE',  ( 18.52753015748618282, 13.92559781766745175, -4.923371831947291888 ) ) ;
#98859 = ORIENTED_EDGE ( 'NONE', *, *, #60675, .T. ) ;
#98858 = CARTESIAN_POINT ( 'NONE',  ( 10.00000000000000000, -2.126365330069579951, -12.81628187352647608 ) ) ;
#98860 = AXIS2_PLACEMENT_3D ( 'NONE', #89923, #43921, #27937 ) ;
#98861 = CARTESIAN_POINT ( 'NONE',  ( 12.91533473730993009, 6.605352010821504471, -10.88017736071109987 ) ) ;
#98862 = FACE_OUTER_BOUND ( 'NONE', #66822, .T. ) ;
#98863 = CARTESIAN_POINT ( 'NONE',  ( 4.380000000000000782, 1.019547802438464545, -2.750000000000000000 ) ) ;
#98864 = CARTESIAN_POINT ( 'NONE',  ( 7.084665262690076126, 9.105352010821503583, 10.88017736071109987 ) ) ;
#98865 = CARTESIAN_POINT ( 'NONE',  ( 12.63842701281683922, 49.55059781766744464, -9.846743663894590881 ) ) ;
#98866 = EDGE_LOOP ( 'NONE', ( #59643, #93950, #49816, #5567 ) ) ;
#98867 = LINE ( 'NONE', #90325, #24956 ) ;
#98868 = CARTESIAN_POINT ( 'NONE',  ( -0.3689425029237898834, 66.17874883491396076, -10.36894250292378850 ) ) ;
#98869 = CARTESIAN_POINT ( 'NONE',  ( 17.96484262340118221, 34.93868534415482685, 7.964842623401181321 ) ) ;
#98870 = CARTESIAN_POINT ( 'NONE',  ( 24.16423886937410614, 49.51208216824730357, -3.795296366450302550 ) ) ;
#98872 = LINE ( 'NONE', #76817, #84595 ) ;
#98871 = CARTESIAN_POINT ( 'NONE',  ( 17.08211943468705130, 63.47041550158063927, 12.26659068614894998 ) ) ;
#98873 = CARTESIAN_POINT ( 'NONE',  ( 17.20831665107776587, 2.883931151000785231, 7.208316651077764980 ) ) ;
#98874 = CARTESIAN_POINT ( 'NONE',  ( 0.1532563361054082862, 26.21726448433411605, 2.638427012816831674 ) ) ;
#98875 = CARTESIAN_POINT ( 'NONE',  ( 21.09922568453595559, 17.04030133659708923, -6.408140936763230044 ) ) ;
#98876 = CARTESIAN_POINT ( 'NONE',  ( -2.518025504887116739, 0.000000000000000000, 4.837081990145610355 ) ) ;
#98877 = ORIENTED_EDGE ( 'NONE', *, *, #65588, .F. ) ;
#98878 = DIRECTION ( 'NONE',  ( -0.000000000000000000, 0.000000000000000000, 1.000000000000000000 ) ) ;
#98879 = CARTESIAN_POINT ( 'NONE',  ( 14.92337183194729633, 57.67559781766745886, 8.527530157486181039 ) ) ;
#98880 = AXIS2_PLACEMENT_3D ( 'NONE', #9891, #70890, #63366 ) ;
#98881 = FACE_OUTER_BOUND ( 'NONE', #2745, .T. ) ;
#98882 = CARTESIAN_POINT ( 'NONE',  ( -11.16008302860135259, -52.90628376244837483, -3.749999999998196998 ) ) ;
#98883 = CARTESIAN_POINT ( 'NONE',  ( 6.204703633549690345, 10.76208216824729824, -14.16423886937410259 ) ) ;
#98884 = CARTESIAN_POINT ( 'NONE',  ( 18.52753015748618282, 28.92559781766745175, -4.923371831947291888 ) ) ;
#98885 = DIRECTION ( 'NONE',  ( 1.636349903325072848E-16, -1.000000000000000000, 0.000000000000000000 ) ) ;
#98886 = VERTEX_POINT ( 'NONE', #36350 ) ;
#98887 = CARTESIAN_POINT ( 'NONE',  ( 24.16423886937409904, 59.09541550158063217, 3.795296366450317205 ) ) ;
#98888 = CARTESIAN_POINT ( 'NONE',  ( 19.84674366389459266, 8.717264484334116048, -2.638427012816827677 ) ) ;
#98890 = CARTESIAN_POINT ( 'NONE',  ( 4.431036607602467647, 14.49999999999999822, 14.33059365769914351 ) ) ;
#98889 = DIRECTION ( 'NONE',  ( 0.5901017155109145040, 0.8073289077885640319, 0.000000000000000000 ) ) ;
#98891 = CARTESIAN_POINT ( 'NONE',  ( 0.5774900079438590739, 37.64701867748817676, -5.440088680355550821 ) ) ;
#98892 = CARTESIAN_POINT ( 'NONE',  ( 21.09922568453594849, 51.20696800326375353, 6.408140936763242479 ) ) ;
#98893 = CARTESIAN_POINT ( 'NONE',  ( 19.42250999205614548, 5.980352010821504471, -5.440088680355545492 ) ) ;
#98894 = CARTESIAN_POINT ( 'NONE',  ( -1.099225684535947600, 34.54030133659708923, 6.408140936763237150 ) ) ;
#98895 = CARTESIAN_POINT ( 'NONE',  ( 19.84674366389459266, 3.717264484334118713, -2.638427012816827677 ) ) ;
#98896 = VERTEX_POINT ( 'NONE', #80867 ) ;
#98897 = DIRECTION ( 'NONE',  ( 0.000000000000000000, 0.000000000000000000, 1.000000000000000000 ) ) ;
#98898 = CARTESIAN_POINT ( 'NONE',  ( -11.35178980618961830, 14.63595249122790065, -9.804941009312081235 ) ) ;
#98899 = CARTESIAN_POINT ( 'NONE',  ( 10.00000000000000000, 45.55374883491397497, -14.16423886937410082 ) ) ;
#98900 = CARTESIAN_POINT ( 'NONE',  ( -4.164238869374098151, 11.59541550158063217, -3.795296366450310543 ) ) ;
#98901 = CARTESIAN_POINT ( 'NONE',  ( 0.5774900079438607392, 8.480352010821505360, 5.440088680355550821 ) ) ;
#98902 = CARTESIAN_POINT ( 'NONE',  ( 10.00000000000000000, 41.81368534415484106, -10.88017736071110342 ) ) ;
#98903 = CARTESIAN_POINT ( 'NONE',  ( 9.876730923139335871, 14.63606899087332991, -11.28938378619065297 ) ) ;
#98904 =( LENGTH_UNIT ( ) NAMED_UNIT ( * ) SI_UNIT ( .MILLI., .METRE. ) );
#98905 = CARTESIAN_POINT ( 'NONE',  ( 2.035157376598824452, 48.68868534415483396, 7.964842623401179544 ) ) ;
#98906 = CARTESIAN_POINT ( 'NONE',  ( 4.559911319644449179, 68.89701867748817676, 9.422509992056141925 ) ) ;
#98907 = CARTESIAN_POINT ( 'NONE',  ( 3.591859063236761518, 29.95696800326375708, 11.09922568453594849 ) ) ;
#98908 = CARTESIAN_POINT ( 'NONE',  ( 18.72515096720568550, 20.05509018479935790, 6.500000000000015099 ) ) ;
#98909 = CARTESIAN_POINT ( 'NONE',  ( -3.270119481323481736, 14.95077488074853456, -14.38584091150425337 ) ) ;
#98910 = CARTESIAN_POINT ( 'NONE',  ( 19.84674366389459621, 38.50893115100078745, 7.409399052514197653E-17 ) ) ;
#98911 = ADVANCED_FACE ( 'NONE', ( #51845 ), #4879, .T. ) ;
#98912 = CARTESIAN_POINT ( 'NONE',  ( 16.40814093676323893, 20.79030133659708923, 11.09922568453595026 ) ) ;
#98913 = CARTESIAN_POINT ( 'NONE',  ( 0.1532563361054082862, 11.21726448433411605, 2.638427012816831674 ) ) ;
#98914 = CARTESIAN_POINT ( 'NONE',  ( 20.88017736071110875, 10.77201867748817143, -2.915334737309920765 ) ) ;
#98915 = CARTESIAN_POINT ( 'NONE',  ( 19.84674366389459621, 38.50893115100078745, 7.409399052514197653E-17 ) ) ;
#98916 = CARTESIAN_POINT ( 'NONE',  ( 13.43411237798106583, 57.66530133659708923, -12.81628187352647252 ) ) ;
#98917 = CARTESIAN_POINT ( 'NONE',  ( 19.84674366389459266, 23.30059781766745530, 2.638427012816836559 ) ) ;
#98918 = CARTESIAN_POINT ( 'NONE',  ( -2.266590686148945544, 6.387082168247300906, -7.082119434687050408 ) ) ;
#98919 = CARTESIAN_POINT ( 'NONE',  ( 13.61464873478162652, 0.5000000000000004441, 6.296136897217931683 ) ) ;
#98920 = CARTESIAN_POINT ( 'NONE',  ( -0.8801773607111008646, 33.27201867748817676, 2.915334737309923430 ) ) ;
#98921 = CARTESIAN_POINT ( 'NONE',  ( 2.035157376598822676, 17.43868534415483751, -7.964842623401177768 ) ) ;
#98922 =( GEOMETRIC_REPRESENTATION_CONTEXT ( 3 ) GLOBAL_UNCERTAINTY_ASSIGNED_CONTEXT ( ( #77214 ) ) GLOBAL_UNIT_ASSIGNED_CONTEXT ( ( #52287, #75775, #37795 ) ) REPRESENTATION_CONTEXT ( 'NONE', 'WORKASPACE' ) );
#98923 = CARTESIAN_POINT ( 'NONE',  ( 20.88017736071110519, 30.56368534415484106, 2.639326808657452039E-16 ) ) ;
#98924 = CARTESIAN_POINT ( 'NONE',  ( 20.88017736071110875, 15.77201867748817143, -2.915334737309920765 ) ) ;
#98925 = ORIENTED_EDGE ( 'NONE', *, *, #38845, .F. ) ;
#98926 = ADVANCED_FACE ( 'NONE', ( #74331 ), #88858, .T. ) ;
#98927 = B_SPLINE_CURVE_WITH_KNOTS ( 'NONE', 3,
 ( #29903, #22929, #53397, #77373, #38909, #62367, #83906, #45914, #31381, #15435, #69396, #918, #16895, #91400, #70389, #54871, #76403, #53903, #7918, #68419, #15909, #77870 ),
 .UNSPECIFIED., .F., .F.,
 ( 4, 2, 2, 2, 2, 2, 2, 2, 2, 2, 4 ),
 ( 0.000000000000000000, 0.002789117597787886711, 0.005578235195575773422, 0.01115647039115154684, 0.02231294078230309369, 0.03346941117345463707, 0.04462588156460618738, 0.06693882234690927413, 0.07809529273806081751, 0.08367352793363661001, 0.08925176312921238864 ),
 .UNSPECIFIED. ) ;
#98928 = CARTESIAN_POINT ( 'NONE',  ( 17.96484262340118221, 29.93868534415484106, 7.964842623401181321 ) ) ;
#98930 = CARTESIAN_POINT ( 'NONE',  ( -2.816281873526471635, 48.91530133659708213, -3.434112377981056508 ) ) ;
#98929 = VECTOR ( 'NONE', #23554, 1000.000000000000000 ) ;
#98931 = CARTESIAN_POINT ( 'NONE',  ( 17.96484262340118221, 46.18868534415484106, -7.964842623401177768 ) ) ;
#98933 = CARTESIAN_POINT ( 'NONE',  ( 20.88017736071110164, 45.35535201082149115, 2.915334737309930979 ) ) ;
#98932 = CARTESIAN_POINT ( 'NONE',  ( 2.603489959281590771, 46.58210964143328425, 6.500000000000003553 ) ) ;
#98934 = ORIENTED_EDGE ( 'NONE', *, *, #80963, .F. ) ;
#98936 = EDGE_CURVE ( 'NONE', #38297, #74440, #58339, .T. ) ;
#98935 = CARTESIAN_POINT ( 'NONE',  ( 7.084665262690076126, 49.10535201082149825, 10.88017736071109987 ) ) ;
#98937 = CARTESIAN_POINT ( 'NONE',  ( 7.079515573063597245, -88.00917032380698402, 4.000000000000000000 ) ) ;
#98938 = DIRECTION ( 'NONE',  ( 0.6626200482157357241, 0.000000000000000000, 0.7489557207890036317 ) ) ;
#98939 = CARTESIAN_POINT ( 'NONE',  ( 22.26659068614894466, 43.88708216824729647, 7.082119434687054849 ) ) ;
#98940 = CARTESIAN_POINT ( 'NONE',  ( 12.91533473730992121, 64.52201867748817676, 10.88017736071110164 ) ) ;
#98941 = ADVANCED_FACE ( 'NONE', ( #74838 ), #3973, .T. ) ;
#98942 = DIRECTION ( 'NONE',  ( -0.000000000000000000, -1.000000000000000000, -0.000000000000000000 ) ) ;
#98943 = CARTESIAN_POINT ( 'NONE',  ( 2.791683348922237240, 60.38393115100078745, -7.208316651077763204 ) ) ;
#98944 = CARTESIAN_POINT ( 'NONE',  ( 4.873787042390789637, 0.000000000000000000, -13.39061984619918988 ) ) ;
#98945 = CARTESIAN_POINT ( 'NONE',  ( 12.63842701281683922, 34.55059781766745886, -9.846743663894590881 ) ) ;
#98946 = EDGE_LOOP ( 'NONE', ( #84788, #43588, #78150, #48565 ) ) ;
#98947 = CARTESIAN_POINT ( 'NONE',  ( 14.92337183194729988, 29.34226448433411960, -8.527530157486177487 ) ) ;
#98948 = CARTESIAN_POINT ( 'NONE',  ( 6.408140936763236262, -7.543031996736241140, -11.09922568453595026 ) ) ;
#98949 = CARTESIAN_POINT ( 'NONE',  ( 15.44008868035555793, 21.39701867748817321, -9.422509992056140149 ) ) ;
#98950 = CARTESIAN_POINT ( 'NONE',  ( 5.076628168052703671, 31.84226448433412315, 8.527530157486179263 ) ) ;
#98951 = CARTESIAN_POINT ( 'NONE',  ( 10.00000000000000178, 25.37363466993041783, 12.81628187352647608 ) ) ;
#98953 = CARTESIAN_POINT ( 'NONE',  ( 2.035157376598824452, 53.68868534415484817, 7.964842623401179544 ) ) ;
#98952 = CARTESIAN_POINT ( 'NONE',  ( 0.000000000000000000, 14.49999999999999822, 0.000000000000000000 ) ) ;
#98955 = SURFACE_STYLE_USAGE ( .BOTH. , #14450 ) ;
#98954 = CARTESIAN_POINT ( 'NONE',  ( 17.96484262340118221, 29.93868534415484106, 7.964842623401181321 ) ) ;
#98956 = CARTESIAN_POINT ( 'NONE',  ( 6.204703633549690345, 57.84541550158063927, 14.16423886937410082 ) ) ;
#98957 = B_SPLINE_CURVE_WITH_KNOTS ( 'NONE', 3,
 ( #86579, #94560, #56085, #87063, #96051, #25593, #79570, #56572, #95553, #10092, #3096, #80049, #94072, #95045, #86088, #42073, #4068, #50046, #18087, #64047, #12046, #63564 ),
 .UNSPECIFIED., .F., .F.,
 ( 4, 2, 2, 2, 2, 2, 2, 2, 2, 2, 4 ),
 ( 0.000000000000000000, 0.005577058014692720320, 0.01115411602938544064, 0.02230823205877083618, 0.04461646411754159602, 0.05577058014692697074, 0.06692469617631234546, 0.07807881220569773406, 0.08365587022039042142, 0.08644439922773676510, 0.08923292823508310878 ),
 .UNSPECIFIED. ) ;
#98958 = CARTESIAN_POINT ( 'NONE',  ( 19.38216949554541557, 27.24863466993041783, -9.382169495545420901 ) ) ;
#98959 = CARTESIAN_POINT ( 'NONE',  ( 6.880000000000009663, 40.99999999999999289, 4.250000000000000000 ) ) ;
#98960 = ORIENTED_EDGE ( 'NONE', *, *, #55564, .T. ) ;
#98961 = CARTESIAN_POINT ( 'NONE',  ( 21.09922568453595559, 12.04030133659708746, -6.408140936763230044 ) ) ;
#98962 = CARTESIAN_POINT ( 'NONE',  ( 12.91533473730992121, 14.52201867748817143, 10.88017736071110164 ) ) ;
#98963 = CARTESIAN_POINT ( 'NONE',  ( 20.88017736071110164, 45.35535201082149115, 2.915334737309930979 ) ) ;
#98964 = CARTESIAN_POINT ( 'NONE',  ( 9.879999999999984794, 27.00000000000000711, 2.958578643762690419 ) ) ;
#98966 = VERTEX_POINT ( 'NONE', #21353 ) ;
#98965 = EDGE_CURVE ( 'NONE', #88314, #13980, #19134, .T. ) ;
#98967 = COLOUR_RGB ( '', 0.66274510, 0.83137255, 0.94901961) ;
#98968 = CARTESIAN_POINT ( 'NONE',  ( -0.8801773607110991993, 62.85535201082150536, -2.915334737309923874 ) ) ;
#98969 = CARTESIAN_POINT ( 'NONE',  ( 10.00000000000000000, 29.75893115100078745, -9.846743663894594434 ) ) ;
#98970 = CARTESIAN_POINT ( 'NONE',  ( 2.791683348922237240, 30.38393115100078390, -7.208316651077763204 ) ) ;
#98971 = CARTESIAN_POINT ( 'NONE',  ( 1.472469842513823179, 10.59226448433411782, -4.923371831947296329 ) ) ;
#98972 = FACE_OUTER_BOUND ( 'NONE', #17981, .T. ) ;
#98974 = CARTESIAN_POINT ( 'NONE',  ( 3.591859063236761518, 39.95696800326375353, 11.09922568453594849 ) ) ;
#98973 = DIRECTION ( 'NONE',  ( 0.000000000000000000, 1.000000000000000000, 0.000000000000000000 ) ) ;
#98976 = DIRECTION ( 'NONE',  ( 0.000000000000000000, 1.000000000000000000, -0.000000000000000000 ) ) ;
#98975 = CARTESIAN_POINT ( 'NONE',  ( 7.361572987183169658, 19.96726448433411960, -9.846743663894592657 ) ) ;
#98977 = CARTESIAN_POINT ( 'NONE',  ( 20.32896413005680714, 45.57879003517447813, -5.963430220938276349 ) ) ;
#98979 = ORIENTED_EDGE ( 'NONE', *, *, #599, .T. ) ;
#98978 = CARTESIAN_POINT ( 'NONE',  ( 10.00000000000000000, 34.75893115100078745, -9.846743663894594434 ) ) ;
#98980 = CARTESIAN_POINT ( 'NONE',  ( 21.09922568453595559, 62.04030133659709634, -6.408140936763230044 ) ) ;
#98981 = CARTESIAN_POINT ( 'NONE',  ( 1.379999999999981908, 20.99999999999999645, 0.000000000000000000 ) ) ;
#98982 = CARTESIAN_POINT ( 'NONE',  ( -1.099225684535947600, 9.540301336597087456, 6.408140936763237150 ) ) ;
#98983 = CARTESIAN_POINT ( 'NONE',  ( 0.5774900079438590739, 47.64701867748817676, -5.440088680355550821 ) ) ;
#98984 = CARTESIAN_POINT ( 'NONE',  ( 24.16423886937410614, 29.30374883491396787, 8.672049930838204340E-16 ) ) ;
#98985 = CARTESIAN_POINT ( 'NONE',  ( -14.40939250469967448, 4.171366831970869137E-16, 1.618458416365661012 ) ) ;
#98986 = CARTESIAN_POINT ( 'NONE',  ( 24.16423886937409904, 34.09541550158064638, 3.795296366450317205 ) ) ;
#98987 = CARTESIAN_POINT ( 'NONE',  ( 22.26659068614894466, 58.88708216824729647, 7.082119434687054849 ) ) ;
#98988 = CARTESIAN_POINT ( 'NONE',  ( 22.26659068614894466, 3.887082168247300906, 7.082119434687054849 ) ) ;
#8810 = FACE_OUTER_BOUND ( 'NONE', #6338, .T. ) ;
#98990 = NEXT_ASSEMBLY_USAGE_OCCURRENCE ( 'NAUO1', ' ', ' ', #32419, #56260, $ ) ;
#98991 = NEXT_ASSEMBLY_USAGE_OCCURRENCE ( 'NAUO2', ' ', ' ', #32419, #66632, $ ) ;
#98992 = NEXT_ASSEMBLY_USAGE_OCCURRENCE ( 'NAUO3', ' ', ' ', #32419, #70937, $ ) ;
#98993 = NEXT_ASSEMBLY_USAGE_OCCURRENCE ( 'NAUO4', ' ', ' ', #32419, #4342, $ ) ;
#98994 = NEXT_ASSEMBLY_USAGE_OCCURRENCE ( 'NAUO5', ' ', ' ', #32419, #48898, $ ) ;
ENDSEC;
END-ISO-10303-21;
